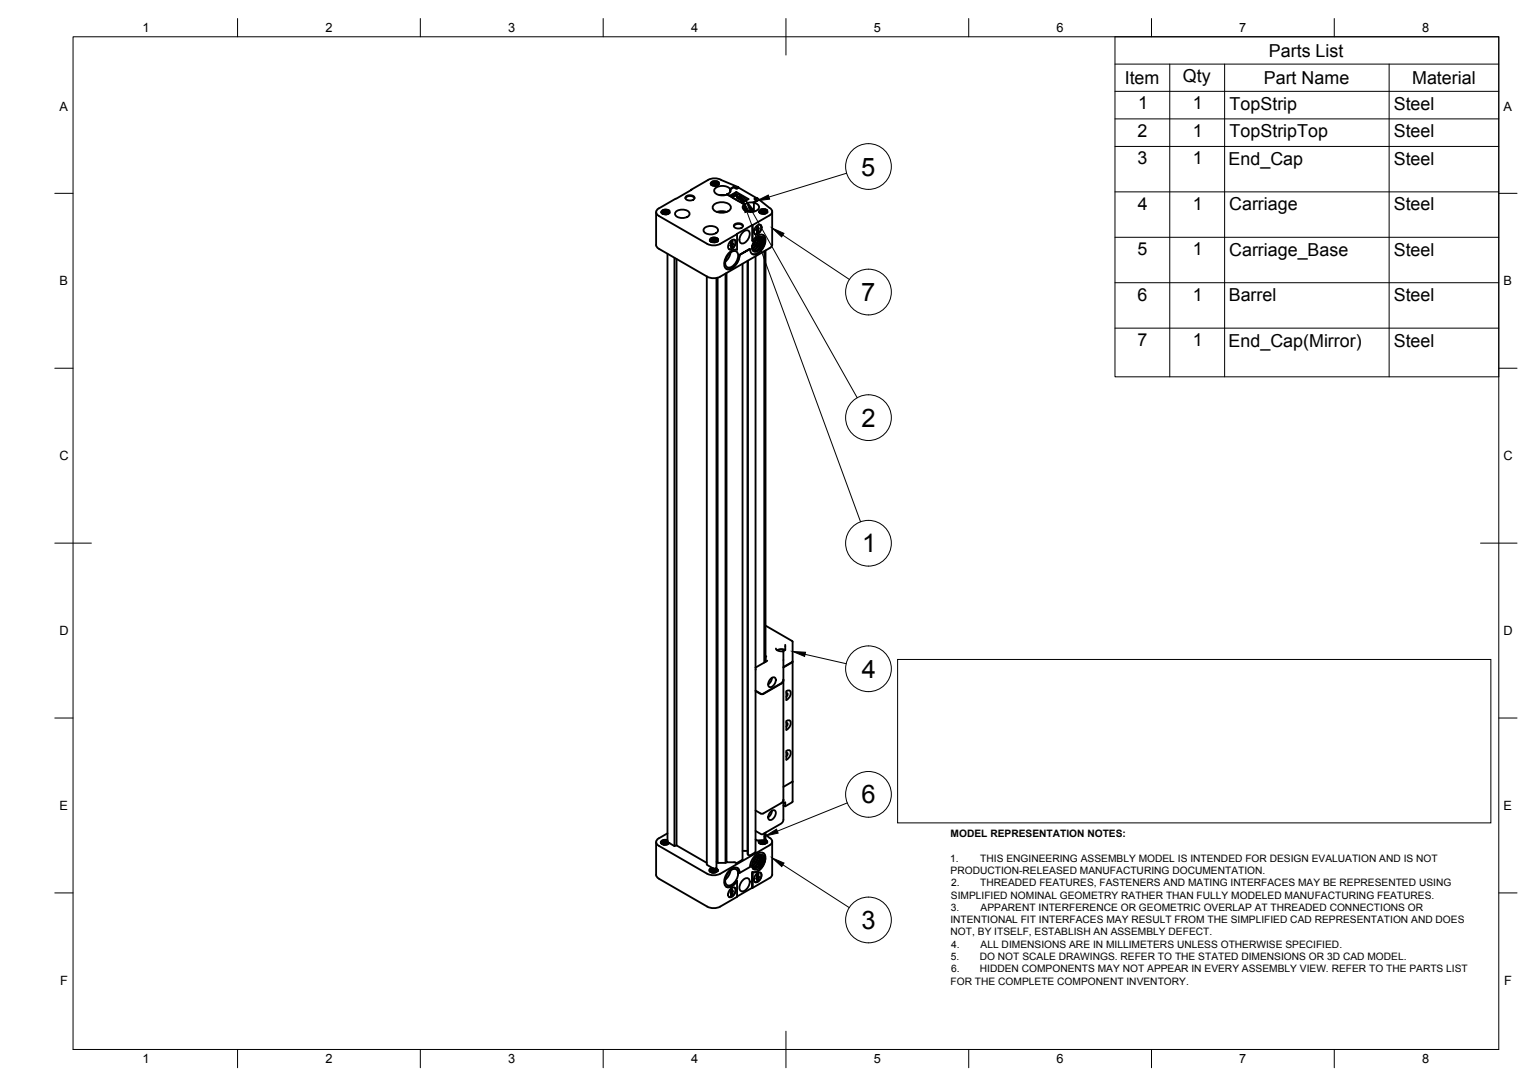
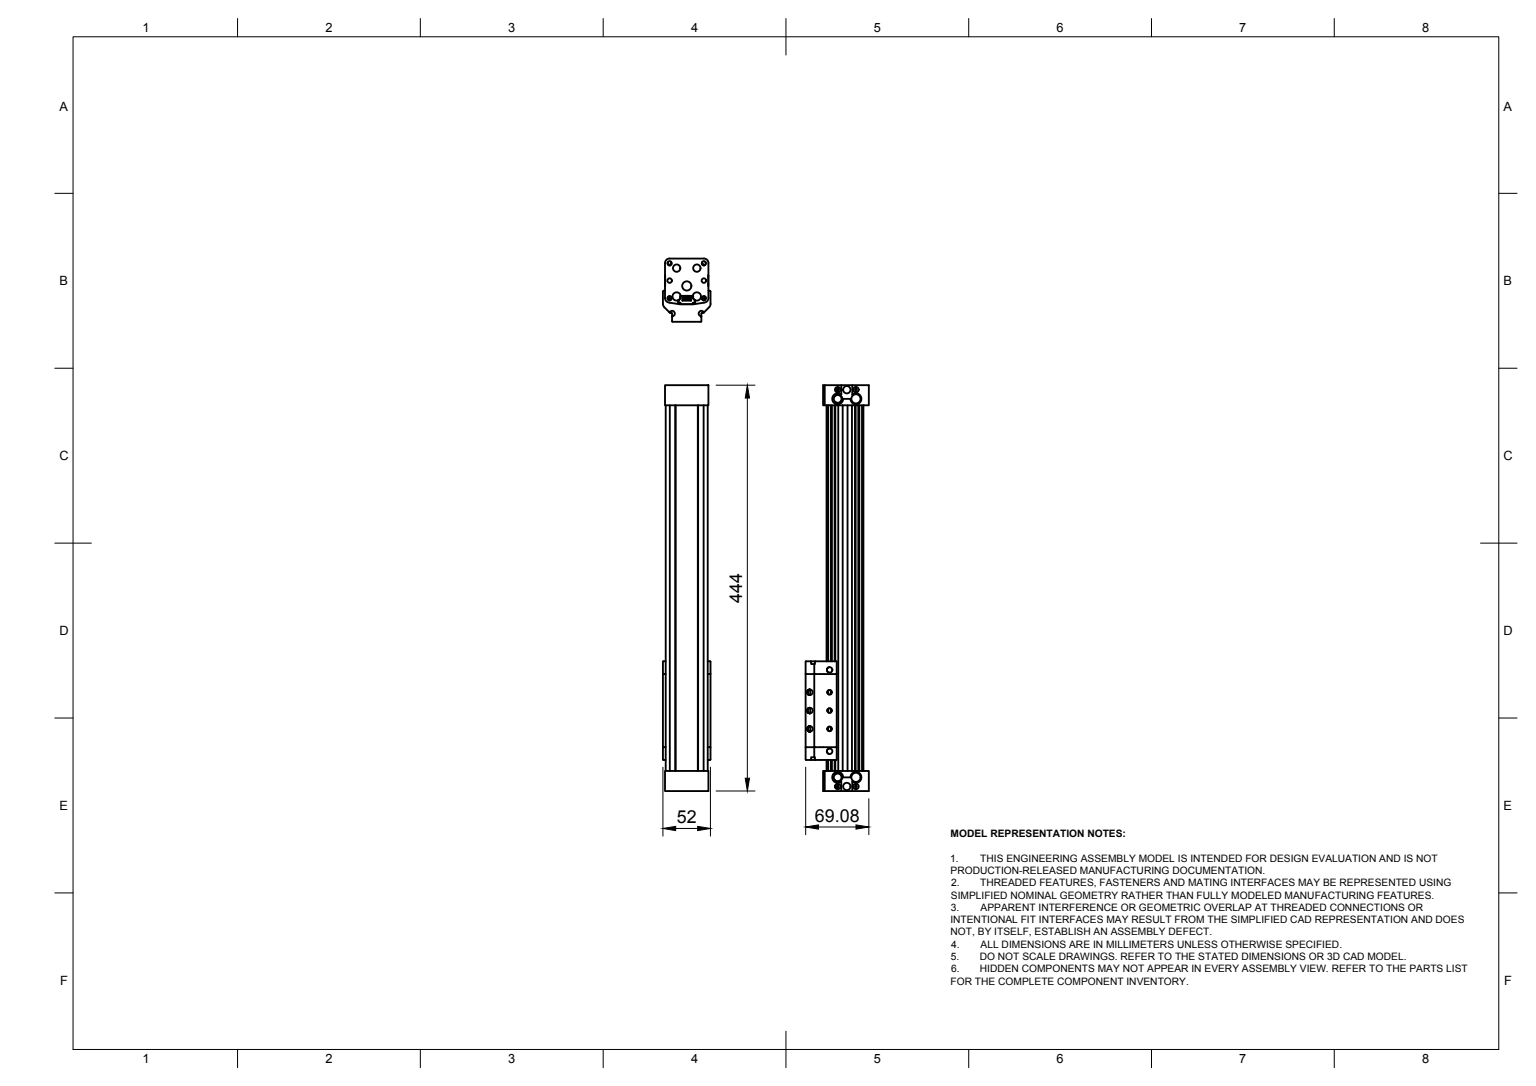
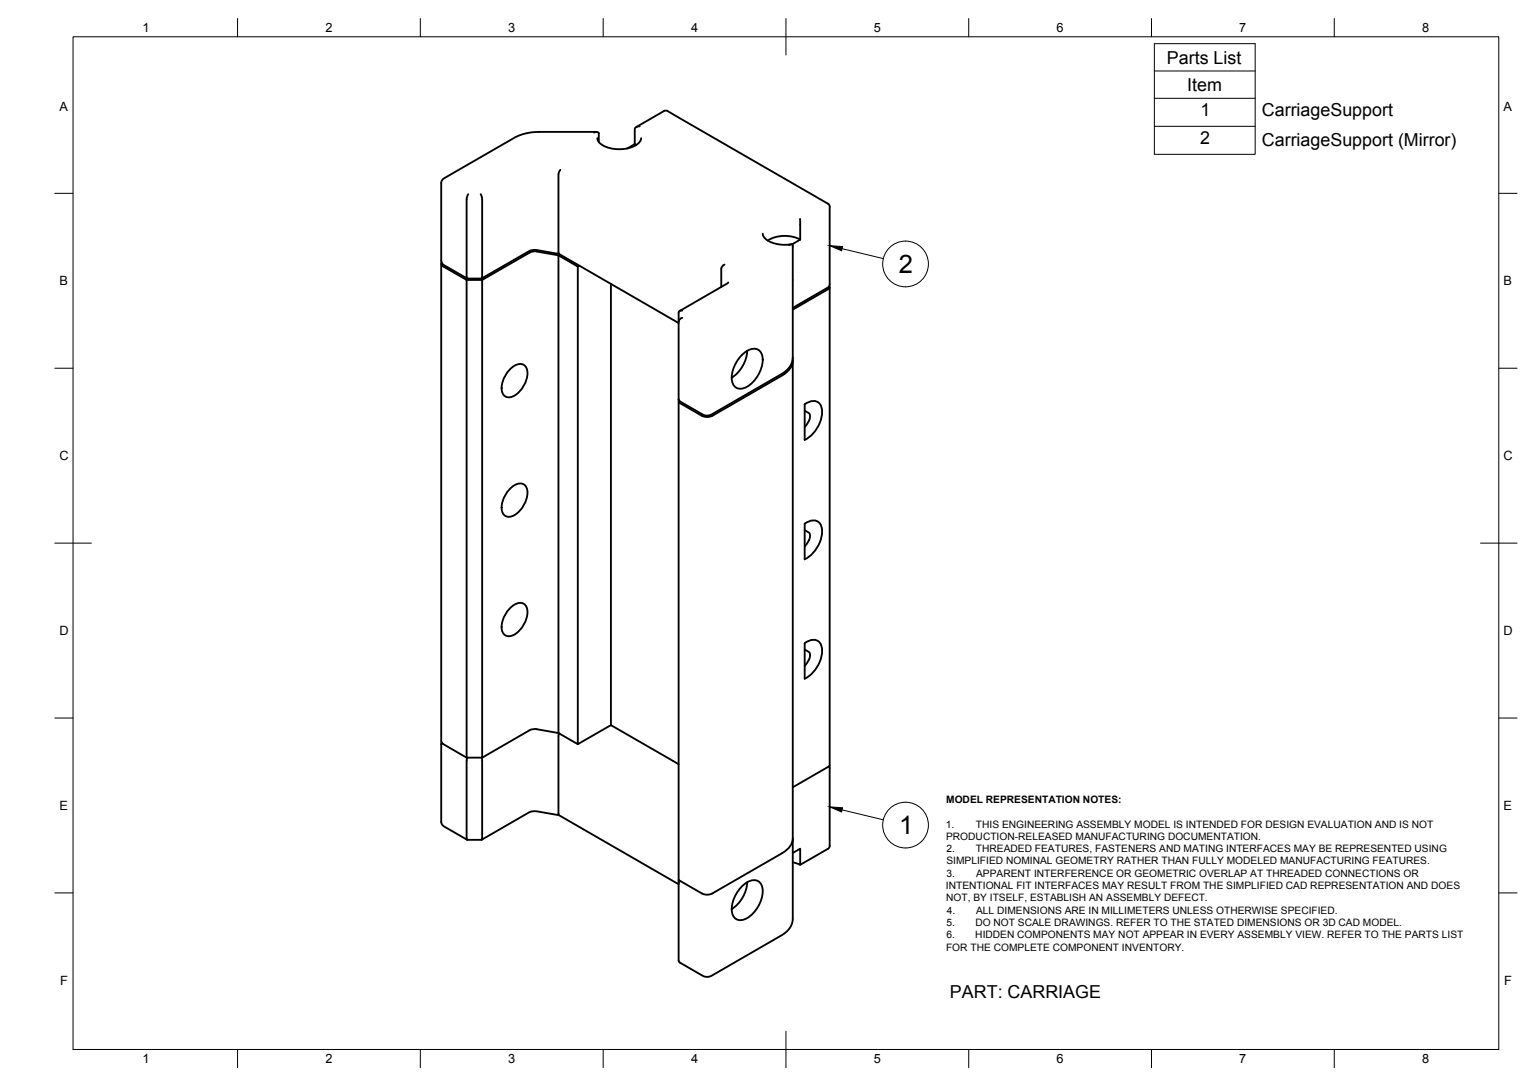
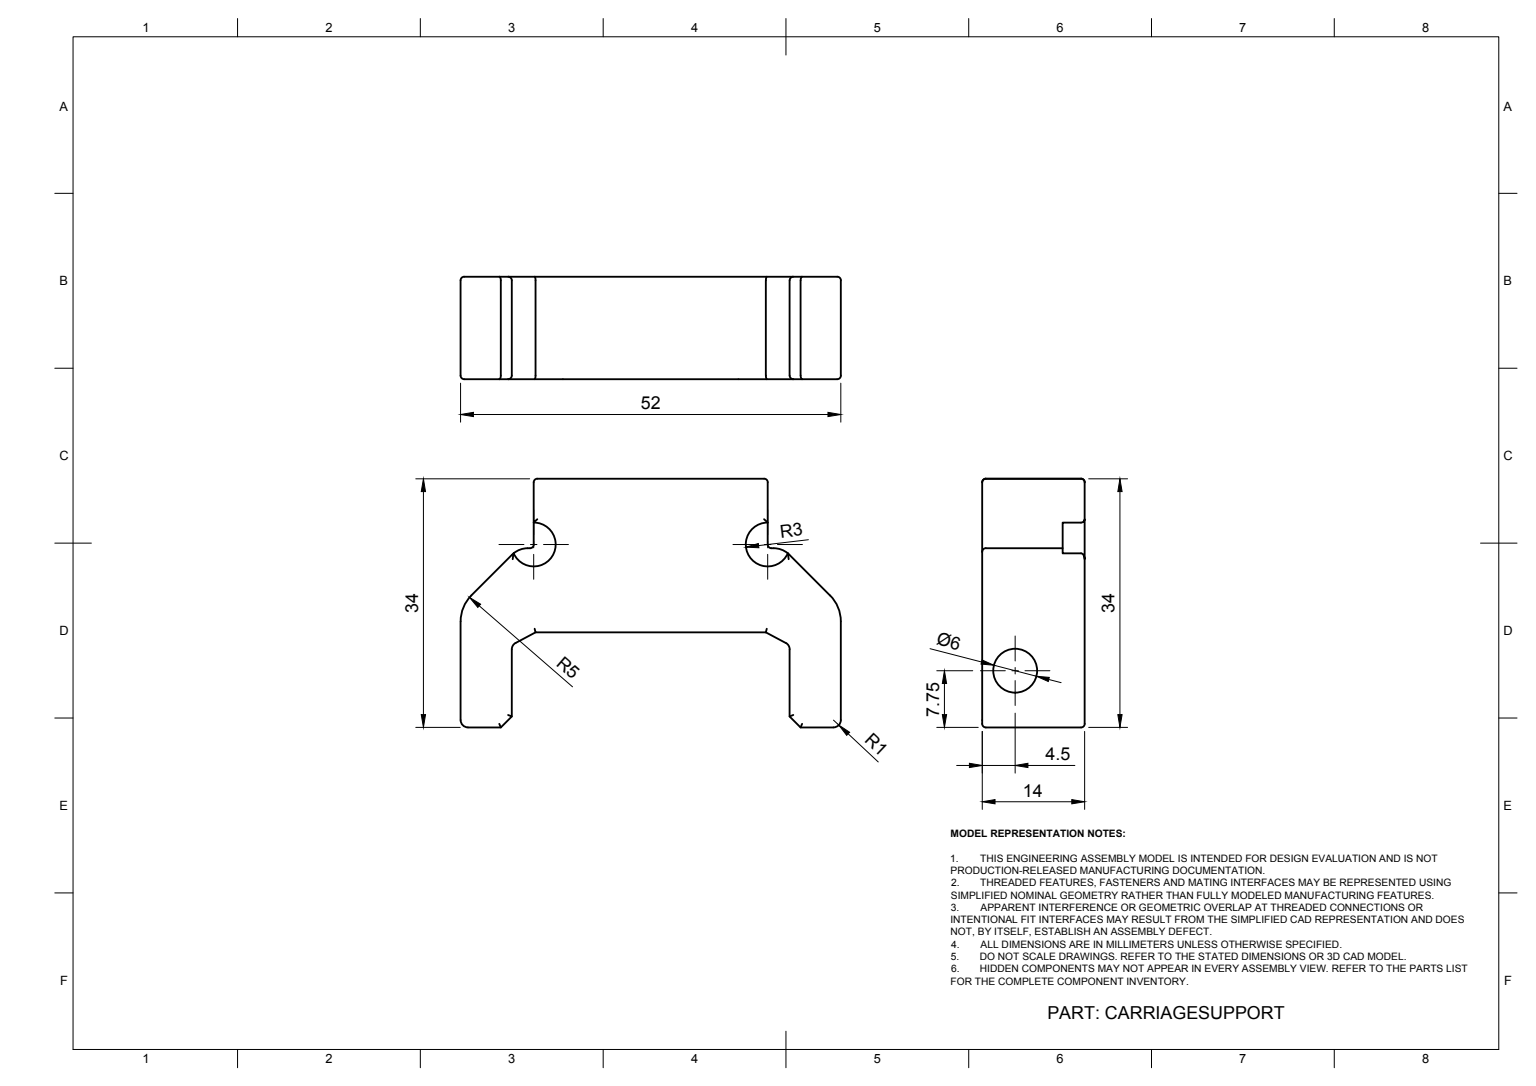
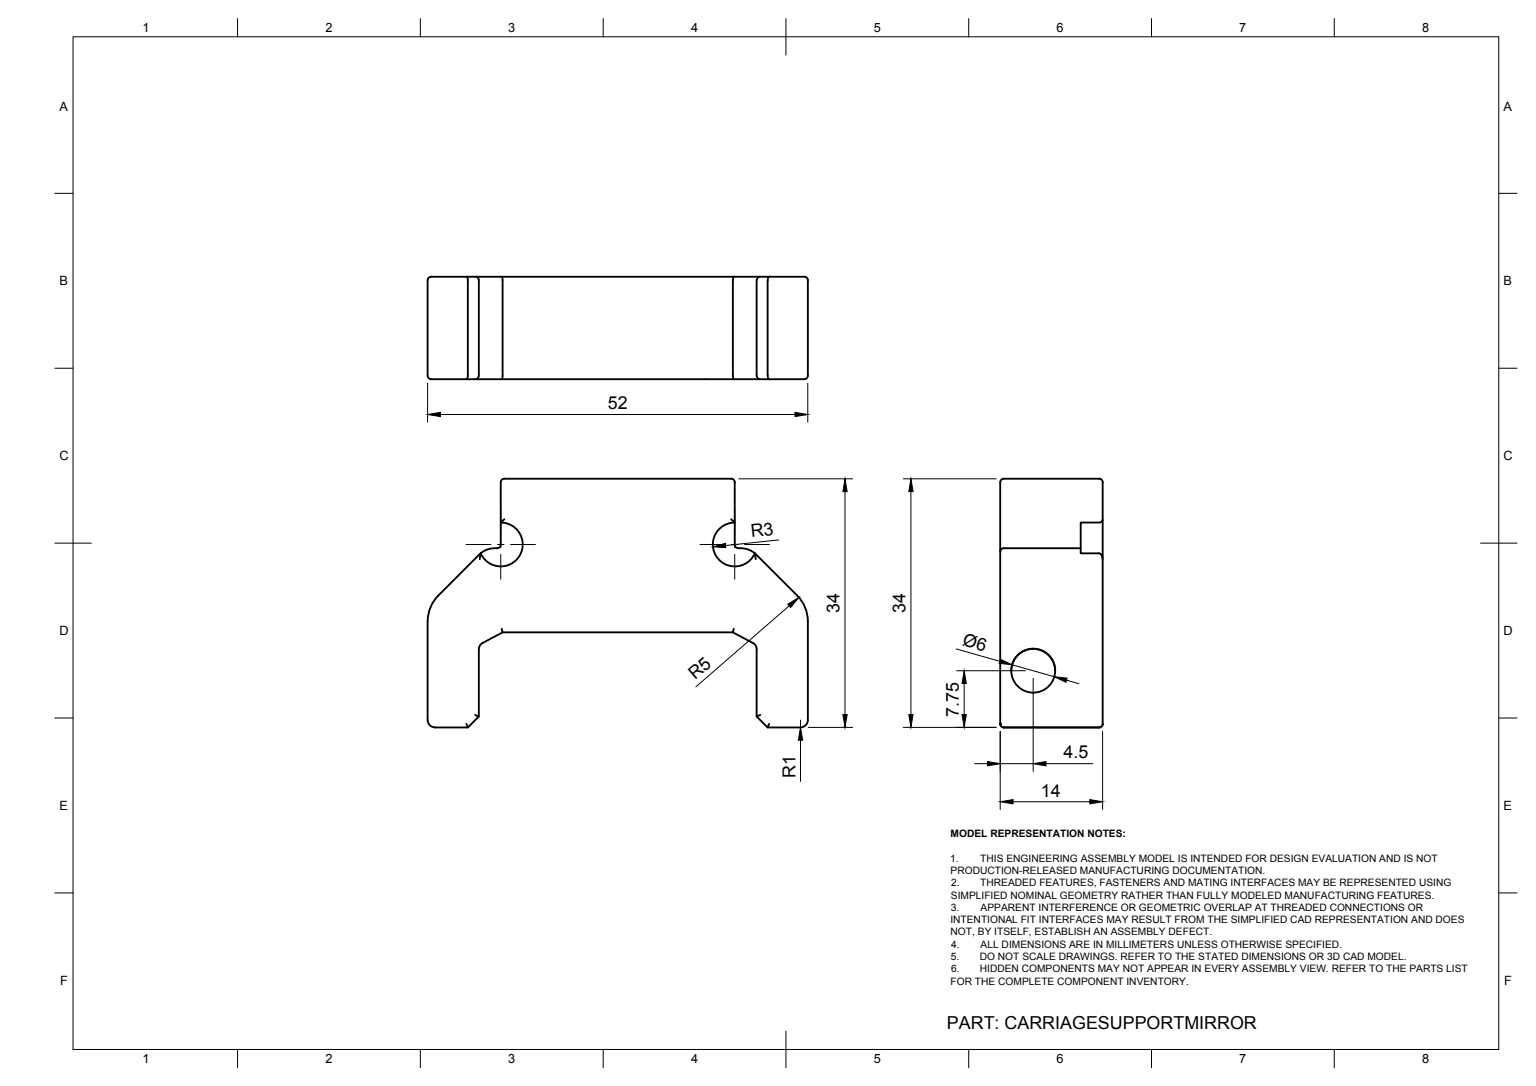
ISO-10303-21;
HEADER;
/* Generated by software containing ST-Developer
 * from STEP Tools, Inc. (www.steptools.com) 
 */

FILE_DESCRIPTION(
/* description */ (''),
/* implementation_level */ '2;1');

FILE_NAME(
/* name */ 'MAS-604',
/* time_stamp */ '2026-10-05T11:01:41-07:00',
/* author */ (''),
/* organization */ (''),
/* preprocessor_version */ 'ST-DEVELOPER v20.2',
/* originating_system */ 'Autodesk Translation Framework v15.15.0.0',
/* authorisation */ '');

FILE_SCHEMA (('AUTOMOTIVE_DESIGN { 1 0 10303 214 3 1 1 }'));
ENDSEC;

DATA;
#10=MECHANICAL_DESIGN_GEOMETRIC_PRESENTATION_REPRESENTATION('',(#2137,#2138,
#2139,#2140,#2141,#2142,#2143,#2144,#2145),#215609);
#11=ITEM_DEFINED_TRANSFORMATION($,$,#28710,#29431);
#12=ITEM_DEFINED_TRANSFORMATION($,$,#28931,#29432);
#13=ITEM_DEFINED_TRANSFORMATION($,$,#28179,#30157);
#14=ITEM_DEFINED_TRANSFORMATION($,$,#28227,#30158);
#15=ITEM_DEFINED_TRANSFORMATION($,$,#28272,#30159);
#16=ITEM_DEFINED_TRANSFORMATION($,$,#28709,#30160);
#17=ITEM_DEFINED_TRANSFORMATION($,$,#29433,#30161);
#18=ITEM_DEFINED_TRANSFORMATION($,$,#29550,#30162);
#19=ITEM_DEFINED_TRANSFORMATION($,$,#29720,#30163);
#20=(
REPRESENTATION_RELATIONSHIP($,$,#215648,#215647)
REPRESENTATION_RELATIONSHIP_WITH_TRANSFORMATION(#11)
SHAPE_REPRESENTATION_RELATIONSHIP()
);
#21=(
REPRESENTATION_RELATIONSHIP($,$,#215649,#215647)
REPRESENTATION_RELATIONSHIP_WITH_TRANSFORMATION(#12)
SHAPE_REPRESENTATION_RELATIONSHIP()
);
#22=(
REPRESENTATION_RELATIONSHIP($,$,#215644,#215643)
REPRESENTATION_RELATIONSHIP_WITH_TRANSFORMATION(#13)
SHAPE_REPRESENTATION_RELATIONSHIP()
);
#23=(
REPRESENTATION_RELATIONSHIP($,$,#215645,#215643)
REPRESENTATION_RELATIONSHIP_WITH_TRANSFORMATION(#14)
SHAPE_REPRESENTATION_RELATIONSHIP()
);
#24=(
REPRESENTATION_RELATIONSHIP($,$,#215646,#215643)
REPRESENTATION_RELATIONSHIP_WITH_TRANSFORMATION(#15)
SHAPE_REPRESENTATION_RELATIONSHIP()
);
#25=(
REPRESENTATION_RELATIONSHIP($,$,#215647,#215643)
REPRESENTATION_RELATIONSHIP_WITH_TRANSFORMATION(#16)
SHAPE_REPRESENTATION_RELATIONSHIP()
);
#26=(
REPRESENTATION_RELATIONSHIP($,$,#215650,#215643)
REPRESENTATION_RELATIONSHIP_WITH_TRANSFORMATION(#17)
SHAPE_REPRESENTATION_RELATIONSHIP()
);
#27=(
REPRESENTATION_RELATIONSHIP($,$,#215651,#215643)
REPRESENTATION_RELATIONSHIP_WITH_TRANSFORMATION(#18)
SHAPE_REPRESENTATION_RELATIONSHIP()
);
#28=(
REPRESENTATION_RELATIONSHIP($,$,#215652,#215643)
REPRESENTATION_RELATIONSHIP_WITH_TRANSFORMATION(#19)
SHAPE_REPRESENTATION_RELATIONSHIP()
);
#29=CONTEXT_DEPENDENT_SHAPE_REPRESENTATION(#20,#215631);
#30=CONTEXT_DEPENDENT_SHAPE_REPRESENTATION(#21,#215632);
#31=CONTEXT_DEPENDENT_SHAPE_REPRESENTATION(#22,#215636);
#32=CONTEXT_DEPENDENT_SHAPE_REPRESENTATION(#23,#215637);
#33=CONTEXT_DEPENDENT_SHAPE_REPRESENTATION(#24,#215638);
#34=CONTEXT_DEPENDENT_SHAPE_REPRESENTATION(#25,#215639);
#35=CONTEXT_DEPENDENT_SHAPE_REPRESENTATION(#26,#215640);
#36=CONTEXT_DEPENDENT_SHAPE_REPRESENTATION(#27,#215641);
#37=CONTEXT_DEPENDENT_SHAPE_REPRESENTATION(#28,#215642);
#38=NEXT_ASSEMBLY_USAGE_OCCURRENCE('CarregeSupport:1',
'CarregeSupport:1','CarregeSupport:1',#215658,#215659,
'CarregeSupport:1');
#39=NEXT_ASSEMBLY_USAGE_OCCURRENCE('CarregeSupport(Mirror):1',
'CarregeSupport(Mirror):1','CarregeSupport(Mirror):1',#215658,#215660,
'CarregeSupport(Mirror):1');
#40=NEXT_ASSEMBLY_USAGE_OCCURRENCE('TopStrip:1','TopStrip:1',
'TopStrip:1',#215654,#215655,'TopStrip:1');
#41=NEXT_ASSEMBLY_USAGE_OCCURRENCE('TopStripTop:1','TopStripTop:1',
'TopStripTop:1',#215654,#215656,'TopStripTop:1');
#42=NEXT_ASSEMBLY_USAGE_OCCURRENCE('End_Cap:1','End_Cap:1','End_Cap:1',
#215654,#215657,'End_Cap:1');
#43=NEXT_ASSEMBLY_USAGE_OCCURRENCE('Carriage:1','Carriage:1',
'Carriage:1',#215654,#215658,'Carriage:1');
#44=NEXT_ASSEMBLY_USAGE_OCCURRENCE('Carriage_Base:1','Carriage_Base:1',
'Carriage_Base:1',#215654,#215661,'Carriage_Base:1');
#45=NEXT_ASSEMBLY_USAGE_OCCURRENCE('Barrel:1','Barrel:1','Barrel:1',#215654,
#215662,'Barrel:1');
#46=NEXT_ASSEMBLY_USAGE_OCCURRENCE('End_Cap(Mirror):1',
'End_Cap(Mirror):1','End_Cap(Mirror):1',#215654,#215663,
'End_Cap(Mirror):1');
#47=SPHERICAL_SURFACE('',#28803,0.5);
#48=SPHERICAL_SURFACE('',#28805,0.5);
#49=SPHERICAL_SURFACE('',#28844,0.5);
#50=SPHERICAL_SURFACE('',#28850,0.5);
#51=SPHERICAL_SURFACE('',#29024,0.5);
#52=SPHERICAL_SURFACE('',#29026,0.5);
#53=SPHERICAL_SURFACE('',#29065,0.5);
#54=SPHERICAL_SURFACE('',#29071,0.5);
#55=(
BOUNDED_SURFACE()
B_SPLINE_SURFACE(2,2,((#124503,#124504,#124505),(#124506,#124507,#124508),
(#124509,#124510,#124511)),.UNSPECIFIED.,.F.,.F.,.F.)
B_SPLINE_SURFACE_WITH_KNOTS((3,3),(3,3),(-1.57079632679498,3.62708052714211E-14),
(-3.14159265358979,-1.57079632679461),.UNSPECIFIED.)
GEOMETRIC_REPRESENTATION_ITEM()
RATIONAL_B_SPLINE_SURFACE(((1.,0.707106781186447,1.),(0.707106781186491,
0.499999999999889,0.707106781186491),(1.,0.707106781186447,1.)))
REPRESENTATION_ITEM('')
SURFACE()
);
#56=(
BOUNDED_SURFACE()
B_SPLINE_SURFACE(2,2,((#124580,#124581,#124582),(#124583,#124584,#124585),
(#124586,#124587,#124588)),.UNSPECIFIED.,.F.,.F.,.F.)
B_SPLINE_SURFACE_WITH_KNOTS((3,3),(3,3),(-1.57079632679491,8.49689085742031E-14),
(-1.57076063039803,3.56963973534065E-5),.UNSPECIFIED.)
GEOMETRIC_REPRESENTATION_ITEM()
RATIONAL_B_SPLINE_SURFACE(((1.,0.707106781186375,1.),(0.707106781186495,
0.499999999999841,0.707106781186495),(1.,0.707106781186375,1.)))
REPRESENTATION_ITEM('')
SURFACE()
);
#57=(
BOUNDED_SURFACE()
B_SPLINE_SURFACE(2,2,((#124901,#124902,#124903),(#124904,#124905,#124906),
(#124907,#124908,#124909)),.UNSPECIFIED.,.F.,.F.,.F.)
B_SPLINE_SURFACE_WITH_KNOTS((3,3),(3,3),(-9.79900252594829E-15,1.57079632679518),
(-1.57076063039766,3.56963969770062E-5),.UNSPECIFIED.)
GEOMETRIC_REPRESENTATION_ITEM()
RATIONAL_B_SPLINE_SURFACE(((1.,0.707106781186639,1.),(0.70710678118645,
0.499999999999996,0.70710678118645),(1.,0.707106781186639,1.)))
REPRESENTATION_ITEM('')
SURFACE()
);
#58=(
BOUNDED_SURFACE()
B_SPLINE_SURFACE(2,2,((#124959,#124960,#124961),(#124962,#124963,#124964),
(#124965,#124966,#124967)),.UNSPECIFIED.,.F.,.F.,.F.)
B_SPLINE_SURFACE_WITH_KNOTS((3,3),(3,3),(-7.03247557642951E-14,1.57079632679488),
(-3.14159265358978,-1.57079632679492),.UNSPECIFIED.)
GEOMETRIC_REPRESENTATION_ITEM()
RATIONAL_B_SPLINE_SURFACE(((1.,0.707106781186562,1.),(0.707106781186541,
0.500000000000006,0.707106781186541),(1.,0.707106781186562,1.)))
REPRESENTATION_ITEM('')
SURFACE()
);
#59=(
BOUNDED_SURFACE()
B_SPLINE_SURFACE(2,2,((#125098,#125099,#125100),(#125101,#125102,#125103),
(#125104,#125105,#125106)),.UNSPECIFIED.,.F.,.F.,.F.)
B_SPLINE_SURFACE_WITH_KNOTS((3,3),(3,3),(-3.62708052714211E-14,1.57079632679498),
(-3.14159265358979,-1.57079632679461),.UNSPECIFIED.)
GEOMETRIC_REPRESENTATION_ITEM()
RATIONAL_B_SPLINE_SURFACE(((1.,0.707106781186447,1.),(0.707106781186491,
0.499999999999889,0.707106781186491),(1.,0.707106781186447,1.)))
REPRESENTATION_ITEM('')
SURFACE()
);
#60=(
BOUNDED_SURFACE()
B_SPLINE_SURFACE(2,2,((#125175,#125176,#125177),(#125178,#125179,#125180),
(#125181,#125182,#125183)),.UNSPECIFIED.,.F.,.F.,.F.)
B_SPLINE_SURFACE_WITH_KNOTS((3,3),(3,3),(-8.49689085742031E-14,1.57079632679491),
(-1.57076063039803,3.56963973534065E-5),.UNSPECIFIED.)
GEOMETRIC_REPRESENTATION_ITEM()
RATIONAL_B_SPLINE_SURFACE(((1.,0.707106781186375,1.),(0.707106781186495,
0.499999999999841,0.707106781186495),(1.,0.707106781186375,1.)))
REPRESENTATION_ITEM('')
SURFACE()
);
#61=(
BOUNDED_SURFACE()
B_SPLINE_SURFACE(2,2,((#125496,#125497,#125498),(#125499,#125500,#125501),
(#125502,#125503,#125504)),.UNSPECIFIED.,.F.,.F.,.F.)
B_SPLINE_SURFACE_WITH_KNOTS((3,3),(3,3),(-1.57079632679518,9.79900252594829E-15),
(-1.57076063039766,3.56963969770062E-5),.UNSPECIFIED.)
GEOMETRIC_REPRESENTATION_ITEM()
RATIONAL_B_SPLINE_SURFACE(((1.,0.707106781186639,1.),(0.70710678118645,
0.499999999999996,0.70710678118645),(1.,0.707106781186639,1.)))
REPRESENTATION_ITEM('')
SURFACE()
);
#62=(
BOUNDED_SURFACE()
B_SPLINE_SURFACE(2,2,((#125554,#125555,#125556),(#125557,#125558,#125559),
(#125560,#125561,#125562)),.UNSPECIFIED.,.F.,.F.,.F.)
B_SPLINE_SURFACE_WITH_KNOTS((3,3),(3,3),(-1.57079632679488,7.03247557642951E-14),
(-3.14159265358978,-1.57079632679492),.UNSPECIFIED.)
GEOMETRIC_REPRESENTATION_ITEM()
RATIONAL_B_SPLINE_SURFACE(((1.,0.707106781186562,1.),(0.707106781186541,
0.500000000000006,0.707106781186541),(1.,0.707106781186562,1.)))
REPRESENTATION_ITEM('')
SURFACE()
);
#63=TOROIDAL_SURFACE('',#28727,1.008,0.5);
#64=TOROIDAL_SURFACE('',#28733,2.5,0.5);
#65=TOROIDAL_SURFACE('',#28739,4.5,0.5);
#66=TOROIDAL_SURFACE('',#28754,1.49999999999999,0.5);
#67=TOROIDAL_SURFACE('',#28763,1.5,0.5);
#68=TOROIDAL_SURFACE('',#28778,4.5,0.5);
#69=TOROIDAL_SURFACE('',#28784,2.5,0.5);
#70=TOROIDAL_SURFACE('',#28790,1.008,0.5);
#71=TOROIDAL_SURFACE('',#28834,3.5,0.5);
#72=TOROIDAL_SURFACE('',#28845,3.5,0.5);
#73=TOROIDAL_SURFACE('',#28865,2.5,0.5);
#74=TOROIDAL_SURFACE('',#28873,4.5,0.5);
#75=TOROIDAL_SURFACE('',#28874,2.5,0.5);
#76=TOROIDAL_SURFACE('',#28880,1.5,0.5);
#77=TOROIDAL_SURFACE('',#28892,1.49999999999999,0.5);
#78=TOROIDAL_SURFACE('',#28898,4.5,0.5);
#79=TOROIDAL_SURFACE('',#28948,1.008,0.5);
#80=TOROIDAL_SURFACE('',#28954,2.5,0.5);
#81=TOROIDAL_SURFACE('',#28960,4.5,0.5);
#82=TOROIDAL_SURFACE('',#28975,1.49999999999999,0.5);
#83=TOROIDAL_SURFACE('',#28984,1.5,0.5);
#84=TOROIDAL_SURFACE('',#28999,4.5,0.5);
#85=TOROIDAL_SURFACE('',#29005,2.5,0.5);
#86=TOROIDAL_SURFACE('',#29011,1.008,0.5);
#87=TOROIDAL_SURFACE('',#29055,3.5,0.5);
#88=TOROIDAL_SURFACE('',#29066,3.5,0.5);
#89=TOROIDAL_SURFACE('',#29086,2.5,0.5);
#90=TOROIDAL_SURFACE('',#29094,4.5,0.5);
#91=TOROIDAL_SURFACE('',#29095,2.5,0.5);
#92=TOROIDAL_SURFACE('',#29101,1.5,0.5);
#93=TOROIDAL_SURFACE('',#29113,1.49999999999999,0.5);
#94=TOROIDAL_SURFACE('',#29119,4.5,0.5);
#95=ELLIPSE('',#28721,0.51530681467495,0.5);
#96=ELLIPSE('',#28749,0.541196100146195,0.5);
#97=ELLIPSE('',#28751,0.541196100146199,0.5);
#98=ELLIPSE('',#28759,0.515306814674945,0.5);
#99=ELLIPSE('',#28768,0.541196100146198,0.5);
#100=ELLIPSE('',#28770,0.541196100146195,0.5);
#101=ELLIPSE('',#28869,0.541196100146197,0.5);
#102=ELLIPSE('',#28876,0.541196100146196,0.5);
#103=ELLIPSE('',#28879,0.51530681467495,0.5);
#104=ELLIPSE('',#28885,0.515306814674951,0.5);
#105=ELLIPSE('',#28891,0.541196100146195,0.5);
#106=ELLIPSE('',#28897,0.541196100146198,0.5);
#107=ELLIPSE('',#28941,0.51530681467495,0.5);
#108=ELLIPSE('',#28970,0.541196100146195,0.5);
#109=ELLIPSE('',#28972,0.541196100146199,0.5);
#110=ELLIPSE('',#28980,0.515306814674945,0.5);
#111=ELLIPSE('',#28989,0.541196100146198,0.5);
#112=ELLIPSE('',#28991,0.541196100146195,0.5);
#113=ELLIPSE('',#29089,0.541196100146197,0.5);
#114=ELLIPSE('',#29097,0.541196100146196,0.5);
#115=ELLIPSE('',#29099,0.51530681467495,0.5);
#116=ELLIPSE('',#29105,0.515306814674951,0.5);
#117=ELLIPSE('',#29111,0.541196100146195,0.5);
#118=ELLIPSE('',#29118,0.541196100146198,0.5);
#119=ELLIPSE('',#29169,4.24264068711927,3.);
#120=ELLIPSE('',#29170,4.24264068711929,3.);
#121=ELLIPSE('',#29171,4.24264068711929,3.);
#122=ELLIPSE('',#29172,4.24279214221557,3.);
#123=ELLIPSE('',#29173,4.24279214221557,3.);
#124=ELLIPSE('',#29174,4.24248924824133,3.);
#125=ELLIPSE('',#29179,4.24248924824133,3.);
#126=ELLIPSE('',#29180,4.24279214221557,3.);
#127=ELLIPSE('',#29181,4.24264068711929,3.);
#128=ELLIPSE('',#29182,4.24264068711927,3.);
#129=ELLIPSE('',#29189,4.24264068711927,3.);
#130=ELLIPSE('',#29190,4.24264068711929,3.);
#131=ELLIPSE('',#29191,4.24264068711929,3.);
#132=ELLIPSE('',#29192,4.24279214221557,3.);
#133=ELLIPSE('',#29193,4.24279214221557,3.);
#134=ELLIPSE('',#29194,4.24248924824133,3.);
#135=ELLIPSE('',#29199,4.24248924824133,3.);
#136=ELLIPSE('',#29200,4.24279214221557,3.);
#137=ELLIPSE('',#29201,4.24264068711929,3.);
#138=ELLIPSE('',#29202,4.24264068711927,3.);
#139=ELLIPSE('',#29209,4.24264068711928,3.00000000000001);
#140=ELLIPSE('',#29210,4.24264068711931,3.00000000000001);
#141=ELLIPSE('',#29211,4.24264068711931,3.00000000000001);
#142=ELLIPSE('',#29212,4.24279214221559,3.00000000000001);
#143=ELLIPSE('',#29213,4.24279214221559,3.00000000000001);
#144=ELLIPSE('',#29214,4.24248924824134,3.00000000000001);
#145=ELLIPSE('',#29219,4.24248924824134,3.00000000000001);
#146=ELLIPSE('',#29220,4.24279214221559,3.00000000000001);
#147=ELLIPSE('',#29221,4.24264068711931,3.00000000000001);
#148=ELLIPSE('',#29222,4.24264068711928,3.00000000000001);
#149=B_SPLINE_SURFACE_WITH_KNOTS('',3,3,((#115948,#115949,#115950,#115951,
#115952,#115953,#115954,#115955,#115956,#115957,#115958,#115959,#115960,
#115961,#115962,#115963,#115964,#115965,#115966,#115967,#115968,#115969,
#115970,#115971,#115972,#115973,#115974,#115975,#115976,#115977,#115978,
#115979,#115980,#115981,#115982,#115983,#115984,#115985,#115986,#115987,
#115988,#115989,#115990,#115991,#115992,#115993,#115994,#115995,#115996,
#115997,#115998,#115999,#116000,#116001),(#116002,#116003,#116004,#116005,
#116006,#116007,#116008,#116009,#116010,#116011,#116012,#116013,#116014,
#116015,#116016,#116017,#116018,#116019,#116020,#116021,#116022,#116023,
#116024,#116025,#116026,#116027,#116028,#116029,#116030,#116031,#116032,
#116033,#116034,#116035,#116036,#116037,#116038,#116039,#116040,#116041,
#116042,#116043,#116044,#116045,#116046,#116047,#116048,#116049,#116050,
#116051,#116052,#116053,#116054,#116055),(#116056,#116057,#116058,#116059,
#116060,#116061,#116062,#116063,#116064,#116065,#116066,#116067,#116068,
#116069,#116070,#116071,#116072,#116073,#116074,#116075,#116076,#116077,
#116078,#116079,#116080,#116081,#116082,#116083,#116084,#116085,#116086,
#116087,#116088,#116089,#116090,#116091,#116092,#116093,#116094,#116095,
#116096,#116097,#116098,#116099,#116100,#116101,#116102,#116103,#116104,
#116105,#116106,#116107,#116108,#116109),(#116110,#116111,#116112,#116113,
#116114,#116115,#116116,#116117,#116118,#116119,#116120,#116121,#116122,
#116123,#116124,#116125,#116126,#116127,#116128,#116129,#116130,#116131,
#116132,#116133,#116134,#116135,#116136,#116137,#116138,#116139,#116140,
#116141,#116142,#116143,#116144,#116145,#116146,#116147,#116148,#116149,
#116150,#116151,#116152,#116153,#116154,#116155,#116156,#116157,#116158,
#116159,#116160,#116161,#116162,#116163)),.UNSPECIFIED.,.F.,.F.,.F.,(4,
4),(4,1,1,1,1,1,1,1,1,1,1,1,1,1,1,1,1,1,1,1,1,1,1,1,1,1,1,1,1,1,1,1,1,1,
1,1,1,1,1,1,1,1,1,1,1,1,1,1,1,1,1,4),(-0.000626221895392836,0.0969365212249631),
(11.8528940954716,12.340290362188,12.8276378599491,13.3149853577101,13.8023328554711,
14.2896803532321,14.7770278509931,15.2643753487541,15.7517228465151,16.2390703442761,
16.7264178420371,17.2137653397981,17.7011128375591,18.1884603353201,18.6758078330811,
19.1631553308421,19.6505028286031,20.1378503263641,20.6251978241251,21.1125453218861,
21.5998928196471,22.0872403174081,22.5745878151691,23.0619353129301,23.5492828106911,
24.5239778062131,25.4986728017351,26.4733677972571,26.9607152950181,27.4480627927791,
27.9354102905401,28.4227577883011,28.9101052860621,29.3974527838231,29.8848002815841,
30.3721477793451,30.8594952771061,31.3468427748671,31.8341902726282,32.3215377703892,
32.8088852681502,33.2962327659112,33.7835802636722,34.2709277614332,34.7582752591942,
35.2456227569552,35.7329702547162,36.2203177524772,36.7076652502382,37.1950127479992,
37.6823602457602,38.1697077435212),.UNSPECIFIED.);
#150=B_SPLINE_SURFACE_WITH_KNOTS('',3,3,((#116370,#116371,#116372,#116373,
#116374,#116375,#116376,#116377,#116378,#116379,#116380,#116381,#116382,
#116383,#116384,#116385,#116386,#116387,#116388,#116389,#116390,#116391,
#116392,#116393,#116394,#116395,#116396,#116397,#116398,#116399,#116400,
#116401,#116402,#116403,#116404,#116405,#116406,#116407,#116408,#116409,
#116410,#116411,#116412,#116413,#116414,#116415,#116416,#116417,#116418,
#116419,#116420,#116421,#116422,#116423),(#116424,#116425,#116426,#116427,
#116428,#116429,#116430,#116431,#116432,#116433,#116434,#116435,#116436,
#116437,#116438,#116439,#116440,#116441,#116442,#116443,#116444,#116445,
#116446,#116447,#116448,#116449,#116450,#116451,#116452,#116453,#116454,
#116455,#116456,#116457,#116458,#116459,#116460,#116461,#116462,#116463,
#116464,#116465,#116466,#116467,#116468,#116469,#116470,#116471,#116472,
#116473,#116474,#116475,#116476,#116477),(#116478,#116479,#116480,#116481,
#116482,#116483,#116484,#116485,#116486,#116487,#116488,#116489,#116490,
#116491,#116492,#116493,#116494,#116495,#116496,#116497,#116498,#116499,
#116500,#116501,#116502,#116503,#116504,#116505,#116506,#116507,#116508,
#116509,#116510,#116511,#116512,#116513,#116514,#116515,#116516,#116517,
#116518,#116519,#116520,#116521,#116522,#116523,#116524,#116525,#116526,
#116527,#116528,#116529,#116530,#116531),(#116532,#116533,#116534,#116535,
#116536,#116537,#116538,#116539,#116540,#116541,#116542,#116543,#116544,
#116545,#116546,#116547,#116548,#116549,#116550,#116551,#116552,#116553,
#116554,#116555,#116556,#116557,#116558,#116559,#116560,#116561,#116562,
#116563,#116564,#116565,#116566,#116567,#116568,#116569,#116570,#116571,
#116572,#116573,#116574,#116575,#116576,#116577,#116578,#116579,#116580,
#116581,#116582,#116583,#116584,#116585)),.UNSPECIFIED.,.F.,.F.,.F.,(4,
4),(4,1,1,1,1,1,1,1,1,1,1,1,1,1,1,1,1,1,1,1,1,1,1,1,1,1,1,1,1,1,1,1,1,1,
1,1,1,1,1,1,1,1,1,1,1,1,1,1,1,1,1,4),(-0.000403511276840155,0.0967757900741628),
(14.399609326548,14.886956824309,15.37430432207,15.861651819831,16.348999317592,
16.836346815353,17.323694313114,17.811041810875,18.298389308636,18.785736806397,
19.273084304158,19.7604318019191,20.2477792996801,20.7351267974411,21.2224742952021,
21.7098217929631,22.1971692907241,22.6845167884851,23.1718642862461,23.6592117840071,
24.1465592817681,24.6339067795291,25.1212542772901,25.6086017750511,26.0959492728121,
27.0706442683341,28.0453392638561,29.0200342593781,29.5073817571391,29.9947292549001,
30.4820767526611,30.9694242504221,31.4567717481831,31.9441192459441,32.4314667437051,
32.9188142414661,33.4061617392271,33.8935092369881,34.3808567347491,34.8682042325101,
35.3555517302711,35.8428992280321,36.3302467257931,36.8175942235541,37.3049417213151,
37.7922892190762,38.2796367168372,38.7669842145982,39.2543317123592,39.7416792101202,
40.2290267078812,40.7164229770097),.UNSPECIFIED.);
#151=B_SPLINE_SURFACE_WITH_KNOTS('',3,3,((#116789,#116790,#116791,#116792,
#116793,#116794,#116795,#116796,#116797,#116798,#116799,#116800,#116801,
#116802,#116803,#116804,#116805,#116806,#116807,#116808,#116809,#116810,
#116811,#116812,#116813,#116814,#116815,#116816,#116817,#116818,#116819,
#116820,#116821,#116822,#116823,#116824,#116825,#116826,#116827,#116828,
#116829,#116830,#116831,#116832,#116833,#116834,#116835,#116836,#116837,
#116838,#116839,#116840,#116841,#116842),(#116843,#116844,#116845,#116846,
#116847,#116848,#116849,#116850,#116851,#116852,#116853,#116854,#116855,
#116856,#116857,#116858,#116859,#116860,#116861,#116862,#116863,#116864,
#116865,#116866,#116867,#116868,#116869,#116870,#116871,#116872,#116873,
#116874,#116875,#116876,#116877,#116878,#116879,#116880,#116881,#116882,
#116883,#116884,#116885,#116886,#116887,#116888,#116889,#116890,#116891,
#116892,#116893,#116894,#116895,#116896),(#116897,#116898,#116899,#116900,
#116901,#116902,#116903,#116904,#116905,#116906,#116907,#116908,#116909,
#116910,#116911,#116912,#116913,#116914,#116915,#116916,#116917,#116918,
#116919,#116920,#116921,#116922,#116923,#116924,#116925,#116926,#116927,
#116928,#116929,#116930,#116931,#116932,#116933,#116934,#116935,#116936,
#116937,#116938,#116939,#116940,#116941,#116942,#116943,#116944,#116945,
#116946,#116947,#116948,#116949,#116950),(#116951,#116952,#116953,#116954,
#116955,#116956,#116957,#116958,#116959,#116960,#116961,#116962,#116963,
#116964,#116965,#116966,#116967,#116968,#116969,#116970,#116971,#116972,
#116973,#116974,#116975,#116976,#116977,#116978,#116979,#116980,#116981,
#116982,#116983,#116984,#116985,#116986,#116987,#116988,#116989,#116990,
#116991,#116992,#116993,#116994,#116995,#116996,#116997,#116998,#116999,
#117000,#117001,#117002,#117003,#117004)),.UNSPECIFIED.,.F.,.F.,.F.,(4,
4),(4,1,1,1,1,1,1,1,1,1,1,1,1,1,1,1,1,1,1,1,1,1,1,1,1,1,1,1,1,1,1,1,1,1,
1,1,1,1,1,1,1,1,1,1,1,1,1,1,1,1,1,4),(-0.000626380093345518,0.0969365193294648),
(11.8528940858174,12.340290362188,12.827637859949,13.31498535771,13.802332855471,
14.289680353232,14.777027850993,15.264375348754,15.751722846515,16.239070344276,
16.7264178420371,17.2137653397981,17.7011128375591,18.1884603353201,18.6758078330811,
19.1631553308421,19.6505028286031,20.1378503263641,20.6251978241251,21.1125453218861,
21.5998928196471,22.0872403174081,22.5745878151691,23.0619353129301,23.5492828106911,
24.5239778062131,25.4986728017351,26.4733677972571,26.9607152950181,27.4480627927791,
27.9354102905401,28.4227577883011,28.9101052860621,29.3974527838231,29.8848002815841,
30.3721477793451,30.8594952771061,31.3468427748671,31.8341902726281,32.3215377703891,
32.8088852681501,33.2962327659111,33.7835802636721,34.2709277614331,34.7582752591941,
35.2456227569552,35.7329702547162,36.2203177524772,36.7076652502382,37.1950127479992,
37.6823602457602,38.1697077435212),.UNSPECIFIED.);
#152=B_SPLINE_SURFACE_WITH_KNOTS('',3,3,((#117214,#117215,#117216,#117217,
#117218,#117219,#117220,#117221,#117222,#117223,#117224,#117225,#117226,
#117227,#117228,#117229,#117230,#117231,#117232,#117233,#117234,#117235,
#117236,#117237,#117238,#117239,#117240,#117241,#117242,#117243,#117244,
#117245,#117246,#117247,#117248,#117249,#117250,#117251,#117252,#117253,
#117254,#117255,#117256,#117257,#117258,#117259,#117260,#117261,#117262,
#117263,#117264,#117265,#117266,#117267),(#117268,#117269,#117270,#117271,
#117272,#117273,#117274,#117275,#117276,#117277,#117278,#117279,#117280,
#117281,#117282,#117283,#117284,#117285,#117286,#117287,#117288,#117289,
#117290,#117291,#117292,#117293,#117294,#117295,#117296,#117297,#117298,
#117299,#117300,#117301,#117302,#117303,#117304,#117305,#117306,#117307,
#117308,#117309,#117310,#117311,#117312,#117313,#117314,#117315,#117316,
#117317,#117318,#117319,#117320,#117321),(#117322,#117323,#117324,#117325,
#117326,#117327,#117328,#117329,#117330,#117331,#117332,#117333,#117334,
#117335,#117336,#117337,#117338,#117339,#117340,#117341,#117342,#117343,
#117344,#117345,#117346,#117347,#117348,#117349,#117350,#117351,#117352,
#117353,#117354,#117355,#117356,#117357,#117358,#117359,#117360,#117361,
#117362,#117363,#117364,#117365,#117366,#117367,#117368,#117369,#117370,
#117371,#117372,#117373,#117374,#117375),(#117376,#117377,#117378,#117379,
#117380,#117381,#117382,#117383,#117384,#117385,#117386,#117387,#117388,
#117389,#117390,#117391,#117392,#117393,#117394,#117395,#117396,#117397,
#117398,#117399,#117400,#117401,#117402,#117403,#117404,#117405,#117406,
#117407,#117408,#117409,#117410,#117411,#117412,#117413,#117414,#117415,
#117416,#117417,#117418,#117419,#117420,#117421,#117422,#117423,#117424,
#117425,#117426,#117427,#117428,#117429)),.UNSPECIFIED.,.F.,.F.,.F.,(4,
4),(4,1,1,1,1,1,1,1,1,1,1,1,1,1,1,1,1,1,1,1,1,1,1,1,1,1,1,1,1,1,1,1,1,1,
1,1,1,1,1,1,1,1,1,1,1,1,1,1,1,1,1,4),(-0.000403508817394493,0.0967757699182735),
(14.399609326548,14.886956824309,15.37430432207,15.861651819831,16.348999317592,
16.836346815353,17.323694313114,17.811041810875,18.298389308636,18.785736806397,
19.273084304158,19.760431801919,20.24777929968,20.735126797441,21.222474295202,
21.709821792963,22.1971692907241,22.6845167884851,23.1718642862461,23.6592117840071,
24.1465592817681,24.6339067795291,25.1212542772901,25.6086017750511,26.0959492728121,
27.0706442683341,28.0453392638561,29.0200342593781,29.5073817571391,29.9947292549001,
30.4820767526611,30.9694242504221,31.4567717481831,31.9441192459441,32.4314667437051,
32.9188142414661,33.4061617392271,33.8935092369881,34.3808567347491,34.8682042325101,
35.3555517302711,35.8428992280321,36.3302467257931,36.8175942235541,37.3049417213151,
37.7922892190761,38.2796367168371,38.7669842145981,39.2543317123591,39.7416792101202,
40.2290267078812,40.7164229892059),.UNSPECIFIED.);
#153=B_SPLINE_SURFACE_WITH_KNOTS('',3,3,((#117642,#117643,#117644,#117645,
#117646,#117647,#117648,#117649,#117650,#117651,#117652,#117653,#117654,
#117655,#117656,#117657,#117658,#117659,#117660,#117661,#117662,#117663,
#117664,#117665,#117666,#117667,#117668,#117669,#117670,#117671,#117672,
#117673,#117674,#117675,#117676,#117677,#117678,#117679,#117680,#117681,
#117682,#117683,#117684,#117685,#117686,#117687,#117688,#117689,#117690,
#117691,#117692,#117693,#117694,#117695,#117696,#117697,#117698,#117699,
#117700,#117701,#117702,#117703,#117704,#117705,#117706,#117707,#117708,
#117709,#117710,#117711,#117712,#117713,#117714,#117715,#117716,#117717,
#117718,#117719,#117720,#117721,#117722,#117723,#117724,#117725,#117726,
#117727,#117728,#117729,#117730,#117731,#117732,#117733,#117734,#117735,
#117736,#117737,#117738,#117739,#117740,#117741,#117742,#117743,#117744,
#117745,#117746,#117747,#117748,#117749,#117750,#117751,#117752,#117753,
#117754,#117755,#117756,#117757,#117758,#117759,#117760,#117761,#117762,
#117763,#117764,#117765,#117766,#117767,#117768,#117769,#117770,#117771,
#117772,#117773,#117774,#117775,#117776,#117777,#117778,#117779,#117780,
#117781,#117782,#117783,#117784,#117785,#117786,#117787,#117788,#117789,
#117790,#117791,#117792,#117793,#117794,#117795,#117796,#117797,#117798,
#117799,#117800,#117801,#117802,#117803,#117804,#117805,#117806,#117807,
#117808,#117809,#117810,#117811,#117812,#117813,#117814,#117815,#117816,
#117817,#117818,#117819),(#117820,#117821,#117822,#117823,#117824,#117825,
#117826,#117827,#117828,#117829,#117830,#117831,#117832,#117833,#117834,
#117835,#117836,#117837,#117838,#117839,#117840,#117841,#117842,#117843,
#117844,#117845,#117846,#117847,#117848,#117849,#117850,#117851,#117852,
#117853,#117854,#117855,#117856,#117857,#117858,#117859,#117860,#117861,
#117862,#117863,#117864,#117865,#117866,#117867,#117868,#117869,#117870,
#117871,#117872,#117873,#117874,#117875,#117876,#117877,#117878,#117879,
#117880,#117881,#117882,#117883,#117884,#117885,#117886,#117887,#117888,
#117889,#117890,#117891,#117892,#117893,#117894,#117895,#117896,#117897,
#117898,#117899,#117900,#117901,#117902,#117903,#117904,#117905,#117906,
#117907,#117908,#117909,#117910,#117911,#117912,#117913,#117914,#117915,
#117916,#117917,#117918,#117919,#117920,#117921,#117922,#117923,#117924,
#117925,#117926,#117927,#117928,#117929,#117930,#117931,#117932,#117933,
#117934,#117935,#117936,#117937,#117938,#117939,#117940,#117941,#117942,
#117943,#117944,#117945,#117946,#117947,#117948,#117949,#117950,#117951,
#117952,#117953,#117954,#117955,#117956,#117957,#117958,#117959,#117960,
#117961,#117962,#117963,#117964,#117965,#117966,#117967,#117968,#117969,
#117970,#117971,#117972,#117973,#117974,#117975,#117976,#117977,#117978,
#117979,#117980,#117981,#117982,#117983,#117984,#117985,#117986,#117987,
#117988,#117989,#117990,#117991,#117992,#117993,#117994,#117995,#117996,
#117997),(#117998,#117999,#118000,#118001,#118002,#118003,#118004,#118005,
#118006,#118007,#118008,#118009,#118010,#118011,#118012,#118013,#118014,
#118015,#118016,#118017,#118018,#118019,#118020,#118021,#118022,#118023,
#118024,#118025,#118026,#118027,#118028,#118029,#118030,#118031,#118032,
#118033,#118034,#118035,#118036,#118037,#118038,#118039,#118040,#118041,
#118042,#118043,#118044,#118045,#118046,#118047,#118048,#118049,#118050,
#118051,#118052,#118053,#118054,#118055,#118056,#118057,#118058,#118059,
#118060,#118061,#118062,#118063,#118064,#118065,#118066,#118067,#118068,
#118069,#118070,#118071,#118072,#118073,#118074,#118075,#118076,#118077,
#118078,#118079,#118080,#118081,#118082,#118083,#118084,#118085,#118086,
#118087,#118088,#118089,#118090,#118091,#118092,#118093,#118094,#118095,
#118096,#118097,#118098,#118099,#118100,#118101,#118102,#118103,#118104,
#118105,#118106,#118107,#118108,#118109,#118110,#118111,#118112,#118113,
#118114,#118115,#118116,#118117,#118118,#118119,#118120,#118121,#118122,
#118123,#118124,#118125,#118126,#118127,#118128,#118129,#118130,#118131,
#118132,#118133,#118134,#118135,#118136,#118137,#118138,#118139,#118140,
#118141,#118142,#118143,#118144,#118145,#118146,#118147,#118148,#118149,
#118150,#118151,#118152,#118153,#118154,#118155,#118156,#118157,#118158,
#118159,#118160,#118161,#118162,#118163,#118164,#118165,#118166,#118167,
#118168,#118169,#118170,#118171,#118172,#118173,#118174,#118175),(#118176,
#118177,#118178,#118179,#118180,#118181,#118182,#118183,#118184,#118185,
#118186,#118187,#118188,#118189,#118190,#118191,#118192,#118193,#118194,
#118195,#118196,#118197,#118198,#118199,#118200,#118201,#118202,#118203,
#118204,#118205,#118206,#118207,#118208,#118209,#118210,#118211,#118212,
#118213,#118214,#118215,#118216,#118217,#118218,#118219,#118220,#118221,
#118222,#118223,#118224,#118225,#118226,#118227,#118228,#118229,#118230,
#118231,#118232,#118233,#118234,#118235,#118236,#118237,#118238,#118239,
#118240,#118241,#118242,#118243,#118244,#118245,#118246,#118247,#118248,
#118249,#118250,#118251,#118252,#118253,#118254,#118255,#118256,#118257,
#118258,#118259,#118260,#118261,#118262,#118263,#118264,#118265,#118266,
#118267,#118268,#118269,#118270,#118271,#118272,#118273,#118274,#118275,
#118276,#118277,#118278,#118279,#118280,#118281,#118282,#118283,#118284,
#118285,#118286,#118287,#118288,#118289,#118290,#118291,#118292,#118293,
#118294,#118295,#118296,#118297,#118298,#118299,#118300,#118301,#118302,
#118303,#118304,#118305,#118306,#118307,#118308,#118309,#118310,#118311,
#118312,#118313,#118314,#118315,#118316,#118317,#118318,#118319,#118320,
#118321,#118322,#118323,#118324,#118325,#118326,#118327,#118328,#118329,
#118330,#118331,#118332,#118333,#118334,#118335,#118336,#118337,#118338,
#118339,#118340,#118341,#118342,#118343,#118344,#118345,#118346,#118347,
#118348,#118349,#118350,#118351,#118352,#118353)),.UNSPECIFIED.,.F.,.F.,
 .F.,(4,4),(4,1,1,1,1,1,1,1,1,1,1,1,1,1,1,1,1,1,1,1,1,1,1,1,1,1,1,1,1,1,
1,1,1,1,1,1,1,1,1,1,1,1,1,1,1,1,1,1,1,1,1,1,1,1,1,1,1,1,1,1,1,1,1,1,1,1,
1,1,1,1,1,1,1,1,1,1,1,1,1,1,1,1,1,1,1,1,1,1,1,1,1,1,1,1,1,1,1,1,1,1,1,1,
1,1,1,1,1,1,1,1,1,1,1,1,1,1,1,1,1,1,1,1,1,1,1,1,1,1,1,1,1,1,1,1,1,1,1,1,
1,1,1,1,1,1,1,1,1,1,1,1,1,1,1,1,1,1,1,1,1,1,1,1,1,1,1,1,1,1,1,1,1,1,1,1,
1,4),(-0.000439606948779746,0.0515314320759051),(11.8664846275776,12.8657606844883,
13.8645971344502,14.8634335844121,15.8622700343739,16.8611064843358,17.8599429342977,
18.8587793842595,19.8576158342214,20.8564522841833,21.8552887341452,22.854125184107,
23.8529616340689,24.8517980840308,25.8506345339927,26.8494709839545,27.8483074339164,
28.8471438838783,29.8459803338402,30.844816783802,31.8436532337639,32.8424896837258,
33.8413261336877,34.8401625836495,35.8389990336114,36.8378354835733,37.8366719335352,
38.835508383497,39.8343448334589,40.8331812834208,41.8320177333826,42.8308541833445,
43.8296906333064,44.8285270832683,45.8273635332301,46.826199983192,47.8250364331539,
48.8238728831158,49.8227093330776,50.8215457830395,51.8203822330014,52.8192186829633,
53.8180551329251,54.816891582887,55.8157280328489,56.8145644828108,57.8134009327726,
58.8122373827345,59.8110738326964,60.8099102826583,61.8087467326201,62.807583182582,
63.8064196325439,64.8052560825058,65.8040925324676,66.8029289824295,67.8017654323914,
68.8006018823532,69.7994383323151,70.798274782277,71.7971112322389,72.7959476822007,
73.7947841321626,74.7936205821245,75.7924570320864,76.7912934820482,77.7901299320101,
78.788966381972,79.7878028319339,80.7866392818957,81.7854757318576,82.7843121818195,
83.7831486317814,84.7819850817432,85.7808215317051,86.779657981667,87.7784944316288,
88.7773308815907,89.7761673315526,90.7750037815145,91.7738402314764,92.7726766814382,
93.7715131314001,94.770349581362,95.7691860313238,96.7680224812857,97.7668589312476,
98.7656953812095,99.7645318311714,100.763368281133,101.762204731095,102.761041181057,
103.759877631019,104.758714080981,105.757550530943,106.756386980904,107.755223430866,
108.754059880828,109.75289633079,110.751732780752,111.750569230714,112.749405680676,
113.748242130638,114.747078580599,115.745915030561,116.744751480523,117.743587930485,
118.742424380447,119.741260830409,120.740097280371,121.738933730333,122.737770180294,
123.736606630256,124.735443080218,125.73427953018,126.733115980142,127.731952430104,
128.730788880066,129.729625330028,130.728461779989,131.727298229951,132.726134679913,
133.724971129875,134.723807579837,135.722644029799,136.721480479761,137.720316929723,
138.719153379684,139.717989829646,140.716826279608,141.71566272957,142.714499179532,
143.713335629494,144.712172079456,145.711008529418,146.709844979379,147.708681429341,
148.707517879303,149.706354329265,150.705190779227,151.704027229189,152.702863679151,
153.701700129113,154.700536579074,155.699373029036,156.698209478998,157.69704592896,
158.695882378922,159.694718828884,160.693555278846,161.692391728808,162.691228178769,
163.690064628731,164.688901078693,165.687737528655,166.686573978617,167.685410428579,
168.684246878541,169.683083328503,170.681919778464,171.680756228426,172.679592678388,
173.67842912835,174.677265578312,175.676102028274,176.674938478236,177.673774928198,
178.672611378159,179.671447828121,180.670284278083,181.669120728045,182.667957178007,
183.666793627969,184.665630077931,185.664466527893,186.663302977854),
 .UNSPECIFIED.);
#154=B_SPLINE_SURFACE_WITH_KNOTS('',3,3,((#118442,#118443,#118444,#118445,
#118446,#118447,#118448,#118449,#118450,#118451,#118452,#118453,#118454,
#118455,#118456,#118457,#118458,#118459,#118460,#118461,#118462,#118463,
#118464,#118465,#118466,#118467,#118468,#118469,#118470,#118471,#118472,
#118473,#118474,#118475,#118476,#118477,#118478,#118479,#118480,#118481,
#118482,#118483,#118484,#118485,#118486,#118487,#118488,#118489,#118490,
#118491,#118492,#118493,#118494,#118495,#118496,#118497,#118498,#118499,
#118500,#118501,#118502,#118503,#118504,#118505,#118506,#118507,#118508,
#118509,#118510,#118511,#118512,#118513,#118514,#118515,#118516,#118517,
#118518,#118519,#118520,#118521,#118522,#118523,#118524,#118525,#118526,
#118527,#118528,#118529,#118530,#118531,#118532,#118533,#118534,#118535,
#118536,#118537,#118538,#118539,#118540,#118541,#118542,#118543,#118544,
#118545,#118546,#118547,#118548,#118549,#118550,#118551,#118552,#118553,
#118554,#118555,#118556,#118557,#118558,#118559,#118560,#118561,#118562,
#118563,#118564,#118565,#118566,#118567,#118568,#118569,#118570,#118571,
#118572,#118573,#118574,#118575,#118576,#118577,#118578,#118579,#118580,
#118581,#118582,#118583,#118584,#118585,#118586,#118587,#118588,#118589,
#118590,#118591,#118592,#118593,#118594,#118595,#118596,#118597,#118598,
#118599,#118600,#118601,#118602,#118603,#118604,#118605,#118606,#118607,
#118608,#118609,#118610,#118611,#118612,#118613,#118614,#118615,#118616,
#118617,#118618,#118619),(#118620,#118621,#118622,#118623,#118624,#118625,
#118626,#118627,#118628,#118629,#118630,#118631,#118632,#118633,#118634,
#118635,#118636,#118637,#118638,#118639,#118640,#118641,#118642,#118643,
#118644,#118645,#118646,#118647,#118648,#118649,#118650,#118651,#118652,
#118653,#118654,#118655,#118656,#118657,#118658,#118659,#118660,#118661,
#118662,#118663,#118664,#118665,#118666,#118667,#118668,#118669,#118670,
#118671,#118672,#118673,#118674,#118675,#118676,#118677,#118678,#118679,
#118680,#118681,#118682,#118683,#118684,#118685,#118686,#118687,#118688,
#118689,#118690,#118691,#118692,#118693,#118694,#118695,#118696,#118697,
#118698,#118699,#118700,#118701,#118702,#118703,#118704,#118705,#118706,
#118707,#118708,#118709,#118710,#118711,#118712,#118713,#118714,#118715,
#118716,#118717,#118718,#118719,#118720,#118721,#118722,#118723,#118724,
#118725,#118726,#118727,#118728,#118729,#118730,#118731,#118732,#118733,
#118734,#118735,#118736,#118737,#118738,#118739,#118740,#118741,#118742,
#118743,#118744,#118745,#118746,#118747,#118748,#118749,#118750,#118751,
#118752,#118753,#118754,#118755,#118756,#118757,#118758,#118759,#118760,
#118761,#118762,#118763,#118764,#118765,#118766,#118767,#118768,#118769,
#118770,#118771,#118772,#118773,#118774,#118775,#118776,#118777,#118778,
#118779,#118780,#118781,#118782,#118783,#118784,#118785,#118786,#118787,
#118788,#118789,#118790,#118791,#118792,#118793,#118794,#118795,#118796,
#118797),(#118798,#118799,#118800,#118801,#118802,#118803,#118804,#118805,
#118806,#118807,#118808,#118809,#118810,#118811,#118812,#118813,#118814,
#118815,#118816,#118817,#118818,#118819,#118820,#118821,#118822,#118823,
#118824,#118825,#118826,#118827,#118828,#118829,#118830,#118831,#118832,
#118833,#118834,#118835,#118836,#118837,#118838,#118839,#118840,#118841,
#118842,#118843,#118844,#118845,#118846,#118847,#118848,#118849,#118850,
#118851,#118852,#118853,#118854,#118855,#118856,#118857,#118858,#118859,
#118860,#118861,#118862,#118863,#118864,#118865,#118866,#118867,#118868,
#118869,#118870,#118871,#118872,#118873,#118874,#118875,#118876,#118877,
#118878,#118879,#118880,#118881,#118882,#118883,#118884,#118885,#118886,
#118887,#118888,#118889,#118890,#118891,#118892,#118893,#118894,#118895,
#118896,#118897,#118898,#118899,#118900,#118901,#118902,#118903,#118904,
#118905,#118906,#118907,#118908,#118909,#118910,#118911,#118912,#118913,
#118914,#118915,#118916,#118917,#118918,#118919,#118920,#118921,#118922,
#118923,#118924,#118925,#118926,#118927,#118928,#118929,#118930,#118931,
#118932,#118933,#118934,#118935,#118936,#118937,#118938,#118939,#118940,
#118941,#118942,#118943,#118944,#118945,#118946,#118947,#118948,#118949,
#118950,#118951,#118952,#118953,#118954,#118955,#118956,#118957,#118958,
#118959,#118960,#118961,#118962,#118963,#118964,#118965,#118966,#118967,
#118968,#118969,#118970,#118971,#118972,#118973,#118974,#118975),(#118976,
#118977,#118978,#118979,#118980,#118981,#118982,#118983,#118984,#118985,
#118986,#118987,#118988,#118989,#118990,#118991,#118992,#118993,#118994,
#118995,#118996,#118997,#118998,#118999,#119000,#119001,#119002,#119003,
#119004,#119005,#119006,#119007,#119008,#119009,#119010,#119011,#119012,
#119013,#119014,#119015,#119016,#119017,#119018,#119019,#119020,#119021,
#119022,#119023,#119024,#119025,#119026,#119027,#119028,#119029,#119030,
#119031,#119032,#119033,#119034,#119035,#119036,#119037,#119038,#119039,
#119040,#119041,#119042,#119043,#119044,#119045,#119046,#119047,#119048,
#119049,#119050,#119051,#119052,#119053,#119054,#119055,#119056,#119057,
#119058,#119059,#119060,#119061,#119062,#119063,#119064,#119065,#119066,
#119067,#119068,#119069,#119070,#119071,#119072,#119073,#119074,#119075,
#119076,#119077,#119078,#119079,#119080,#119081,#119082,#119083,#119084,
#119085,#119086,#119087,#119088,#119089,#119090,#119091,#119092,#119093,
#119094,#119095,#119096,#119097,#119098,#119099,#119100,#119101,#119102,
#119103,#119104,#119105,#119106,#119107,#119108,#119109,#119110,#119111,
#119112,#119113,#119114,#119115,#119116,#119117,#119118,#119119,#119120,
#119121,#119122,#119123,#119124,#119125,#119126,#119127,#119128,#119129,
#119130,#119131,#119132,#119133,#119134,#119135,#119136,#119137,#119138,
#119139,#119140,#119141,#119142,#119143,#119144,#119145,#119146,#119147,
#119148,#119149,#119150,#119151,#119152,#119153)),.UNSPECIFIED.,.F.,.F.,
 .F.,(4,4),(4,1,1,1,1,1,1,1,1,1,1,1,1,1,1,1,1,1,1,1,1,1,1,1,1,1,1,1,1,1,
1,1,1,1,1,1,1,1,1,1,1,1,1,1,1,1,1,1,1,1,1,1,1,1,1,1,1,1,1,1,1,1,1,1,1,1,
1,1,1,1,1,1,1,1,1,1,1,1,1,1,1,1,1,1,1,1,1,1,1,1,1,1,1,1,1,1,1,1,1,1,1,1,
1,1,1,1,1,1,1,1,1,1,1,1,1,1,1,1,1,1,1,1,1,1,1,1,1,1,1,1,1,1,1,1,1,1,1,1,
1,1,1,1,1,1,1,1,1,1,1,1,1,1,1,1,1,1,1,1,1,1,1,1,1,1,1,1,1,1,1,1,1,1,1,1,
1,4),(-0.000378201108639058,0.051592837406338),(14.3986268518925,15.3974633018543,
16.3962997518162,17.3951362017781,18.39397265174,19.3928091017018,20.3916455516637,
21.3904820016256,22.3893184515875,23.3881549015493,24.3869913515112,25.3858278014731,
26.3846642514349,27.3835007013968,28.3823371513587,29.3811736013206,30.3800100512824,
31.3788465012443,32.3776829512062,33.3765194011681,34.3753558511299,35.3741923010918,
36.3730287510537,37.3718652010156,38.3707016509774,39.3695381009393,40.3683745509012,
41.3672110008631,42.3660474508249,43.3648839007868,44.3637203507487,45.3625568007106,
46.3613932506724,47.3602297006343,48.3590661505962,49.3579026005581,50.3567390505199,
51.3555755004818,52.3544119504437,53.3532484004055,54.3520848503674,55.3509213003293,
56.3497577502912,57.348594200253,58.3474306502149,59.3462671001768,60.3451035501387,
61.3439400001005,62.3427764500624,63.3416129000243,64.3404493499862,65.339285799948,
66.3381222499099,67.3369586998718,68.3357951498337,69.3346315997955,70.3334680497574,
71.3323044997193,72.3311409496812,73.329977399643,74.3288138496049,75.3276502995668,
76.3264867495287,77.3253231994905,78.3241596494524,79.3229960994143,80.3218325493762,
81.320668999338,82.3195054492999,83.3183418992618,84.3171783492237,85.3160147991855,
86.3148512491474,87.3136876991093,88.3125241490712,89.311360599033,90.3101970489949,
91.3090334989568,92.3078699489186,93.3067063988805,94.3055428488424,95.3043792988043,
96.3032157487661,97.302052198728,98.3008886486899,99.2997250986518,100.298561548614,
101.297397998576,102.296234448537,103.295070898499,104.293907348461,105.292743798423,
106.291580248385,107.290416698347,108.289253148309,109.288089598271,110.286926048232,
111.285762498194,112.284598948156,113.283435398118,114.28227184808,115.281108298042,
116.279944748004,117.278781197966,118.277617647927,119.276454097889,120.275290547851,
121.274126997813,122.272963447775,123.271799897737,124.270636347699,125.26947279766,
126.268309247622,127.267145697584,128.265982147546,129.264818597508,130.26365504747,
131.262491497432,132.261327947394,133.260164397355,134.259000847317,135.257837297279,
136.256673747241,137.255510197203,138.254346647165,139.253183097127,140.252019547089,
141.25085599705,142.249692447012,143.248528896974,144.247365346936,145.246201796898,
146.24503824686,147.243874696822,148.242711146784,149.241547596745,150.240384046707,
151.239220496669,152.238056946631,153.236893396593,154.235729846555,155.234566296517,
156.233402746479,157.23223919644,158.231075646402,159.229912096364,160.228748546326,
161.227584996288,162.22642144625,163.225257896212,164.224094346174,165.222930796135,
166.221767246097,167.220603696059,168.219440146021,169.218276595983,170.217113045945,
171.215949495907,172.214785945869,173.21362239583,174.212458845792,175.211295295754,
176.210131745716,177.208968195678,178.20780464564,179.206641095602,180.205477545564,
181.204313995525,182.203150445487,183.201986895449,184.200823345411,185.199659795373,
186.198496245335,187.197332695297,188.196169145259,189.195445198776),
 .UNSPECIFIED.);
#155=B_SPLINE_SURFACE_WITH_KNOTS('',3,3,((#119245,#119246,#119247,#119248,
#119249,#119250,#119251,#119252,#119253,#119254,#119255,#119256,#119257,
#119258,#119259,#119260,#119261,#119262,#119263,#119264,#119265,#119266,
#119267,#119268,#119269,#119270,#119271,#119272,#119273,#119274,#119275,
#119276,#119277,#119278,#119279,#119280,#119281,#119282,#119283,#119284,
#119285,#119286,#119287,#119288,#119289,#119290,#119291,#119292,#119293,
#119294,#119295,#119296,#119297,#119298,#119299,#119300,#119301,#119302,
#119303,#119304,#119305,#119306,#119307,#119308,#119309,#119310,#119311,
#119312,#119313,#119314,#119315,#119316,#119317,#119318,#119319,#119320,
#119321,#119322,#119323,#119324,#119325,#119326,#119327,#119328,#119329,
#119330,#119331,#119332,#119333,#119334,#119335,#119336,#119337,#119338,
#119339,#119340,#119341,#119342,#119343,#119344,#119345,#119346,#119347,
#119348,#119349,#119350,#119351,#119352,#119353,#119354,#119355,#119356,
#119357,#119358,#119359,#119360,#119361,#119362,#119363,#119364,#119365,
#119366,#119367,#119368,#119369,#119370,#119371,#119372,#119373,#119374,
#119375,#119376,#119377,#119378,#119379,#119380,#119381,#119382,#119383,
#119384,#119385,#119386,#119387,#119388,#119389,#119390,#119391,#119392,
#119393,#119394,#119395,#119396,#119397,#119398,#119399,#119400,#119401,
#119402,#119403,#119404,#119405,#119406,#119407,#119408,#119409,#119410,
#119411,#119412,#119413,#119414,#119415,#119416,#119417,#119418,#119419,
#119420,#119421,#119422),(#119423,#119424,#119425,#119426,#119427,#119428,
#119429,#119430,#119431,#119432,#119433,#119434,#119435,#119436,#119437,
#119438,#119439,#119440,#119441,#119442,#119443,#119444,#119445,#119446,
#119447,#119448,#119449,#119450,#119451,#119452,#119453,#119454,#119455,
#119456,#119457,#119458,#119459,#119460,#119461,#119462,#119463,#119464,
#119465,#119466,#119467,#119468,#119469,#119470,#119471,#119472,#119473,
#119474,#119475,#119476,#119477,#119478,#119479,#119480,#119481,#119482,
#119483,#119484,#119485,#119486,#119487,#119488,#119489,#119490,#119491,
#119492,#119493,#119494,#119495,#119496,#119497,#119498,#119499,#119500,
#119501,#119502,#119503,#119504,#119505,#119506,#119507,#119508,#119509,
#119510,#119511,#119512,#119513,#119514,#119515,#119516,#119517,#119518,
#119519,#119520,#119521,#119522,#119523,#119524,#119525,#119526,#119527,
#119528,#119529,#119530,#119531,#119532,#119533,#119534,#119535,#119536,
#119537,#119538,#119539,#119540,#119541,#119542,#119543,#119544,#119545,
#119546,#119547,#119548,#119549,#119550,#119551,#119552,#119553,#119554,
#119555,#119556,#119557,#119558,#119559,#119560,#119561,#119562,#119563,
#119564,#119565,#119566,#119567,#119568,#119569,#119570,#119571,#119572,
#119573,#119574,#119575,#119576,#119577,#119578,#119579,#119580,#119581,
#119582,#119583,#119584,#119585,#119586,#119587,#119588,#119589,#119590,
#119591,#119592,#119593,#119594,#119595,#119596,#119597,#119598,#119599,
#119600),(#119601,#119602,#119603,#119604,#119605,#119606,#119607,#119608,
#119609,#119610,#119611,#119612,#119613,#119614,#119615,#119616,#119617,
#119618,#119619,#119620,#119621,#119622,#119623,#119624,#119625,#119626,
#119627,#119628,#119629,#119630,#119631,#119632,#119633,#119634,#119635,
#119636,#119637,#119638,#119639,#119640,#119641,#119642,#119643,#119644,
#119645,#119646,#119647,#119648,#119649,#119650,#119651,#119652,#119653,
#119654,#119655,#119656,#119657,#119658,#119659,#119660,#119661,#119662,
#119663,#119664,#119665,#119666,#119667,#119668,#119669,#119670,#119671,
#119672,#119673,#119674,#119675,#119676,#119677,#119678,#119679,#119680,
#119681,#119682,#119683,#119684,#119685,#119686,#119687,#119688,#119689,
#119690,#119691,#119692,#119693,#119694,#119695,#119696,#119697,#119698,
#119699,#119700,#119701,#119702,#119703,#119704,#119705,#119706,#119707,
#119708,#119709,#119710,#119711,#119712,#119713,#119714,#119715,#119716,
#119717,#119718,#119719,#119720,#119721,#119722,#119723,#119724,#119725,
#119726,#119727,#119728,#119729,#119730,#119731,#119732,#119733,#119734,
#119735,#119736,#119737,#119738,#119739,#119740,#119741,#119742,#119743,
#119744,#119745,#119746,#119747,#119748,#119749,#119750,#119751,#119752,
#119753,#119754,#119755,#119756,#119757,#119758,#119759,#119760,#119761,
#119762,#119763,#119764,#119765,#119766,#119767,#119768,#119769,#119770,
#119771,#119772,#119773,#119774,#119775,#119776,#119777,#119778),(#119779,
#119780,#119781,#119782,#119783,#119784,#119785,#119786,#119787,#119788,
#119789,#119790,#119791,#119792,#119793,#119794,#119795,#119796,#119797,
#119798,#119799,#119800,#119801,#119802,#119803,#119804,#119805,#119806,
#119807,#119808,#119809,#119810,#119811,#119812,#119813,#119814,#119815,
#119816,#119817,#119818,#119819,#119820,#119821,#119822,#119823,#119824,
#119825,#119826,#119827,#119828,#119829,#119830,#119831,#119832,#119833,
#119834,#119835,#119836,#119837,#119838,#119839,#119840,#119841,#119842,
#119843,#119844,#119845,#119846,#119847,#119848,#119849,#119850,#119851,
#119852,#119853,#119854,#119855,#119856,#119857,#119858,#119859,#119860,
#119861,#119862,#119863,#119864,#119865,#119866,#119867,#119868,#119869,
#119870,#119871,#119872,#119873,#119874,#119875,#119876,#119877,#119878,
#119879,#119880,#119881,#119882,#119883,#119884,#119885,#119886,#119887,
#119888,#119889,#119890,#119891,#119892,#119893,#119894,#119895,#119896,
#119897,#119898,#119899,#119900,#119901,#119902,#119903,#119904,#119905,
#119906,#119907,#119908,#119909,#119910,#119911,#119912,#119913,#119914,
#119915,#119916,#119917,#119918,#119919,#119920,#119921,#119922,#119923,
#119924,#119925,#119926,#119927,#119928,#119929,#119930,#119931,#119932,
#119933,#119934,#119935,#119936,#119937,#119938,#119939,#119940,#119941,
#119942,#119943,#119944,#119945,#119946,#119947,#119948,#119949,#119950,
#119951,#119952,#119953,#119954,#119955,#119956)),.UNSPECIFIED.,.F.,.F.,
 .F.,(4,4),(4,1,1,1,1,1,1,1,1,1,1,1,1,1,1,1,1,1,1,1,1,1,1,1,1,1,1,1,1,1,
1,1,1,1,1,1,1,1,1,1,1,1,1,1,1,1,1,1,1,1,1,1,1,1,1,1,1,1,1,1,1,1,1,1,1,1,
1,1,1,1,1,1,1,1,1,1,1,1,1,1,1,1,1,1,1,1,1,1,1,1,1,1,1,1,1,1,1,1,1,1,1,1,
1,1,1,1,1,1,1,1,1,1,1,1,1,1,1,1,1,1,1,1,1,1,1,1,1,1,1,1,1,1,1,1,1,1,1,1,
1,1,1,1,1,1,1,1,1,1,1,1,1,1,1,1,1,1,1,1,1,1,1,1,1,1,1,1,1,1,1,1,1,1,1,1,
1,4),(-0.000439572862182687,0.0515314610720387),(11.8664846616642,12.8657606844883,
13.8645971344502,14.8634335844121,15.8622700343739,16.8611064843358,17.8599429342977,
18.8587793842595,19.8576158342214,20.8564522841833,21.8552887341452,22.854125184107,
23.8529616340689,24.8517980840308,25.8506345339927,26.8494709839545,27.8483074339164,
28.8471438838783,29.8459803338402,30.844816783802,31.8436532337639,32.8424896837258,
33.8413261336877,34.8401625836495,35.8389990336114,36.8378354835733,37.8366719335352,
38.835508383497,39.8343448334589,40.8331812834208,41.8320177333826,42.8308541833445,
43.8296906333064,44.8285270832683,45.8273635332301,46.826199983192,47.8250364331539,
48.8238728831158,49.8227093330776,50.8215457830395,51.8203822330014,52.8192186829633,
53.8180551329251,54.816891582887,55.8157280328489,56.8145644828108,57.8134009327726,
58.8122373827345,59.8110738326964,60.8099102826583,61.8087467326201,62.807583182582,
63.8064196325439,64.8052560825058,65.8040925324676,66.8029289824295,67.8017654323914,
68.8006018823532,69.7994383323151,70.798274782277,71.7971112322389,72.7959476822007,
73.7947841321626,74.7936205821245,75.7924570320864,76.7912934820482,77.7901299320101,
78.788966381972,79.7878028319339,80.7866392818957,81.7854757318576,82.7843121818195,
83.7831486317814,84.7819850817432,85.7808215317051,86.779657981667,87.7784944316289,
88.7773308815907,89.7761673315526,90.7750037815145,91.7738402314764,92.7726766814382,
93.7715131314001,94.770349581362,95.7691860313239,96.7680224812857,97.7668589312476,
98.7656953812095,99.7645318311714,100.763368281133,101.762204731095,102.761041181057,
103.759877631019,104.758714080981,105.757550530943,106.756386980904,107.755223430866,
108.754059880828,109.75289633079,110.751732780752,111.750569230714,112.749405680676,
113.748242130638,114.747078580599,115.745915030561,116.744751480523,117.743587930485,
118.742424380447,119.741260830409,120.740097280371,121.738933730333,122.737770180294,
123.736606630256,124.735443080218,125.73427953018,126.733115980142,127.731952430104,
128.730788880066,129.729625330028,130.728461779989,131.727298229951,132.726134679913,
133.724971129875,134.723807579837,135.722644029799,136.721480479761,137.720316929723,
138.719153379684,139.717989829646,140.716826279608,141.71566272957,142.714499179532,
143.713335629494,144.712172079456,145.711008529418,146.709844979379,147.708681429341,
148.707517879303,149.706354329265,150.705190779227,151.704027229189,152.702863679151,
153.701700129113,154.700536579074,155.699373029036,156.698209478998,157.69704592896,
158.695882378922,159.694718828884,160.693555278846,161.692391728808,162.691228178769,
163.690064628731,164.688901078693,165.687737528655,166.686573978617,167.685410428579,
168.684246878541,169.683083328503,170.681919778464,171.680756228426,172.679592678388,
173.67842912835,174.677265578312,175.676102028274,176.674938478236,177.673774928198,
178.672611378159,179.671447828121,180.670284278083,181.669120728045,182.667957178007,
183.666793627969,184.665630077931,185.664466527893,186.663302977854),
 .UNSPECIFIED.);
#156=B_SPLINE_SURFACE_WITH_KNOTS('',3,3,((#120045,#120046,#120047,#120048,
#120049,#120050,#120051,#120052,#120053,#120054,#120055,#120056,#120057,
#120058,#120059,#120060,#120061,#120062,#120063,#120064,#120065,#120066,
#120067,#120068,#120069,#120070,#120071,#120072,#120073,#120074,#120075,
#120076,#120077,#120078,#120079,#120080,#120081,#120082,#120083,#120084,
#120085,#120086,#120087,#120088,#120089,#120090,#120091,#120092,#120093,
#120094,#120095,#120096,#120097,#120098,#120099,#120100,#120101,#120102,
#120103,#120104,#120105,#120106,#120107,#120108,#120109,#120110,#120111,
#120112,#120113,#120114,#120115,#120116,#120117,#120118,#120119,#120120,
#120121,#120122,#120123,#120124,#120125,#120126,#120127,#120128,#120129,
#120130,#120131,#120132,#120133,#120134,#120135,#120136,#120137,#120138,
#120139,#120140,#120141,#120142,#120143,#120144,#120145,#120146,#120147,
#120148,#120149,#120150,#120151,#120152,#120153,#120154,#120155,#120156,
#120157,#120158,#120159,#120160,#120161,#120162,#120163,#120164,#120165,
#120166,#120167,#120168,#120169,#120170,#120171,#120172,#120173,#120174,
#120175,#120176,#120177,#120178,#120179,#120180,#120181,#120182,#120183,
#120184,#120185,#120186,#120187,#120188,#120189,#120190,#120191,#120192,
#120193,#120194,#120195,#120196,#120197,#120198,#120199,#120200,#120201,
#120202,#120203,#120204,#120205,#120206,#120207,#120208,#120209,#120210,
#120211,#120212,#120213,#120214,#120215,#120216,#120217,#120218,#120219,
#120220,#120221,#120222),(#120223,#120224,#120225,#120226,#120227,#120228,
#120229,#120230,#120231,#120232,#120233,#120234,#120235,#120236,#120237,
#120238,#120239,#120240,#120241,#120242,#120243,#120244,#120245,#120246,
#120247,#120248,#120249,#120250,#120251,#120252,#120253,#120254,#120255,
#120256,#120257,#120258,#120259,#120260,#120261,#120262,#120263,#120264,
#120265,#120266,#120267,#120268,#120269,#120270,#120271,#120272,#120273,
#120274,#120275,#120276,#120277,#120278,#120279,#120280,#120281,#120282,
#120283,#120284,#120285,#120286,#120287,#120288,#120289,#120290,#120291,
#120292,#120293,#120294,#120295,#120296,#120297,#120298,#120299,#120300,
#120301,#120302,#120303,#120304,#120305,#120306,#120307,#120308,#120309,
#120310,#120311,#120312,#120313,#120314,#120315,#120316,#120317,#120318,
#120319,#120320,#120321,#120322,#120323,#120324,#120325,#120326,#120327,
#120328,#120329,#120330,#120331,#120332,#120333,#120334,#120335,#120336,
#120337,#120338,#120339,#120340,#120341,#120342,#120343,#120344,#120345,
#120346,#120347,#120348,#120349,#120350,#120351,#120352,#120353,#120354,
#120355,#120356,#120357,#120358,#120359,#120360,#120361,#120362,#120363,
#120364,#120365,#120366,#120367,#120368,#120369,#120370,#120371,#120372,
#120373,#120374,#120375,#120376,#120377,#120378,#120379,#120380,#120381,
#120382,#120383,#120384,#120385,#120386,#120387,#120388,#120389,#120390,
#120391,#120392,#120393,#120394,#120395,#120396,#120397,#120398,#120399,
#120400),(#120401,#120402,#120403,#120404,#120405,#120406,#120407,#120408,
#120409,#120410,#120411,#120412,#120413,#120414,#120415,#120416,#120417,
#120418,#120419,#120420,#120421,#120422,#120423,#120424,#120425,#120426,
#120427,#120428,#120429,#120430,#120431,#120432,#120433,#120434,#120435,
#120436,#120437,#120438,#120439,#120440,#120441,#120442,#120443,#120444,
#120445,#120446,#120447,#120448,#120449,#120450,#120451,#120452,#120453,
#120454,#120455,#120456,#120457,#120458,#120459,#120460,#120461,#120462,
#120463,#120464,#120465,#120466,#120467,#120468,#120469,#120470,#120471,
#120472,#120473,#120474,#120475,#120476,#120477,#120478,#120479,#120480,
#120481,#120482,#120483,#120484,#120485,#120486,#120487,#120488,#120489,
#120490,#120491,#120492,#120493,#120494,#120495,#120496,#120497,#120498,
#120499,#120500,#120501,#120502,#120503,#120504,#120505,#120506,#120507,
#120508,#120509,#120510,#120511,#120512,#120513,#120514,#120515,#120516,
#120517,#120518,#120519,#120520,#120521,#120522,#120523,#120524,#120525,
#120526,#120527,#120528,#120529,#120530,#120531,#120532,#120533,#120534,
#120535,#120536,#120537,#120538,#120539,#120540,#120541,#120542,#120543,
#120544,#120545,#120546,#120547,#120548,#120549,#120550,#120551,#120552,
#120553,#120554,#120555,#120556,#120557,#120558,#120559,#120560,#120561,
#120562,#120563,#120564,#120565,#120566,#120567,#120568,#120569,#120570,
#120571,#120572,#120573,#120574,#120575,#120576,#120577,#120578),(#120579,
#120580,#120581,#120582,#120583,#120584,#120585,#120586,#120587,#120588,
#120589,#120590,#120591,#120592,#120593,#120594,#120595,#120596,#120597,
#120598,#120599,#120600,#120601,#120602,#120603,#120604,#120605,#120606,
#120607,#120608,#120609,#120610,#120611,#120612,#120613,#120614,#120615,
#120616,#120617,#120618,#120619,#120620,#120621,#120622,#120623,#120624,
#120625,#120626,#120627,#120628,#120629,#120630,#120631,#120632,#120633,
#120634,#120635,#120636,#120637,#120638,#120639,#120640,#120641,#120642,
#120643,#120644,#120645,#120646,#120647,#120648,#120649,#120650,#120651,
#120652,#120653,#120654,#120655,#120656,#120657,#120658,#120659,#120660,
#120661,#120662,#120663,#120664,#120665,#120666,#120667,#120668,#120669,
#120670,#120671,#120672,#120673,#120674,#120675,#120676,#120677,#120678,
#120679,#120680,#120681,#120682,#120683,#120684,#120685,#120686,#120687,
#120688,#120689,#120690,#120691,#120692,#120693,#120694,#120695,#120696,
#120697,#120698,#120699,#120700,#120701,#120702,#120703,#120704,#120705,
#120706,#120707,#120708,#120709,#120710,#120711,#120712,#120713,#120714,
#120715,#120716,#120717,#120718,#120719,#120720,#120721,#120722,#120723,
#120724,#120725,#120726,#120727,#120728,#120729,#120730,#120731,#120732,
#120733,#120734,#120735,#120736,#120737,#120738,#120739,#120740,#120741,
#120742,#120743,#120744,#120745,#120746,#120747,#120748,#120749,#120750,
#120751,#120752,#120753,#120754,#120755,#120756)),.UNSPECIFIED.,.F.,.F.,
 .F.,(4,4),(4,1,1,1,1,1,1,1,1,1,1,1,1,1,1,1,1,1,1,1,1,1,1,1,1,1,1,1,1,1,
1,1,1,1,1,1,1,1,1,1,1,1,1,1,1,1,1,1,1,1,1,1,1,1,1,1,1,1,1,1,1,1,1,1,1,1,
1,1,1,1,1,1,1,1,1,1,1,1,1,1,1,1,1,1,1,1,1,1,1,1,1,1,1,1,1,1,1,1,1,1,1,1,
1,1,1,1,1,1,1,1,1,1,1,1,1,1,1,1,1,1,1,1,1,1,1,1,1,1,1,1,1,1,1,1,1,1,1,1,
1,1,1,1,1,1,1,1,1,1,1,1,1,1,1,1,1,1,1,1,1,1,1,1,1,1,1,1,1,1,1,1,1,1,1,1,
1,4),(-0.000378192696996877,0.0515928473073541),(14.3986268518925,15.3974633018543,
16.3962997518162,17.3951362017781,18.39397265174,19.3928091017018,20.3916455516637,
21.3904820016256,22.3893184515875,23.3881549015493,24.3869913515112,25.3858278014731,
26.3846642514349,27.3835007013968,28.3823371513587,29.3811736013206,30.3800100512824,
31.3788465012443,32.3776829512062,33.3765194011681,34.3753558511299,35.3741923010918,
36.3730287510537,37.3718652010156,38.3707016509774,39.3695381009393,40.3683745509012,
41.3672110008631,42.3660474508249,43.3648839007868,44.3637203507487,45.3625568007106,
46.3613932506724,47.3602297006343,48.3590661505962,49.3579026005581,50.3567390505199,
51.3555755004818,52.3544119504437,53.3532484004055,54.3520848503674,55.3509213003293,
56.3497577502912,57.348594200253,58.3474306502149,59.3462671001768,60.3451035501387,
61.3439400001005,62.3427764500624,63.3416129000243,64.3404493499862,65.339285799948,
66.3381222499099,67.3369586998718,68.3357951498337,69.3346315997955,70.3334680497574,
71.3323044997193,72.3311409496812,73.329977399643,74.3288138496049,75.3276502995668,
76.3264867495287,77.3253231994905,78.3241596494524,79.3229960994143,80.3218325493762,
81.320668999338,82.3195054492999,83.3183418992618,84.3171783492237,85.3160147991855,
86.3148512491474,87.3136876991093,88.3125241490712,89.311360599033,90.3101970489949,
91.3090334989568,92.3078699489186,93.3067063988805,94.3055428488424,95.3043792988043,
96.3032157487661,97.302052198728,98.3008886486899,99.2997250986518,100.298561548614,
101.297397998576,102.296234448537,103.295070898499,104.293907348461,105.292743798423,
106.291580248385,107.290416698347,108.289253148309,109.288089598271,110.286926048232,
111.285762498194,112.284598948156,113.283435398118,114.28227184808,115.281108298042,
116.279944748004,117.278781197966,118.277617647927,119.276454097889,120.275290547851,
121.274126997813,122.272963447775,123.271799897737,124.270636347699,125.26947279766,
126.268309247622,127.267145697584,128.265982147546,129.264818597508,130.26365504747,
131.262491497432,132.261327947394,133.260164397355,134.259000847317,135.257837297279,
136.256673747241,137.255510197203,138.254346647165,139.253183097127,140.252019547089,
141.25085599705,142.249692447012,143.248528896974,144.247365346936,145.246201796898,
146.24503824686,147.243874696822,148.242711146784,149.241547596745,150.240384046707,
151.239220496669,152.238056946631,153.236893396593,154.235729846555,155.234566296517,
156.233402746479,157.23223919644,158.231075646402,159.229912096364,160.228748546326,
161.227584996288,162.22642144625,163.225257896212,164.224094346174,165.222930796135,
166.221767246097,167.220603696059,168.219440146021,169.218276595983,170.217113045945,
171.215949495907,172.214785945869,173.21362239583,174.212458845792,175.211295295754,
176.210131745716,177.208968195678,178.20780464564,179.206641095602,180.205477545564,
181.204313995525,182.203150445487,183.201986895449,184.200823345411,185.199659795373,
186.198496245335,187.197332695297,188.196169145259,189.195445208677),
 .UNSPECIFIED.);
#157=B_SPLINE_SURFACE_WITH_KNOTS('',3,3,((#120845,#120846,#120847,#120848,
#120849,#120850,#120851,#120852,#120853,#120854,#120855,#120856,#120857,
#120858,#120859,#120860,#120861,#120862,#120863,#120864,#120865,#120866,
#120867,#120868,#120869,#120870,#120871,#120872,#120873,#120874,#120875,
#120876,#120877,#120878,#120879,#120880,#120881,#120882,#120883,#120884,
#120885,#120886,#120887,#120888,#120889,#120890,#120891,#120892,#120893,
#120894,#120895,#120896,#120897,#120898,#120899,#120900,#120901,#120902,
#120903,#120904,#120905,#120906,#120907,#120908,#120909,#120910,#120911,
#120912,#120913,#120914,#120915,#120916,#120917,#120918,#120919,#120920,
#120921,#120922,#120923,#120924,#120925,#120926,#120927,#120928,#120929,
#120930,#120931,#120932,#120933,#120934,#120935,#120936,#120937,#120938,
#120939,#120940,#120941,#120942,#120943,#120944,#120945,#120946,#120947,
#120948,#120949,#120950,#120951,#120952,#120953,#120954,#120955,#120956,
#120957,#120958,#120959,#120960,#120961,#120962,#120963,#120964,#120965,
#120966,#120967,#120968,#120969,#120970,#120971,#120972,#120973,#120974,
#120975,#120976,#120977,#120978,#120979,#120980,#120981,#120982,#120983,
#120984,#120985,#120986,#120987,#120988,#120989,#120990,#120991,#120992,
#120993,#120994,#120995,#120996,#120997,#120998,#120999,#121000,#121001,
#121002,#121003,#121004,#121005,#121006,#121007,#121008,#121009,#121010,
#121011,#121012,#121013,#121014,#121015,#121016,#121017,#121018,#121019,
#121020,#121021,#121022),(#121023,#121024,#121025,#121026,#121027,#121028,
#121029,#121030,#121031,#121032,#121033,#121034,#121035,#121036,#121037,
#121038,#121039,#121040,#121041,#121042,#121043,#121044,#121045,#121046,
#121047,#121048,#121049,#121050,#121051,#121052,#121053,#121054,#121055,
#121056,#121057,#121058,#121059,#121060,#121061,#121062,#121063,#121064,
#121065,#121066,#121067,#121068,#121069,#121070,#121071,#121072,#121073,
#121074,#121075,#121076,#121077,#121078,#121079,#121080,#121081,#121082,
#121083,#121084,#121085,#121086,#121087,#121088,#121089,#121090,#121091,
#121092,#121093,#121094,#121095,#121096,#121097,#121098,#121099,#121100,
#121101,#121102,#121103,#121104,#121105,#121106,#121107,#121108,#121109,
#121110,#121111,#121112,#121113,#121114,#121115,#121116,#121117,#121118,
#121119,#121120,#121121,#121122,#121123,#121124,#121125,#121126,#121127,
#121128,#121129,#121130,#121131,#121132,#121133,#121134,#121135,#121136,
#121137,#121138,#121139,#121140,#121141,#121142,#121143,#121144,#121145,
#121146,#121147,#121148,#121149,#121150,#121151,#121152,#121153,#121154,
#121155,#121156,#121157,#121158,#121159,#121160,#121161,#121162,#121163,
#121164,#121165,#121166,#121167,#121168,#121169,#121170,#121171,#121172,
#121173,#121174,#121175,#121176,#121177,#121178,#121179,#121180,#121181,
#121182,#121183,#121184,#121185,#121186,#121187,#121188,#121189,#121190,
#121191,#121192,#121193,#121194,#121195,#121196,#121197,#121198,#121199,
#121200),(#121201,#121202,#121203,#121204,#121205,#121206,#121207,#121208,
#121209,#121210,#121211,#121212,#121213,#121214,#121215,#121216,#121217,
#121218,#121219,#121220,#121221,#121222,#121223,#121224,#121225,#121226,
#121227,#121228,#121229,#121230,#121231,#121232,#121233,#121234,#121235,
#121236,#121237,#121238,#121239,#121240,#121241,#121242,#121243,#121244,
#121245,#121246,#121247,#121248,#121249,#121250,#121251,#121252,#121253,
#121254,#121255,#121256,#121257,#121258,#121259,#121260,#121261,#121262,
#121263,#121264,#121265,#121266,#121267,#121268,#121269,#121270,#121271,
#121272,#121273,#121274,#121275,#121276,#121277,#121278,#121279,#121280,
#121281,#121282,#121283,#121284,#121285,#121286,#121287,#121288,#121289,
#121290,#121291,#121292,#121293,#121294,#121295,#121296,#121297,#121298,
#121299,#121300,#121301,#121302,#121303,#121304,#121305,#121306,#121307,
#121308,#121309,#121310,#121311,#121312,#121313,#121314,#121315,#121316,
#121317,#121318,#121319,#121320,#121321,#121322,#121323,#121324,#121325,
#121326,#121327,#121328,#121329,#121330,#121331,#121332,#121333,#121334,
#121335,#121336,#121337,#121338,#121339,#121340,#121341,#121342,#121343,
#121344,#121345,#121346,#121347,#121348,#121349,#121350,#121351,#121352,
#121353,#121354,#121355,#121356,#121357,#121358,#121359,#121360,#121361,
#121362,#121363,#121364,#121365,#121366,#121367,#121368,#121369,#121370,
#121371,#121372,#121373,#121374,#121375,#121376,#121377,#121378),(#121379,
#121380,#121381,#121382,#121383,#121384,#121385,#121386,#121387,#121388,
#121389,#121390,#121391,#121392,#121393,#121394,#121395,#121396,#121397,
#121398,#121399,#121400,#121401,#121402,#121403,#121404,#121405,#121406,
#121407,#121408,#121409,#121410,#121411,#121412,#121413,#121414,#121415,
#121416,#121417,#121418,#121419,#121420,#121421,#121422,#121423,#121424,
#121425,#121426,#121427,#121428,#121429,#121430,#121431,#121432,#121433,
#121434,#121435,#121436,#121437,#121438,#121439,#121440,#121441,#121442,
#121443,#121444,#121445,#121446,#121447,#121448,#121449,#121450,#121451,
#121452,#121453,#121454,#121455,#121456,#121457,#121458,#121459,#121460,
#121461,#121462,#121463,#121464,#121465,#121466,#121467,#121468,#121469,
#121470,#121471,#121472,#121473,#121474,#121475,#121476,#121477,#121478,
#121479,#121480,#121481,#121482,#121483,#121484,#121485,#121486,#121487,
#121488,#121489,#121490,#121491,#121492,#121493,#121494,#121495,#121496,
#121497,#121498,#121499,#121500,#121501,#121502,#121503,#121504,#121505,
#121506,#121507,#121508,#121509,#121510,#121511,#121512,#121513,#121514,
#121515,#121516,#121517,#121518,#121519,#121520,#121521,#121522,#121523,
#121524,#121525,#121526,#121527,#121528,#121529,#121530,#121531,#121532,
#121533,#121534,#121535,#121536,#121537,#121538,#121539,#121540,#121541,
#121542,#121543,#121544,#121545,#121546,#121547,#121548,#121549,#121550,
#121551,#121552,#121553,#121554,#121555,#121556)),.UNSPECIFIED.,.F.,.F.,
 .F.,(4,4),(4,1,1,1,1,1,1,1,1,1,1,1,1,1,1,1,1,1,1,1,1,1,1,1,1,1,1,1,1,1,
1,1,1,1,1,1,1,1,1,1,1,1,1,1,1,1,1,1,1,1,1,1,1,1,1,1,1,1,1,1,1,1,1,1,1,1,
1,1,1,1,1,1,1,1,1,1,1,1,1,1,1,1,1,1,1,1,1,1,1,1,1,1,1,1,1,1,1,1,1,1,1,1,
1,1,1,1,1,1,1,1,1,1,1,1,1,1,1,1,1,1,1,1,1,1,1,1,1,1,1,1,1,1,1,1,1,1,1,1,
1,1,1,1,1,1,1,1,1,1,1,1,1,1,1,1,1,1,1,1,1,1,1,1,1,1,1,1,1,1,1,1,1,1,1,1,
1,4),(-0.000439572128271918,0.0515314616970906),(11.8664846623981,12.8657606844883,
13.8645971344502,14.8634335844121,15.8622700343739,16.8611064843358,17.8599429342977,
18.8587793842596,19.8576158342214,20.8564522841833,21.8552887341452,22.854125184107,
23.8529616340689,24.8517980840308,25.8506345339927,26.8494709839545,27.8483074339164,
28.8471438838783,29.8459803338402,30.844816783802,31.8436532337639,32.8424896837258,
33.8413261336877,34.8401625836495,35.8389990336114,36.8378354835733,37.8366719335352,
38.835508383497,39.8343448334589,40.8331812834208,41.8320177333827,42.8308541833445,
43.8296906333064,44.8285270832683,45.8273635332302,46.826199983192,47.8250364331539,
48.8238728831158,49.8227093330777,50.8215457830395,51.8203822330014,52.8192186829633,
53.8180551329252,54.816891582887,55.8157280328489,56.8145644828108,57.8134009327727,
58.8122373827345,59.8110738326964,60.8099102826583,61.8087467326202,62.807583182582,
63.8064196325439,64.8052560825058,65.8040925324676,66.8029289824295,67.8017654323914,
68.8006018823533,69.7994383323151,70.798274782277,71.7971112322389,72.7959476822008,
73.7947841321626,74.7936205821245,75.7924570320864,76.7912934820483,77.7901299320101,
78.788966381972,79.7878028319339,80.7866392818958,81.7854757318576,82.7843121818195,
83.7831486317814,84.7819850817433,85.7808215317051,86.779657981667,87.7784944316289,
88.7773308815908,89.7761673315526,90.7750037815145,91.7738402314764,92.7726766814383,
93.7715131314001,94.770349581362,95.7691860313239,96.7680224812858,97.7668589312476,
98.7656953812095,99.7645318311714,100.763368281133,101.762204731095,102.761041181057,
103.759877631019,104.758714080981,105.757550530943,106.756386980905,107.755223430866,
108.754059880828,109.75289633079,110.751732780752,111.750569230714,112.749405680676,
113.748242130638,114.747078580599,115.745915030561,116.744751480523,117.743587930485,
118.742424380447,119.741260830409,120.740097280371,121.738933730333,122.737770180294,
123.736606630256,124.735443080218,125.73427953018,126.733115980142,127.731952430104,
128.730788880066,129.729625330028,130.728461779989,131.727298229951,132.726134679913,
133.724971129875,134.723807579837,135.722644029799,136.721480479761,137.720316929723,
138.719153379684,139.717989829646,140.716826279608,141.71566272957,142.714499179532,
143.713335629494,144.712172079456,145.711008529418,146.709844979379,147.708681429341,
148.707517879303,149.706354329265,150.705190779227,151.704027229189,152.702863679151,
153.701700129113,154.700536579074,155.699373029036,156.698209478998,157.69704592896,
158.695882378922,159.694718828884,160.693555278846,161.692391728808,162.691228178769,
163.690064628731,164.688901078693,165.687737528655,166.686573978617,167.685410428579,
168.684246878541,169.683083328503,170.681919778464,171.680756228426,172.679592678388,
173.67842912835,174.677265578312,175.676102028274,176.674938478236,177.673774928198,
178.672611378159,179.671447828121,180.670284278083,181.669120728045,182.667957178007,
183.666793627969,184.665630077931,185.664466527893,186.663302977854),
 .UNSPECIFIED.);
#158=B_SPLINE_SURFACE_WITH_KNOTS('',3,3,((#121645,#121646,#121647,#121648,
#121649,#121650,#121651,#121652,#121653,#121654,#121655,#121656,#121657,
#121658,#121659,#121660,#121661,#121662,#121663,#121664,#121665,#121666,
#121667,#121668,#121669,#121670,#121671,#121672,#121673,#121674,#121675,
#121676,#121677,#121678,#121679,#121680,#121681,#121682,#121683,#121684,
#121685,#121686,#121687,#121688,#121689,#121690,#121691,#121692,#121693,
#121694,#121695,#121696,#121697,#121698,#121699,#121700,#121701,#121702,
#121703,#121704,#121705,#121706,#121707,#121708,#121709,#121710,#121711,
#121712,#121713,#121714,#121715,#121716,#121717,#121718,#121719,#121720,
#121721,#121722,#121723,#121724,#121725,#121726,#121727,#121728,#121729,
#121730,#121731,#121732,#121733,#121734,#121735,#121736,#121737,#121738,
#121739,#121740,#121741,#121742,#121743,#121744,#121745,#121746,#121747,
#121748,#121749,#121750,#121751,#121752,#121753,#121754,#121755,#121756,
#121757,#121758,#121759,#121760,#121761,#121762,#121763,#121764,#121765,
#121766,#121767,#121768,#121769,#121770,#121771,#121772,#121773,#121774,
#121775,#121776,#121777,#121778,#121779,#121780,#121781,#121782,#121783,
#121784,#121785,#121786,#121787,#121788,#121789,#121790,#121791,#121792,
#121793,#121794,#121795,#121796,#121797,#121798,#121799,#121800,#121801,
#121802,#121803,#121804,#121805,#121806,#121807,#121808,#121809,#121810,
#121811,#121812,#121813,#121814,#121815,#121816,#121817,#121818,#121819,
#121820,#121821,#121822),(#121823,#121824,#121825,#121826,#121827,#121828,
#121829,#121830,#121831,#121832,#121833,#121834,#121835,#121836,#121837,
#121838,#121839,#121840,#121841,#121842,#121843,#121844,#121845,#121846,
#121847,#121848,#121849,#121850,#121851,#121852,#121853,#121854,#121855,
#121856,#121857,#121858,#121859,#121860,#121861,#121862,#121863,#121864,
#121865,#121866,#121867,#121868,#121869,#121870,#121871,#121872,#121873,
#121874,#121875,#121876,#121877,#121878,#121879,#121880,#121881,#121882,
#121883,#121884,#121885,#121886,#121887,#121888,#121889,#121890,#121891,
#121892,#121893,#121894,#121895,#121896,#121897,#121898,#121899,#121900,
#121901,#121902,#121903,#121904,#121905,#121906,#121907,#121908,#121909,
#121910,#121911,#121912,#121913,#121914,#121915,#121916,#121917,#121918,
#121919,#121920,#121921,#121922,#121923,#121924,#121925,#121926,#121927,
#121928,#121929,#121930,#121931,#121932,#121933,#121934,#121935,#121936,
#121937,#121938,#121939,#121940,#121941,#121942,#121943,#121944,#121945,
#121946,#121947,#121948,#121949,#121950,#121951,#121952,#121953,#121954,
#121955,#121956,#121957,#121958,#121959,#121960,#121961,#121962,#121963,
#121964,#121965,#121966,#121967,#121968,#121969,#121970,#121971,#121972,
#121973,#121974,#121975,#121976,#121977,#121978,#121979,#121980,#121981,
#121982,#121983,#121984,#121985,#121986,#121987,#121988,#121989,#121990,
#121991,#121992,#121993,#121994,#121995,#121996,#121997,#121998,#121999,
#122000),(#122001,#122002,#122003,#122004,#122005,#122006,#122007,#122008,
#122009,#122010,#122011,#122012,#122013,#122014,#122015,#122016,#122017,
#122018,#122019,#122020,#122021,#122022,#122023,#122024,#122025,#122026,
#122027,#122028,#122029,#122030,#122031,#122032,#122033,#122034,#122035,
#122036,#122037,#122038,#122039,#122040,#122041,#122042,#122043,#122044,
#122045,#122046,#122047,#122048,#122049,#122050,#122051,#122052,#122053,
#122054,#122055,#122056,#122057,#122058,#122059,#122060,#122061,#122062,
#122063,#122064,#122065,#122066,#122067,#122068,#122069,#122070,#122071,
#122072,#122073,#122074,#122075,#122076,#122077,#122078,#122079,#122080,
#122081,#122082,#122083,#122084,#122085,#122086,#122087,#122088,#122089,
#122090,#122091,#122092,#122093,#122094,#122095,#122096,#122097,#122098,
#122099,#122100,#122101,#122102,#122103,#122104,#122105,#122106,#122107,
#122108,#122109,#122110,#122111,#122112,#122113,#122114,#122115,#122116,
#122117,#122118,#122119,#122120,#122121,#122122,#122123,#122124,#122125,
#122126,#122127,#122128,#122129,#122130,#122131,#122132,#122133,#122134,
#122135,#122136,#122137,#122138,#122139,#122140,#122141,#122142,#122143,
#122144,#122145,#122146,#122147,#122148,#122149,#122150,#122151,#122152,
#122153,#122154,#122155,#122156,#122157,#122158,#122159,#122160,#122161,
#122162,#122163,#122164,#122165,#122166,#122167,#122168,#122169,#122170,
#122171,#122172,#122173,#122174,#122175,#122176,#122177,#122178),(#122179,
#122180,#122181,#122182,#122183,#122184,#122185,#122186,#122187,#122188,
#122189,#122190,#122191,#122192,#122193,#122194,#122195,#122196,#122197,
#122198,#122199,#122200,#122201,#122202,#122203,#122204,#122205,#122206,
#122207,#122208,#122209,#122210,#122211,#122212,#122213,#122214,#122215,
#122216,#122217,#122218,#122219,#122220,#122221,#122222,#122223,#122224,
#122225,#122226,#122227,#122228,#122229,#122230,#122231,#122232,#122233,
#122234,#122235,#122236,#122237,#122238,#122239,#122240,#122241,#122242,
#122243,#122244,#122245,#122246,#122247,#122248,#122249,#122250,#122251,
#122252,#122253,#122254,#122255,#122256,#122257,#122258,#122259,#122260,
#122261,#122262,#122263,#122264,#122265,#122266,#122267,#122268,#122269,
#122270,#122271,#122272,#122273,#122274,#122275,#122276,#122277,#122278,
#122279,#122280,#122281,#122282,#122283,#122284,#122285,#122286,#122287,
#122288,#122289,#122290,#122291,#122292,#122293,#122294,#122295,#122296,
#122297,#122298,#122299,#122300,#122301,#122302,#122303,#122304,#122305,
#122306,#122307,#122308,#122309,#122310,#122311,#122312,#122313,#122314,
#122315,#122316,#122317,#122318,#122319,#122320,#122321,#122322,#122323,
#122324,#122325,#122326,#122327,#122328,#122329,#122330,#122331,#122332,
#122333,#122334,#122335,#122336,#122337,#122338,#122339,#122340,#122341,
#122342,#122343,#122344,#122345,#122346,#122347,#122348,#122349,#122350,
#122351,#122352,#122353,#122354,#122355,#122356)),.UNSPECIFIED.,.F.,.F.,
 .F.,(4,4),(4,1,1,1,1,1,1,1,1,1,1,1,1,1,1,1,1,1,1,1,1,1,1,1,1,1,1,1,1,1,
1,1,1,1,1,1,1,1,1,1,1,1,1,1,1,1,1,1,1,1,1,1,1,1,1,1,1,1,1,1,1,1,1,1,1,1,
1,1,1,1,1,1,1,1,1,1,1,1,1,1,1,1,1,1,1,1,1,1,1,1,1,1,1,1,1,1,1,1,1,1,1,1,
1,1,1,1,1,1,1,1,1,1,1,1,1,1,1,1,1,1,1,1,1,1,1,1,1,1,1,1,1,1,1,1,1,1,1,1,
1,1,1,1,1,1,1,1,1,1,1,1,1,1,1,1,1,1,1,1,1,1,1,1,1,1,1,1,1,1,1,1,1,1,1,1,
1,4),(-0.000378196170333863,0.0515928432182127),(14.3986268518925,15.3974633018543,
16.3962997518162,17.3951362017781,18.39397265174,19.3928091017018,20.3916455516637,
21.3904820016256,22.3893184515875,23.3881549015493,24.3869913515112,25.3858278014731,
26.384664251435,27.3835007013968,28.3823371513587,29.3811736013206,30.3800100512825,
31.3788465012443,32.3776829512062,33.3765194011681,34.37535585113,35.3741923010918,
36.3730287510537,37.3718652010156,38.3707016509774,39.3695381009393,40.3683745509012,
41.3672110008631,42.3660474508249,43.3648839007868,44.3637203507487,45.3625568007106,
46.3613932506724,47.3602297006343,48.3590661505962,49.3579026005581,50.3567390505199,
51.3555755004818,52.3544119504437,53.3532484004056,54.3520848503674,55.3509213003293,
56.3497577502912,57.3485942002531,58.3474306502149,59.3462671001768,60.3451035501387,
61.3439400001006,62.3427764500624,63.3416129000243,64.3404493499862,65.3392857999481,
66.3381222499099,67.3369586998718,68.3357951498337,69.3346315997956,70.3334680497574,
71.3323044997193,72.3311409496812,73.3299773996431,74.3288138496049,75.3276502995668,
76.3264867495287,77.3253231994906,78.3241596494524,79.3229960994143,80.3218325493762,
81.3206689993381,82.3195054492999,83.3183418992618,84.3171783492237,85.3160147991856,
86.3148512491474,87.3136876991093,88.3125241490712,89.3113605990331,90.3101970489949,
91.3090334989568,92.3078699489187,93.3067063988806,94.3055428488424,95.3043792988043,
96.3032157487662,97.302052198728,98.3008886486899,99.2997250986518,100.298561548614,
101.297397998576,102.296234448537,103.295070898499,104.293907348461,105.292743798423,
106.291580248385,107.290416698347,108.289253148309,109.288089598271,110.286926048232,
111.285762498194,112.284598948156,113.283435398118,114.28227184808,115.281108298042,
116.279944748004,117.278781197966,118.277617647927,119.276454097889,120.275290547851,
121.274126997813,122.272963447775,123.271799897737,124.270636347699,125.269472797661,
126.268309247622,127.267145697584,128.265982147546,129.264818597508,130.26365504747,
131.262491497432,132.261327947394,133.260164397356,134.259000847317,135.257837297279,
136.256673747241,137.255510197203,138.254346647165,139.253183097127,140.252019547089,
141.250855997051,142.249692447012,143.248528896974,144.247365346936,145.246201796898,
146.24503824686,147.243874696822,148.242711146784,149.241547596746,150.240384046707,
151.239220496669,152.238056946631,153.236893396593,154.235729846555,155.234566296517,
156.233402746479,157.232239196441,158.231075646402,159.229912096364,160.228748546326,
161.227584996288,162.22642144625,163.225257896212,164.224094346174,165.222930796136,
166.221767246097,167.220603696059,168.219440146021,169.218276595983,170.217113045945,
171.215949495907,172.214785945869,173.21362239583,174.212458845792,175.211295295754,
176.210131745716,177.208968195678,178.20780464564,179.206641095602,180.205477545564,
181.204313995525,182.203150445487,183.201986895449,184.200823345411,185.199659795373,
186.198496245335,187.197332695297,188.196169145259,189.195445204588),
 .UNSPECIFIED.);
#159=B_SPLINE_SURFACE_WITH_KNOTS('',3,3,((#122445,#122446,#122447,#122448,
#122449,#122450,#122451,#122452,#122453,#122454,#122455,#122456,#122457,
#122458,#122459,#122460,#122461,#122462,#122463,#122464,#122465,#122466,
#122467,#122468,#122469,#122470,#122471,#122472,#122473,#122474,#122475,
#122476,#122477,#122478,#122479,#122480,#122481,#122482,#122483,#122484,
#122485,#122486,#122487,#122488,#122489,#122490,#122491,#122492,#122493,
#122494,#122495,#122496,#122497,#122498,#122499,#122500,#122501,#122502,
#122503,#122504,#122505,#122506,#122507,#122508,#122509,#122510,#122511,
#122512,#122513,#122514,#122515,#122516,#122517,#122518,#122519,#122520,
#122521,#122522,#122523,#122524,#122525,#122526,#122527,#122528,#122529,
#122530,#122531,#122532,#122533,#122534,#122535,#122536,#122537,#122538,
#122539,#122540,#122541,#122542,#122543,#122544,#122545,#122546,#122547,
#122548,#122549,#122550,#122551,#122552,#122553,#122554,#122555,#122556,
#122557,#122558,#122559,#122560,#122561,#122562,#122563,#122564,#122565,
#122566,#122567,#122568,#122569,#122570,#122571,#122572,#122573,#122574,
#122575,#122576,#122577,#122578,#122579,#122580,#122581,#122582,#122583,
#122584,#122585,#122586,#122587,#122588,#122589,#122590,#122591,#122592,
#122593,#122594,#122595,#122596,#122597,#122598,#122599,#122600,#122601,
#122602,#122603,#122604,#122605,#122606,#122607,#122608,#122609,#122610,
#122611,#122612,#122613,#122614,#122615,#122616,#122617,#122618,#122619,
#122620,#122621,#122622),(#122623,#122624,#122625,#122626,#122627,#122628,
#122629,#122630,#122631,#122632,#122633,#122634,#122635,#122636,#122637,
#122638,#122639,#122640,#122641,#122642,#122643,#122644,#122645,#122646,
#122647,#122648,#122649,#122650,#122651,#122652,#122653,#122654,#122655,
#122656,#122657,#122658,#122659,#122660,#122661,#122662,#122663,#122664,
#122665,#122666,#122667,#122668,#122669,#122670,#122671,#122672,#122673,
#122674,#122675,#122676,#122677,#122678,#122679,#122680,#122681,#122682,
#122683,#122684,#122685,#122686,#122687,#122688,#122689,#122690,#122691,
#122692,#122693,#122694,#122695,#122696,#122697,#122698,#122699,#122700,
#122701,#122702,#122703,#122704,#122705,#122706,#122707,#122708,#122709,
#122710,#122711,#122712,#122713,#122714,#122715,#122716,#122717,#122718,
#122719,#122720,#122721,#122722,#122723,#122724,#122725,#122726,#122727,
#122728,#122729,#122730,#122731,#122732,#122733,#122734,#122735,#122736,
#122737,#122738,#122739,#122740,#122741,#122742,#122743,#122744,#122745,
#122746,#122747,#122748,#122749,#122750,#122751,#122752,#122753,#122754,
#122755,#122756,#122757,#122758,#122759,#122760,#122761,#122762,#122763,
#122764,#122765,#122766,#122767,#122768,#122769,#122770,#122771,#122772,
#122773,#122774,#122775,#122776,#122777,#122778,#122779,#122780,#122781,
#122782,#122783,#122784,#122785,#122786,#122787,#122788,#122789,#122790,
#122791,#122792,#122793,#122794,#122795,#122796,#122797,#122798,#122799,
#122800),(#122801,#122802,#122803,#122804,#122805,#122806,#122807,#122808,
#122809,#122810,#122811,#122812,#122813,#122814,#122815,#122816,#122817,
#122818,#122819,#122820,#122821,#122822,#122823,#122824,#122825,#122826,
#122827,#122828,#122829,#122830,#122831,#122832,#122833,#122834,#122835,
#122836,#122837,#122838,#122839,#122840,#122841,#122842,#122843,#122844,
#122845,#122846,#122847,#122848,#122849,#122850,#122851,#122852,#122853,
#122854,#122855,#122856,#122857,#122858,#122859,#122860,#122861,#122862,
#122863,#122864,#122865,#122866,#122867,#122868,#122869,#122870,#122871,
#122872,#122873,#122874,#122875,#122876,#122877,#122878,#122879,#122880,
#122881,#122882,#122883,#122884,#122885,#122886,#122887,#122888,#122889,
#122890,#122891,#122892,#122893,#122894,#122895,#122896,#122897,#122898,
#122899,#122900,#122901,#122902,#122903,#122904,#122905,#122906,#122907,
#122908,#122909,#122910,#122911,#122912,#122913,#122914,#122915,#122916,
#122917,#122918,#122919,#122920,#122921,#122922,#122923,#122924,#122925,
#122926,#122927,#122928,#122929,#122930,#122931,#122932,#122933,#122934,
#122935,#122936,#122937,#122938,#122939,#122940,#122941,#122942,#122943,
#122944,#122945,#122946,#122947,#122948,#122949,#122950,#122951,#122952,
#122953,#122954,#122955,#122956,#122957,#122958,#122959,#122960,#122961,
#122962,#122963,#122964,#122965,#122966,#122967,#122968,#122969,#122970,
#122971,#122972,#122973,#122974,#122975,#122976,#122977,#122978),(#122979,
#122980,#122981,#122982,#122983,#122984,#122985,#122986,#122987,#122988,
#122989,#122990,#122991,#122992,#122993,#122994,#122995,#122996,#122997,
#122998,#122999,#123000,#123001,#123002,#123003,#123004,#123005,#123006,
#123007,#123008,#123009,#123010,#123011,#123012,#123013,#123014,#123015,
#123016,#123017,#123018,#123019,#123020,#123021,#123022,#123023,#123024,
#123025,#123026,#123027,#123028,#123029,#123030,#123031,#123032,#123033,
#123034,#123035,#123036,#123037,#123038,#123039,#123040,#123041,#123042,
#123043,#123044,#123045,#123046,#123047,#123048,#123049,#123050,#123051,
#123052,#123053,#123054,#123055,#123056,#123057,#123058,#123059,#123060,
#123061,#123062,#123063,#123064,#123065,#123066,#123067,#123068,#123069,
#123070,#123071,#123072,#123073,#123074,#123075,#123076,#123077,#123078,
#123079,#123080,#123081,#123082,#123083,#123084,#123085,#123086,#123087,
#123088,#123089,#123090,#123091,#123092,#123093,#123094,#123095,#123096,
#123097,#123098,#123099,#123100,#123101,#123102,#123103,#123104,#123105,
#123106,#123107,#123108,#123109,#123110,#123111,#123112,#123113,#123114,
#123115,#123116,#123117,#123118,#123119,#123120,#123121,#123122,#123123,
#123124,#123125,#123126,#123127,#123128,#123129,#123130,#123131,#123132,
#123133,#123134,#123135,#123136,#123137,#123138,#123139,#123140,#123141,
#123142,#123143,#123144,#123145,#123146,#123147,#123148,#123149,#123150,
#123151,#123152,#123153,#123154,#123155,#123156)),.UNSPECIFIED.,.F.,.F.,
 .F.,(4,4),(4,1,1,1,1,1,1,1,1,1,1,1,1,1,1,1,1,1,1,1,1,1,1,1,1,1,1,1,1,1,
1,1,1,1,1,1,1,1,1,1,1,1,1,1,1,1,1,1,1,1,1,1,1,1,1,1,1,1,1,1,1,1,1,1,1,1,
1,1,1,1,1,1,1,1,1,1,1,1,1,1,1,1,1,1,1,1,1,1,1,1,1,1,1,1,1,1,1,1,1,1,1,1,
1,1,1,1,1,1,1,1,1,1,1,1,1,1,1,1,1,1,1,1,1,1,1,1,1,1,1,1,1,1,1,1,1,1,1,1,
1,1,1,1,1,1,1,1,1,1,1,1,1,1,1,1,1,1,1,1,1,1,1,1,1,1,1,1,1,1,1,1,1,1,1,1,
1,4),(-0.000439583499978536,0.051531452015598),(11.8664846510264,12.8657606844883,
13.8645971344502,14.8634335844121,15.8622700343739,16.8611064843358,17.8599429342977,
18.8587793842596,19.8576158342214,20.8564522841833,21.8552887341452,22.854125184107,
23.8529616340689,24.8517980840308,25.8506345339927,26.8494709839545,27.8483074339164,
28.8471438838783,29.8459803338402,30.844816783802,31.8436532337639,32.8424896837258,
33.8413261336877,34.8401625836495,35.8389990336114,36.8378354835733,37.8366719335352,
38.835508383497,39.8343448334589,40.8331812834208,41.8320177333827,42.8308541833445,
43.8296906333064,44.8285270832683,45.8273635332302,46.826199983192,47.8250364331539,
48.8238728831158,49.8227093330777,50.8215457830395,51.8203822330014,52.8192186829633,
53.8180551329252,54.816891582887,55.8157280328489,56.8145644828108,57.8134009327727,
58.8122373827345,59.8110738326964,60.8099102826583,61.8087467326202,62.807583182582,
63.8064196325439,64.8052560825058,65.8040925324676,66.8029289824295,67.8017654323914,
68.8006018823533,69.7994383323151,70.798274782277,71.7971112322389,72.7959476822008,
73.7947841321626,74.7936205821245,75.7924570320864,76.7912934820483,77.7901299320101,
78.788966381972,79.7878028319339,80.7866392818958,81.7854757318576,82.7843121818195,
83.7831486317814,84.7819850817433,85.7808215317051,86.779657981667,87.7784944316289,
88.7773308815908,89.7761673315526,90.7750037815145,91.7738402314764,92.7726766814383,
93.7715131314001,94.770349581362,95.7691860313239,96.7680224812858,97.7668589312476,
98.7656953812095,99.7645318311714,100.763368281133,101.762204731095,102.761041181057,
103.759877631019,104.758714080981,105.757550530943,106.756386980905,107.755223430866,
108.754059880828,109.75289633079,110.751732780752,111.750569230714,112.749405680676,
113.748242130638,114.747078580599,115.745915030561,116.744751480523,117.743587930485,
118.742424380447,119.741260830409,120.740097280371,121.738933730333,122.737770180294,
123.736606630256,124.735443080218,125.73427953018,126.733115980142,127.731952430104,
128.730788880066,129.729625330028,130.728461779989,131.727298229951,132.726134679913,
133.724971129875,134.723807579837,135.722644029799,136.721480479761,137.720316929723,
138.719153379684,139.717989829646,140.716826279608,141.71566272957,142.714499179532,
143.713335629494,144.712172079456,145.711008529418,146.709844979379,147.708681429341,
148.707517879303,149.706354329265,150.705190779227,151.704027229189,152.702863679151,
153.701700129113,154.700536579074,155.699373029036,156.698209478998,157.69704592896,
158.695882378922,159.694718828884,160.693555278846,161.692391728808,162.691228178769,
163.690064628731,164.688901078693,165.687737528655,166.686573978617,167.685410428579,
168.684246878541,169.683083328503,170.681919778464,171.680756228426,172.679592678388,
173.67842912835,174.677265578312,175.676102028274,176.674938478236,177.673774928198,
178.672611378159,179.671447828121,180.670284278083,181.669120728045,182.667957178007,
183.666793627969,184.665630077931,185.664466527893,186.663302977854),
 .UNSPECIFIED.);
#160=B_SPLINE_SURFACE_WITH_KNOTS('',3,3,((#123242,#123243,#123244,#123245,
#123246,#123247,#123248,#123249,#123250,#123251,#123252,#123253,#123254,
#123255,#123256,#123257,#123258,#123259,#123260,#123261,#123262,#123263,
#123264,#123265,#123266,#123267,#123268,#123269,#123270,#123271,#123272,
#123273,#123274,#123275,#123276,#123277,#123278,#123279,#123280,#123281,
#123282,#123283,#123284,#123285,#123286,#123287,#123288,#123289,#123290,
#123291,#123292,#123293,#123294,#123295,#123296,#123297,#123298,#123299,
#123300,#123301,#123302,#123303,#123304,#123305,#123306,#123307,#123308,
#123309,#123310,#123311,#123312,#123313,#123314,#123315,#123316,#123317,
#123318,#123319,#123320,#123321,#123322,#123323,#123324,#123325,#123326,
#123327,#123328,#123329,#123330,#123331,#123332,#123333,#123334,#123335,
#123336,#123337,#123338,#123339,#123340,#123341,#123342,#123343,#123344,
#123345,#123346,#123347,#123348,#123349,#123350,#123351,#123352,#123353,
#123354,#123355,#123356,#123357,#123358,#123359,#123360,#123361,#123362,
#123363,#123364,#123365,#123366,#123367,#123368,#123369,#123370,#123371,
#123372,#123373,#123374,#123375,#123376,#123377,#123378,#123379,#123380,
#123381,#123382,#123383,#123384,#123385,#123386,#123387,#123388,#123389,
#123390,#123391,#123392,#123393,#123394,#123395,#123396,#123397,#123398,
#123399,#123400,#123401,#123402,#123403,#123404,#123405,#123406,#123407,
#123408,#123409,#123410,#123411,#123412,#123413,#123414,#123415,#123416,
#123417,#123418,#123419),(#123420,#123421,#123422,#123423,#123424,#123425,
#123426,#123427,#123428,#123429,#123430,#123431,#123432,#123433,#123434,
#123435,#123436,#123437,#123438,#123439,#123440,#123441,#123442,#123443,
#123444,#123445,#123446,#123447,#123448,#123449,#123450,#123451,#123452,
#123453,#123454,#123455,#123456,#123457,#123458,#123459,#123460,#123461,
#123462,#123463,#123464,#123465,#123466,#123467,#123468,#123469,#123470,
#123471,#123472,#123473,#123474,#123475,#123476,#123477,#123478,#123479,
#123480,#123481,#123482,#123483,#123484,#123485,#123486,#123487,#123488,
#123489,#123490,#123491,#123492,#123493,#123494,#123495,#123496,#123497,
#123498,#123499,#123500,#123501,#123502,#123503,#123504,#123505,#123506,
#123507,#123508,#123509,#123510,#123511,#123512,#123513,#123514,#123515,
#123516,#123517,#123518,#123519,#123520,#123521,#123522,#123523,#123524,
#123525,#123526,#123527,#123528,#123529,#123530,#123531,#123532,#123533,
#123534,#123535,#123536,#123537,#123538,#123539,#123540,#123541,#123542,
#123543,#123544,#123545,#123546,#123547,#123548,#123549,#123550,#123551,
#123552,#123553,#123554,#123555,#123556,#123557,#123558,#123559,#123560,
#123561,#123562,#123563,#123564,#123565,#123566,#123567,#123568,#123569,
#123570,#123571,#123572,#123573,#123574,#123575,#123576,#123577,#123578,
#123579,#123580,#123581,#123582,#123583,#123584,#123585,#123586,#123587,
#123588,#123589,#123590,#123591,#123592,#123593,#123594,#123595,#123596,
#123597),(#123598,#123599,#123600,#123601,#123602,#123603,#123604,#123605,
#123606,#123607,#123608,#123609,#123610,#123611,#123612,#123613,#123614,
#123615,#123616,#123617,#123618,#123619,#123620,#123621,#123622,#123623,
#123624,#123625,#123626,#123627,#123628,#123629,#123630,#123631,#123632,
#123633,#123634,#123635,#123636,#123637,#123638,#123639,#123640,#123641,
#123642,#123643,#123644,#123645,#123646,#123647,#123648,#123649,#123650,
#123651,#123652,#123653,#123654,#123655,#123656,#123657,#123658,#123659,
#123660,#123661,#123662,#123663,#123664,#123665,#123666,#123667,#123668,
#123669,#123670,#123671,#123672,#123673,#123674,#123675,#123676,#123677,
#123678,#123679,#123680,#123681,#123682,#123683,#123684,#123685,#123686,
#123687,#123688,#123689,#123690,#123691,#123692,#123693,#123694,#123695,
#123696,#123697,#123698,#123699,#123700,#123701,#123702,#123703,#123704,
#123705,#123706,#123707,#123708,#123709,#123710,#123711,#123712,#123713,
#123714,#123715,#123716,#123717,#123718,#123719,#123720,#123721,#123722,
#123723,#123724,#123725,#123726,#123727,#123728,#123729,#123730,#123731,
#123732,#123733,#123734,#123735,#123736,#123737,#123738,#123739,#123740,
#123741,#123742,#123743,#123744,#123745,#123746,#123747,#123748,#123749,
#123750,#123751,#123752,#123753,#123754,#123755,#123756,#123757,#123758,
#123759,#123760,#123761,#123762,#123763,#123764,#123765,#123766,#123767,
#123768,#123769,#123770,#123771,#123772,#123773,#123774,#123775),(#123776,
#123777,#123778,#123779,#123780,#123781,#123782,#123783,#123784,#123785,
#123786,#123787,#123788,#123789,#123790,#123791,#123792,#123793,#123794,
#123795,#123796,#123797,#123798,#123799,#123800,#123801,#123802,#123803,
#123804,#123805,#123806,#123807,#123808,#123809,#123810,#123811,#123812,
#123813,#123814,#123815,#123816,#123817,#123818,#123819,#123820,#123821,
#123822,#123823,#123824,#123825,#123826,#123827,#123828,#123829,#123830,
#123831,#123832,#123833,#123834,#123835,#123836,#123837,#123838,#123839,
#123840,#123841,#123842,#123843,#123844,#123845,#123846,#123847,#123848,
#123849,#123850,#123851,#123852,#123853,#123854,#123855,#123856,#123857,
#123858,#123859,#123860,#123861,#123862,#123863,#123864,#123865,#123866,
#123867,#123868,#123869,#123870,#123871,#123872,#123873,#123874,#123875,
#123876,#123877,#123878,#123879,#123880,#123881,#123882,#123883,#123884,
#123885,#123886,#123887,#123888,#123889,#123890,#123891,#123892,#123893,
#123894,#123895,#123896,#123897,#123898,#123899,#123900,#123901,#123902,
#123903,#123904,#123905,#123906,#123907,#123908,#123909,#123910,#123911,
#123912,#123913,#123914,#123915,#123916,#123917,#123918,#123919,#123920,
#123921,#123922,#123923,#123924,#123925,#123926,#123927,#123928,#123929,
#123930,#123931,#123932,#123933,#123934,#123935,#123936,#123937,#123938,
#123939,#123940,#123941,#123942,#123943,#123944,#123945,#123946,#123947,
#123948,#123949,#123950,#123951,#123952,#123953)),.UNSPECIFIED.,.F.,.F.,
 .F.,(4,4),(4,1,1,1,1,1,1,1,1,1,1,1,1,1,1,1,1,1,1,1,1,1,1,1,1,1,1,1,1,1,
1,1,1,1,1,1,1,1,1,1,1,1,1,1,1,1,1,1,1,1,1,1,1,1,1,1,1,1,1,1,1,1,1,1,1,1,
1,1,1,1,1,1,1,1,1,1,1,1,1,1,1,1,1,1,1,1,1,1,1,1,1,1,1,1,1,1,1,1,1,1,1,1,
1,1,1,1,1,1,1,1,1,1,1,1,1,1,1,1,1,1,1,1,1,1,1,1,1,1,1,1,1,1,1,1,1,1,1,1,
1,1,1,1,1,1,1,1,1,1,1,1,1,1,1,1,1,1,1,1,1,1,1,1,1,1,1,1,1,1,1,1,1,1,1,1,
1,4),(-0.000378221444736312,0.0515928134973294),(14.3986268518925,15.3974633018543,
16.3962997518162,17.3951362017781,18.39397265174,19.3928091017018,20.3916455516637,
21.3904820016256,22.3893184515875,23.3881549015493,24.3869913515112,25.3858278014731,
26.384664251435,27.3835007013968,28.3823371513587,29.3811736013206,30.3800100512825,
31.3788465012443,32.3776829512062,33.3765194011681,34.37535585113,35.3741923010918,
36.3730287510537,37.3718652010156,38.3707016509774,39.3695381009393,40.3683745509012,
41.3672110008631,42.3660474508249,43.3648839007868,44.3637203507487,45.3625568007106,
46.3613932506724,47.3602297006343,48.3590661505962,49.3579026005581,50.3567390505199,
51.3555755004818,52.3544119504437,53.3532484004056,54.3520848503674,55.3509213003293,
56.3497577502912,57.3485942002531,58.3474306502149,59.3462671001768,60.3451035501387,
61.3439400001006,62.3427764500624,63.3416129000243,64.3404493499862,65.3392857999481,
66.3381222499099,67.3369586998718,68.3357951498337,69.3346315997956,70.3334680497574,
71.3323044997193,72.3311409496812,73.3299773996431,74.3288138496049,75.3276502995668,
76.3264867495287,77.3253231994906,78.3241596494524,79.3229960994143,80.3218325493762,
81.3206689993381,82.3195054492999,83.3183418992618,84.3171783492237,85.3160147991856,
86.3148512491474,87.3136876991093,88.3125241490712,89.3113605990331,90.3101970489949,
91.3090334989568,92.3078699489187,93.3067063988806,94.3055428488424,95.3043792988043,
96.3032157487662,97.302052198728,98.3008886486899,99.2997250986518,100.298561548614,
101.297397998576,102.296234448537,103.295070898499,104.293907348461,105.292743798423,
106.291580248385,107.290416698347,108.289253148309,109.288089598271,110.286926048232,
111.285762498194,112.284598948156,113.283435398118,114.28227184808,115.281108298042,
116.279944748004,117.278781197966,118.277617647927,119.276454097889,120.275290547851,
121.274126997813,122.272963447775,123.271799897737,124.270636347699,125.269472797661,
126.268309247622,127.267145697584,128.265982147546,129.264818597508,130.26365504747,
131.262491497432,132.261327947394,133.260164397356,134.259000847317,135.257837297279,
136.256673747241,137.255510197203,138.254346647165,139.253183097127,140.252019547089,
141.250855997051,142.249692447012,143.248528896974,144.247365346936,145.246201796898,
146.24503824686,147.243874696822,148.242711146784,149.241547596746,150.240384046707,
151.239220496669,152.238056946631,153.236893396593,154.235729846555,155.234566296517,
156.233402746479,157.232239196441,158.231075646402,159.229912096364,160.228748546326,
161.227584996288,162.22642144625,163.225257896212,164.224094346174,165.222930796136,
166.221767246097,167.220603696059,168.219440146021,169.218276595983,170.217113045945,
171.215949495907,172.214785945869,173.21362239583,174.212458845792,175.211295295754,
176.210131745716,177.208968195678,178.20780464564,179.206641095602,180.205477545564,
181.204313995525,182.203150445487,183.201986895449,184.200823345411,185.199659795373,
186.198496245335,187.197332695297,188.196169145259,189.195445174867),
 .UNSPECIFIED.);
#161=B_SPLINE_SURFACE_WITH_KNOTS('',3,3,((#207102,#207103,#207104,#207105,
#207106,#207107,#207108,#207109,#207110,#207111,#207112,#207113,#207114,
#207115,#207116,#207117,#207118,#207119,#207120,#207121,#207122,#207123,
#207124,#207125,#207126,#207127,#207128,#207129,#207130,#207131,#207132,
#207133,#207134,#207135,#207136,#207137,#207138,#207139,#207140,#207141,
#207142,#207143,#207144,#207145,#207146,#207147,#207148,#207149,#207150,
#207151,#207152,#207153,#207154,#207155),(#207156,#207157,#207158,#207159,
#207160,#207161,#207162,#207163,#207164,#207165,#207166,#207167,#207168,
#207169,#207170,#207171,#207172,#207173,#207174,#207175,#207176,#207177,
#207178,#207179,#207180,#207181,#207182,#207183,#207184,#207185,#207186,
#207187,#207188,#207189,#207190,#207191,#207192,#207193,#207194,#207195,
#207196,#207197,#207198,#207199,#207200,#207201,#207202,#207203,#207204,
#207205,#207206,#207207,#207208,#207209),(#207210,#207211,#207212,#207213,
#207214,#207215,#207216,#207217,#207218,#207219,#207220,#207221,#207222,
#207223,#207224,#207225,#207226,#207227,#207228,#207229,#207230,#207231,
#207232,#207233,#207234,#207235,#207236,#207237,#207238,#207239,#207240,
#207241,#207242,#207243,#207244,#207245,#207246,#207247,#207248,#207249,
#207250,#207251,#207252,#207253,#207254,#207255,#207256,#207257,#207258,
#207259,#207260,#207261,#207262,#207263),(#207264,#207265,#207266,#207267,
#207268,#207269,#207270,#207271,#207272,#207273,#207274,#207275,#207276,
#207277,#207278,#207279,#207280,#207281,#207282,#207283,#207284,#207285,
#207286,#207287,#207288,#207289,#207290,#207291,#207292,#207293,#207294,
#207295,#207296,#207297,#207298,#207299,#207300,#207301,#207302,#207303,
#207304,#207305,#207306,#207307,#207308,#207309,#207310,#207311,#207312,
#207313,#207314,#207315,#207316,#207317)),.UNSPECIFIED.,.F.,.F.,.F.,(4,
4),(4,1,1,1,1,1,1,1,1,1,1,1,1,1,1,1,1,1,1,1,1,1,1,1,1,1,1,1,1,1,1,1,1,1,
1,1,1,1,1,1,1,1,1,1,1,1,1,1,1,1,1,4),(-0.000616514442677502,0.096936516137423),
(11.8528940954716,12.340290362188,12.8276378599491,13.3149853577101,13.8023328554711,
14.2896803532321,14.7770278509931,15.2643753487541,15.7517228465151,16.2390703442761,
16.7264178420371,17.2137653397981,17.7011128375591,18.1884603353201,18.6758078330811,
19.1631553308421,19.6505028286031,20.1378503263641,20.6251978241251,21.1125453218861,
21.5998928196471,22.0872403174081,22.5745878151691,23.0619353129301,23.5492828106911,
24.5239778062131,25.4986728017351,26.4733677972571,26.9607152950181,27.4480627927791,
27.9354102905401,28.4227577883011,28.9101052860621,29.3974527838231,29.8848002815841,
30.3721477793451,30.8594952771061,31.3468427748671,31.8341902726282,32.3215377703892,
32.8088852681502,33.2962327659112,33.7835802636722,34.2709277614332,34.7582752591942,
35.2456227569552,35.7329702547162,36.2203177524772,36.7076652502382,37.1950127479992,
37.6823602457602,38.1697077435212),.UNSPECIFIED.);
#162=B_SPLINE_SURFACE_WITH_KNOTS('',3,3,((#207524,#207525,#207526,#207527,
#207528,#207529,#207530,#207531,#207532,#207533,#207534,#207535,#207536,
#207537,#207538,#207539,#207540,#207541,#207542,#207543,#207544,#207545,
#207546,#207547,#207548,#207549,#207550,#207551,#207552,#207553,#207554,
#207555,#207556,#207557,#207558,#207559,#207560,#207561,#207562,#207563,
#207564,#207565,#207566,#207567,#207568,#207569,#207570,#207571,#207572,
#207573,#207574,#207575,#207576,#207577),(#207578,#207579,#207580,#207581,
#207582,#207583,#207584,#207585,#207586,#207587,#207588,#207589,#207590,
#207591,#207592,#207593,#207594,#207595,#207596,#207597,#207598,#207599,
#207600,#207601,#207602,#207603,#207604,#207605,#207606,#207607,#207608,
#207609,#207610,#207611,#207612,#207613,#207614,#207615,#207616,#207617,
#207618,#207619,#207620,#207621,#207622,#207623,#207624,#207625,#207626,
#207627,#207628,#207629,#207630,#207631),(#207632,#207633,#207634,#207635,
#207636,#207637,#207638,#207639,#207640,#207641,#207642,#207643,#207644,
#207645,#207646,#207647,#207648,#207649,#207650,#207651,#207652,#207653,
#207654,#207655,#207656,#207657,#207658,#207659,#207660,#207661,#207662,
#207663,#207664,#207665,#207666,#207667,#207668,#207669,#207670,#207671,
#207672,#207673,#207674,#207675,#207676,#207677,#207678,#207679,#207680,
#207681,#207682,#207683,#207684,#207685),(#207686,#207687,#207688,#207689,
#207690,#207691,#207692,#207693,#207694,#207695,#207696,#207697,#207698,
#207699,#207700,#207701,#207702,#207703,#207704,#207705,#207706,#207707,
#207708,#207709,#207710,#207711,#207712,#207713,#207714,#207715,#207716,
#207717,#207718,#207719,#207720,#207721,#207722,#207723,#207724,#207725,
#207726,#207727,#207728,#207729,#207730,#207731,#207732,#207733,#207734,
#207735,#207736,#207737,#207738,#207739)),.UNSPECIFIED.,.F.,.F.,.F.,(4,
4),(4,1,1,1,1,1,1,1,1,1,1,1,1,1,1,1,1,1,1,1,1,1,1,1,1,1,1,1,1,1,1,1,1,1,
1,1,1,1,1,1,1,1,1,1,1,1,1,1,1,1,1,4),(-0.000403550678892824,0.0971495250489538),
(14.399609326548,14.886956824309,15.37430432207,15.861651819831,16.348999317592,
16.836346815353,17.323694313114,17.811041810875,18.298389308636,18.785736806397,
19.273084304158,19.7604318019191,20.2477792996801,20.7351267974411,21.2224742952021,
21.7098217929631,22.1971692907241,22.6845167884851,23.1718642862461,23.6592117840071,
24.1465592817681,24.6339067795291,25.1212542772901,25.6086017750511,26.0959492728121,
27.0706442683341,28.0453392638561,29.0200342593781,29.5073817571391,29.9947292549001,
30.4820767526611,30.9694242504221,31.4567717481831,31.9441192459441,32.4314667437051,
32.9188142414661,33.4061617392271,33.8935092369881,34.3808567347491,34.8682042325101,
35.3555517302711,35.8428992280321,36.3302467257931,36.8175942235541,37.3049417213151,
37.7922892190762,38.2796367168372,38.7669842145982,39.2543317123592,39.7416792101202,
40.2290267078812,40.7164229770097),.UNSPECIFIED.);
#163=B_SPLINE_SURFACE_WITH_KNOTS('',3,3,((#207943,#207944,#207945,#207946,
#207947,#207948,#207949,#207950,#207951,#207952,#207953,#207954,#207955,
#207956,#207957,#207958,#207959,#207960,#207961,#207962,#207963,#207964,
#207965,#207966,#207967,#207968,#207969,#207970,#207971,#207972,#207973,
#207974,#207975,#207976,#207977,#207978,#207979,#207980,#207981,#207982,
#207983,#207984,#207985,#207986,#207987,#207988,#207989,#207990,#207991,
#207992,#207993,#207994,#207995,#207996),(#207997,#207998,#207999,#208000,
#208001,#208002,#208003,#208004,#208005,#208006,#208007,#208008,#208009,
#208010,#208011,#208012,#208013,#208014,#208015,#208016,#208017,#208018,
#208019,#208020,#208021,#208022,#208023,#208024,#208025,#208026,#208027,
#208028,#208029,#208030,#208031,#208032,#208033,#208034,#208035,#208036,
#208037,#208038,#208039,#208040,#208041,#208042,#208043,#208044,#208045,
#208046,#208047,#208048,#208049,#208050),(#208051,#208052,#208053,#208054,
#208055,#208056,#208057,#208058,#208059,#208060,#208061,#208062,#208063,
#208064,#208065,#208066,#208067,#208068,#208069,#208070,#208071,#208072,
#208073,#208074,#208075,#208076,#208077,#208078,#208079,#208080,#208081,
#208082,#208083,#208084,#208085,#208086,#208087,#208088,#208089,#208090,
#208091,#208092,#208093,#208094,#208095,#208096,#208097,#208098,#208099,
#208100,#208101,#208102,#208103,#208104),(#208105,#208106,#208107,#208108,
#208109,#208110,#208111,#208112,#208113,#208114,#208115,#208116,#208117,
#208118,#208119,#208120,#208121,#208122,#208123,#208124,#208125,#208126,
#208127,#208128,#208129,#208130,#208131,#208132,#208133,#208134,#208135,
#208136,#208137,#208138,#208139,#208140,#208141,#208142,#208143,#208144,
#208145,#208146,#208147,#208148,#208149,#208150,#208151,#208152,#208153,
#208154,#208155,#208156,#208157,#208158)),.UNSPECIFIED.,.F.,.F.,.F.,(4,
4),(4,1,1,1,1,1,1,1,1,1,1,1,1,1,1,1,1,1,1,1,1,1,1,1,1,1,1,1,1,1,1,1,1,1,
1,1,1,1,1,1,1,1,1,1,1,1,1,1,1,1,1,4),(-0.000616665549394816,0.0969365142669611),
(11.8528940858174,12.340290362188,12.827637859949,13.31498535771,13.802332855471,
14.289680353232,14.777027850993,15.264375348754,15.751722846515,16.239070344276,
16.7264178420371,17.2137653397981,17.7011128375591,18.1884603353201,18.6758078330811,
19.1631553308421,19.6505028286031,20.1378503263641,20.6251978241251,21.1125453218861,
21.5998928196471,22.0872403174081,22.5745878151691,23.0619353129301,23.5492828106911,
24.5239778062131,25.4986728017351,26.4733677972571,26.9607152950181,27.4480627927791,
27.9354102905401,28.4227577883011,28.9101052860621,29.3974527838231,29.8848002815841,
30.3721477793451,30.8594952771061,31.3468427748671,31.8341902726281,32.3215377703891,
32.8088852681501,33.2962327659111,33.7835802636721,34.2709277614331,34.7582752591941,
35.2456227569552,35.7329702547162,36.2203177524772,36.7076652502382,37.1950127479992,
37.6823602457602,38.1697077435212),.UNSPECIFIED.);
#164=B_SPLINE_SURFACE_WITH_KNOTS('',3,3,((#208368,#208369,#208370,#208371,
#208372,#208373,#208374,#208375,#208376,#208377,#208378,#208379,#208380,
#208381,#208382,#208383,#208384,#208385,#208386,#208387,#208388,#208389,
#208390,#208391,#208392,#208393,#208394,#208395,#208396,#208397,#208398,
#208399,#208400,#208401,#208402,#208403,#208404,#208405,#208406,#208407,
#208408,#208409,#208410,#208411,#208412,#208413,#208414,#208415,#208416,
#208417,#208418,#208419,#208420,#208421),(#208422,#208423,#208424,#208425,
#208426,#208427,#208428,#208429,#208430,#208431,#208432,#208433,#208434,
#208435,#208436,#208437,#208438,#208439,#208440,#208441,#208442,#208443,
#208444,#208445,#208446,#208447,#208448,#208449,#208450,#208451,#208452,
#208453,#208454,#208455,#208456,#208457,#208458,#208459,#208460,#208461,
#208462,#208463,#208464,#208465,#208466,#208467,#208468,#208469,#208470,
#208471,#208472,#208473,#208474,#208475),(#208476,#208477,#208478,#208479,
#208480,#208481,#208482,#208483,#208484,#208485,#208486,#208487,#208488,
#208489,#208490,#208491,#208492,#208493,#208494,#208495,#208496,#208497,
#208498,#208499,#208500,#208501,#208502,#208503,#208504,#208505,#208506,
#208507,#208508,#208509,#208510,#208511,#208512,#208513,#208514,#208515,
#208516,#208517,#208518,#208519,#208520,#208521,#208522,#208523,#208524,
#208525,#208526,#208527,#208528,#208529),(#208530,#208531,#208532,#208533,
#208534,#208535,#208536,#208537,#208538,#208539,#208540,#208541,#208542,
#208543,#208544,#208545,#208546,#208547,#208548,#208549,#208550,#208551,
#208552,#208553,#208554,#208555,#208556,#208557,#208558,#208559,#208560,
#208561,#208562,#208563,#208564,#208565,#208566,#208567,#208568,#208569,
#208570,#208571,#208572,#208573,#208574,#208575,#208576,#208577,#208578,
#208579,#208580,#208581,#208582,#208583)),.UNSPECIFIED.,.F.,.F.,.F.,(4,
4),(4,1,1,1,1,1,1,1,1,1,1,1,1,1,1,1,1,1,1,1,1,1,1,1,1,1,1,1,1,1,1,1,1,1,
1,1,1,1,1,1,1,1,1,1,1,1,1,1,1,1,1,4),(-0.000403548226902083,0.0971496961622332),
(14.399609326548,14.886956824309,15.37430432207,15.861651819831,16.348999317592,
16.836346815353,17.323694313114,17.811041810875,18.298389308636,18.785736806397,
19.273084304158,19.760431801919,20.24777929968,20.735126797441,21.222474295202,
21.709821792963,22.1971692907241,22.6845167884851,23.1718642862461,23.6592117840071,
24.1465592817681,24.6339067795291,25.1212542772901,25.6086017750511,26.0959492728121,
27.0706442683341,28.0453392638561,29.0200342593781,29.5073817571391,29.9947292549001,
30.4820767526611,30.9694242504221,31.4567717481831,31.9441192459441,32.4314667437051,
32.9188142414661,33.4061617392271,33.8935092369881,34.3808567347491,34.8682042325101,
35.3555517302711,35.8428992280321,36.3302467257931,36.8175942235541,37.3049417213151,
37.7922892190761,38.2796367168371,38.7669842145981,39.2543317123591,39.7416792101202,
40.2290267078812,40.7164229892059),.UNSPECIFIED.);
#165=B_SPLINE_SURFACE_WITH_KNOTS('',3,3,((#208796,#208797,#208798,#208799,
#208800,#208801,#208802,#208803,#208804,#208805,#208806,#208807,#208808,
#208809,#208810,#208811,#208812,#208813,#208814,#208815,#208816,#208817,
#208818,#208819,#208820,#208821,#208822,#208823,#208824,#208825,#208826,
#208827,#208828,#208829,#208830,#208831,#208832,#208833,#208834,#208835,
#208836,#208837,#208838,#208839,#208840,#208841,#208842,#208843,#208844,
#208845,#208846,#208847,#208848,#208849,#208850,#208851,#208852,#208853,
#208854,#208855,#208856,#208857,#208858,#208859,#208860,#208861,#208862,
#208863,#208864,#208865,#208866,#208867,#208868,#208869,#208870,#208871,
#208872,#208873,#208874,#208875,#208876,#208877,#208878,#208879,#208880,
#208881,#208882,#208883,#208884,#208885,#208886,#208887,#208888,#208889,
#208890,#208891,#208892,#208893,#208894,#208895,#208896,#208897,#208898,
#208899,#208900,#208901,#208902,#208903,#208904,#208905,#208906,#208907,
#208908,#208909,#208910,#208911,#208912,#208913,#208914,#208915,#208916,
#208917,#208918,#208919,#208920,#208921,#208922,#208923,#208924,#208925,
#208926,#208927,#208928,#208929,#208930,#208931,#208932,#208933,#208934,
#208935,#208936,#208937,#208938,#208939,#208940,#208941,#208942,#208943,
#208944,#208945,#208946,#208947,#208948,#208949,#208950,#208951,#208952,
#208953,#208954,#208955,#208956,#208957,#208958,#208959,#208960,#208961,
#208962,#208963,#208964,#208965,#208966,#208967,#208968,#208969,#208970,
#208971,#208972,#208973),(#208974,#208975,#208976,#208977,#208978,#208979,
#208980,#208981,#208982,#208983,#208984,#208985,#208986,#208987,#208988,
#208989,#208990,#208991,#208992,#208993,#208994,#208995,#208996,#208997,
#208998,#208999,#209000,#209001,#209002,#209003,#209004,#209005,#209006,
#209007,#209008,#209009,#209010,#209011,#209012,#209013,#209014,#209015,
#209016,#209017,#209018,#209019,#209020,#209021,#209022,#209023,#209024,
#209025,#209026,#209027,#209028,#209029,#209030,#209031,#209032,#209033,
#209034,#209035,#209036,#209037,#209038,#209039,#209040,#209041,#209042,
#209043,#209044,#209045,#209046,#209047,#209048,#209049,#209050,#209051,
#209052,#209053,#209054,#209055,#209056,#209057,#209058,#209059,#209060,
#209061,#209062,#209063,#209064,#209065,#209066,#209067,#209068,#209069,
#209070,#209071,#209072,#209073,#209074,#209075,#209076,#209077,#209078,
#209079,#209080,#209081,#209082,#209083,#209084,#209085,#209086,#209087,
#209088,#209089,#209090,#209091,#209092,#209093,#209094,#209095,#209096,
#209097,#209098,#209099,#209100,#209101,#209102,#209103,#209104,#209105,
#209106,#209107,#209108,#209109,#209110,#209111,#209112,#209113,#209114,
#209115,#209116,#209117,#209118,#209119,#209120,#209121,#209122,#209123,
#209124,#209125,#209126,#209127,#209128,#209129,#209130,#209131,#209132,
#209133,#209134,#209135,#209136,#209137,#209138,#209139,#209140,#209141,
#209142,#209143,#209144,#209145,#209146,#209147,#209148,#209149,#209150,
#209151),(#209152,#209153,#209154,#209155,#209156,#209157,#209158,#209159,
#209160,#209161,#209162,#209163,#209164,#209165,#209166,#209167,#209168,
#209169,#209170,#209171,#209172,#209173,#209174,#209175,#209176,#209177,
#209178,#209179,#209180,#209181,#209182,#209183,#209184,#209185,#209186,
#209187,#209188,#209189,#209190,#209191,#209192,#209193,#209194,#209195,
#209196,#209197,#209198,#209199,#209200,#209201,#209202,#209203,#209204,
#209205,#209206,#209207,#209208,#209209,#209210,#209211,#209212,#209213,
#209214,#209215,#209216,#209217,#209218,#209219,#209220,#209221,#209222,
#209223,#209224,#209225,#209226,#209227,#209228,#209229,#209230,#209231,
#209232,#209233,#209234,#209235,#209236,#209237,#209238,#209239,#209240,
#209241,#209242,#209243,#209244,#209245,#209246,#209247,#209248,#209249,
#209250,#209251,#209252,#209253,#209254,#209255,#209256,#209257,#209258,
#209259,#209260,#209261,#209262,#209263,#209264,#209265,#209266,#209267,
#209268,#209269,#209270,#209271,#209272,#209273,#209274,#209275,#209276,
#209277,#209278,#209279,#209280,#209281,#209282,#209283,#209284,#209285,
#209286,#209287,#209288,#209289,#209290,#209291,#209292,#209293,#209294,
#209295,#209296,#209297,#209298,#209299,#209300,#209301,#209302,#209303,
#209304,#209305,#209306,#209307,#209308,#209309,#209310,#209311,#209312,
#209313,#209314,#209315,#209316,#209317,#209318,#209319,#209320,#209321,
#209322,#209323,#209324,#209325,#209326,#209327,#209328,#209329),(#209330,
#209331,#209332,#209333,#209334,#209335,#209336,#209337,#209338,#209339,
#209340,#209341,#209342,#209343,#209344,#209345,#209346,#209347,#209348,
#209349,#209350,#209351,#209352,#209353,#209354,#209355,#209356,#209357,
#209358,#209359,#209360,#209361,#209362,#209363,#209364,#209365,#209366,
#209367,#209368,#209369,#209370,#209371,#209372,#209373,#209374,#209375,
#209376,#209377,#209378,#209379,#209380,#209381,#209382,#209383,#209384,
#209385,#209386,#209387,#209388,#209389,#209390,#209391,#209392,#209393,
#209394,#209395,#209396,#209397,#209398,#209399,#209400,#209401,#209402,
#209403,#209404,#209405,#209406,#209407,#209408,#209409,#209410,#209411,
#209412,#209413,#209414,#209415,#209416,#209417,#209418,#209419,#209420,
#209421,#209422,#209423,#209424,#209425,#209426,#209427,#209428,#209429,
#209430,#209431,#209432,#209433,#209434,#209435,#209436,#209437,#209438,
#209439,#209440,#209441,#209442,#209443,#209444,#209445,#209446,#209447,
#209448,#209449,#209450,#209451,#209452,#209453,#209454,#209455,#209456,
#209457,#209458,#209459,#209460,#209461,#209462,#209463,#209464,#209465,
#209466,#209467,#209468,#209469,#209470,#209471,#209472,#209473,#209474,
#209475,#209476,#209477,#209478,#209479,#209480,#209481,#209482,#209483,
#209484,#209485,#209486,#209487,#209488,#209489,#209490,#209491,#209492,
#209493,#209494,#209495,#209496,#209497,#209498,#209499,#209500,#209501,
#209502,#209503,#209504,#209505,#209506,#209507)),.UNSPECIFIED.,.F.,.F.,
 .F.,(4,4),(4,1,1,1,1,1,1,1,1,1,1,1,1,1,1,1,1,1,1,1,1,1,1,1,1,1,1,1,1,1,
1,1,1,1,1,1,1,1,1,1,1,1,1,1,1,1,1,1,1,1,1,1,1,1,1,1,1,1,1,1,1,1,1,1,1,1,
1,1,1,1,1,1,1,1,1,1,1,1,1,1,1,1,1,1,1,1,1,1,1,1,1,1,1,1,1,1,1,1,1,1,1,1,
1,1,1,1,1,1,1,1,1,1,1,1,1,1,1,1,1,1,1,1,1,1,1,1,1,1,1,1,1,1,1,1,1,1,1,1,
1,1,1,1,1,1,1,1,1,1,1,1,1,1,1,1,1,1,1,1,1,1,1,1,1,1,1,1,1,1,1,1,1,1,1,1,
1,4),(-0.000439606948779753,0.0515314320759051),(11.8664846275776,12.8657606844883,
13.8645971344502,14.8634335844121,15.8622700343739,16.8611064843358,17.8599429342977,
18.8587793842595,19.8576158342214,20.8564522841833,21.8552887341452,22.854125184107,
23.8529616340689,24.8517980840308,25.8506345339927,26.8494709839545,27.8483074339164,
28.8471438838783,29.8459803338402,30.844816783802,31.8436532337639,32.8424896837258,
33.8413261336877,34.8401625836495,35.8389990336114,36.8378354835733,37.8366719335352,
38.835508383497,39.8343448334589,40.8331812834208,41.8320177333826,42.8308541833445,
43.8296906333064,44.8285270832683,45.8273635332301,46.826199983192,47.8250364331539,
48.8238728831158,49.8227093330776,50.8215457830395,51.8203822330014,52.8192186829633,
53.8180551329251,54.816891582887,55.8157280328489,56.8145644828108,57.8134009327726,
58.8122373827345,59.8110738326964,60.8099102826583,61.8087467326201,62.807583182582,
63.8064196325439,64.8052560825058,65.8040925324676,66.8029289824295,67.8017654323914,
68.8006018823532,69.7994383323151,70.798274782277,71.7971112322389,72.7959476822007,
73.7947841321626,74.7936205821245,75.7924570320864,76.7912934820482,77.7901299320101,
78.788966381972,79.7878028319339,80.7866392818957,81.7854757318576,82.7843121818195,
83.7831486317814,84.7819850817432,85.7808215317051,86.779657981667,87.7784944316288,
88.7773308815907,89.7761673315526,90.7750037815145,91.7738402314764,92.7726766814382,
93.7715131314001,94.770349581362,95.7691860313238,96.7680224812857,97.7668589312476,
98.7656953812095,99.7645318311714,100.763368281133,101.762204731095,102.761041181057,
103.759877631019,104.758714080981,105.757550530943,106.756386980904,107.755223430866,
108.754059880828,109.75289633079,110.751732780752,111.750569230714,112.749405680676,
113.748242130638,114.747078580599,115.745915030561,116.744751480523,117.743587930485,
118.742424380447,119.741260830409,120.740097280371,121.738933730333,122.737770180294,
123.736606630256,124.735443080218,125.73427953018,126.733115980142,127.731952430104,
128.730788880066,129.729625330028,130.728461779989,131.727298229951,132.726134679913,
133.724971129875,134.723807579837,135.722644029799,136.721480479761,137.720316929723,
138.719153379684,139.717989829646,140.716826279608,141.71566272957,142.714499179532,
143.713335629494,144.712172079456,145.711008529418,146.709844979379,147.708681429341,
148.707517879303,149.706354329265,150.705190779227,151.704027229189,152.702863679151,
153.701700129113,154.700536579074,155.699373029036,156.698209478998,157.69704592896,
158.695882378922,159.694718828884,160.693555278846,161.692391728808,162.691228178769,
163.690064628731,164.688901078693,165.687737528655,166.686573978617,167.685410428579,
168.684246878541,169.683083328503,170.681919778464,171.680756228426,172.679592678388,
173.67842912835,174.677265578312,175.676102028274,176.674938478236,177.673774928198,
178.672611378159,179.671447828121,180.670284278083,181.669120728045,182.667957178007,
183.666793627969,184.665630077931,185.664466527893,186.663302977854),
 .UNSPECIFIED.);
#166=B_SPLINE_SURFACE_WITH_KNOTS('',3,3,((#209596,#209597,#209598,#209599,
#209600,#209601,#209602,#209603,#209604,#209605,#209606,#209607,#209608,
#209609,#209610,#209611,#209612,#209613,#209614,#209615,#209616,#209617,
#209618,#209619,#209620,#209621,#209622,#209623,#209624,#209625,#209626,
#209627,#209628,#209629,#209630,#209631,#209632,#209633,#209634,#209635,
#209636,#209637,#209638,#209639,#209640,#209641,#209642,#209643,#209644,
#209645,#209646,#209647,#209648,#209649,#209650,#209651,#209652,#209653,
#209654,#209655,#209656,#209657,#209658,#209659,#209660,#209661,#209662,
#209663,#209664,#209665,#209666,#209667,#209668,#209669,#209670,#209671,
#209672,#209673,#209674,#209675,#209676,#209677,#209678,#209679,#209680,
#209681,#209682,#209683,#209684,#209685,#209686,#209687,#209688,#209689,
#209690,#209691,#209692,#209693,#209694,#209695,#209696,#209697,#209698,
#209699,#209700,#209701,#209702,#209703,#209704,#209705,#209706,#209707,
#209708,#209709,#209710,#209711,#209712,#209713,#209714,#209715,#209716,
#209717,#209718,#209719,#209720,#209721,#209722,#209723,#209724,#209725,
#209726,#209727,#209728,#209729,#209730,#209731,#209732,#209733,#209734,
#209735,#209736,#209737,#209738,#209739,#209740,#209741,#209742,#209743,
#209744,#209745,#209746,#209747,#209748,#209749,#209750,#209751,#209752,
#209753,#209754,#209755,#209756,#209757,#209758,#209759,#209760,#209761,
#209762,#209763,#209764,#209765,#209766,#209767,#209768,#209769,#209770,
#209771,#209772,#209773),(#209774,#209775,#209776,#209777,#209778,#209779,
#209780,#209781,#209782,#209783,#209784,#209785,#209786,#209787,#209788,
#209789,#209790,#209791,#209792,#209793,#209794,#209795,#209796,#209797,
#209798,#209799,#209800,#209801,#209802,#209803,#209804,#209805,#209806,
#209807,#209808,#209809,#209810,#209811,#209812,#209813,#209814,#209815,
#209816,#209817,#209818,#209819,#209820,#209821,#209822,#209823,#209824,
#209825,#209826,#209827,#209828,#209829,#209830,#209831,#209832,#209833,
#209834,#209835,#209836,#209837,#209838,#209839,#209840,#209841,#209842,
#209843,#209844,#209845,#209846,#209847,#209848,#209849,#209850,#209851,
#209852,#209853,#209854,#209855,#209856,#209857,#209858,#209859,#209860,
#209861,#209862,#209863,#209864,#209865,#209866,#209867,#209868,#209869,
#209870,#209871,#209872,#209873,#209874,#209875,#209876,#209877,#209878,
#209879,#209880,#209881,#209882,#209883,#209884,#209885,#209886,#209887,
#209888,#209889,#209890,#209891,#209892,#209893,#209894,#209895,#209896,
#209897,#209898,#209899,#209900,#209901,#209902,#209903,#209904,#209905,
#209906,#209907,#209908,#209909,#209910,#209911,#209912,#209913,#209914,
#209915,#209916,#209917,#209918,#209919,#209920,#209921,#209922,#209923,
#209924,#209925,#209926,#209927,#209928,#209929,#209930,#209931,#209932,
#209933,#209934,#209935,#209936,#209937,#209938,#209939,#209940,#209941,
#209942,#209943,#209944,#209945,#209946,#209947,#209948,#209949,#209950,
#209951),(#209952,#209953,#209954,#209955,#209956,#209957,#209958,#209959,
#209960,#209961,#209962,#209963,#209964,#209965,#209966,#209967,#209968,
#209969,#209970,#209971,#209972,#209973,#209974,#209975,#209976,#209977,
#209978,#209979,#209980,#209981,#209982,#209983,#209984,#209985,#209986,
#209987,#209988,#209989,#209990,#209991,#209992,#209993,#209994,#209995,
#209996,#209997,#209998,#209999,#210000,#210001,#210002,#210003,#210004,
#210005,#210006,#210007,#210008,#210009,#210010,#210011,#210012,#210013,
#210014,#210015,#210016,#210017,#210018,#210019,#210020,#210021,#210022,
#210023,#210024,#210025,#210026,#210027,#210028,#210029,#210030,#210031,
#210032,#210033,#210034,#210035,#210036,#210037,#210038,#210039,#210040,
#210041,#210042,#210043,#210044,#210045,#210046,#210047,#210048,#210049,
#210050,#210051,#210052,#210053,#210054,#210055,#210056,#210057,#210058,
#210059,#210060,#210061,#210062,#210063,#210064,#210065,#210066,#210067,
#210068,#210069,#210070,#210071,#210072,#210073,#210074,#210075,#210076,
#210077,#210078,#210079,#210080,#210081,#210082,#210083,#210084,#210085,
#210086,#210087,#210088,#210089,#210090,#210091,#210092,#210093,#210094,
#210095,#210096,#210097,#210098,#210099,#210100,#210101,#210102,#210103,
#210104,#210105,#210106,#210107,#210108,#210109,#210110,#210111,#210112,
#210113,#210114,#210115,#210116,#210117,#210118,#210119,#210120,#210121,
#210122,#210123,#210124,#210125,#210126,#210127,#210128,#210129),(#210130,
#210131,#210132,#210133,#210134,#210135,#210136,#210137,#210138,#210139,
#210140,#210141,#210142,#210143,#210144,#210145,#210146,#210147,#210148,
#210149,#210150,#210151,#210152,#210153,#210154,#210155,#210156,#210157,
#210158,#210159,#210160,#210161,#210162,#210163,#210164,#210165,#210166,
#210167,#210168,#210169,#210170,#210171,#210172,#210173,#210174,#210175,
#210176,#210177,#210178,#210179,#210180,#210181,#210182,#210183,#210184,
#210185,#210186,#210187,#210188,#210189,#210190,#210191,#210192,#210193,
#210194,#210195,#210196,#210197,#210198,#210199,#210200,#210201,#210202,
#210203,#210204,#210205,#210206,#210207,#210208,#210209,#210210,#210211,
#210212,#210213,#210214,#210215,#210216,#210217,#210218,#210219,#210220,
#210221,#210222,#210223,#210224,#210225,#210226,#210227,#210228,#210229,
#210230,#210231,#210232,#210233,#210234,#210235,#210236,#210237,#210238,
#210239,#210240,#210241,#210242,#210243,#210244,#210245,#210246,#210247,
#210248,#210249,#210250,#210251,#210252,#210253,#210254,#210255,#210256,
#210257,#210258,#210259,#210260,#210261,#210262,#210263,#210264,#210265,
#210266,#210267,#210268,#210269,#210270,#210271,#210272,#210273,#210274,
#210275,#210276,#210277,#210278,#210279,#210280,#210281,#210282,#210283,
#210284,#210285,#210286,#210287,#210288,#210289,#210290,#210291,#210292,
#210293,#210294,#210295,#210296,#210297,#210298,#210299,#210300,#210301,
#210302,#210303,#210304,#210305,#210306,#210307)),.UNSPECIFIED.,.F.,.F.,
 .F.,(4,4),(4,1,1,1,1,1,1,1,1,1,1,1,1,1,1,1,1,1,1,1,1,1,1,1,1,1,1,1,1,1,
1,1,1,1,1,1,1,1,1,1,1,1,1,1,1,1,1,1,1,1,1,1,1,1,1,1,1,1,1,1,1,1,1,1,1,1,
1,1,1,1,1,1,1,1,1,1,1,1,1,1,1,1,1,1,1,1,1,1,1,1,1,1,1,1,1,1,1,1,1,1,1,1,
1,1,1,1,1,1,1,1,1,1,1,1,1,1,1,1,1,1,1,1,1,1,1,1,1,1,1,1,1,1,1,1,1,1,1,1,
1,1,1,1,1,1,1,1,1,1,1,1,1,1,1,1,1,1,1,1,1,1,1,1,1,1,1,1,1,1,1,1,1,1,1,1,
1,4),(-0.000378201108638619,0.051592837406338),(14.3986268518925,15.3974633018543,
16.3962997518162,17.3951362017781,18.39397265174,19.3928091017018,20.3916455516637,
21.3904820016256,22.3893184515875,23.3881549015493,24.3869913515112,25.3858278014731,
26.3846642514349,27.3835007013968,28.3823371513587,29.3811736013206,30.3800100512824,
31.3788465012443,32.3776829512062,33.3765194011681,34.3753558511299,35.3741923010918,
36.3730287510537,37.3718652010156,38.3707016509774,39.3695381009393,40.3683745509012,
41.3672110008631,42.3660474508249,43.3648839007868,44.3637203507487,45.3625568007106,
46.3613932506724,47.3602297006343,48.3590661505962,49.3579026005581,50.3567390505199,
51.3555755004818,52.3544119504437,53.3532484004055,54.3520848503674,55.3509213003293,
56.3497577502912,57.348594200253,58.3474306502149,59.3462671001768,60.3451035501387,
61.3439400001005,62.3427764500624,63.3416129000243,64.3404493499862,65.339285799948,
66.3381222499099,67.3369586998718,68.3357951498337,69.3346315997955,70.3334680497574,
71.3323044997193,72.3311409496812,73.329977399643,74.3288138496049,75.3276502995668,
76.3264867495287,77.3253231994905,78.3241596494524,79.3229960994143,80.3218325493762,
81.320668999338,82.3195054492999,83.3183418992618,84.3171783492237,85.3160147991855,
86.3148512491474,87.3136876991093,88.3125241490712,89.311360599033,90.3101970489949,
91.3090334989568,92.3078699489186,93.3067063988805,94.3055428488424,95.3043792988043,
96.3032157487661,97.302052198728,98.3008886486899,99.2997250986518,100.298561548614,
101.297397998576,102.296234448537,103.295070898499,104.293907348461,105.292743798423,
106.291580248385,107.290416698347,108.289253148309,109.288089598271,110.286926048232,
111.285762498194,112.284598948156,113.283435398118,114.28227184808,115.281108298042,
116.279944748004,117.278781197966,118.277617647927,119.276454097889,120.275290547851,
121.274126997813,122.272963447775,123.271799897737,124.270636347699,125.26947279766,
126.268309247622,127.267145697584,128.265982147546,129.264818597508,130.26365504747,
131.262491497432,132.261327947394,133.260164397355,134.259000847317,135.257837297279,
136.256673747241,137.255510197203,138.254346647165,139.253183097127,140.252019547089,
141.25085599705,142.249692447012,143.248528896974,144.247365346936,145.246201796898,
146.24503824686,147.243874696822,148.242711146784,149.241547596745,150.240384046707,
151.239220496669,152.238056946631,153.236893396593,154.235729846555,155.234566296517,
156.233402746479,157.23223919644,158.231075646402,159.229912096364,160.228748546326,
161.227584996288,162.22642144625,163.225257896212,164.224094346174,165.222930796135,
166.221767246097,167.220603696059,168.219440146021,169.218276595983,170.217113045945,
171.215949495907,172.214785945869,173.21362239583,174.212458845792,175.211295295754,
176.210131745716,177.208968195678,178.20780464564,179.206641095602,180.205477545564,
181.204313995525,182.203150445487,183.201986895449,184.200823345411,185.199659795373,
186.198496245335,187.197332695297,188.196169145259,189.195445198776),
 .UNSPECIFIED.);
#167=B_SPLINE_SURFACE_WITH_KNOTS('',3,3,((#210399,#210400,#210401,#210402,
#210403,#210404,#210405,#210406,#210407,#210408,#210409,#210410,#210411,
#210412,#210413,#210414,#210415,#210416,#210417,#210418,#210419,#210420,
#210421,#210422,#210423,#210424,#210425,#210426,#210427,#210428,#210429,
#210430,#210431,#210432,#210433,#210434,#210435,#210436,#210437,#210438,
#210439,#210440,#210441,#210442,#210443,#210444,#210445,#210446,#210447,
#210448,#210449,#210450,#210451,#210452,#210453,#210454,#210455,#210456,
#210457,#210458,#210459,#210460,#210461,#210462,#210463,#210464,#210465,
#210466,#210467,#210468,#210469,#210470,#210471,#210472,#210473,#210474,
#210475,#210476,#210477,#210478,#210479,#210480,#210481,#210482,#210483,
#210484,#210485,#210486,#210487,#210488,#210489,#210490,#210491,#210492,
#210493,#210494,#210495,#210496,#210497,#210498,#210499,#210500,#210501,
#210502,#210503,#210504,#210505,#210506,#210507,#210508,#210509,#210510,
#210511,#210512,#210513,#210514,#210515,#210516,#210517,#210518,#210519,
#210520,#210521,#210522,#210523,#210524,#210525,#210526,#210527,#210528,
#210529,#210530,#210531,#210532,#210533,#210534,#210535,#210536,#210537,
#210538,#210539,#210540,#210541,#210542,#210543,#210544,#210545,#210546,
#210547,#210548,#210549,#210550,#210551,#210552,#210553,#210554,#210555,
#210556,#210557,#210558,#210559,#210560,#210561,#210562,#210563,#210564,
#210565,#210566,#210567,#210568,#210569,#210570,#210571,#210572,#210573,
#210574,#210575,#210576),(#210577,#210578,#210579,#210580,#210581,#210582,
#210583,#210584,#210585,#210586,#210587,#210588,#210589,#210590,#210591,
#210592,#210593,#210594,#210595,#210596,#210597,#210598,#210599,#210600,
#210601,#210602,#210603,#210604,#210605,#210606,#210607,#210608,#210609,
#210610,#210611,#210612,#210613,#210614,#210615,#210616,#210617,#210618,
#210619,#210620,#210621,#210622,#210623,#210624,#210625,#210626,#210627,
#210628,#210629,#210630,#210631,#210632,#210633,#210634,#210635,#210636,
#210637,#210638,#210639,#210640,#210641,#210642,#210643,#210644,#210645,
#210646,#210647,#210648,#210649,#210650,#210651,#210652,#210653,#210654,
#210655,#210656,#210657,#210658,#210659,#210660,#210661,#210662,#210663,
#210664,#210665,#210666,#210667,#210668,#210669,#210670,#210671,#210672,
#210673,#210674,#210675,#210676,#210677,#210678,#210679,#210680,#210681,
#210682,#210683,#210684,#210685,#210686,#210687,#210688,#210689,#210690,
#210691,#210692,#210693,#210694,#210695,#210696,#210697,#210698,#210699,
#210700,#210701,#210702,#210703,#210704,#210705,#210706,#210707,#210708,
#210709,#210710,#210711,#210712,#210713,#210714,#210715,#210716,#210717,
#210718,#210719,#210720,#210721,#210722,#210723,#210724,#210725,#210726,
#210727,#210728,#210729,#210730,#210731,#210732,#210733,#210734,#210735,
#210736,#210737,#210738,#210739,#210740,#210741,#210742,#210743,#210744,
#210745,#210746,#210747,#210748,#210749,#210750,#210751,#210752,#210753,
#210754),(#210755,#210756,#210757,#210758,#210759,#210760,#210761,#210762,
#210763,#210764,#210765,#210766,#210767,#210768,#210769,#210770,#210771,
#210772,#210773,#210774,#210775,#210776,#210777,#210778,#210779,#210780,
#210781,#210782,#210783,#210784,#210785,#210786,#210787,#210788,#210789,
#210790,#210791,#210792,#210793,#210794,#210795,#210796,#210797,#210798,
#210799,#210800,#210801,#210802,#210803,#210804,#210805,#210806,#210807,
#210808,#210809,#210810,#210811,#210812,#210813,#210814,#210815,#210816,
#210817,#210818,#210819,#210820,#210821,#210822,#210823,#210824,#210825,
#210826,#210827,#210828,#210829,#210830,#210831,#210832,#210833,#210834,
#210835,#210836,#210837,#210838,#210839,#210840,#210841,#210842,#210843,
#210844,#210845,#210846,#210847,#210848,#210849,#210850,#210851,#210852,
#210853,#210854,#210855,#210856,#210857,#210858,#210859,#210860,#210861,
#210862,#210863,#210864,#210865,#210866,#210867,#210868,#210869,#210870,
#210871,#210872,#210873,#210874,#210875,#210876,#210877,#210878,#210879,
#210880,#210881,#210882,#210883,#210884,#210885,#210886,#210887,#210888,
#210889,#210890,#210891,#210892,#210893,#210894,#210895,#210896,#210897,
#210898,#210899,#210900,#210901,#210902,#210903,#210904,#210905,#210906,
#210907,#210908,#210909,#210910,#210911,#210912,#210913,#210914,#210915,
#210916,#210917,#210918,#210919,#210920,#210921,#210922,#210923,#210924,
#210925,#210926,#210927,#210928,#210929,#210930,#210931,#210932),(#210933,
#210934,#210935,#210936,#210937,#210938,#210939,#210940,#210941,#210942,
#210943,#210944,#210945,#210946,#210947,#210948,#210949,#210950,#210951,
#210952,#210953,#210954,#210955,#210956,#210957,#210958,#210959,#210960,
#210961,#210962,#210963,#210964,#210965,#210966,#210967,#210968,#210969,
#210970,#210971,#210972,#210973,#210974,#210975,#210976,#210977,#210978,
#210979,#210980,#210981,#210982,#210983,#210984,#210985,#210986,#210987,
#210988,#210989,#210990,#210991,#210992,#210993,#210994,#210995,#210996,
#210997,#210998,#210999,#211000,#211001,#211002,#211003,#211004,#211005,
#211006,#211007,#211008,#211009,#211010,#211011,#211012,#211013,#211014,
#211015,#211016,#211017,#211018,#211019,#211020,#211021,#211022,#211023,
#211024,#211025,#211026,#211027,#211028,#211029,#211030,#211031,#211032,
#211033,#211034,#211035,#211036,#211037,#211038,#211039,#211040,#211041,
#211042,#211043,#211044,#211045,#211046,#211047,#211048,#211049,#211050,
#211051,#211052,#211053,#211054,#211055,#211056,#211057,#211058,#211059,
#211060,#211061,#211062,#211063,#211064,#211065,#211066,#211067,#211068,
#211069,#211070,#211071,#211072,#211073,#211074,#211075,#211076,#211077,
#211078,#211079,#211080,#211081,#211082,#211083,#211084,#211085,#211086,
#211087,#211088,#211089,#211090,#211091,#211092,#211093,#211094,#211095,
#211096,#211097,#211098,#211099,#211100,#211101,#211102,#211103,#211104,
#211105,#211106,#211107,#211108,#211109,#211110)),.UNSPECIFIED.,.F.,.F.,
 .F.,(4,4),(4,1,1,1,1,1,1,1,1,1,1,1,1,1,1,1,1,1,1,1,1,1,1,1,1,1,1,1,1,1,
1,1,1,1,1,1,1,1,1,1,1,1,1,1,1,1,1,1,1,1,1,1,1,1,1,1,1,1,1,1,1,1,1,1,1,1,
1,1,1,1,1,1,1,1,1,1,1,1,1,1,1,1,1,1,1,1,1,1,1,1,1,1,1,1,1,1,1,1,1,1,1,1,
1,1,1,1,1,1,1,1,1,1,1,1,1,1,1,1,1,1,1,1,1,1,1,1,1,1,1,1,1,1,1,1,1,1,1,1,
1,1,1,1,1,1,1,1,1,1,1,1,1,1,1,1,1,1,1,1,1,1,1,1,1,1,1,1,1,1,1,1,1,1,1,1,
1,4),(-0.000439572862182752,0.0515314610720388),(11.8664846616642,12.8657606844883,
13.8645971344502,14.8634335844121,15.8622700343739,16.8611064843358,17.8599429342977,
18.8587793842595,19.8576158342214,20.8564522841833,21.8552887341452,22.854125184107,
23.8529616340689,24.8517980840308,25.8506345339927,26.8494709839545,27.8483074339164,
28.8471438838783,29.8459803338402,30.844816783802,31.8436532337639,32.8424896837258,
33.8413261336877,34.8401625836495,35.8389990336114,36.8378354835733,37.8366719335352,
38.835508383497,39.8343448334589,40.8331812834208,41.8320177333826,42.8308541833445,
43.8296906333064,44.8285270832683,45.8273635332301,46.826199983192,47.8250364331539,
48.8238728831158,49.8227093330776,50.8215457830395,51.8203822330014,52.8192186829633,
53.8180551329251,54.816891582887,55.8157280328489,56.8145644828108,57.8134009327726,
58.8122373827345,59.8110738326964,60.8099102826583,61.8087467326201,62.807583182582,
63.8064196325439,64.8052560825058,65.8040925324676,66.8029289824295,67.8017654323914,
68.8006018823532,69.7994383323151,70.798274782277,71.7971112322389,72.7959476822007,
73.7947841321626,74.7936205821245,75.7924570320864,76.7912934820482,77.7901299320101,
78.788966381972,79.7878028319339,80.7866392818957,81.7854757318576,82.7843121818195,
83.7831486317814,84.7819850817432,85.7808215317051,86.779657981667,87.7784944316289,
88.7773308815907,89.7761673315526,90.7750037815145,91.7738402314764,92.7726766814382,
93.7715131314001,94.770349581362,95.7691860313239,96.7680224812857,97.7668589312476,
98.7656953812095,99.7645318311714,100.763368281133,101.762204731095,102.761041181057,
103.759877631019,104.758714080981,105.757550530943,106.756386980904,107.755223430866,
108.754059880828,109.75289633079,110.751732780752,111.750569230714,112.749405680676,
113.748242130638,114.747078580599,115.745915030561,116.744751480523,117.743587930485,
118.742424380447,119.741260830409,120.740097280371,121.738933730333,122.737770180294,
123.736606630256,124.735443080218,125.73427953018,126.733115980142,127.731952430104,
128.730788880066,129.729625330028,130.728461779989,131.727298229951,132.726134679913,
133.724971129875,134.723807579837,135.722644029799,136.721480479761,137.720316929723,
138.719153379684,139.717989829646,140.716826279608,141.71566272957,142.714499179532,
143.713335629494,144.712172079456,145.711008529418,146.709844979379,147.708681429341,
148.707517879303,149.706354329265,150.705190779227,151.704027229189,152.702863679151,
153.701700129113,154.700536579074,155.699373029036,156.698209478998,157.69704592896,
158.695882378922,159.694718828884,160.693555278846,161.692391728808,162.691228178769,
163.690064628731,164.688901078693,165.687737528655,166.686573978617,167.685410428579,
168.684246878541,169.683083328503,170.681919778464,171.680756228426,172.679592678388,
173.67842912835,174.677265578312,175.676102028274,176.674938478236,177.673774928198,
178.672611378159,179.671447828121,180.670284278083,181.669120728045,182.667957178007,
183.666793627969,184.665630077931,185.664466527893,186.663302977854),
 .UNSPECIFIED.);
#168=B_SPLINE_SURFACE_WITH_KNOTS('',3,3,((#211199,#211200,#211201,#211202,
#211203,#211204,#211205,#211206,#211207,#211208,#211209,#211210,#211211,
#211212,#211213,#211214,#211215,#211216,#211217,#211218,#211219,#211220,
#211221,#211222,#211223,#211224,#211225,#211226,#211227,#211228,#211229,
#211230,#211231,#211232,#211233,#211234,#211235,#211236,#211237,#211238,
#211239,#211240,#211241,#211242,#211243,#211244,#211245,#211246,#211247,
#211248,#211249,#211250,#211251,#211252,#211253,#211254,#211255,#211256,
#211257,#211258,#211259,#211260,#211261,#211262,#211263,#211264,#211265,
#211266,#211267,#211268,#211269,#211270,#211271,#211272,#211273,#211274,
#211275,#211276,#211277,#211278,#211279,#211280,#211281,#211282,#211283,
#211284,#211285,#211286,#211287,#211288,#211289,#211290,#211291,#211292,
#211293,#211294,#211295,#211296,#211297,#211298,#211299,#211300,#211301,
#211302,#211303,#211304,#211305,#211306,#211307,#211308,#211309,#211310,
#211311,#211312,#211313,#211314,#211315,#211316,#211317,#211318,#211319,
#211320,#211321,#211322,#211323,#211324,#211325,#211326,#211327,#211328,
#211329,#211330,#211331,#211332,#211333,#211334,#211335,#211336,#211337,
#211338,#211339,#211340,#211341,#211342,#211343,#211344,#211345,#211346,
#211347,#211348,#211349,#211350,#211351,#211352,#211353,#211354,#211355,
#211356,#211357,#211358,#211359,#211360,#211361,#211362,#211363,#211364,
#211365,#211366,#211367,#211368,#211369,#211370,#211371,#211372,#211373,
#211374,#211375,#211376),(#211377,#211378,#211379,#211380,#211381,#211382,
#211383,#211384,#211385,#211386,#211387,#211388,#211389,#211390,#211391,
#211392,#211393,#211394,#211395,#211396,#211397,#211398,#211399,#211400,
#211401,#211402,#211403,#211404,#211405,#211406,#211407,#211408,#211409,
#211410,#211411,#211412,#211413,#211414,#211415,#211416,#211417,#211418,
#211419,#211420,#211421,#211422,#211423,#211424,#211425,#211426,#211427,
#211428,#211429,#211430,#211431,#211432,#211433,#211434,#211435,#211436,
#211437,#211438,#211439,#211440,#211441,#211442,#211443,#211444,#211445,
#211446,#211447,#211448,#211449,#211450,#211451,#211452,#211453,#211454,
#211455,#211456,#211457,#211458,#211459,#211460,#211461,#211462,#211463,
#211464,#211465,#211466,#211467,#211468,#211469,#211470,#211471,#211472,
#211473,#211474,#211475,#211476,#211477,#211478,#211479,#211480,#211481,
#211482,#211483,#211484,#211485,#211486,#211487,#211488,#211489,#211490,
#211491,#211492,#211493,#211494,#211495,#211496,#211497,#211498,#211499,
#211500,#211501,#211502,#211503,#211504,#211505,#211506,#211507,#211508,
#211509,#211510,#211511,#211512,#211513,#211514,#211515,#211516,#211517,
#211518,#211519,#211520,#211521,#211522,#211523,#211524,#211525,#211526,
#211527,#211528,#211529,#211530,#211531,#211532,#211533,#211534,#211535,
#211536,#211537,#211538,#211539,#211540,#211541,#211542,#211543,#211544,
#211545,#211546,#211547,#211548,#211549,#211550,#211551,#211552,#211553,
#211554),(#211555,#211556,#211557,#211558,#211559,#211560,#211561,#211562,
#211563,#211564,#211565,#211566,#211567,#211568,#211569,#211570,#211571,
#211572,#211573,#211574,#211575,#211576,#211577,#211578,#211579,#211580,
#211581,#211582,#211583,#211584,#211585,#211586,#211587,#211588,#211589,
#211590,#211591,#211592,#211593,#211594,#211595,#211596,#211597,#211598,
#211599,#211600,#211601,#211602,#211603,#211604,#211605,#211606,#211607,
#211608,#211609,#211610,#211611,#211612,#211613,#211614,#211615,#211616,
#211617,#211618,#211619,#211620,#211621,#211622,#211623,#211624,#211625,
#211626,#211627,#211628,#211629,#211630,#211631,#211632,#211633,#211634,
#211635,#211636,#211637,#211638,#211639,#211640,#211641,#211642,#211643,
#211644,#211645,#211646,#211647,#211648,#211649,#211650,#211651,#211652,
#211653,#211654,#211655,#211656,#211657,#211658,#211659,#211660,#211661,
#211662,#211663,#211664,#211665,#211666,#211667,#211668,#211669,#211670,
#211671,#211672,#211673,#211674,#211675,#211676,#211677,#211678,#211679,
#211680,#211681,#211682,#211683,#211684,#211685,#211686,#211687,#211688,
#211689,#211690,#211691,#211692,#211693,#211694,#211695,#211696,#211697,
#211698,#211699,#211700,#211701,#211702,#211703,#211704,#211705,#211706,
#211707,#211708,#211709,#211710,#211711,#211712,#211713,#211714,#211715,
#211716,#211717,#211718,#211719,#211720,#211721,#211722,#211723,#211724,
#211725,#211726,#211727,#211728,#211729,#211730,#211731,#211732),(#211733,
#211734,#211735,#211736,#211737,#211738,#211739,#211740,#211741,#211742,
#211743,#211744,#211745,#211746,#211747,#211748,#211749,#211750,#211751,
#211752,#211753,#211754,#211755,#211756,#211757,#211758,#211759,#211760,
#211761,#211762,#211763,#211764,#211765,#211766,#211767,#211768,#211769,
#211770,#211771,#211772,#211773,#211774,#211775,#211776,#211777,#211778,
#211779,#211780,#211781,#211782,#211783,#211784,#211785,#211786,#211787,
#211788,#211789,#211790,#211791,#211792,#211793,#211794,#211795,#211796,
#211797,#211798,#211799,#211800,#211801,#211802,#211803,#211804,#211805,
#211806,#211807,#211808,#211809,#211810,#211811,#211812,#211813,#211814,
#211815,#211816,#211817,#211818,#211819,#211820,#211821,#211822,#211823,
#211824,#211825,#211826,#211827,#211828,#211829,#211830,#211831,#211832,
#211833,#211834,#211835,#211836,#211837,#211838,#211839,#211840,#211841,
#211842,#211843,#211844,#211845,#211846,#211847,#211848,#211849,#211850,
#211851,#211852,#211853,#211854,#211855,#211856,#211857,#211858,#211859,
#211860,#211861,#211862,#211863,#211864,#211865,#211866,#211867,#211868,
#211869,#211870,#211871,#211872,#211873,#211874,#211875,#211876,#211877,
#211878,#211879,#211880,#211881,#211882,#211883,#211884,#211885,#211886,
#211887,#211888,#211889,#211890,#211891,#211892,#211893,#211894,#211895,
#211896,#211897,#211898,#211899,#211900,#211901,#211902,#211903,#211904,
#211905,#211906,#211907,#211908,#211909,#211910)),.UNSPECIFIED.,.F.,.F.,
 .F.,(4,4),(4,1,1,1,1,1,1,1,1,1,1,1,1,1,1,1,1,1,1,1,1,1,1,1,1,1,1,1,1,1,
1,1,1,1,1,1,1,1,1,1,1,1,1,1,1,1,1,1,1,1,1,1,1,1,1,1,1,1,1,1,1,1,1,1,1,1,
1,1,1,1,1,1,1,1,1,1,1,1,1,1,1,1,1,1,1,1,1,1,1,1,1,1,1,1,1,1,1,1,1,1,1,1,
1,1,1,1,1,1,1,1,1,1,1,1,1,1,1,1,1,1,1,1,1,1,1,1,1,1,1,1,1,1,1,1,1,1,1,1,
1,1,1,1,1,1,1,1,1,1,1,1,1,1,1,1,1,1,1,1,1,1,1,1,1,1,1,1,1,1,1,1,1,1,1,1,
1,4),(-0.000378192696997217,0.0515928473073539),(14.3986268518925,15.3974633018543,
16.3962997518162,17.3951362017781,18.39397265174,19.3928091017018,20.3916455516637,
21.3904820016256,22.3893184515875,23.3881549015493,24.3869913515112,25.3858278014731,
26.3846642514349,27.3835007013968,28.3823371513587,29.3811736013206,30.3800100512824,
31.3788465012443,32.3776829512062,33.3765194011681,34.3753558511299,35.3741923010918,
36.3730287510537,37.3718652010156,38.3707016509774,39.3695381009393,40.3683745509012,
41.3672110008631,42.3660474508249,43.3648839007868,44.3637203507487,45.3625568007106,
46.3613932506724,47.3602297006343,48.3590661505962,49.3579026005581,50.3567390505199,
51.3555755004818,52.3544119504437,53.3532484004055,54.3520848503674,55.3509213003293,
56.3497577502912,57.348594200253,58.3474306502149,59.3462671001768,60.3451035501387,
61.3439400001005,62.3427764500624,63.3416129000243,64.3404493499862,65.339285799948,
66.3381222499099,67.3369586998718,68.3357951498337,69.3346315997955,70.3334680497574,
71.3323044997193,72.3311409496812,73.329977399643,74.3288138496049,75.3276502995668,
76.3264867495287,77.3253231994905,78.3241596494524,79.3229960994143,80.3218325493762,
81.320668999338,82.3195054492999,83.3183418992618,84.3171783492237,85.3160147991855,
86.3148512491474,87.3136876991093,88.3125241490712,89.311360599033,90.3101970489949,
91.3090334989568,92.3078699489186,93.3067063988805,94.3055428488424,95.3043792988043,
96.3032157487661,97.302052198728,98.3008886486899,99.2997250986518,100.298561548614,
101.297397998576,102.296234448537,103.295070898499,104.293907348461,105.292743798423,
106.291580248385,107.290416698347,108.289253148309,109.288089598271,110.286926048232,
111.285762498194,112.284598948156,113.283435398118,114.28227184808,115.281108298042,
116.279944748004,117.278781197966,118.277617647927,119.276454097889,120.275290547851,
121.274126997813,122.272963447775,123.271799897737,124.270636347699,125.26947279766,
126.268309247622,127.267145697584,128.265982147546,129.264818597508,130.26365504747,
131.262491497432,132.261327947394,133.260164397355,134.259000847317,135.257837297279,
136.256673747241,137.255510197203,138.254346647165,139.253183097127,140.252019547089,
141.25085599705,142.249692447012,143.248528896974,144.247365346936,145.246201796898,
146.24503824686,147.243874696822,148.242711146784,149.241547596745,150.240384046707,
151.239220496669,152.238056946631,153.236893396593,154.235729846555,155.234566296517,
156.233402746479,157.23223919644,158.231075646402,159.229912096364,160.228748546326,
161.227584996288,162.22642144625,163.225257896212,164.224094346174,165.222930796135,
166.221767246097,167.220603696059,168.219440146021,169.218276595983,170.217113045945,
171.215949495907,172.214785945869,173.21362239583,174.212458845792,175.211295295754,
176.210131745716,177.208968195678,178.20780464564,179.206641095602,180.205477545564,
181.204313995525,182.203150445487,183.201986895449,184.200823345411,185.199659795373,
186.198496245335,187.197332695297,188.196169145259,189.195445208677),
 .UNSPECIFIED.);
#169=B_SPLINE_SURFACE_WITH_KNOTS('',3,3,((#211999,#212000,#212001,#212002,
#212003,#212004,#212005,#212006,#212007,#212008,#212009,#212010,#212011,
#212012,#212013,#212014,#212015,#212016,#212017,#212018,#212019,#212020,
#212021,#212022,#212023,#212024,#212025,#212026,#212027,#212028,#212029,
#212030,#212031,#212032,#212033,#212034,#212035,#212036,#212037,#212038,
#212039,#212040,#212041,#212042,#212043,#212044,#212045,#212046,#212047,
#212048,#212049,#212050,#212051,#212052,#212053,#212054,#212055,#212056,
#212057,#212058,#212059,#212060,#212061,#212062,#212063,#212064,#212065,
#212066,#212067,#212068,#212069,#212070,#212071,#212072,#212073,#212074,
#212075,#212076,#212077,#212078,#212079,#212080,#212081,#212082,#212083,
#212084,#212085,#212086,#212087,#212088,#212089,#212090,#212091,#212092,
#212093,#212094,#212095,#212096,#212097,#212098,#212099,#212100,#212101,
#212102,#212103,#212104,#212105,#212106,#212107,#212108,#212109,#212110,
#212111,#212112,#212113,#212114,#212115,#212116,#212117,#212118,#212119,
#212120,#212121,#212122,#212123,#212124,#212125,#212126,#212127,#212128,
#212129,#212130,#212131,#212132,#212133,#212134,#212135,#212136,#212137,
#212138,#212139,#212140,#212141,#212142,#212143,#212144,#212145,#212146,
#212147,#212148,#212149,#212150,#212151,#212152,#212153,#212154,#212155,
#212156,#212157,#212158,#212159,#212160,#212161,#212162,#212163,#212164,
#212165,#212166,#212167,#212168,#212169,#212170,#212171,#212172,#212173,
#212174,#212175,#212176),(#212177,#212178,#212179,#212180,#212181,#212182,
#212183,#212184,#212185,#212186,#212187,#212188,#212189,#212190,#212191,
#212192,#212193,#212194,#212195,#212196,#212197,#212198,#212199,#212200,
#212201,#212202,#212203,#212204,#212205,#212206,#212207,#212208,#212209,
#212210,#212211,#212212,#212213,#212214,#212215,#212216,#212217,#212218,
#212219,#212220,#212221,#212222,#212223,#212224,#212225,#212226,#212227,
#212228,#212229,#212230,#212231,#212232,#212233,#212234,#212235,#212236,
#212237,#212238,#212239,#212240,#212241,#212242,#212243,#212244,#212245,
#212246,#212247,#212248,#212249,#212250,#212251,#212252,#212253,#212254,
#212255,#212256,#212257,#212258,#212259,#212260,#212261,#212262,#212263,
#212264,#212265,#212266,#212267,#212268,#212269,#212270,#212271,#212272,
#212273,#212274,#212275,#212276,#212277,#212278,#212279,#212280,#212281,
#212282,#212283,#212284,#212285,#212286,#212287,#212288,#212289,#212290,
#212291,#212292,#212293,#212294,#212295,#212296,#212297,#212298,#212299,
#212300,#212301,#212302,#212303,#212304,#212305,#212306,#212307,#212308,
#212309,#212310,#212311,#212312,#212313,#212314,#212315,#212316,#212317,
#212318,#212319,#212320,#212321,#212322,#212323,#212324,#212325,#212326,
#212327,#212328,#212329,#212330,#212331,#212332,#212333,#212334,#212335,
#212336,#212337,#212338,#212339,#212340,#212341,#212342,#212343,#212344,
#212345,#212346,#212347,#212348,#212349,#212350,#212351,#212352,#212353,
#212354),(#212355,#212356,#212357,#212358,#212359,#212360,#212361,#212362,
#212363,#212364,#212365,#212366,#212367,#212368,#212369,#212370,#212371,
#212372,#212373,#212374,#212375,#212376,#212377,#212378,#212379,#212380,
#212381,#212382,#212383,#212384,#212385,#212386,#212387,#212388,#212389,
#212390,#212391,#212392,#212393,#212394,#212395,#212396,#212397,#212398,
#212399,#212400,#212401,#212402,#212403,#212404,#212405,#212406,#212407,
#212408,#212409,#212410,#212411,#212412,#212413,#212414,#212415,#212416,
#212417,#212418,#212419,#212420,#212421,#212422,#212423,#212424,#212425,
#212426,#212427,#212428,#212429,#212430,#212431,#212432,#212433,#212434,
#212435,#212436,#212437,#212438,#212439,#212440,#212441,#212442,#212443,
#212444,#212445,#212446,#212447,#212448,#212449,#212450,#212451,#212452,
#212453,#212454,#212455,#212456,#212457,#212458,#212459,#212460,#212461,
#212462,#212463,#212464,#212465,#212466,#212467,#212468,#212469,#212470,
#212471,#212472,#212473,#212474,#212475,#212476,#212477,#212478,#212479,
#212480,#212481,#212482,#212483,#212484,#212485,#212486,#212487,#212488,
#212489,#212490,#212491,#212492,#212493,#212494,#212495,#212496,#212497,
#212498,#212499,#212500,#212501,#212502,#212503,#212504,#212505,#212506,
#212507,#212508,#212509,#212510,#212511,#212512,#212513,#212514,#212515,
#212516,#212517,#212518,#212519,#212520,#212521,#212522,#212523,#212524,
#212525,#212526,#212527,#212528,#212529,#212530,#212531,#212532),(#212533,
#212534,#212535,#212536,#212537,#212538,#212539,#212540,#212541,#212542,
#212543,#212544,#212545,#212546,#212547,#212548,#212549,#212550,#212551,
#212552,#212553,#212554,#212555,#212556,#212557,#212558,#212559,#212560,
#212561,#212562,#212563,#212564,#212565,#212566,#212567,#212568,#212569,
#212570,#212571,#212572,#212573,#212574,#212575,#212576,#212577,#212578,
#212579,#212580,#212581,#212582,#212583,#212584,#212585,#212586,#212587,
#212588,#212589,#212590,#212591,#212592,#212593,#212594,#212595,#212596,
#212597,#212598,#212599,#212600,#212601,#212602,#212603,#212604,#212605,
#212606,#212607,#212608,#212609,#212610,#212611,#212612,#212613,#212614,
#212615,#212616,#212617,#212618,#212619,#212620,#212621,#212622,#212623,
#212624,#212625,#212626,#212627,#212628,#212629,#212630,#212631,#212632,
#212633,#212634,#212635,#212636,#212637,#212638,#212639,#212640,#212641,
#212642,#212643,#212644,#212645,#212646,#212647,#212648,#212649,#212650,
#212651,#212652,#212653,#212654,#212655,#212656,#212657,#212658,#212659,
#212660,#212661,#212662,#212663,#212664,#212665,#212666,#212667,#212668,
#212669,#212670,#212671,#212672,#212673,#212674,#212675,#212676,#212677,
#212678,#212679,#212680,#212681,#212682,#212683,#212684,#212685,#212686,
#212687,#212688,#212689,#212690,#212691,#212692,#212693,#212694,#212695,
#212696,#212697,#212698,#212699,#212700,#212701,#212702,#212703,#212704,
#212705,#212706,#212707,#212708,#212709,#212710)),.UNSPECIFIED.,.F.,.F.,
 .F.,(4,4),(4,1,1,1,1,1,1,1,1,1,1,1,1,1,1,1,1,1,1,1,1,1,1,1,1,1,1,1,1,1,
1,1,1,1,1,1,1,1,1,1,1,1,1,1,1,1,1,1,1,1,1,1,1,1,1,1,1,1,1,1,1,1,1,1,1,1,
1,1,1,1,1,1,1,1,1,1,1,1,1,1,1,1,1,1,1,1,1,1,1,1,1,1,1,1,1,1,1,1,1,1,1,1,
1,1,1,1,1,1,1,1,1,1,1,1,1,1,1,1,1,1,1,1,1,1,1,1,1,1,1,1,1,1,1,1,1,1,1,1,
1,1,1,1,1,1,1,1,1,1,1,1,1,1,1,1,1,1,1,1,1,1,1,1,1,1,1,1,1,1,1,1,1,1,1,1,
1,4),(-0.000439572128272221,0.0515314616970906),(11.8664846623981,12.8657606844883,
13.8645971344502,14.8634335844121,15.8622700343739,16.8611064843358,17.8599429342977,
18.8587793842596,19.8576158342214,20.8564522841833,21.8552887341452,22.854125184107,
23.8529616340689,24.8517980840308,25.8506345339927,26.8494709839545,27.8483074339164,
28.8471438838783,29.8459803338402,30.844816783802,31.8436532337639,32.8424896837258,
33.8413261336877,34.8401625836495,35.8389990336114,36.8378354835733,37.8366719335352,
38.835508383497,39.8343448334589,40.8331812834208,41.8320177333827,42.8308541833445,
43.8296906333064,44.8285270832683,45.8273635332302,46.826199983192,47.8250364331539,
48.8238728831158,49.8227093330777,50.8215457830395,51.8203822330014,52.8192186829633,
53.8180551329252,54.816891582887,55.8157280328489,56.8145644828108,57.8134009327727,
58.8122373827345,59.8110738326964,60.8099102826583,61.8087467326202,62.807583182582,
63.8064196325439,64.8052560825058,65.8040925324676,66.8029289824295,67.8017654323914,
68.8006018823533,69.7994383323151,70.798274782277,71.7971112322389,72.7959476822008,
73.7947841321626,74.7936205821245,75.7924570320864,76.7912934820483,77.7901299320101,
78.788966381972,79.7878028319339,80.7866392818958,81.7854757318576,82.7843121818195,
83.7831486317814,84.7819850817433,85.7808215317051,86.779657981667,87.7784944316289,
88.7773308815908,89.7761673315526,90.7750037815145,91.7738402314764,92.7726766814383,
93.7715131314001,94.770349581362,95.7691860313239,96.7680224812858,97.7668589312476,
98.7656953812095,99.7645318311714,100.763368281133,101.762204731095,102.761041181057,
103.759877631019,104.758714080981,105.757550530943,106.756386980905,107.755223430866,
108.754059880828,109.75289633079,110.751732780752,111.750569230714,112.749405680676,
113.748242130638,114.747078580599,115.745915030561,116.744751480523,117.743587930485,
118.742424380447,119.741260830409,120.740097280371,121.738933730333,122.737770180294,
123.736606630256,124.735443080218,125.73427953018,126.733115980142,127.731952430104,
128.730788880066,129.729625330028,130.728461779989,131.727298229951,132.726134679913,
133.724971129875,134.723807579837,135.722644029799,136.721480479761,137.720316929723,
138.719153379684,139.717989829646,140.716826279608,141.71566272957,142.714499179532,
143.713335629494,144.712172079456,145.711008529418,146.709844979379,147.708681429341,
148.707517879303,149.706354329265,150.705190779227,151.704027229189,152.702863679151,
153.701700129113,154.700536579074,155.699373029036,156.698209478998,157.69704592896,
158.695882378922,159.694718828884,160.693555278846,161.692391728808,162.691228178769,
163.690064628731,164.688901078693,165.687737528655,166.686573978617,167.685410428579,
168.684246878541,169.683083328503,170.681919778464,171.680756228426,172.679592678388,
173.67842912835,174.677265578312,175.676102028274,176.674938478236,177.673774928198,
178.672611378159,179.671447828121,180.670284278083,181.669120728045,182.667957178007,
183.666793627969,184.665630077931,185.664466527893,186.663302977854),
 .UNSPECIFIED.);
#170=B_SPLINE_SURFACE_WITH_KNOTS('',3,3,((#212799,#212800,#212801,#212802,
#212803,#212804,#212805,#212806,#212807,#212808,#212809,#212810,#212811,
#212812,#212813,#212814,#212815,#212816,#212817,#212818,#212819,#212820,
#212821,#212822,#212823,#212824,#212825,#212826,#212827,#212828,#212829,
#212830,#212831,#212832,#212833,#212834,#212835,#212836,#212837,#212838,
#212839,#212840,#212841,#212842,#212843,#212844,#212845,#212846,#212847,
#212848,#212849,#212850,#212851,#212852,#212853,#212854,#212855,#212856,
#212857,#212858,#212859,#212860,#212861,#212862,#212863,#212864,#212865,
#212866,#212867,#212868,#212869,#212870,#212871,#212872,#212873,#212874,
#212875,#212876,#212877,#212878,#212879,#212880,#212881,#212882,#212883,
#212884,#212885,#212886,#212887,#212888,#212889,#212890,#212891,#212892,
#212893,#212894,#212895,#212896,#212897,#212898,#212899,#212900,#212901,
#212902,#212903,#212904,#212905,#212906,#212907,#212908,#212909,#212910,
#212911,#212912,#212913,#212914,#212915,#212916,#212917,#212918,#212919,
#212920,#212921,#212922,#212923,#212924,#212925,#212926,#212927,#212928,
#212929,#212930,#212931,#212932,#212933,#212934,#212935,#212936,#212937,
#212938,#212939,#212940,#212941,#212942,#212943,#212944,#212945,#212946,
#212947,#212948,#212949,#212950,#212951,#212952,#212953,#212954,#212955,
#212956,#212957,#212958,#212959,#212960,#212961,#212962,#212963,#212964,
#212965,#212966,#212967,#212968,#212969,#212970,#212971,#212972,#212973,
#212974,#212975,#212976),(#212977,#212978,#212979,#212980,#212981,#212982,
#212983,#212984,#212985,#212986,#212987,#212988,#212989,#212990,#212991,
#212992,#212993,#212994,#212995,#212996,#212997,#212998,#212999,#213000,
#213001,#213002,#213003,#213004,#213005,#213006,#213007,#213008,#213009,
#213010,#213011,#213012,#213013,#213014,#213015,#213016,#213017,#213018,
#213019,#213020,#213021,#213022,#213023,#213024,#213025,#213026,#213027,
#213028,#213029,#213030,#213031,#213032,#213033,#213034,#213035,#213036,
#213037,#213038,#213039,#213040,#213041,#213042,#213043,#213044,#213045,
#213046,#213047,#213048,#213049,#213050,#213051,#213052,#213053,#213054,
#213055,#213056,#213057,#213058,#213059,#213060,#213061,#213062,#213063,
#213064,#213065,#213066,#213067,#213068,#213069,#213070,#213071,#213072,
#213073,#213074,#213075,#213076,#213077,#213078,#213079,#213080,#213081,
#213082,#213083,#213084,#213085,#213086,#213087,#213088,#213089,#213090,
#213091,#213092,#213093,#213094,#213095,#213096,#213097,#213098,#213099,
#213100,#213101,#213102,#213103,#213104,#213105,#213106,#213107,#213108,
#213109,#213110,#213111,#213112,#213113,#213114,#213115,#213116,#213117,
#213118,#213119,#213120,#213121,#213122,#213123,#213124,#213125,#213126,
#213127,#213128,#213129,#213130,#213131,#213132,#213133,#213134,#213135,
#213136,#213137,#213138,#213139,#213140,#213141,#213142,#213143,#213144,
#213145,#213146,#213147,#213148,#213149,#213150,#213151,#213152,#213153,
#213154),(#213155,#213156,#213157,#213158,#213159,#213160,#213161,#213162,
#213163,#213164,#213165,#213166,#213167,#213168,#213169,#213170,#213171,
#213172,#213173,#213174,#213175,#213176,#213177,#213178,#213179,#213180,
#213181,#213182,#213183,#213184,#213185,#213186,#213187,#213188,#213189,
#213190,#213191,#213192,#213193,#213194,#213195,#213196,#213197,#213198,
#213199,#213200,#213201,#213202,#213203,#213204,#213205,#213206,#213207,
#213208,#213209,#213210,#213211,#213212,#213213,#213214,#213215,#213216,
#213217,#213218,#213219,#213220,#213221,#213222,#213223,#213224,#213225,
#213226,#213227,#213228,#213229,#213230,#213231,#213232,#213233,#213234,
#213235,#213236,#213237,#213238,#213239,#213240,#213241,#213242,#213243,
#213244,#213245,#213246,#213247,#213248,#213249,#213250,#213251,#213252,
#213253,#213254,#213255,#213256,#213257,#213258,#213259,#213260,#213261,
#213262,#213263,#213264,#213265,#213266,#213267,#213268,#213269,#213270,
#213271,#213272,#213273,#213274,#213275,#213276,#213277,#213278,#213279,
#213280,#213281,#213282,#213283,#213284,#213285,#213286,#213287,#213288,
#213289,#213290,#213291,#213292,#213293,#213294,#213295,#213296,#213297,
#213298,#213299,#213300,#213301,#213302,#213303,#213304,#213305,#213306,
#213307,#213308,#213309,#213310,#213311,#213312,#213313,#213314,#213315,
#213316,#213317,#213318,#213319,#213320,#213321,#213322,#213323,#213324,
#213325,#213326,#213327,#213328,#213329,#213330,#213331,#213332),(#213333,
#213334,#213335,#213336,#213337,#213338,#213339,#213340,#213341,#213342,
#213343,#213344,#213345,#213346,#213347,#213348,#213349,#213350,#213351,
#213352,#213353,#213354,#213355,#213356,#213357,#213358,#213359,#213360,
#213361,#213362,#213363,#213364,#213365,#213366,#213367,#213368,#213369,
#213370,#213371,#213372,#213373,#213374,#213375,#213376,#213377,#213378,
#213379,#213380,#213381,#213382,#213383,#213384,#213385,#213386,#213387,
#213388,#213389,#213390,#213391,#213392,#213393,#213394,#213395,#213396,
#213397,#213398,#213399,#213400,#213401,#213402,#213403,#213404,#213405,
#213406,#213407,#213408,#213409,#213410,#213411,#213412,#213413,#213414,
#213415,#213416,#213417,#213418,#213419,#213420,#213421,#213422,#213423,
#213424,#213425,#213426,#213427,#213428,#213429,#213430,#213431,#213432,
#213433,#213434,#213435,#213436,#213437,#213438,#213439,#213440,#213441,
#213442,#213443,#213444,#213445,#213446,#213447,#213448,#213449,#213450,
#213451,#213452,#213453,#213454,#213455,#213456,#213457,#213458,#213459,
#213460,#213461,#213462,#213463,#213464,#213465,#213466,#213467,#213468,
#213469,#213470,#213471,#213472,#213473,#213474,#213475,#213476,#213477,
#213478,#213479,#213480,#213481,#213482,#213483,#213484,#213485,#213486,
#213487,#213488,#213489,#213490,#213491,#213492,#213493,#213494,#213495,
#213496,#213497,#213498,#213499,#213500,#213501,#213502,#213503,#213504,
#213505,#213506,#213507,#213508,#213509,#213510)),.UNSPECIFIED.,.F.,.F.,
 .F.,(4,4),(4,1,1,1,1,1,1,1,1,1,1,1,1,1,1,1,1,1,1,1,1,1,1,1,1,1,1,1,1,1,
1,1,1,1,1,1,1,1,1,1,1,1,1,1,1,1,1,1,1,1,1,1,1,1,1,1,1,1,1,1,1,1,1,1,1,1,
1,1,1,1,1,1,1,1,1,1,1,1,1,1,1,1,1,1,1,1,1,1,1,1,1,1,1,1,1,1,1,1,1,1,1,1,
1,1,1,1,1,1,1,1,1,1,1,1,1,1,1,1,1,1,1,1,1,1,1,1,1,1,1,1,1,1,1,1,1,1,1,1,
1,1,1,1,1,1,1,1,1,1,1,1,1,1,1,1,1,1,1,1,1,1,1,1,1,1,1,1,1,1,1,1,1,1,1,1,
1,4),(-0.000378196170333693,0.0515928432182127),(14.3986268518925,15.3974633018543,
16.3962997518162,17.3951362017781,18.39397265174,19.3928091017018,20.3916455516637,
21.3904820016256,22.3893184515875,23.3881549015493,24.3869913515112,25.3858278014731,
26.384664251435,27.3835007013968,28.3823371513587,29.3811736013206,30.3800100512825,
31.3788465012443,32.3776829512062,33.3765194011681,34.37535585113,35.3741923010918,
36.3730287510537,37.3718652010156,38.3707016509774,39.3695381009393,40.3683745509012,
41.3672110008631,42.3660474508249,43.3648839007868,44.3637203507487,45.3625568007106,
46.3613932506724,47.3602297006343,48.3590661505962,49.3579026005581,50.3567390505199,
51.3555755004818,52.3544119504437,53.3532484004056,54.3520848503674,55.3509213003293,
56.3497577502912,57.3485942002531,58.3474306502149,59.3462671001768,60.3451035501387,
61.3439400001006,62.3427764500624,63.3416129000243,64.3404493499862,65.3392857999481,
66.3381222499099,67.3369586998718,68.3357951498337,69.3346315997956,70.3334680497574,
71.3323044997193,72.3311409496812,73.3299773996431,74.3288138496049,75.3276502995668,
76.3264867495287,77.3253231994906,78.3241596494524,79.3229960994143,80.3218325493762,
81.3206689993381,82.3195054492999,83.3183418992618,84.3171783492237,85.3160147991856,
86.3148512491474,87.3136876991093,88.3125241490712,89.3113605990331,90.3101970489949,
91.3090334989568,92.3078699489187,93.3067063988806,94.3055428488424,95.3043792988043,
96.3032157487662,97.302052198728,98.3008886486899,99.2997250986518,100.298561548614,
101.297397998576,102.296234448537,103.295070898499,104.293907348461,105.292743798423,
106.291580248385,107.290416698347,108.289253148309,109.288089598271,110.286926048232,
111.285762498194,112.284598948156,113.283435398118,114.28227184808,115.281108298042,
116.279944748004,117.278781197966,118.277617647927,119.276454097889,120.275290547851,
121.274126997813,122.272963447775,123.271799897737,124.270636347699,125.269472797661,
126.268309247622,127.267145697584,128.265982147546,129.264818597508,130.26365504747,
131.262491497432,132.261327947394,133.260164397356,134.259000847317,135.257837297279,
136.256673747241,137.255510197203,138.254346647165,139.253183097127,140.252019547089,
141.250855997051,142.249692447012,143.248528896974,144.247365346936,145.246201796898,
146.24503824686,147.243874696822,148.242711146784,149.241547596746,150.240384046707,
151.239220496669,152.238056946631,153.236893396593,154.235729846555,155.234566296517,
156.233402746479,157.232239196441,158.231075646402,159.229912096364,160.228748546326,
161.227584996288,162.22642144625,163.225257896212,164.224094346174,165.222930796136,
166.221767246097,167.220603696059,168.219440146021,169.218276595983,170.217113045945,
171.215949495907,172.214785945869,173.21362239583,174.212458845792,175.211295295754,
176.210131745716,177.208968195678,178.20780464564,179.206641095602,180.205477545564,
181.204313995525,182.203150445487,183.201986895449,184.200823345411,185.199659795373,
186.198496245335,187.197332695297,188.196169145259,189.195445204588),
 .UNSPECIFIED.);
#171=B_SPLINE_SURFACE_WITH_KNOTS('',3,3,((#213599,#213600,#213601,#213602,
#213603,#213604,#213605,#213606,#213607,#213608,#213609,#213610,#213611,
#213612,#213613,#213614,#213615,#213616,#213617,#213618,#213619,#213620,
#213621,#213622,#213623,#213624,#213625,#213626,#213627,#213628,#213629,
#213630,#213631,#213632,#213633,#213634,#213635,#213636,#213637,#213638,
#213639,#213640,#213641,#213642,#213643,#213644,#213645,#213646,#213647,
#213648,#213649,#213650,#213651,#213652,#213653,#213654,#213655,#213656,
#213657,#213658,#213659,#213660,#213661,#213662,#213663,#213664,#213665,
#213666,#213667,#213668,#213669,#213670,#213671,#213672,#213673,#213674,
#213675,#213676,#213677,#213678,#213679,#213680,#213681,#213682,#213683,
#213684,#213685,#213686,#213687,#213688,#213689,#213690,#213691,#213692,
#213693,#213694,#213695,#213696,#213697,#213698,#213699,#213700,#213701,
#213702,#213703,#213704,#213705,#213706,#213707,#213708,#213709,#213710,
#213711,#213712,#213713,#213714,#213715,#213716,#213717,#213718,#213719,
#213720,#213721,#213722,#213723,#213724,#213725,#213726,#213727,#213728,
#213729,#213730,#213731,#213732,#213733,#213734,#213735,#213736,#213737,
#213738,#213739,#213740,#213741,#213742,#213743,#213744,#213745,#213746,
#213747,#213748,#213749,#213750,#213751,#213752,#213753,#213754,#213755,
#213756,#213757,#213758,#213759,#213760,#213761,#213762,#213763,#213764,
#213765,#213766,#213767,#213768,#213769,#213770,#213771,#213772,#213773,
#213774,#213775,#213776),(#213777,#213778,#213779,#213780,#213781,#213782,
#213783,#213784,#213785,#213786,#213787,#213788,#213789,#213790,#213791,
#213792,#213793,#213794,#213795,#213796,#213797,#213798,#213799,#213800,
#213801,#213802,#213803,#213804,#213805,#213806,#213807,#213808,#213809,
#213810,#213811,#213812,#213813,#213814,#213815,#213816,#213817,#213818,
#213819,#213820,#213821,#213822,#213823,#213824,#213825,#213826,#213827,
#213828,#213829,#213830,#213831,#213832,#213833,#213834,#213835,#213836,
#213837,#213838,#213839,#213840,#213841,#213842,#213843,#213844,#213845,
#213846,#213847,#213848,#213849,#213850,#213851,#213852,#213853,#213854,
#213855,#213856,#213857,#213858,#213859,#213860,#213861,#213862,#213863,
#213864,#213865,#213866,#213867,#213868,#213869,#213870,#213871,#213872,
#213873,#213874,#213875,#213876,#213877,#213878,#213879,#213880,#213881,
#213882,#213883,#213884,#213885,#213886,#213887,#213888,#213889,#213890,
#213891,#213892,#213893,#213894,#213895,#213896,#213897,#213898,#213899,
#213900,#213901,#213902,#213903,#213904,#213905,#213906,#213907,#213908,
#213909,#213910,#213911,#213912,#213913,#213914,#213915,#213916,#213917,
#213918,#213919,#213920,#213921,#213922,#213923,#213924,#213925,#213926,
#213927,#213928,#213929,#213930,#213931,#213932,#213933,#213934,#213935,
#213936,#213937,#213938,#213939,#213940,#213941,#213942,#213943,#213944,
#213945,#213946,#213947,#213948,#213949,#213950,#213951,#213952,#213953,
#213954),(#213955,#213956,#213957,#213958,#213959,#213960,#213961,#213962,
#213963,#213964,#213965,#213966,#213967,#213968,#213969,#213970,#213971,
#213972,#213973,#213974,#213975,#213976,#213977,#213978,#213979,#213980,
#213981,#213982,#213983,#213984,#213985,#213986,#213987,#213988,#213989,
#213990,#213991,#213992,#213993,#213994,#213995,#213996,#213997,#213998,
#213999,#214000,#214001,#214002,#214003,#214004,#214005,#214006,#214007,
#214008,#214009,#214010,#214011,#214012,#214013,#214014,#214015,#214016,
#214017,#214018,#214019,#214020,#214021,#214022,#214023,#214024,#214025,
#214026,#214027,#214028,#214029,#214030,#214031,#214032,#214033,#214034,
#214035,#214036,#214037,#214038,#214039,#214040,#214041,#214042,#214043,
#214044,#214045,#214046,#214047,#214048,#214049,#214050,#214051,#214052,
#214053,#214054,#214055,#214056,#214057,#214058,#214059,#214060,#214061,
#214062,#214063,#214064,#214065,#214066,#214067,#214068,#214069,#214070,
#214071,#214072,#214073,#214074,#214075,#214076,#214077,#214078,#214079,
#214080,#214081,#214082,#214083,#214084,#214085,#214086,#214087,#214088,
#214089,#214090,#214091,#214092,#214093,#214094,#214095,#214096,#214097,
#214098,#214099,#214100,#214101,#214102,#214103,#214104,#214105,#214106,
#214107,#214108,#214109,#214110,#214111,#214112,#214113,#214114,#214115,
#214116,#214117,#214118,#214119,#214120,#214121,#214122,#214123,#214124,
#214125,#214126,#214127,#214128,#214129,#214130,#214131,#214132),(#214133,
#214134,#214135,#214136,#214137,#214138,#214139,#214140,#214141,#214142,
#214143,#214144,#214145,#214146,#214147,#214148,#214149,#214150,#214151,
#214152,#214153,#214154,#214155,#214156,#214157,#214158,#214159,#214160,
#214161,#214162,#214163,#214164,#214165,#214166,#214167,#214168,#214169,
#214170,#214171,#214172,#214173,#214174,#214175,#214176,#214177,#214178,
#214179,#214180,#214181,#214182,#214183,#214184,#214185,#214186,#214187,
#214188,#214189,#214190,#214191,#214192,#214193,#214194,#214195,#214196,
#214197,#214198,#214199,#214200,#214201,#214202,#214203,#214204,#214205,
#214206,#214207,#214208,#214209,#214210,#214211,#214212,#214213,#214214,
#214215,#214216,#214217,#214218,#214219,#214220,#214221,#214222,#214223,
#214224,#214225,#214226,#214227,#214228,#214229,#214230,#214231,#214232,
#214233,#214234,#214235,#214236,#214237,#214238,#214239,#214240,#214241,
#214242,#214243,#214244,#214245,#214246,#214247,#214248,#214249,#214250,
#214251,#214252,#214253,#214254,#214255,#214256,#214257,#214258,#214259,
#214260,#214261,#214262,#214263,#214264,#214265,#214266,#214267,#214268,
#214269,#214270,#214271,#214272,#214273,#214274,#214275,#214276,#214277,
#214278,#214279,#214280,#214281,#214282,#214283,#214284,#214285,#214286,
#214287,#214288,#214289,#214290,#214291,#214292,#214293,#214294,#214295,
#214296,#214297,#214298,#214299,#214300,#214301,#214302,#214303,#214304,
#214305,#214306,#214307,#214308,#214309,#214310)),.UNSPECIFIED.,.F.,.F.,
 .F.,(4,4),(4,1,1,1,1,1,1,1,1,1,1,1,1,1,1,1,1,1,1,1,1,1,1,1,1,1,1,1,1,1,
1,1,1,1,1,1,1,1,1,1,1,1,1,1,1,1,1,1,1,1,1,1,1,1,1,1,1,1,1,1,1,1,1,1,1,1,
1,1,1,1,1,1,1,1,1,1,1,1,1,1,1,1,1,1,1,1,1,1,1,1,1,1,1,1,1,1,1,1,1,1,1,1,
1,1,1,1,1,1,1,1,1,1,1,1,1,1,1,1,1,1,1,1,1,1,1,1,1,1,1,1,1,1,1,1,1,1,1,1,
1,1,1,1,1,1,1,1,1,1,1,1,1,1,1,1,1,1,1,1,1,1,1,1,1,1,1,1,1,1,1,1,1,1,1,1,
1,4),(-0.000439583499978536,0.0515314520155978),(11.8664846510264,12.8657606844883,
13.8645971344502,14.8634335844121,15.8622700343739,16.8611064843358,17.8599429342977,
18.8587793842596,19.8576158342214,20.8564522841833,21.8552887341452,22.854125184107,
23.8529616340689,24.8517980840308,25.8506345339927,26.8494709839545,27.8483074339164,
28.8471438838783,29.8459803338402,30.844816783802,31.8436532337639,32.8424896837258,
33.8413261336877,34.8401625836495,35.8389990336114,36.8378354835733,37.8366719335352,
38.835508383497,39.8343448334589,40.8331812834208,41.8320177333827,42.8308541833445,
43.8296906333064,44.8285270832683,45.8273635332302,46.826199983192,47.8250364331539,
48.8238728831158,49.8227093330777,50.8215457830395,51.8203822330014,52.8192186829633,
53.8180551329252,54.816891582887,55.8157280328489,56.8145644828108,57.8134009327727,
58.8122373827345,59.8110738326964,60.8099102826583,61.8087467326202,62.807583182582,
63.8064196325439,64.8052560825058,65.8040925324676,66.8029289824295,67.8017654323914,
68.8006018823533,69.7994383323151,70.798274782277,71.7971112322389,72.7959476822008,
73.7947841321626,74.7936205821245,75.7924570320864,76.7912934820483,77.7901299320101,
78.788966381972,79.7878028319339,80.7866392818958,81.7854757318576,82.7843121818195,
83.7831486317814,84.7819850817433,85.7808215317051,86.779657981667,87.7784944316289,
88.7773308815908,89.7761673315526,90.7750037815145,91.7738402314764,92.7726766814383,
93.7715131314001,94.770349581362,95.7691860313239,96.7680224812858,97.7668589312476,
98.7656953812095,99.7645318311714,100.763368281133,101.762204731095,102.761041181057,
103.759877631019,104.758714080981,105.757550530943,106.756386980905,107.755223430866,
108.754059880828,109.75289633079,110.751732780752,111.750569230714,112.749405680676,
113.748242130638,114.747078580599,115.745915030561,116.744751480523,117.743587930485,
118.742424380447,119.741260830409,120.740097280371,121.738933730333,122.737770180294,
123.736606630256,124.735443080218,125.73427953018,126.733115980142,127.731952430104,
128.730788880066,129.729625330028,130.728461779989,131.727298229951,132.726134679913,
133.724971129875,134.723807579837,135.722644029799,136.721480479761,137.720316929723,
138.719153379684,139.717989829646,140.716826279608,141.71566272957,142.714499179532,
143.713335629494,144.712172079456,145.711008529418,146.709844979379,147.708681429341,
148.707517879303,149.706354329265,150.705190779227,151.704027229189,152.702863679151,
153.701700129113,154.700536579074,155.699373029036,156.698209478998,157.69704592896,
158.695882378922,159.694718828884,160.693555278846,161.692391728808,162.691228178769,
163.690064628731,164.688901078693,165.687737528655,166.686573978617,167.685410428579,
168.684246878541,169.683083328503,170.681919778464,171.680756228426,172.679592678388,
173.67842912835,174.677265578312,175.676102028274,176.674938478236,177.673774928198,
178.672611378159,179.671447828121,180.670284278083,181.669120728045,182.667957178007,
183.666793627969,184.665630077931,185.664466527893,186.663302977854),
 .UNSPECIFIED.);
#172=B_SPLINE_SURFACE_WITH_KNOTS('',3,3,((#214396,#214397,#214398,#214399,
#214400,#214401,#214402,#214403,#214404,#214405,#214406,#214407,#214408,
#214409,#214410,#214411,#214412,#214413,#214414,#214415,#214416,#214417,
#214418,#214419,#214420,#214421,#214422,#214423,#214424,#214425,#214426,
#214427,#214428,#214429,#214430,#214431,#214432,#214433,#214434,#214435,
#214436,#214437,#214438,#214439,#214440,#214441,#214442,#214443,#214444,
#214445,#214446,#214447,#214448,#214449,#214450,#214451,#214452,#214453,
#214454,#214455,#214456,#214457,#214458,#214459,#214460,#214461,#214462,
#214463,#214464,#214465,#214466,#214467,#214468,#214469,#214470,#214471,
#214472,#214473,#214474,#214475,#214476,#214477,#214478,#214479,#214480,
#214481,#214482,#214483,#214484,#214485,#214486,#214487,#214488,#214489,
#214490,#214491,#214492,#214493,#214494,#214495,#214496,#214497,#214498,
#214499,#214500,#214501,#214502,#214503,#214504,#214505,#214506,#214507,
#214508,#214509,#214510,#214511,#214512,#214513,#214514,#214515,#214516,
#214517,#214518,#214519,#214520,#214521,#214522,#214523,#214524,#214525,
#214526,#214527,#214528,#214529,#214530,#214531,#214532,#214533,#214534,
#214535,#214536,#214537,#214538,#214539,#214540,#214541,#214542,#214543,
#214544,#214545,#214546,#214547,#214548,#214549,#214550,#214551,#214552,
#214553,#214554,#214555,#214556,#214557,#214558,#214559,#214560,#214561,
#214562,#214563,#214564,#214565,#214566,#214567,#214568,#214569,#214570,
#214571,#214572,#214573),(#214574,#214575,#214576,#214577,#214578,#214579,
#214580,#214581,#214582,#214583,#214584,#214585,#214586,#214587,#214588,
#214589,#214590,#214591,#214592,#214593,#214594,#214595,#214596,#214597,
#214598,#214599,#214600,#214601,#214602,#214603,#214604,#214605,#214606,
#214607,#214608,#214609,#214610,#214611,#214612,#214613,#214614,#214615,
#214616,#214617,#214618,#214619,#214620,#214621,#214622,#214623,#214624,
#214625,#214626,#214627,#214628,#214629,#214630,#214631,#214632,#214633,
#214634,#214635,#214636,#214637,#214638,#214639,#214640,#214641,#214642,
#214643,#214644,#214645,#214646,#214647,#214648,#214649,#214650,#214651,
#214652,#214653,#214654,#214655,#214656,#214657,#214658,#214659,#214660,
#214661,#214662,#214663,#214664,#214665,#214666,#214667,#214668,#214669,
#214670,#214671,#214672,#214673,#214674,#214675,#214676,#214677,#214678,
#214679,#214680,#214681,#214682,#214683,#214684,#214685,#214686,#214687,
#214688,#214689,#214690,#214691,#214692,#214693,#214694,#214695,#214696,
#214697,#214698,#214699,#214700,#214701,#214702,#214703,#214704,#214705,
#214706,#214707,#214708,#214709,#214710,#214711,#214712,#214713,#214714,
#214715,#214716,#214717,#214718,#214719,#214720,#214721,#214722,#214723,
#214724,#214725,#214726,#214727,#214728,#214729,#214730,#214731,#214732,
#214733,#214734,#214735,#214736,#214737,#214738,#214739,#214740,#214741,
#214742,#214743,#214744,#214745,#214746,#214747,#214748,#214749,#214750,
#214751),(#214752,#214753,#214754,#214755,#214756,#214757,#214758,#214759,
#214760,#214761,#214762,#214763,#214764,#214765,#214766,#214767,#214768,
#214769,#214770,#214771,#214772,#214773,#214774,#214775,#214776,#214777,
#214778,#214779,#214780,#214781,#214782,#214783,#214784,#214785,#214786,
#214787,#214788,#214789,#214790,#214791,#214792,#214793,#214794,#214795,
#214796,#214797,#214798,#214799,#214800,#214801,#214802,#214803,#214804,
#214805,#214806,#214807,#214808,#214809,#214810,#214811,#214812,#214813,
#214814,#214815,#214816,#214817,#214818,#214819,#214820,#214821,#214822,
#214823,#214824,#214825,#214826,#214827,#214828,#214829,#214830,#214831,
#214832,#214833,#214834,#214835,#214836,#214837,#214838,#214839,#214840,
#214841,#214842,#214843,#214844,#214845,#214846,#214847,#214848,#214849,
#214850,#214851,#214852,#214853,#214854,#214855,#214856,#214857,#214858,
#214859,#214860,#214861,#214862,#214863,#214864,#214865,#214866,#214867,
#214868,#214869,#214870,#214871,#214872,#214873,#214874,#214875,#214876,
#214877,#214878,#214879,#214880,#214881,#214882,#214883,#214884,#214885,
#214886,#214887,#214888,#214889,#214890,#214891,#214892,#214893,#214894,
#214895,#214896,#214897,#214898,#214899,#214900,#214901,#214902,#214903,
#214904,#214905,#214906,#214907,#214908,#214909,#214910,#214911,#214912,
#214913,#214914,#214915,#214916,#214917,#214918,#214919,#214920,#214921,
#214922,#214923,#214924,#214925,#214926,#214927,#214928,#214929),(#214930,
#214931,#214932,#214933,#214934,#214935,#214936,#214937,#214938,#214939,
#214940,#214941,#214942,#214943,#214944,#214945,#214946,#214947,#214948,
#214949,#214950,#214951,#214952,#214953,#214954,#214955,#214956,#214957,
#214958,#214959,#214960,#214961,#214962,#214963,#214964,#214965,#214966,
#214967,#214968,#214969,#214970,#214971,#214972,#214973,#214974,#214975,
#214976,#214977,#214978,#214979,#214980,#214981,#214982,#214983,#214984,
#214985,#214986,#214987,#214988,#214989,#214990,#214991,#214992,#214993,
#214994,#214995,#214996,#214997,#214998,#214999,#215000,#215001,#215002,
#215003,#215004,#215005,#215006,#215007,#215008,#215009,#215010,#215011,
#215012,#215013,#215014,#215015,#215016,#215017,#215018,#215019,#215020,
#215021,#215022,#215023,#215024,#215025,#215026,#215027,#215028,#215029,
#215030,#215031,#215032,#215033,#215034,#215035,#215036,#215037,#215038,
#215039,#215040,#215041,#215042,#215043,#215044,#215045,#215046,#215047,
#215048,#215049,#215050,#215051,#215052,#215053,#215054,#215055,#215056,
#215057,#215058,#215059,#215060,#215061,#215062,#215063,#215064,#215065,
#215066,#215067,#215068,#215069,#215070,#215071,#215072,#215073,#215074,
#215075,#215076,#215077,#215078,#215079,#215080,#215081,#215082,#215083,
#215084,#215085,#215086,#215087,#215088,#215089,#215090,#215091,#215092,
#215093,#215094,#215095,#215096,#215097,#215098,#215099,#215100,#215101,
#215102,#215103,#215104,#215105,#215106,#215107)),.UNSPECIFIED.,.F.,.F.,
 .F.,(4,4),(4,1,1,1,1,1,1,1,1,1,1,1,1,1,1,1,1,1,1,1,1,1,1,1,1,1,1,1,1,1,
1,1,1,1,1,1,1,1,1,1,1,1,1,1,1,1,1,1,1,1,1,1,1,1,1,1,1,1,1,1,1,1,1,1,1,1,
1,1,1,1,1,1,1,1,1,1,1,1,1,1,1,1,1,1,1,1,1,1,1,1,1,1,1,1,1,1,1,1,1,1,1,1,
1,1,1,1,1,1,1,1,1,1,1,1,1,1,1,1,1,1,1,1,1,1,1,1,1,1,1,1,1,1,1,1,1,1,1,1,
1,1,1,1,1,1,1,1,1,1,1,1,1,1,1,1,1,1,1,1,1,1,1,1,1,1,1,1,1,1,1,1,1,1,1,1,
1,4),(-0.00037822144473665,0.0515928134973294),(14.3986268518925,15.3974633018543,
16.3962997518162,17.3951362017781,18.39397265174,19.3928091017018,20.3916455516637,
21.3904820016256,22.3893184515875,23.3881549015493,24.3869913515112,25.3858278014731,
26.384664251435,27.3835007013968,28.3823371513587,29.3811736013206,30.3800100512825,
31.3788465012443,32.3776829512062,33.3765194011681,34.37535585113,35.3741923010918,
36.3730287510537,37.3718652010156,38.3707016509774,39.3695381009393,40.3683745509012,
41.3672110008631,42.3660474508249,43.3648839007868,44.3637203507487,45.3625568007106,
46.3613932506724,47.3602297006343,48.3590661505962,49.3579026005581,50.3567390505199,
51.3555755004818,52.3544119504437,53.3532484004056,54.3520848503674,55.3509213003293,
56.3497577502912,57.3485942002531,58.3474306502149,59.3462671001768,60.3451035501387,
61.3439400001006,62.3427764500624,63.3416129000243,64.3404493499862,65.3392857999481,
66.3381222499099,67.3369586998718,68.3357951498337,69.3346315997956,70.3334680497574,
71.3323044997193,72.3311409496812,73.3299773996431,74.3288138496049,75.3276502995668,
76.3264867495287,77.3253231994906,78.3241596494524,79.3229960994143,80.3218325493762,
81.3206689993381,82.3195054492999,83.3183418992618,84.3171783492237,85.3160147991856,
86.3148512491474,87.3136876991093,88.3125241490712,89.3113605990331,90.3101970489949,
91.3090334989568,92.3078699489187,93.3067063988806,94.3055428488424,95.3043792988043,
96.3032157487662,97.302052198728,98.3008886486899,99.2997250986518,100.298561548614,
101.297397998576,102.296234448537,103.295070898499,104.293907348461,105.292743798423,
106.291580248385,107.290416698347,108.289253148309,109.288089598271,110.286926048232,
111.285762498194,112.284598948156,113.283435398118,114.28227184808,115.281108298042,
116.279944748004,117.278781197966,118.277617647927,119.276454097889,120.275290547851,
121.274126997813,122.272963447775,123.271799897737,124.270636347699,125.269472797661,
126.268309247622,127.267145697584,128.265982147546,129.264818597508,130.26365504747,
131.262491497432,132.261327947394,133.260164397356,134.259000847317,135.257837297279,
136.256673747241,137.255510197203,138.254346647165,139.253183097127,140.252019547089,
141.250855997051,142.249692447012,143.248528896974,144.247365346936,145.246201796898,
146.24503824686,147.243874696822,148.242711146784,149.241547596746,150.240384046707,
151.239220496669,152.238056946631,153.236893396593,154.235729846555,155.234566296517,
156.233402746479,157.232239196441,158.231075646402,159.229912096364,160.228748546326,
161.227584996288,162.22642144625,163.225257896212,164.224094346174,165.222930796136,
166.221767246097,167.220603696059,168.219440146021,169.218276595983,170.217113045945,
171.215949495907,172.214785945869,173.21362239583,174.212458845792,175.211295295754,
176.210131745716,177.208968195678,178.20780464564,179.206641095602,180.205477545564,
181.204313995525,182.203150445487,183.201986895449,184.200823345411,185.199659795373,
186.198496245335,187.197332695297,188.196169145259,189.195445174867),
 .UNSPECIFIED.);
#173=FACE_BOUND('',#4590,.T.);
#174=FACE_BOUND('',#4591,.T.);
#175=FACE_BOUND('',#4592,.T.);
#176=FACE_BOUND('',#4593,.T.);
#177=FACE_BOUND('',#4594,.T.);
#178=FACE_BOUND('',#4595,.T.);
#179=FACE_BOUND('',#4596,.T.);
#180=FACE_BOUND('',#4597,.T.);
#181=FACE_BOUND('',#4598,.T.);
#182=FACE_BOUND('',#4620,.T.);
#183=FACE_BOUND('',#4627,.T.);
#184=FACE_BOUND('',#4628,.T.);
#185=FACE_BOUND('',#4629,.T.);
#186=FACE_BOUND('',#4639,.T.);
#187=FACE_BOUND('',#4653,.T.);
#188=FACE_BOUND('',#4654,.T.);
#189=FACE_BOUND('',#4655,.T.);
#190=FACE_BOUND('',#4665,.T.);
#191=FACE_BOUND('',#4675,.T.);
#192=FACE_BOUND('',#4679,.T.);
#193=FACE_BOUND('',#4680,.T.);
#194=FACE_BOUND('',#4703,.T.);
#195=FACE_BOUND('',#4704,.T.);
#196=FACE_BOUND('',#4715,.T.);
#197=FACE_BOUND('',#4716,.T.);
#198=FACE_BOUND('',#4717,.T.);
#199=FACE_BOUND('',#4718,.T.);
#200=FACE_BOUND('',#4764,.T.);
#201=FACE_BOUND('',#4819,.T.);
#202=FACE_BOUND('',#4876,.T.);
#203=FACE_BOUND('',#4931,.T.);
#204=FACE_BOUND('',#5046,.T.);
#205=FACE_BOUND('',#5047,.T.);
#206=FACE_BOUND('',#5048,.T.);
#207=FACE_BOUND('',#5055,.T.);
#208=FACE_BOUND('',#5056,.T.);
#209=FACE_BOUND('',#5057,.T.);
#210=FACE_BOUND('',#5062,.T.);
#211=FACE_BOUND('',#5063,.T.);
#212=FACE_BOUND('',#5064,.T.);
#213=FACE_BOUND('',#5089,.T.);
#214=FACE_BOUND('',#5090,.T.);
#215=FACE_BOUND('',#5091,.T.);
#216=FACE_BOUND('',#5119,.T.);
#217=FACE_BOUND('',#5154,.T.);
#218=FACE_BOUND('',#5274,.T.);
#219=FACE_BOUND('',#5276,.T.);
#220=FACE_BOUND('',#5535,.T.);
#221=FACE_BOUND('',#5536,.T.);
#222=FACE_BOUND('',#5537,.T.);
#223=FACE_BOUND('',#5538,.T.);
#224=FACE_BOUND('',#5539,.T.);
#225=FACE_BOUND('',#5540,.T.);
#226=FACE_BOUND('',#5541,.T.);
#227=FACE_BOUND('',#5542,.T.);
#228=FACE_BOUND('',#5543,.T.);
#229=FACE_BOUND('',#5565,.T.);
#230=FACE_BOUND('',#5572,.T.);
#231=FACE_BOUND('',#5573,.T.);
#232=FACE_BOUND('',#5574,.T.);
#233=FACE_BOUND('',#5584,.T.);
#234=FACE_BOUND('',#5598,.T.);
#235=FACE_BOUND('',#5599,.T.);
#236=FACE_BOUND('',#5600,.T.);
#237=FACE_BOUND('',#5610,.T.);
#238=FACE_BOUND('',#5620,.T.);
#239=FACE_BOUND('',#5624,.T.);
#240=FACE_BOUND('',#5625,.T.);
#241=FACE_BOUND('',#5648,.T.);
#242=FACE_BOUND('',#5649,.T.);
#243=FACE_BOUND('',#5660,.T.);
#244=FACE_BOUND('',#5661,.T.);
#245=FACE_BOUND('',#5662,.T.);
#246=FACE_BOUND('',#5663,.T.);
#247=B_SPLINE_CURVE_WITH_KNOTS('',3,(#36300,#36301,#36302,#36303,#36304,
#36305),.UNSPECIFIED.,.F.,.F.,(4,1,1,4),(36.782513561854,37.1950127479992,
37.6823602457602,38.1697077435212),.UNSPECIFIED.);
#248=B_SPLINE_CURVE_WITH_KNOTS('',3,(#36308,#36309,#36310,#36311,#36312,
#36313,#36314,#36315,#36316,#36317,#36318,#36319,#36320,#36321,#36322,#36323,
#36324,#36325,#36326,#36327,#36328,#36329,#36330,#36331,#36332,#36333,#36334,
#36335,#36336,#36337,#36338,#36339,#36340,#36341,#36342,#36343,#36344,#36345,
#36346,#36347,#36348,#36349,#36350,#36351,#36352,#36353,#36354,#36355,#36356,
#36357,#36358,#36359,#36360,#36361,#36362,#36363,#36364,#36365,#36366,#36367,
#36368,#36369,#36370,#36371,#36372,#36373,#36374,#36375,#36376,#36377,#36378,
#36379,#36380),.UNSPECIFIED.,.F.,.F.,(4,3,3,3,3,3,3,3,3,3,3,3,3,3,3,3,3,
3,3,3,3,3,3,3,4),(36.7824851161968,36.8175942235541,36.9047259080441,36.9918410494598,
37.0789592472834,37.166072719263,37.2532055288754,37.3049417213151,37.3920685377782,
37.4791788064371,37.5662921716237,37.6534008452347,37.7405289511405,37.7922892190762,
37.8794201571563,37.966534535352,38.0536519523545,38.1407646354665,38.2278966508317,
38.2796367168372,38.3664398614179,38.4532350920939,38.5400193187296,38.6268191082651,
38.6945925143091),.UNSPECIFIED.);
#249=B_SPLINE_CURVE_WITH_KNOTS('',3,(#36386,#36387,#36388,#36389,#36390,
#36391,#36392,#36393,#36394,#36395,#36396,#36397,#36398,#36399,#36400,#36401,
#36402,#36403,#36404,#36405,#36406,#36407,#36408,#36409,#36410,#36411,#36412,
#36413,#36414,#36415,#36416,#36417,#36418,#36419,#36420,#36421,#36422,#36423,
#36424,#36425,#36426,#36427,#36428,#36429,#36430,#36431,#36432,#36433,#36434,
#36435,#36436,#36437,#36438,#36439,#36440,#36441,#36442,#36443,#36444,#36445,
#36446,#36447,#36448,#36449,#36450,#36451,#36452,#36453,#36454,#36455,#36456,
#36457,#36458,#36459,#36460,#36461,#36462,#36463,#36464,#36465,#36466,#36467,
#36468,#36469,#36470,#36471,#36472,#36473,#36474,#36475,#36476,#36477,#36478,
#36479,#36480,#36481,#36482,#36483,#36484,#36485,#36486,#36487,#36488,#36489,
#36490,#36491,#36492,#36493,#36494,#36495,#36496,#36497,#36498,#36499,#36500,
#36501,#36502,#36503,#36504,#36505,#36506,#36507,#36508,#36509,#36510,#36511,
#36512,#36513,#36514,#36515,#36516,#36517,#36518,#36519,#36520,#36521,#36522,
#36523,#36524,#36525,#36526,#36527,#36528,#36529,#36530,#36531,#36532,#36533,
#36534,#36535,#36536),.UNSPECIFIED.,.F.,.F.,(4,3,3,3,3,3,3,3,3,3,3,3,3,
3,3,3,3,3,3,3,3,3,3,3,3,3,3,3,3,3,3,3,3,3,3,3,3,3,3,3,3,3,3,3,3,3,3,3,3,
3,4),(30.4993214241099,30.589364887359,30.6765073736468,30.7680013253765,
30.8594952771061,30.9466072614862,31.0337024468151,31.1208004982627,31.2078937641911,
31.2950064517671,31.3468427748671,31.4339808001712,31.5211023922076,31.6082271424273,
31.6953472086888,31.7824866195326,31.8341902726282,31.9213169014601,32.0084269463445,
32.0955400358983,32.1826484052062,32.2697761653463,32.3215377703892,32.4086680911823,
32.4957818717525,32.5828987261604,32.6700108677988,32.7571423788036,32.8088852681502,
32.8960149192679,32.9831280267967,33.0702442097147,33.1573556823675,33.2444865341393,
33.2962327659112,33.3833626291845,33.4704759436101,33.5575923235023,33.6447039870287,
33.7318350185696,33.7835802636722,33.8707089656242,33.9578211205362,34.0449363548941,
34.1320468835505,34.2191768065887,34.2709277614332,34.3584567439305,34.4459664831206,
34.5334668399684,34.5575191894877),.UNSPECIFIED.);
#250=B_SPLINE_CURVE_WITH_KNOTS('',3,(#36537,#36538,#36539,#36540,#36541,
#36542,#36543,#36544,#36545),.UNSPECIFIED.,.F.,.F.,(4,1,1,1,1,1,4),(34.5575192147699,
34.7582752591942,35.2456227569552,35.7329702547162,36.2203177524772,36.7076652502382,
36.782513561854),.UNSPECIFIED.);
#251=B_SPLINE_CURVE_WITH_KNOTS('',3,(#36547,#36548,#36549,#36550,#36551,
#36552,#36553,#36554,#36555,#36556,#36557,#36558,#36559,#36560,#36561,#36562,
#36563,#36564,#36565,#36566,#36567,#36568,#36569,#36570,#36571,#36572,#36573,
#36574,#36575,#36576,#36577,#36578,#36579,#36580,#36581,#36582,#36583,#36584,
#36585,#36586,#36587,#36588,#36589,#36590,#36591,#36592,#36593,#36594,#36595,
#36596,#36597,#36598,#36599,#36600,#36601,#36602,#36603,#36604,#36605,#36606,
#36607,#36608,#36609,#36610,#36611,#36612,#36613,#36614,#36615,#36616,#36617,
#36618,#36619,#36620,#36621,#36622,#36623,#36624,#36625,#36626,#36627,#36628,
#36629,#36630,#36631),.UNSPECIFIED.,.F.,.F.,(4,3,3,3,3,3,3,3,3,3,3,3,3,
3,3,3,3,3,3,3,3,3,3,3,3,3,3,3,4),(34.5575191894877,34.6447569757657,34.7319918970944,
34.8192474416769,34.8682042325101,34.9553345524685,35.0424483321962,35.1295651857588,
35.2166773265522,35.3038088367198,35.3555517302711,35.4426813814716,35.5297944890805,
35.6169106720737,35.7040221447989,35.7911529966377,35.8428992280321,35.9300290910938,
36.0171424053112,36.1042587850018,36.191370448331,36.278501479683,36.3302467257931,
36.4173750047355,36.5086525326009,36.5957638112878,36.6828711022947,36.7699915625257,
36.7824851161968),.UNSPECIFIED.);
#252=B_SPLINE_CURVE_WITH_KNOTS('',3,(#36632,#36633,#36634,#36635,#36636,
#36637,#36638,#36639,#36640,#36641,#36642,#36643),.UNSPECIFIED.,.F.,.F.,
(4,1,1,1,1,1,1,1,1,4),(30.4992328073076,30.9694242504221,31.4567717481831,
31.9441192459441,32.4314667437051,32.9188142414661,33.4061617392271,33.8935092369881,
34.3808567347491,34.5575191593289),.UNSPECIFIED.);
#253=B_SPLINE_CURVE_WITH_KNOTS('',3,(#36649,#36650,#36651,#36652,#36653,
#36654,#36655,#36656,#36657,#36658,#36659,#36660,#36661,#36662,#36663,#36664,
#36665,#36666,#36667,#36668,#36669,#36670,#36671,#36672,#36673,#36674,#36675,
#36676,#36677,#36678,#36679,#36680,#36681,#36682,#36683,#36684,#36685,#36686,
#36687,#36688,#36689,#36690,#36691,#36692,#36693,#36694,#36695,#36696,#36697,
#36698,#36699,#36700,#36701,#36702,#36703,#36704,#36705,#36706,#36707,#36708,
#36709,#36710,#36711,#36712,#36713,#36714,#36715,#36716,#36717,#36718,#36719,
#36720,#36721,#36722,#36723,#36724,#36725,#36726,#36727,#36728,#36729,#36730,
#36731,#36732,#36733,#36734,#36735,#36736,#36737,#36738,#36739,#36740,#36741,
#36742,#36743,#36744,#36745,#36746,#36747,#36748,#36749,#36750,#36751,#36752,
#36753,#36754,#36755,#36756,#36757,#36758,#36759,#36760,#36761,#36762,#36763,
#36764,#36765,#36766,#36767,#36768,#36769,#36770,#36771,#36772,#36773,#36774,
#36775,#36776,#36777,#36778,#36779,#36780,#36781,#36782,#36783,#36784,#36785,
#36786,#36787,#36788,#36789,#36790,#36791,#36792,#36793,#36794,#36795,#36796,
#36797,#36798,#36799),.UNSPECIFIED.,.F.,.F.,(4,3,3,3,3,3,3,3,3,3,3,3,3,
3,3,3,3,3,3,3,3,3,3,3,3,3,3,3,3,3,3,3,3,3,3,3,3,3,3,3,3,3,3,3,3,3,3,3,3,
3,4),(24.2156474862923,24.3000483267107,24.3845029110786,24.4690844734779,
24.5239778062131,24.6055741796599,24.6870642443222,24.7684687650885,24.8498084045712,
24.9311114331561,25.0123964584347,25.0936820583996,25.174986810145,25.2563827962254,
25.337824621091,25.4194048181542,25.4986728017351,25.5832623133344,25.6677481822996,
25.7521477829318,25.836478417448,25.9207557824206,26.0050040171561,26.0892387031326,
26.1734754092372,26.2577612684093,26.3420733549027,26.426466141403,26.4733677972571,
26.558092298325,26.6427552017968,26.7273710330641,26.8119574560143,26.8965425130992,
26.9607152950181,27.0519442316041,27.1432666559618,27.2346896336238,27.3261417991208,
27.4176104484587,27.4480627927791,27.532586803755,27.6170657800487,27.7015239814603,
27.7859674988434,27.8704340010683,27.9354102905401,28.0240768753705,28.1127462609405,
28.2014356078663,28.2743338823081),.UNSPECIFIED.);
#254=B_SPLINE_CURVE_WITH_KNOTS('',3,(#36800,#36801,#36802,#36803,#36804,
#36805,#36806,#36807,#36808,#36809,#36810,#36811,#36812,#36813,#36814,#36815,
#36816,#36817,#36818,#36819,#36820,#36821,#36822,#36823,#36824,#36825,#36826,
#36827,#36828,#36829,#36830,#36831,#36832,#36833,#36834,#36835,#36836,#36837,
#36838,#36839,#36840,#36841,#36842,#36843,#36844,#36845,#36846,#36847,#36848,
#36849,#36850,#36851,#36852,#36853,#36854,#36855,#36856,#36857,#36858,#36859,
#36860,#36861,#36862,#36863,#36864,#36865,#36866,#36867,#36868,#36869,#36870,
#36871,#36872,#36873,#36874,#36875,#36876,#36877,#36878,#36879,#36880,#36881,
#36882,#36883,#36884),.UNSPECIFIED.,.F.,.F.,(4,3,3,3,3,3,3,3,3,3,3,3,3,
3,3,3,3,3,3,3,3,3,3,3,3,3,3,3,4),(28.2743338824266,28.3664532240664,28.4227577883011,
28.5092520935557,28.5957221727376,28.6821896165034,28.7686504765288,28.8551332349923,
28.9101052860621,28.9974342563849,29.084749014768,29.1720683332772,29.2593832734799,
29.3467162971122,29.3974527838231,29.4845626300906,29.5716559384561,29.6587525257064,
29.7458445655353,29.8329564077084,29.8848002815841,29.9719013840595,30.0589854167832,
30.1460720162916,30.2331536875928,30.3202546601054,30.3721477793451,30.459306450247,
30.4993214241099),.UNSPECIFIED.);
#255=B_SPLINE_CURVE_WITH_KNOTS('',3,(#36886,#36887,#36888,#36889,#36890,
#36891,#36892,#36893),.UNSPECIFIED.,.F.,.F.,(4,1,1,1,1,4),(28.2743353147298,
29.0200342593781,29.5073817571391,29.9947292549001,30.4820767526611,30.4992328073076),
 .UNSPECIFIED.);
#256=B_SPLINE_CURVE_WITH_KNOTS('',3,(#36894,#36895,#36896,#36897,#36898,
#36899,#36900,#36901,#36902,#36903,#36904,#36905,#36906,#36907,#36908,#36909,
#36910,#36911,#36912,#36913,#36914,#36915,#36916,#36917,#36918,#36919,#36920,
#36921,#36922,#36923,#36924,#36925,#36926,#36927,#36928,#36929,#36930,#36931,
#36932,#36933,#36934,#36935,#36936,#36937,#36938,#36939,#36940,#36941,#36942,
#36943,#36944,#36945,#36946,#36947,#36948,#36949,#36950,#36951,#36952,#36953,
#36954,#36955,#36956,#36957,#36958,#36959,#36960,#36961,#36962,#36963,#36964,
#36965,#36966,#36967,#36968,#36969,#36970,#36971,#36972,#36973,#36974,#36975,
#36976,#36977,#36978,#36979,#36980,#36981,#36982,#36983,#36984,#36985,#36986,
#36987,#36988,#36989,#36990,#36991,#36992,#36993,#36994,#36995,#36996,#36997,
#36998,#36999,#37000,#37001,#37002,#37003,#37004,#37005,#37006,#37007,#37008,
#37009,#37010,#37011,#37012,#37013,#37014,#37015,#37016,#37017,#37018,#37019,
#37020,#37021,#37022,#37023,#37024,#37025,#37026,#37027,#37028,#37029,#37030,
#37031,#37032,#37033,#37034,#37035,#37036,#37037,#37038,#37039,#37040,#37041),
 .UNSPECIFIED.,.F.,.F.,(4,3,3,3,3,3,3,3,3,3,3,3,3,3,3,3,3,3,3,3,3,3,3,3,
3,3,3,3,3,3,3,3,3,3,3,3,3,3,3,3,3,3,3,3,3,3,3,3,3,4),(24.2161265625725,
24.304879340127,24.3936266169366,24.4823579099005,24.57107729379,24.6339067795291,
24.7183716294415,24.8028157469338,24.887276430042,24.9717432184832,25.0562660667606,
25.1212542772901,25.2127216661248,25.304178010292,25.3955797066455,25.4869204524289,
25.5781480948867,25.6086017750511,25.6931817036893,25.7777588769285,25.8623793056185,
25.9470206674601,26.0317405844674,26.0959492728121,26.1803442406883,26.2646718670788,
26.3489493912654,26.4331940089271,26.5174394793457,26.6016893548484,26.6859592070288,
26.7702646181268,26.8546699103581,26.9391302810329,27.0237153293478,27.0706442683341,
27.1522405465237,27.2337305154638,27.3151349401118,27.3964744831466,27.4777774150383,
27.5590623434471,27.6403478464199,27.7216525011054,27.8030483905001,27.8844901186951,
27.9660702200751,28.0453392638561,28.1696765530861,28.2743338823081),
 .UNSPECIFIED.);
#257=B_SPLINE_CURVE_WITH_KNOTS('',3,(#37047,#37048,#37049,#37050,#37051,
#37052,#37053,#37054,#37055,#37056,#37057,#37058,#37059,#37060,#37061,#37062,
#37063,#37064,#37065,#37066,#37067,#37068,#37069,#37070,#37071,#37072,#37073,
#37074,#37075,#37076,#37077,#37078,#37079,#37080,#37081,#37082,#37083,#37084,
#37085,#37086,#37087,#37088,#37089,#37090,#37091,#37092,#37093,#37094,#37095,
#37096,#37097,#37098,#37099,#37100,#37101,#37102,#37103,#37104,#37105,#37106,
#37107,#37108,#37109,#37110,#37111,#37112,#37113,#37114,#37115,#37116,#37117,
#37118,#37119,#37120,#37121,#37122,#37123,#37124,#37125,#37126,#37127,#37128,
#37129,#37130,#37131),.UNSPECIFIED.,.F.,.F.,(4,3,3,3,3,3,3,3,3,3,3,3,3,
3,3,3,3,3,3,3,3,3,3,3,3,3,3,3,4),(15.7079632709821,15.7983391757108,15.861651819831,
15.9487473765214,16.0358259589805,16.1229073061607,16.2099838502341,16.2970799349332,
16.348999317592,16.4361366999986,16.523257608915,16.6103816220701,16.6975009223997,
16.7846395292193,16.836346815353,16.923477639889,17.010591951935,17.0977093744499,
17.1848221036438,17.2719542272672,17.323694313114,17.4108212348644,17.4979315648647,
17.5850449249431,17.6721535558284,17.7592815613529,17.811041810875,17.8981734346075,
17.932952833811),.UNSPECIFIED.);
#258=B_SPLINE_CURVE_WITH_KNOTS('',3,(#37133,#37134,#37135,#37136,#37137,
#37138),.UNSPECIFIED.,.F.,.F.,(4,1,1,4),(14.399609326548,14.886956824309,
15.37430432207,15.707963267949),.UNSPECIFIED.);
#259=B_SPLINE_CURVE_WITH_KNOTS('',3,(#37142,#37143,#37144,#37145,#37146,
#37147,#37148,#37149,#37150,#37151,#37152,#37153,#37154,#37155,#37156,#37157,
#37158,#37159,#37160,#37161,#37162,#37163,#37164,#37165,#37166,#37167,#37168,
#37169,#37170,#37171,#37172,#37173,#37174,#37175,#37176,#37177,#37178,#37179,
#37180,#37181,#37182,#37183,#37184,#37185,#37186,#37187,#37188,#37189,#37190,
#37191,#37192,#37193,#37194,#37195,#37196,#37197,#37198,#37199,#37200,#37201,
#37202,#37203,#37204,#37205,#37206,#37207,#37208),.UNSPECIFIED.,.F.,.F.,
(4,3,3,3,3,3,3,3,3,3,3,3,3,3,3,3,3,3,3,3,3,3,4),(13.8747245557601,13.9615196181783,
14.0483128516542,14.1350984649827,14.2219050359775,14.2896803532321,14.3768111748519,
14.4639254839518,14.5510429035049,14.638155629735,14.7252877504178,14.7770278509931,
14.864154772311,14.9512651018674,15.0383784614888,15.1254870919108,15.2126150969663,
15.2643753487541,15.3512430161605,15.4404230791076,15.5272738475405,15.6176185577448,
15.707963267949),.UNSPECIFIED.);
#260=B_SPLINE_CURVE_WITH_KNOTS('',3,(#37209,#37210,#37211,#37212,#37213,
#37214,#37215,#37216,#37217),.UNSPECIFIED.,.F.,.F.,(4,1,1,1,1,1,4),(15.707963267949,
15.7517228465151,16.2390703442761,16.7264178420371,17.2137653397981,17.7011128375591,
17.9329414836179),.UNSPECIFIED.);
#261=B_SPLINE_CURVE_WITH_KNOTS('',3,(#37223,#37224,#37225,#37226,#37227,
#37228),.UNSPECIFIED.,.F.,.F.,(4,1,1,4),(36.7825135685384,37.1950127479992,
37.6823602457602,38.1697077435212),.UNSPECIFIED.);
#262=B_SPLINE_CURVE_WITH_KNOTS('',3,(#37231,#37232,#37233,#37234,#37235,
#37236,#37237,#37238,#37239,#37240,#37241,#37242,#37243,#37244,#37245,#37246,
#37247,#37248,#37249,#37250,#37251,#37252,#37253,#37254,#37255,#37256,#37257,
#37258,#37259,#37260,#37261,#37262,#37263,#37264,#37265,#37266,#37267,#37268,
#37269,#37270,#37271,#37272,#37273,#37274,#37275,#37276,#37277,#37278,#37279,
#37280,#37281,#37282,#37283,#37284,#37285,#37286,#37287,#37288,#37289,#37290,
#37291,#37292,#37293,#37294,#37295,#37296,#37297,#37298,#37299,#37300,#37301,
#37302,#37303),.UNSPECIFIED.,.F.,.F.,(4,3,3,3,3,3,3,3,3,3,3,3,3,3,3,3,3,
3,3,3,3,3,3,3,4),(36.7824851168753,36.8175942235541,36.9047259024205,36.9918410382111,
37.0789592304617,37.1660726969111,37.2532055011074,37.3049417213151,37.3920685401476,
37.4791788111556,37.5662921786384,37.6534008545103,37.7405289626034,37.7922892190761,
37.8794201719593,37.966534565058,38.0536519969681,38.1407646949544,38.2278967250119,
38.2796367168371,38.3664398085489,38.4532349861649,38.5400191597449,38.6268188966943,
38.6945925143091),.UNSPECIFIED.);
#263=B_SPLINE_CURVE_WITH_KNOTS('',3,(#37309,#37310,#37311,#37312,#37313,
#37314,#37315,#37316,#37317,#37318,#37319,#37320,#37321,#37322,#37323,#37324,
#37325,#37326,#37327,#37328,#37329,#37330,#37331,#37332,#37333,#37334,#37335,
#37336,#37337,#37338,#37339,#37340,#37341,#37342,#37343,#37344,#37345,#37346,
#37347,#37348,#37349,#37350,#37351,#37352,#37353,#37354,#37355,#37356,#37357,
#37358,#37359,#37360,#37361,#37362,#37363,#37364,#37365,#37366,#37367,#37368,
#37369,#37370,#37371,#37372,#37373,#37374,#37375,#37376,#37377,#37378,#37379,
#37380,#37381,#37382,#37383,#37384,#37385,#37386,#37387,#37388,#37389,#37390,
#37391,#37392,#37393,#37394,#37395,#37396,#37397,#37398,#37399,#37400,#37401,
#37402,#37403,#37404,#37405,#37406,#37407,#37408,#37409,#37410,#37411,#37412,
#37413,#37414,#37415,#37416,#37417,#37418,#37419,#37420,#37421,#37422,#37423,
#37424,#37425,#37426,#37427,#37428,#37429,#37430,#37431,#37432,#37433,#37434,
#37435,#37436,#37437,#37438,#37439,#37440,#37441,#37442,#37443,#37444,#37445,
#37446,#37447,#37448,#37449,#37450,#37451,#37452,#37453,#37454,#37455,#37456,
#37457,#37458,#37459),.UNSPECIFIED.,.F.,.F.,(4,3,3,3,3,3,3,3,3,3,3,3,3,
3,3,3,3,3,3,3,3,3,3,3,3,3,3,3,3,3,3,3,3,3,3,3,3,3,3,3,3,3,3,3,3,3,3,3,3,
3,4),(30.4993214304177,30.5893648920898,30.6765072859223,30.7680012815142,
30.8594952771061,30.9466073231606,31.0337025710101,31.1208006856437,31.2078940149848,
31.2950067657722,31.3468427748671,31.4339807679861,31.5211023274172,31.6082270447182,
31.6953470779628,31.7824864559265,31.8341902726281,31.9213169142658,32.0084269721101,
32.0955400747291,32.1826484571305,32.2697762302935,32.3215377703891,32.4086680878499,
32.4957818650579,32.5828987160914,32.6700108543567,32.75714236202,32.8088852681501,
32.8960149195982,32.9831280274467,33.0702442106651,33.1573556836068,33.2444865356467,
33.2962327659111,33.3833626283388,33.4704759419317,33.5575923210181,33.6447039837563,
33.7318350145424,33.7835802636721,33.8707089685104,33.9578211263054,34.0449363635137,
34.1320468949955,34.2191768207951,34.2709277614331,34.3584567371214,34.4459664694995,
34.5334668195807,34.5575191894877),.UNSPECIFIED.);
#264=B_SPLINE_CURVE_WITH_KNOTS('',3,(#37460,#37461,#37462,#37463,#37464,
#37465,#37466,#37467,#37468),.UNSPECIFIED.,.F.,.F.,(4,1,1,1,1,1,4),(34.5575192147677,
34.7582752591941,35.2456227569552,35.7329702547162,36.2203177524772,36.7076652502382,
36.7825135685384),.UNSPECIFIED.);
#265=B_SPLINE_CURVE_WITH_KNOTS('',3,(#37470,#37471,#37472,#37473,#37474,
#37475,#37476,#37477,#37478,#37479,#37480,#37481,#37482,#37483,#37484,#37485,
#37486,#37487,#37488,#37489,#37490,#37491,#37492,#37493,#37494,#37495,#37496,
#37497,#37498,#37499,#37500,#37501,#37502,#37503,#37504,#37505,#37506,#37507,
#37508,#37509,#37510,#37511,#37512,#37513,#37514,#37515,#37516,#37517,#37518,
#37519,#37520,#37521,#37522,#37523,#37524,#37525,#37526,#37527,#37528,#37529,
#37530,#37531,#37532,#37533,#37534,#37535,#37536,#37537,#37538,#37539,#37540,
#37541,#37542,#37543,#37544,#37545,#37546,#37547,#37548,#37549,#37550,#37551,
#37552,#37553,#37554),.UNSPECIFIED.,.F.,.F.,(4,3,3,3,3,3,3,3,3,3,3,3,3,
3,3,3,3,3,3,3,3,3,3,3,3,3,3,3,4),(34.5575191894877,34.6447569868975,34.7319919193617,
34.8192474749927,34.8682042325101,34.9553345482705,35.0424483237626,35.1295651730742,
35.2166773096183,35.3038088155763,35.3555517302711,35.4426813818879,35.5297944898996,
35.6169106732714,35.7040221463605,35.7911529985374,35.8428992280321,35.9300290900273,
36.0171424031941,36.1042587818684,36.1913704442032,36.2785014746032,36.3302467257931,
36.4173750083753,36.5086525355003,36.5957638177863,36.6828711123603,36.7699915760908,
36.7824851168753),.UNSPECIFIED.);
#266=B_SPLINE_CURVE_WITH_KNOTS('',3,(#37555,#37556,#37557,#37558,#37559,
#37560,#37561,#37562,#37563,#37564,#37565,#37566),.UNSPECIFIED.,.F.,.F.,
(4,1,1,1,1,1,1,1,1,4),(30.4992330148162,30.9694242504221,31.4567717481831,
31.9441192459441,32.4314667437051,32.9188142414661,33.4061617392271,33.8935092369881,
34.3808567347491,34.5575191593334),.UNSPECIFIED.);
#267=B_SPLINE_CURVE_WITH_KNOTS('',3,(#37572,#37573,#37574,#37575,#37576,
#37577,#37578,#37579,#37580,#37581,#37582,#37583,#37584,#37585,#37586,#37587,
#37588,#37589,#37590,#37591,#37592,#37593,#37594,#37595,#37596,#37597,#37598,
#37599,#37600,#37601,#37602,#37603,#37604,#37605,#37606,#37607,#37608,#37609,
#37610,#37611,#37612,#37613,#37614,#37615,#37616,#37617,#37618,#37619,#37620,
#37621,#37622,#37623,#37624,#37625,#37626,#37627,#37628,#37629,#37630,#37631,
#37632,#37633,#37634,#37635,#37636,#37637,#37638,#37639,#37640,#37641,#37642,
#37643,#37644,#37645,#37646,#37647,#37648,#37649,#37650,#37651,#37652,#37653,
#37654,#37655,#37656,#37657,#37658,#37659,#37660,#37661,#37662,#37663,#37664,
#37665,#37666,#37667,#37668,#37669,#37670,#37671,#37672,#37673,#37674,#37675,
#37676,#37677,#37678,#37679,#37680,#37681,#37682,#37683,#37684,#37685,#37686,
#37687,#37688,#37689,#37690,#37691,#37692,#37693,#37694,#37695,#37696,#37697,
#37698,#37699,#37700,#37701,#37702,#37703,#37704,#37705,#37706,#37707,#37708,
#37709,#37710,#37711,#37712,#37713,#37714,#37715,#37716,#37717,#37718,#37719,
#37720,#37721,#37722),.UNSPECIFIED.,.F.,.F.,(4,3,3,3,3,3,3,3,3,3,3,3,3,
3,3,3,3,3,3,3,3,3,3,3,3,3,3,3,3,3,3,3,3,3,3,3,3,3,3,3,3,3,3,3,3,3,3,3,3,
3,4),(24.2156473321997,24.3000481377873,24.3845026911335,24.469084228759,
24.5239778062131,24.605573799559,24.687063482264,24.7684676194937,24.8498068741228,
24.931109516876,25.0123941556188,25.0936793685597,25.1749837330098,25.2563793332889,
25.3378207724143,25.4194005876772,25.4986728017351,25.583262289203,25.6677481290383,
25.7521476956501,25.8364782913607,25.9207556105826,26.0050037953159,26.0892384271216,
26.1734750749651,26.2577608699837,26.3420728889482,26.4264656031797,26.4733677972571,
26.5580943048163,26.642759224378,26.727377075819,26.8119655200819,26.8965525888317,
26.9607152950181,27.051939514377,27.1432570572615,27.234675022306,27.3261221417869,
27.4175857805144,27.4480627927791,27.5325902280114,27.617072650843,27.7015343147517,
27.7859813021922,27.8704512660146,27.9354102905401,28.0240739238239,28.1127403128143,
28.2014266288529,28.2743338823081),.UNSPECIFIED.);
#268=B_SPLINE_CURVE_WITH_KNOTS('',3,(#37723,#37724,#37725,#37726,#37727,
#37728,#37729,#37730,#37731,#37732,#37733,#37734,#37735,#37736,#37737,#37738,
#37739,#37740,#37741,#37742,#37743,#37744,#37745,#37746,#37747,#37748,#37749,
#37750,#37751,#37752,#37753,#37754,#37755,#37756,#37757,#37758,#37759,#37760,
#37761,#37762,#37763,#37764,#37765,#37766,#37767,#37768,#37769,#37770,#37771,
#37772,#37773,#37774,#37775,#37776,#37777,#37778,#37779,#37780,#37781,#37782,
#37783,#37784,#37785,#37786,#37787,#37788,#37789,#37790,#37791,#37792,#37793,
#37794,#37795,#37796,#37797,#37798,#37799,#37800,#37801,#37802,#37803,#37804,
#37805,#37806,#37807),.UNSPECIFIED.,.F.,.F.,(4,3,3,3,3,3,3,3,3,3,3,3,3,
3,3,3,3,3,3,3,3,3,3,3,3,3,3,3,4),(28.2743338824266,28.3664499676938,28.4227577883011,
28.5092534192787,28.5957248380328,28.6821936309558,28.768655843137,28.8551399477051,
28.9101052860621,28.9974337506621,29.0847479974582,29.1720668007956,29.2593812251369,
29.3467137364858,29.3974527838231,29.4845627017913,29.5716560821199,29.658752741023,
29.7458448521569,29.8329567644714,29.8848002815841,29.9719014591824,30.0589855683635,
30.1460722455977,30.2331539951606,30.3202550460865,30.3721477793451,30.459306360454,
30.4993214304177),.UNSPECIFIED.);
#269=B_SPLINE_CURVE_WITH_KNOTS('',3,(#37809,#37810,#37811,#37812,#37813,
#37814,#37815,#37816),.UNSPECIFIED.,.F.,.F.,(4,1,1,1,1,4),(28.2743353127056,
29.0200342593781,29.5073817571391,29.9947292549001,30.4820767526611,30.4992330148162),
 .UNSPECIFIED.);
#270=B_SPLINE_CURVE_WITH_KNOTS('',3,(#37817,#37818,#37819,#37820,#37821,
#37822,#37823,#37824,#37825,#37826,#37827,#37828,#37829,#37830,#37831,#37832,
#37833,#37834,#37835,#37836,#37837,#37838,#37839,#37840,#37841,#37842,#37843,
#37844,#37845,#37846,#37847,#37848,#37849,#37850,#37851,#37852,#37853,#37854,
#37855,#37856,#37857,#37858,#37859,#37860,#37861,#37862,#37863,#37864,#37865,
#37866,#37867,#37868,#37869,#37870,#37871,#37872,#37873,#37874,#37875,#37876,
#37877,#37878,#37879,#37880,#37881,#37882,#37883,#37884,#37885,#37886,#37887,
#37888,#37889,#37890,#37891,#37892,#37893,#37894,#37895,#37896,#37897,#37898,
#37899,#37900,#37901,#37902,#37903,#37904,#37905,#37906,#37907,#37908,#37909,
#37910,#37911,#37912,#37913,#37914,#37915,#37916,#37917,#37918,#37919,#37920,
#37921,#37922,#37923,#37924,#37925,#37926,#37927,#37928,#37929,#37930,#37931,
#37932,#37933,#37934,#37935,#37936,#37937,#37938,#37939,#37940,#37941,#37942,
#37943,#37944,#37945,#37946,#37947,#37948,#37949,#37950,#37951,#37952,#37953,
#37954,#37955,#37956,#37957,#37958,#37959,#37960,#37961,#37962,#37963,#37964),
 .UNSPECIFIED.,.F.,.F.,(4,3,3,3,3,3,3,3,3,3,3,3,3,3,3,3,3,3,3,3,3,3,3,3,
3,3,3,3,3,3,3,3,3,3,3,3,3,3,3,3,3,3,3,3,3,3,3,3,3,4),(24.2161266164728,
24.3048755834868,24.3936190635417,24.482346583967,24.5710622783973,24.6339067795291,
24.7183759992437,24.8028244958566,24.8872895482853,24.9717606994971,25.0562878722159,
25.1212542772901,25.212715341686,25.3041653224886,25.3955607374181,25.486895306588,
25.578117015447,25.6086017750511,25.6931842451492,25.7777639703814,25.8623869523081,
25.9470308674618,26.0317533205491,26.0959492728121,26.1803441484525,26.2646716876325,
26.3489491297302,26.433193670525,26.5174390722406,26.6016888841523,26.6859586779554,
26.770264035995,26.8546692836303,26.9391296144661,27.0237146307952,27.0706442683341,
27.1522400678308,27.2337295557392,27.3151334973669,27.3964725557215,27.4777750017013,
27.5590594433115,27.640344458871,27.7216486258011,27.8030440293227,27.8844852717219,
27.9660648922686,28.0453392638561,28.1696867713369,28.2743338823081),
 .UNSPECIFIED.);
#271=B_SPLINE_CURVE_WITH_KNOTS('',3,(#37970,#37971,#37972,#37973,#37974,
#37975,#37976,#37977,#37978,#37979,#37980,#37981,#37982,#37983,#37984,#37985,
#37986,#37987,#37988,#37989,#37990,#37991,#37992,#37993,#37994,#37995,#37996,
#37997,#37998,#37999,#38000,#38001,#38002,#38003,#38004,#38005,#38006,#38007,
#38008,#38009,#38010,#38011,#38012,#38013,#38014,#38015,#38016,#38017,#38018,
#38019,#38020,#38021,#38022,#38023,#38024,#38025,#38026,#38027,#38028,#38029,
#38030,#38031,#38032,#38033,#38034,#38035,#38036,#38037,#38038,#38039,#38040,
#38041,#38042,#38043,#38044,#38045,#38046,#38047,#38048,#38049,#38050,#38051,
#38052,#38053,#38054),.UNSPECIFIED.,.F.,.F.,(4,3,3,3,3,3,3,3,3,3,3,3,3,
3,3,3,3,3,3,3,3,3,3,3,3,3,3,3,4),(15.7079632709815,15.7983388023486,15.861651819831,
15.9487475083028,16.0358262241585,16.122907705879,16.2099843848246,16.2970806037435,
16.348999317592,16.4361366409196,16.5232574899998,16.6103814427677,16.6975006825434,
16.784639229082,16.836346815353,16.9234776545726,17.010591981452,17.0977094188805,
17.1848221629971,17.2719543014269,17.323694313114,17.4108212370465,17.4979315692867,
17.5850449316704,17.6721535648928,17.7592815727833,17.811041810875,17.8981734291986,
17.9329528346437),.UNSPECIFIED.);
#272=B_SPLINE_CURVE_WITH_KNOTS('',3,(#38056,#38057,#38058,#38059,#38060,
#38061),.UNSPECIFIED.,.F.,.F.,(4,1,1,4),(14.399609326548,14.886956824309,
15.37430432207,15.707963267949),.UNSPECIFIED.);
#273=B_SPLINE_CURVE_WITH_KNOTS('',3,(#38065,#38066,#38067,#38068,#38069,
#38070,#38071,#38072,#38073,#38074,#38075,#38076,#38077,#38078,#38079,#38080,
#38081,#38082,#38083,#38084,#38085,#38086,#38087,#38088,#38089,#38090,#38091,
#38092,#38093,#38094,#38095,#38096,#38097,#38098,#38099,#38100,#38101,#38102,
#38103,#38104,#38105,#38106,#38107,#38108,#38109,#38110,#38111,#38112,#38113,
#38114,#38115,#38116,#38117,#38118,#38119,#38120,#38121,#38122,#38123,#38124,
#38125,#38126,#38127,#38128,#38129,#38130,#38131),.UNSPECIFIED.,.F.,.F.,
(4,3,3,3,3,3,3,3,3,3,3,3,3,3,3,3,3,3,3,3,3,3,4),(13.8747245557601,13.96151957655,
14.0483127680288,14.1350983392423,14.2219048683033,14.289680353232,14.3768111864995,
14.4639255073661,14.5510429387493,14.6381556768169,14.7252878092448,14.777027850993,
14.8641547740402,14.9512651053716,15.03837846682,15.1254870990942,15.2126151060248,
15.264375348754,15.3512430123807,15.4404230762728,15.5272738407879,15.6176185543684,
15.707963267949),.UNSPECIFIED.);
#274=B_SPLINE_CURVE_WITH_KNOTS('',3,(#38132,#38133,#38134,#38135,#38136,
#38137,#38138,#38139,#38140),.UNSPECIFIED.,.F.,.F.,(4,1,1,1,1,1,4),(15.707963267949,
15.751722846515,16.239070344276,16.7264178420371,17.2137653397981,17.7011128375591,
17.9329414843961),.UNSPECIFIED.);
#275=B_SPLINE_CURVE_WITH_KNOTS('',3,(#38146,#38147,#38148,#38149,#38150,
#38151,#38152,#38153),.UNSPECIFIED.,.F.,.F.,(4,1,1,1,1,4),(181.295997048056,
181.669120728045,182.667957178007,183.666793627969,184.665630077931,185.353966561798),
 .UNSPECIFIED.);
#276=B_SPLINE_CURVE_WITH_KNOTS('',3,(#38155,#38156,#38157,#38158,#38159),
 .UNSPECIFIED.,.F.,.F.,(4,1,4),(185.353966561798,185.664466527893,186.663302977854),
 .UNSPECIFIED.);
#277=B_SPLINE_CURVE_WITH_KNOTS('',3,(#38163,#38164,#38165,#38166,#38167,
#38168,#38169,#38170,#38171,#38172,#38173,#38174,#38175,#38176,#38177,#38178,
#38179,#38180,#38181,#38182,#38183,#38184,#38185,#38186,#38187,#38188,#38189,
#38190,#38191,#38192,#38193,#38194,#38195,#38196,#38197,#38198,#38199,#38200,
#38201,#38202,#38203,#38204,#38205,#38206,#38207,#38208,#38209,#38210,#38211,
#38212,#38213,#38214,#38215,#38216,#38217,#38218,#38219,#38220),
 .UNSPECIFIED.,.F.,.F.,(4,3,3,3,3,3,3,3,3,3,3,3,3,3,3,3,3,3,3,4),(185.353966561798,
185.451129858625,185.54817353966,185.645152137366,185.742096643968,185.839038006741,
185.9360686719,186.033145887057,186.130383559085,186.198496245335,186.297011795472,
186.395389344314,186.494243526173,186.592449207881,186.690623911412,186.788797212158,
186.888153608916,186.986470035736,187.086346417463,187.18622279919),
 .UNSPECIFIED.);
#278=B_SPLINE_CURVE_WITH_KNOTS('',3,(#38221,#38222,#38223,#38224,#38225,
#38226,#38227,#38228),.UNSPECIFIED.,.F.,.F.,(4,1,1,1,1,4),(181.297167488959,
182.203150445487,183.201986895449,184.200823345411,185.199659795373,185.353966561798),
 .UNSPECIFIED.);
#279=B_SPLINE_CURVE_WITH_KNOTS('',3,(#38234,#38235,#38236,#38237,#38238,
#38239,#38240,#38241,#38242,#38243,#38244,#38245,#38246,#38247,#38248,#38249,
#38250,#38251,#38252,#38253,#38254,#38255,#38256,#38257,#38258,#38259,#38260,
#38261,#38262,#38263,#38264,#38265,#38266,#38267,#38268,#38269,#38270,#38271,
#38272,#38273,#38274,#38275,#38276,#38277,#38278,#38279,#38280,#38281,#38282,
#38283,#38284,#38285,#38286,#38287,#38288,#38289,#38290,#38291,#38292,#38293,
#38294,#38295,#38296,#38297,#38298,#38299,#38300,#38301,#38302,#38303,#38304,
#38305,#38306,#38307,#38308,#38309,#38310,#38311,#38312,#38313,#38314,#38315,
#38316,#38317,#38318,#38319,#38320,#38321,#38322,#38323,#38324,#38325,#38326,
#38327,#38328,#38329,#38330,#38331,#38332,#38333,#38334,#38335,#38336,#38337,
#38338,#38339,#38340,#38341,#38342,#38343,#38344,#38345,#38346,#38347,#38348,
#38349,#38350,#38351,#38352,#38353,#38354,#38355,#38356,#38357),
 .UNSPECIFIED.,.F.,.F.,(4,3,3,3,3,3,3,3,3,3,3,3,3,3,3,3,3,3,3,3,3,3,3,3,
3,3,3,3,3,3,3,3,3,3,3,3,3,3,3,3,3,4),(175.013888595044,175.112152253394,
175.210394737751,175.308645521428,175.40699963151,175.505407688072,175.603986032395,
175.676102028274,175.774697491594,175.873152609552,175.973375843138,176.071652747408,
176.169896682952,176.268137135791,176.369837471402,176.468219314363,176.571578896299,
176.674938478236,176.773539089412,176.871999342765,176.972221290944,177.070503263901,
177.168752232521,177.266997676458,177.368691989393,177.467078669032,177.570426798615,
177.673774928198,177.772377752086,177.87084027796,177.971061665485,178.069346039596,
178.167597451745,178.265845378085,178.367536878104,178.465926110356,178.569268744258,
178.672611378159,178.782250156969,178.891545552981,179.000249474037,179.070781030164),
 .UNSPECIFIED.);
#280=B_SPLINE_CURVE_WITH_KNOTS('',3,(#38358,#38359,#38360,#38361,#38362,
#38363),.UNSPECIFIED.,.F.,.F.,(4,1,1,4),(179.070781254618,179.671447828121,
180.670284278083,181.295997048056),.UNSPECIFIED.);
#281=B_SPLINE_CURVE_WITH_KNOTS('',3,(#38365,#38366,#38367,#38368,#38369,
#38370,#38371),.UNSPECIFIED.,.F.,.F.,(4,1,1,1,4),(179.070781254618,179.206641095602,
180.205477545564,181.204313995525,181.297167488959),.UNSPECIFIED.);
#282=B_SPLINE_CURVE_WITH_KNOTS('',3,(#38372,#38373,#38374,#38375,#38376,
#38377,#38378,#38379),.UNSPECIFIED.,.F.,.F.,(4,1,1,1,1,4),(175.012544756164,
175.211295295754,176.210131745716,177.208968195678,178.20780464564,179.070781254618),
 .UNSPECIFIED.);
#283=B_SPLINE_CURVE_WITH_KNOTS('',3,(#38385,#38386,#38387,#38388,#38389,
#38390,#38391,#38392,#38393,#38394,#38395,#38396,#38397,#38398,#38399,#38400,
#38401,#38402,#38403,#38404,#38405,#38406,#38407,#38408,#38409,#38410,#38411,
#38412,#38413,#38414,#38415,#38416,#38417,#38418,#38419,#38420,#38421,#38422,
#38423,#38424,#38425,#38426,#38427,#38428,#38429,#38430,#38431,#38432,#38433,
#38434,#38435,#38436,#38437,#38438,#38439,#38440,#38441,#38442,#38443,#38444,
#38445,#38446,#38447,#38448,#38449,#38450,#38451,#38452,#38453,#38454,#38455,
#38456,#38457,#38458,#38459,#38460,#38461,#38462,#38463,#38464,#38465,#38466,
#38467,#38468,#38469,#38470,#38471,#38472,#38473,#38474,#38475,#38476,#38477,
#38478,#38479,#38480,#38481,#38482,#38483,#38484,#38485,#38486,#38487,#38488,
#38489,#38490,#38491,#38492,#38493,#38494,#38495,#38496,#38497,#38498,#38499,
#38500,#38501,#38502,#38503,#38504,#38505,#38506,#38507,#38508),
 .UNSPECIFIED.,.F.,.F.,(4,3,3,3,3,3,3,3,3,3,3,3,3,3,3,3,3,3,3,3,3,3,3,3,
3,3,3,3,3,3,3,3,3,3,3,3,3,3,3,3,3,4),(168.73049948352,168.829027726418,
168.927431036374,169.025741344548,169.124002438926,169.222243820297,169.320494962343,
169.418850307068,169.517260913146,169.615840311951,169.683083328503,169.781681404697,
169.880139138671,169.980361718645,170.078641227933,170.176887758804,170.275130793941,
170.376828040072,170.475212406819,170.578566092641,170.681919778464,170.780517924844,
170.878975728609,170.979198291086,171.077477868714,171.175724467241,171.273967569265,
171.375664734055,171.474049165113,171.57740269677,171.680756228426,171.779354490085,
171.877812410303,171.978034943814,172.076314639908,172.174561357392,172.272804578702,
172.374501603624,172.472886153556,172.576239415972,172.679592678388,172.787595947439),
 .UNSPECIFIED.);
#284=B_SPLINE_CURVE_WITH_KNOTS('',3,(#38509,#38510,#38511,#38512,#38513,
#38514,#38515,#38516,#38517,#38518,#38519,#38520,#38521,#38522,#38523,#38524,
#38525,#38526,#38527,#38528,#38529,#38530,#38531,#38532,#38533,#38534,#38535,
#38536,#38537,#38538,#38539,#38540,#38541,#38542,#38543,#38544,#38545,#38546,
#38547,#38548,#38549,#38550,#38551,#38552,#38553,#38554,#38555,#38556,#38557,
#38558,#38559,#38560,#38561,#38562,#38563,#38564,#38565,#38566,#38567,#38568,
#38569,#38570,#38571,#38572,#38573,#38574,#38575,#38576,#38577,#38578,#38579,
#38580,#38581),.UNSPECIFIED.,.F.,.F.,(4,3,3,3,3,3,3,3,3,3,3,3,3,3,3,3,3,
3,3,3,3,3,3,3,4),(172.787595947668,172.884841559506,172.984040005612,173.081071838667,
173.178059271087,173.275033215733,173.375882193887,173.472980628238,173.570144972561,
173.667458410759,173.67842912835,173.777027506202,173.875485539322,173.975708044196,
174.073987844422,174.172234662569,174.270477980966,174.372174880302,174.470559517526,
174.573912547919,174.677265578312,174.775844825957,174.874301063312,174.972645507633,
175.013888595044),.UNSPECIFIED.);
#285=B_SPLINE_CURVE_WITH_KNOTS('',3,(#38583,#38584,#38585,#38586,#38587,
#38588),.UNSPECIFIED.,.F.,.F.,(4,1,1,4),(172.787601414733,173.21362239583,
174.212458845792,175.012544756164),.UNSPECIFIED.);
#286=B_SPLINE_CURVE_WITH_KNOTS('',3,(#38589,#38590,#38591,#38592,#38593,
#38594,#38595,#38596,#38597,#38598,#38599,#38600,#38601,#38602,#38603,#38604,
#38605,#38606,#38607,#38608,#38609,#38610,#38611,#38612,#38613,#38614,#38615,
#38616,#38617,#38618,#38619,#38620,#38621,#38622,#38623,#38624,#38625,#38626,
#38627,#38628,#38629,#38630,#38631,#38632,#38633,#38634,#38635,#38636,#38637,
#38638,#38639,#38640,#38641,#38642,#38643,#38644,#38645,#38646,#38647,#38648,
#38649,#38650,#38651,#38652,#38653,#38654,#38655,#38656,#38657,#38658,#38659,
#38660,#38661,#38662,#38663,#38664,#38665,#38666,#38667,#38668,#38669,#38670,
#38671,#38672,#38673,#38674,#38675,#38676,#38677,#38678,#38679,#38680,#38681,
#38682,#38683,#38684,#38685,#38686,#38687,#38688,#38689,#38690,#38691,#38692,
#38693,#38694,#38695,#38696,#38697,#38698,#38699,#38700,#38701,#38702,#38703,
#38704,#38705,#38706,#38707,#38708,#38709,#38710,#38711,#38712),
 .UNSPECIFIED.,.F.,.F.,(4,3,3,3,3,3,3,3,3,3,3,3,3,3,3,3,3,3,3,3,3,3,3,3,
3,3,3,3,3,3,3,3,3,3,3,3,3,3,3,3,3,4),(168.73021503563,168.828460503106,
168.92680521135,169.025197844636,169.123767881175,169.218276595983,169.316874714603,
169.415332491002,169.51555506037,169.61383461178,169.71208118457,169.810324261369,
169.912021457513,170.010405864863,170.113759455404,170.217113045945,170.315711171922,
170.414168955614,170.514391523151,170.612671081646,170.710917661431,170.809160745123,
170.910857932819,171.009242346745,171.112595921326,171.215949495907,171.314547642583,
171.413005447132,171.513228009474,171.611507589065,171.709754189987,171.807997294831,
171.90969445759,172.008078892486,172.111432419178,172.214785945869,172.315617765289,
172.416285943601,172.51678187547,172.617176498695,172.717484580153,172.787595947439),
 .UNSPECIFIED.);
#287=B_SPLINE_CURVE_WITH_KNOTS('',3,(#38718,#38719,#38720,#38721,#38722,
#38723,#38724,#38725),.UNSPECIFIED.,.F.,.F.,(4,1,1,1,1,4),(162.446146668403,
162.691228178769,163.690064628731,164.688901078693,165.687737528655,166.504405682607),
 .UNSPECIFIED.);
#288=B_SPLINE_CURVE_WITH_KNOTS('',3,(#38726,#38727,#38728,#38729,#38730,
#38731,#38732,#38733,#38734,#38735,#38736,#38737,#38738,#38739,#38740,#38741,
#38742,#38743,#38744,#38745,#38746,#38747,#38748,#38749,#38750,#38751,#38752,
#38753,#38754,#38755,#38756,#38757,#38758,#38759,#38760,#38761,#38762,#38763,
#38764,#38765,#38766,#38767,#38768,#38769,#38770,#38771,#38772,#38773,#38774,
#38775,#38776,#38777,#38778,#38779,#38780,#38781,#38782,#38783,#38784,#38785,
#38786,#38787,#38788,#38789,#38790,#38791,#38792,#38793,#38794,#38795),
 .UNSPECIFIED.,.F.,.F.,(4,3,3,3,3,3,3,3,3,3,3,3,3,3,3,3,3,3,3,3,3,3,3,4),
(166.504410640259,166.652910770048,166.686573978617,166.78517209724,166.883629873641,
166.983852443008,167.08213199442,167.180378567212,167.278621644013,167.380318840155,
167.478703247507,167.582056838043,167.685410428579,167.784008554557,167.882466338249,
167.982688905786,168.080968464281,168.179215044066,168.277458127759,168.379155315454,
168.477539729381,168.580893303961,168.684246878541,168.73049948352),
 .UNSPECIFIED.);
#289=B_SPLINE_CURVE_WITH_KNOTS('',3,(#38797,#38798,#38799,#38800,#38801,
#38802,#38803,#38804,#38805,#38806,#38807,#38808,#38809,#38810,#38811,#38812,
#38813,#38814,#38815,#38816,#38817,#38818,#38819,#38820,#38821,#38822,#38823,
#38824,#38825,#38826,#38827,#38828,#38829,#38830,#38831,#38832,#38833,#38834,
#38835,#38836,#38837,#38838,#38839,#38840,#38841,#38842,#38843,#38844,#38845,
#38846,#38847,#38848,#38849,#38850,#38851,#38852,#38853,#38854,#38855,#38856,
#38857,#38858,#38859,#38860,#38861,#38862,#38863,#38864,#38865,#38866,#38867,
#38868,#38869),.UNSPECIFIED.,.F.,.F.,(4,3,3,3,3,3,3,3,3,3,3,3,3,3,3,3,3,
3,3,3,3,3,3,3,4),(166.504410640259,166.6019131263,166.699371433808,166.79681599036,
166.894277201722,166.991846173226,167.089478292235,167.187269535436,167.220603696059,
167.319201820914,167.417659603534,167.517882171345,167.616161728897,167.714408307787,
167.812651390635,167.914348579482,168.012732992696,168.116086569359,168.219440146021,
168.318036793105,168.421081353736,168.51941990506,168.617691685804,168.715928358201,
168.73021503563),.UNSPECIFIED.);
#290=B_SPLINE_CURVE_WITH_KNOTS('',3,(#38870,#38871,#38872,#38873,#38874,
#38875,#38876,#38877,#38878,#38879,#38880,#38881,#38882,#38883,#38884,#38885,
#38886,#38887,#38888,#38889,#38890,#38891,#38892,#38893,#38894,#38895,#38896,
#38897,#38898,#38899,#38900,#38901,#38902,#38903,#38904,#38905,#38906,#38907,
#38908,#38909,#38910,#38911,#38912,#38913,#38914,#38915,#38916,#38917,#38918,
#38919,#38920,#38921,#38922,#38923,#38924,#38925,#38926,#38927,#38928,#38929,
#38930,#38931,#38932,#38933,#38934,#38935,#38936,#38937,#38938,#38939,#38940,
#38941,#38942,#38943,#38944,#38945,#38946,#38947,#38948,#38949,#38950,#38951,
#38952,#38953,#38954,#38955,#38956,#38957,#38958,#38959,#38960,#38961,#38962,
#38963,#38964,#38965,#38966,#38967,#38968,#38969,#38970,#38971,#38972,#38973,
#38974,#38975,#38976,#38977,#38978,#38979,#38980,#38981,#38982,#38983,#38984,
#38985,#38986,#38987,#38988,#38989,#38990,#38991,#38992,#38993),
 .UNSPECIFIED.,.F.,.F.,(4,3,3,3,3,3,3,3,3,3,3,3,3,3,3,3,3,3,3,3,3,3,3,3,
3,3,3,3,3,3,3,3,3,3,3,3,3,3,3,3,3,4),(162.447662171796,162.545987468187,
162.644256962553,162.742500165391,162.840746554158,162.939093168736,163.037489137586,
163.136060795295,163.225257896212,163.323856021116,163.422313803793,163.522536371591,
163.62081592922,163.719062508196,163.817305591138,163.919002779897,164.017387193222,
164.120740769698,164.224094346174,164.322692471118,164.421150253833,164.521372821621,
164.619652379285,164.717898958294,164.816142041267,164.917839229984,165.016223643336,
165.119577219736,165.222930796135,165.321528921635,165.419986704909,165.520209272557,
165.618488830783,165.716735410353,165.814978493886,165.916675681939,166.015060095843,
166.11841367097,166.221767246097,166.344599874415,166.465474953167,166.504410639987),
 .UNSPECIFIED.);
#291=B_SPLINE_CURVE_WITH_KNOTS('',3,(#38999,#39000,#39001,#39002,#39003,
#39004,#39005,#39006,#39007,#39008,#39009,#39010,#39011,#39012,#39013,#39014,
#39015,#39016,#39017,#39018,#39019,#39020,#39021,#39022,#39023,#39024,#39025,
#39026,#39027,#39028,#39029,#39030,#39031,#39032,#39033,#39034,#39035,#39036,
#39037,#39038,#39039,#39040,#39041,#39042,#39043,#39044,#39045,#39046,#39047,
#39048,#39049,#39050,#39051,#39052,#39053,#39054,#39055,#39056,#39057,#39058,
#39059,#39060,#39061,#39062,#39063,#39064,#39065,#39066,#39067,#39068,#39069,
#39070,#39071,#39072,#39073,#39074,#39075,#39076,#39077,#39078,#39079,#39080,
#39081,#39082,#39083,#39084,#39085,#39086,#39087,#39088,#39089,#39090,#39091,
#39092,#39093,#39094,#39095,#39096,#39097,#39098,#39099,#39100,#39101,#39102,
#39103,#39104,#39105,#39106,#39107,#39108,#39109,#39110,#39111,#39112,#39113,
#39114,#39115,#39116,#39117,#39118,#39119,#39120,#39121,#39122,#39123,#39124,
#39125),.UNSPECIFIED.,.F.,.F.,(4,3,3,3,3,3,3,3,3,3,3,3,3,3,3,3,3,3,3,3,
3,3,3,3,3,3,3,3,3,3,3,3,3,3,3,3,3,3,3,3,3,3,4),(156.163987530313,156.262228574752,
156.360486836606,156.458853630025,156.557282386566,156.655872483791,156.698209478998,
156.796807604012,156.895265386799,156.995487954569,157.093767512308,157.192014091391,
157.29025717444,157.39195436307,157.490338776499,157.593692352729,157.69704592896,
157.795644053952,157.894101836717,157.994324404493,158.092603962209,158.190850541271,
158.289093624298,158.390790812954,158.489175226362,158.592528802642,158.695882378922,
158.794480503912,158.892938286675,158.993160854451,159.091440412165,159.189686991224,
159.287930074248,159.389627262907,159.488011676312,159.591365252598,159.694718828884,
159.797216560019,159.903218753284,160.005303397591,160.107256278835,160.209067828953,
160.22122533308),.UNSPECIFIED.);
#292=B_SPLINE_CURVE_WITH_KNOTS('',3,(#39126,#39127,#39128,#39129,#39130,
#39131),.UNSPECIFIED.,.F.,.F.,(4,1,1,4),(160.221227414795,160.693555278846,
161.692391728808,162.446146668403),.UNSPECIFIED.);
#293=B_SPLINE_CURVE_WITH_KNOTS('',3,(#39133,#39134,#39135,#39136,#39137,
#39138,#39139,#39140,#39141,#39142,#39143,#39144,#39145,#39146,#39147,#39148,
#39149,#39150,#39151,#39152,#39153,#39154,#39155,#39156,#39157,#39158,#39159,
#39160,#39161,#39162,#39163,#39164,#39165,#39166,#39167,#39168,#39169,#39170,
#39171,#39172,#39173,#39174,#39175,#39176,#39177,#39178,#39179,#39180,#39181,
#39182,#39183,#39184,#39185,#39186,#39187,#39188,#39189,#39190,#39191,#39192,
#39193,#39194,#39195,#39196,#39197,#39198,#39199,#39200,#39201,#39202,#39203,
#39204,#39205),.UNSPECIFIED.,.F.,.F.,(4,3,3,3,3,3,3,3,3,3,3,3,3,3,3,3,3,
3,3,3,3,3,3,3,4),(160.22122533308,160.228748546326,160.327346671318,160.425804454083,
160.526027021859,160.624306579575,160.722553158637,160.820796241664,160.92249343032,
161.020877843728,161.124231420008,161.227584996288,161.326183121278,161.424640904041,
161.524863471817,161.623143029531,161.72138960859,161.819632691614,161.921329880273,
162.019714293678,162.123067869964,162.22642144625,162.325027406001,162.423481500101,
162.447662171796),.UNSPECIFIED.);
#294=B_SPLINE_CURVE_WITH_KNOTS('',3,(#39206,#39207,#39208,#39209,#39210,
#39211,#39212,#39213,#39214,#39215,#39216,#39217,#39218,#39219,#39220,#39221,
#39222,#39223,#39224,#39225,#39226,#39227,#39228,#39229,#39230,#39231,#39232,
#39233,#39234,#39235,#39236,#39237,#39238,#39239,#39240,#39241,#39242,#39243,
#39244,#39245,#39246,#39247,#39248,#39249,#39250,#39251,#39252,#39253,#39254,
#39255,#39256,#39257,#39258,#39259,#39260,#39261,#39262,#39263,#39264,#39265,
#39266,#39267,#39268,#39269,#39270,#39271,#39272,#39273,#39274,#39275,#39276,
#39277,#39278,#39279,#39280,#39281,#39282,#39283,#39284,#39285,#39286,#39287,
#39288,#39289,#39290,#39291,#39292,#39293,#39294,#39295,#39296,#39297,#39298,
#39299,#39300,#39301,#39302,#39303,#39304,#39305,#39306,#39307,#39308,#39309,
#39310,#39311,#39312,#39313,#39314,#39315,#39316,#39317,#39318,#39319,#39320,
#39321,#39322,#39323,#39324,#39325,#39326,#39327,#39328,#39329),
 .UNSPECIFIED.,.F.,.F.,(4,3,3,3,3,3,3,3,3,3,3,3,3,3,3,3,3,3,3,3,3,3,3,3,
3,3,3,3,3,3,3,3,3,3,3,3,3,3,3,3,3,4),(156.163531866271,156.233402746479,
156.332000871484,156.430458654262,156.530681222034,156.628960779764,156.727207358839,
156.825450441879,156.927147630519,157.025532043939,157.12888562019,157.23223919644,
157.330837321442,157.429295104218,157.529517671991,157.627797229718,157.72604380879,
157.824286891827,157.925984080471,158.024368493888,158.127722070145,158.231075646402,
158.329673771403,158.428131554177,158.528354121951,158.626633679676,158.724880258747,
158.823123341783,158.924820530428,159.023204943844,159.126558520104,159.229912096364,
159.328378576654,159.426704810661,159.526019875932,159.624169149678,159.722285836342,
159.820399593048,159.920606027993,160.018861091251,160.120043212039,160.221225332828),
 .UNSPECIFIED.);
#295=B_SPLINE_CURVE_WITH_KNOTS('',3,(#39335,#39336,#39337,#39338,#39339,
#39340,#39341,#39342),.UNSPECIFIED.,.F.,.F.,(4,1,1,1,1,4),(149.881541639708,
150.705190779227,151.704027229189,152.702863679151,153.701700129113,153.938039726867),
 .UNSPECIFIED.);
#296=B_SPLINE_CURVE_WITH_KNOTS('',3,(#39343,#39344,#39345,#39346,#39347,
#39348,#39349,#39350,#39351,#39352,#39353,#39354,#39355,#39356,#39357,#39358,
#39359,#39360,#39361,#39362,#39363,#39364,#39365,#39366,#39367,#39368,#39369,
#39370,#39371,#39372,#39373,#39374,#39375,#39376,#39377,#39378,#39379,#39380,
#39381,#39382,#39383,#39384,#39385,#39386,#39387,#39388,#39389,#39390,#39391,
#39392,#39393,#39394,#39395,#39396,#39397,#39398,#39399,#39400,#39401,#39402,
#39403,#39404,#39405,#39406,#39407,#39408,#39409,#39410,#39411,#39412),
 .UNSPECIFIED.,.F.,.F.,(4,3,3,3,3,3,3,3,3,3,3,3,3,3,3,3,3,3,3,3,3,3,3,4),
(153.9380400259,154.035163898234,154.132222574362,154.229246955324,154.326267897773,
154.423381488606,154.520541056366,154.617870832504,154.700536579074,154.799134704076,
154.897592486852,154.997815054625,155.096094612352,155.194341191424,155.292584274461,
155.394281463105,155.492665876523,155.596019452779,155.699373029036,155.797975862229,
155.896415143044,155.994759399118,156.093038592398,156.163987530313),
 .UNSPECIFIED.);
#297=B_SPLINE_CURVE_WITH_KNOTS('',3,(#39414,#39415,#39416,#39417,#39418,
#39419,#39420,#39421,#39422,#39423,#39424,#39425,#39426,#39427,#39428,#39429,
#39430,#39431,#39432,#39433,#39434,#39435,#39436,#39437,#39438,#39439,#39440,
#39441,#39442,#39443,#39444,#39445,#39446,#39447,#39448,#39449,#39450,#39451,
#39452,#39453,#39454,#39455,#39456,#39457,#39458,#39459,#39460,#39461,#39462,
#39463,#39464,#39465,#39466,#39467,#39468,#39469,#39470,#39471,#39472,#39473,
#39474,#39475,#39476,#39477,#39478,#39479,#39480,#39481,#39482,#39483),
 .UNSPECIFIED.,.F.,.F.,(4,3,3,3,3,3,3,3,3,3,3,3,3,3,3,3,3,3,3,3,3,3,3,4),
(153.938040202769,154.056659980237,154.176963650994,154.235729846555,154.334327971559,
154.432785754335,154.533008322108,154.631287879836,154.729534458909,154.827777541948,
154.92947473059,155.027859144009,155.131212720263,155.234566296517,155.333169148014,
155.431630381054,155.529972651705,155.628250049486,155.726492098718,155.824728281924,
155.923038846763,156.021391522228,156.119876942615,156.163531866271),
 .UNSPECIFIED.);
#298=B_SPLINE_CURVE_WITH_KNOTS('',3,(#39484,#39485,#39486,#39487,#39488,
#39489,#39490,#39491),.UNSPECIFIED.,.F.,.F.,(4,1,1,1,1,4),(149.880018430852,
150.240384046707,151.239220496669,152.238056946631,153.236893396593,153.9380400259),
 .UNSPECIFIED.);
#299=B_SPLINE_CURVE_WITH_KNOTS('',3,(#39497,#39498,#39499,#39500,#39501,
#39502,#39503,#39504,#39505,#39506,#39507,#39508,#39509,#39510,#39511,#39512,
#39513,#39514,#39515,#39516,#39517,#39518,#39519,#39520,#39521,#39522,#39523,
#39524,#39525,#39526,#39527,#39528,#39529,#39530,#39531,#39532,#39533,#39534,
#39535,#39536,#39537,#39538,#39539,#39540,#39541,#39542,#39543,#39544,#39545,
#39546,#39547,#39548,#39549,#39550,#39551,#39552,#39553,#39554,#39555,#39556,
#39557,#39558,#39559,#39560,#39561,#39562,#39563,#39564,#39565,#39566,#39567,
#39568,#39569,#39570,#39571,#39572,#39573,#39574,#39575,#39576,#39577,#39578,
#39579,#39580,#39581,#39582,#39583,#39584,#39585,#39586,#39587,#39588,#39589,
#39590,#39591,#39592,#39593,#39594,#39595,#39596,#39597,#39598,#39599,#39600,
#39601,#39602,#39603,#39604,#39605,#39606,#39607,#39608,#39609,#39610,#39611,
#39612,#39613,#39614,#39615,#39616,#39617,#39618,#39619,#39620,#39621,#39622,
#39623),.UNSPECIFIED.,.F.,.F.,(4,3,3,3,3,3,3,3,3,3,3,3,3,3,3,3,3,3,3,3,
3,3,3,3,3,3,3,3,3,3,3,3,3,3,3,3,3,3,3,3,3,3,4),(143.597018446188,143.695621188533,
143.713335629494,143.811933754498,143.910391537275,144.010614105047,144.108893662775,
144.207140241849,144.305383324887,144.40708051353,144.505464926948,144.608818503202,
144.712172079456,144.81077020446,144.909227987236,145.009450555009,145.107730112737,
145.20597669181,145.304219774849,145.405916963491,145.50430137691,145.607654953164,
145.711008529418,145.809606654422,145.908064437198,146.008287004971,146.106566562699,
146.204813141772,146.303056224811,146.404753413453,146.503137826872,146.606491403125,
146.709844979379,146.807643480436,146.905302408374,147.002849316603,147.100335701354,
147.197792033696,147.295248746519,147.392798083501,147.490396206244,147.588155506493,
147.65485471872),.UNSPECIFIED.);
#300=B_SPLINE_CURVE_WITH_KNOTS('',3,(#39624,#39625,#39626,#39627,#39628,
#39629,#39630),.UNSPECIFIED.,.F.,.F.,(4,1,1,1,4),(147.65485471872,147.708681429341,
148.707517879303,149.706354329265,149.881541639708),.UNSPECIFIED.);
#301=B_SPLINE_CURVE_WITH_KNOTS('',3,(#39632,#39633,#39634,#39635,#39636,
#39637),.UNSPECIFIED.,.F.,.F.,(4,1,1,4),(147.65485471872,148.242711146784,
149.241547596745,149.880018430852),.UNSPECIFIED.);
#302=B_SPLINE_CURVE_WITH_KNOTS('',3,(#39638,#39639,#39640,#39641,#39642,
#39643,#39644,#39645,#39646,#39647,#39648,#39649,#39650,#39651,#39652,#39653,
#39654,#39655,#39656,#39657,#39658,#39659,#39660,#39661,#39662,#39663,#39664,
#39665,#39666,#39667,#39668,#39669,#39670,#39671,#39672,#39673,#39674,#39675,
#39676,#39677,#39678,#39679,#39680,#39681,#39682,#39683,#39684,#39685,#39686,
#39687,#39688,#39689,#39690,#39691,#39692,#39693,#39694,#39695,#39696,#39697,
#39698,#39699,#39700,#39701,#39702,#39703,#39704,#39705,#39706,#39707,#39708,
#39709,#39710,#39711,#39712,#39713,#39714,#39715,#39716,#39717,#39718,#39719,
#39720,#39721,#39722,#39723,#39724,#39725,#39726,#39727,#39728,#39729,#39730,
#39731,#39732,#39733,#39734,#39735,#39736,#39737,#39738,#39739,#39740,#39741,
#39742,#39743,#39744,#39745,#39746,#39747,#39748,#39749,#39750,#39751,#39752,
#39753,#39754,#39755,#39756,#39757,#39758,#39759,#39760,#39761),
 .UNSPECIFIED.,.F.,.F.,(4,3,3,3,3,3,3,3,3,3,3,3,3,3,3,3,3,3,3,3,3,3,3,3,
3,3,3,3,3,3,3,3,3,3,3,3,3,3,3,3,3,4),(143.597933860091,143.696192254726,
143.794433309395,143.89268649678,143.991045284982,144.089461466197,144.188044027423,
144.247365346936,144.34596347194,144.444421254716,144.544643822489,144.642923380217,
144.741169959291,144.839413042329,144.941110230971,145.03949464439,145.142848220644,
145.246201796898,145.344799921902,145.443257704679,145.543480272451,145.64175983018,
145.740006409253,145.838249492291,145.939946680933,146.038331094352,146.141684670606,
146.24503824686,146.343636371864,146.442094154641,146.542316722413,146.640596280141,
146.738842859215,146.837085942254,146.938783130896,147.037167544314,147.140521120568,
147.243874696822,147.352569174393,147.460952550047,147.568802109383,147.654854305396),
 .UNSPECIFIED.);
#303=B_SPLINE_CURVE_WITH_KNOTS('',3,(#39767,#39768,#39769,#39770,#39771,
#39772,#39773,#39774,#39775,#39776,#39777,#39778,#39779,#39780,#39781,#39782,
#39783,#39784,#39785,#39786,#39787,#39788,#39789,#39790,#39791,#39792,#39793,
#39794,#39795,#39796,#39797,#39798,#39799,#39800,#39801,#39802,#39803,#39804,
#39805,#39806,#39807,#39808,#39809,#39810,#39811,#39812,#39813,#39814,#39815,
#39816,#39817,#39818,#39819,#39820,#39821,#39822,#39823,#39824,#39825,#39826,
#39827,#39828,#39829,#39830,#39831,#39832,#39833,#39834,#39835,#39836,#39837,
#39838,#39839,#39840,#39841,#39842,#39843,#39844,#39845,#39846,#39847,#39848,
#39849,#39850,#39851,#39852,#39853,#39854,#39855,#39856,#39857,#39858,#39859,
#39860,#39861,#39862,#39863,#39864,#39865,#39866,#39867,#39868,#39869,#39870,
#39871,#39872,#39873,#39874,#39875,#39876,#39877,#39878,#39879,#39880,#39881,
#39882,#39883,#39884,#39885,#39886,#39887,#39888,#39889,#39890),
 .UNSPECIFIED.,.F.,.F.,(4,3,3,3,3,3,3,3,3,3,3,3,3,3,3,3,3,3,3,3,3,3,3,3,
3,3,3,3,3,3,3,3,3,3,3,3,3,3,3,3,3,4),(137.314044031679,137.41561225619,
137.513996896003,137.617156912863,137.720316929723,137.818915054727,137.917372837504,
138.017595405276,138.115874963004,138.214121542078,138.312364625116,138.414061813758,
138.512446227177,138.61579980343,138.719153379684,138.817751504688,138.916209287464,
139.016431855237,139.114711412965,139.212957992039,139.311201075077,139.412898263719,
139.511282677138,139.614636253392,139.717989829646,139.81658795465,139.915045737427,
140.015268305199,140.113547862927,140.211794442001,140.310037525039,140.411734713682,
140.5101191271,140.613472703354,140.716826279608,140.815569227393,140.914173010821,
141.012667061739,141.111081830931,141.209449097701,141.307822396312,141.371669411541),
 .UNSPECIFIED.);
#304=B_SPLINE_CURVE_WITH_KNOTS('',3,(#39891,#39892,#39893,#39894,#39895,
#39896,#39897,#39898,#39899,#39900,#39901,#39902,#39903,#39904,#39905,#39906,
#39907,#39908,#39909,#39910,#39911,#39912,#39913,#39914,#39915,#39916,#39917,
#39918,#39919,#39920,#39921,#39922,#39923,#39924,#39925,#39926,#39927,#39928,
#39929,#39930,#39931,#39932,#39933,#39934,#39935,#39936,#39937,#39938,#39939,
#39940,#39941,#39942,#39943,#39944,#39945,#39946,#39947,#39948,#39949,#39950,
#39951,#39952,#39953,#39954,#39955,#39956,#39957),.UNSPECIFIED.,.F.,.F.,
(4,3,3,3,3,3,3,3,3,3,3,3,3,3,3,3,3,3,3,3,3,3,4),(141.371669411768,141.485016004535,
141.600339367052,141.71566272957,141.814260854574,141.91271863735,142.012941205123,
142.111220762851,142.209467341925,142.307710424963,142.409407613605,142.507792027024,
142.611145603278,142.714499179532,142.813105314799,142.911543009971,143.009885026333,
143.108160960057,143.206400336868,143.304679404108,143.402973649619,143.501391759057,
143.597018446188),.UNSPECIFIED.);
#305=B_SPLINE_CURVE_WITH_KNOTS('',3,(#39959,#39960,#39961,#39962,#39963,
#39964,#39965,#39966,#39967,#39968,#39969,#39970,#39971,#39972,#39973,#39974,
#39975,#39976,#39977,#39978,#39979,#39980,#39981,#39982,#39983,#39984,#39985,
#39986,#39987,#39988,#39989,#39990,#39991,#39992,#39993,#39994,#39995,#39996,
#39997,#39998,#39999,#40000,#40001,#40002,#40003,#40004,#40005,#40006,#40007,
#40008,#40009,#40010,#40011,#40012,#40013,#40014,#40015,#40016,#40017,#40018,
#40019,#40020,#40021,#40022,#40023,#40024,#40025,#40026,#40027,#40028),
 .UNSPECIFIED.,.F.,.F.,(4,3,3,3,3,3,3,3,3,3,3,3,3,3,3,3,3,3,3,3,3,3,3,4),
(141.371669411541,141.468831254161,141.566438903267,141.66339620349,141.760311911022,
141.857216996242,141.955335858935,142.052368429038,142.151030438025,142.249692447012,
142.348290572016,142.446748354792,142.546970922565,142.645250480293,142.743497059367,
142.841740142405,142.943437331047,143.041821744466,143.14517532072,143.248528896974,
143.347104955711,143.445558136395,143.543900701735,143.597933860091),
 .UNSPECIFIED.);
#306=B_SPLINE_CURVE_WITH_KNOTS('',3,(#40029,#40030,#40031,#40032,#40033,
#40034,#40035,#40036),.UNSPECIFIED.,.F.,.F.,(4,1,1,1,1,4),(137.314688012658,
138.254346647165,139.253183097127,140.252019547089,141.25085599705,141.371669411541),
 .UNSPECIFIED.);
#307=B_SPLINE_CURVE_WITH_KNOTS('',3,(#40042,#40043,#40044,#40045,#40046,
#40047,#40048,#40049,#40050,#40051,#40052,#40053,#40054,#40055,#40056,#40057,
#40058,#40059,#40060,#40061,#40062,#40063,#40064,#40065,#40066,#40067,#40068,
#40069,#40070,#40071,#40072,#40073,#40074,#40075,#40076,#40077,#40078,#40079,
#40080,#40081,#40082,#40083,#40084,#40085,#40086,#40087,#40088,#40089,#40090,
#40091,#40092,#40093,#40094,#40095,#40096,#40097,#40098,#40099,#40100,#40101,
#40102,#40103,#40104,#40105,#40106,#40107,#40108,#40109,#40110,#40111,#40112,
#40113,#40114,#40115,#40116,#40117,#40118,#40119,#40120,#40121,#40122,#40123,
#40124,#40125,#40126,#40127,#40128,#40129,#40130,#40131,#40132,#40133,#40134,
#40135,#40136,#40137,#40138,#40139,#40140,#40141,#40142,#40143,#40144,#40145,
#40146,#40147,#40148,#40149,#40150,#40151,#40152,#40153,#40154,#40155,#40156,
#40157,#40158,#40159,#40160,#40161,#40162,#40163,#40164,#40165),
 .UNSPECIFIED.,.F.,.F.,(4,3,3,3,3,3,3,3,3,3,3,3,3,3,3,3,3,3,3,3,3,3,3,3,
3,3,3,3,3,3,3,3,3,3,3,3,3,3,3,3,3,4),(131.031654909927,131.129931649269,
131.228177184675,131.326420997262,131.426640305434,131.525027337791,131.626162783871,
131.727298229951,131.825896354955,131.924354137731,132.024576705504,132.122856263232,
132.221102842306,132.319345925344,132.421043113987,132.519427527405,132.622781103659,
132.726134679913,132.824732804917,132.923190587693,133.023413155466,133.121692713194,
133.219939292268,133.318182375306,133.419879563948,133.518263977367,133.621617553621,
133.724971129875,133.823569254879,133.922027037655,134.022249605428,134.120529163156,
134.218775742229,134.317018825268,134.41871601391,134.517100427329,134.620454003583,
134.723807579837,134.8363385207,134.948409000642,135.059693750754,135.088484104126),
 .UNSPECIFIED.);
#308=B_SPLINE_CURVE_WITH_KNOTS('',3,(#40166,#40167,#40168,#40169,#40170,
#40171,#40172,#40173,#40174,#40175,#40176,#40177,#40178,#40179,#40180,#40181,
#40182,#40183,#40184,#40185,#40186,#40187,#40188,#40189,#40190,#40191,#40192,
#40193,#40194,#40195,#40196,#40197,#40198,#40199,#40200,#40201,#40202,#40203,
#40204,#40205,#40206,#40207,#40208,#40209,#40210,#40211,#40212,#40213,#40214,
#40215,#40216,#40217,#40218,#40219,#40220,#40221,#40222,#40223,#40224,#40225,
#40226,#40227,#40228,#40229,#40230,#40231,#40232,#40233,#40234,#40235),
 .UNSPECIFIED.,.F.,.F.,(4,3,3,3,3,3,3,3,3,3,3,3,3,3,3,3,3,3,3,3,3,3,3,4),
(135.088484104361,135.187254556185,135.286029876603,135.384838499173,135.483776463585,
135.582788468007,135.681976179005,135.722644029799,135.821242154803,135.919699937579,
136.019922505352,136.11820206308,136.216448642154,136.314691725192,136.416388913834,
136.514773327253,136.618126903507,136.721480479761,136.820067256337,136.918521077998,
137.017401816418,137.115677656305,137.214860843992,137.314044031679),
 .UNSPECIFIED.);
#309=B_SPLINE_CURVE_WITH_KNOTS('',3,(#40237,#40238,#40239,#40240,#40241,
#40242,#40243),.UNSPECIFIED.,.F.,.F.,(4,1,1,1,4),(135.088484104361,135.257837297279,
136.256673747241,137.255510197203,137.314688012658),.UNSPECIFIED.);
#310=B_SPLINE_CURVE_WITH_KNOTS('',3,(#40244,#40245,#40246,#40247,#40248,
#40249,#40250,#40251,#40252,#40253,#40254,#40255,#40256,#40257,#40258,#40259,
#40260,#40261,#40262,#40263,#40264,#40265,#40266,#40267,#40268,#40269,#40270,
#40271,#40272,#40273,#40274,#40275,#40276,#40277,#40278,#40279,#40280,#40281,
#40282,#40283,#40284,#40285,#40286,#40287,#40288,#40289,#40290,#40291,#40292,
#40293,#40294,#40295,#40296,#40297,#40298,#40299,#40300,#40301,#40302,#40303,
#40304,#40305,#40306,#40307,#40308,#40309,#40310,#40311,#40312,#40313,#40314,
#40315,#40316,#40317,#40318,#40319,#40320,#40321,#40322,#40323,#40324,#40325,
#40326,#40327,#40328,#40329,#40330,#40331,#40332,#40333,#40334,#40335,#40336,
#40337,#40338,#40339,#40340,#40341,#40342,#40343,#40344,#40345,#40346,#40347,
#40348,#40349,#40350,#40351,#40352,#40353,#40354,#40355,#40356,#40357,#40358,
#40359,#40360,#40361,#40362,#40363,#40364,#40365,#40366,#40367,#40368,#40369,
#40370),.UNSPECIFIED.,.F.,.F.,(4,3,3,3,3,3,3,3,3,3,3,3,3,3,3,3,3,3,3,3,
3,3,3,3,3,3,3,3,3,3,3,3,3,3,3,3,3,3,3,3,3,3,4),(131.030544881201,131.128979377099,
131.227573069973,131.262491497432,131.361089622436,131.459547405212,131.559769972985,
131.658049530713,131.756296109786,131.854539192825,131.956236381467,132.054620794886,
132.15797437114,132.261327947394,132.359926072398,132.458383855174,132.558606422947,
132.656885980675,132.755132559748,132.853375642787,132.955072831429,133.053457244848,
133.156810821101,133.260164397355,133.358762522359,133.457220305135,133.557442872908,
133.655722430636,133.753969009709,133.852212092748,133.95390928139,134.052293694809,
134.155647271063,134.259000847317,134.356128675187,134.453094160804,134.549968416923,
134.6467826177,134.743567858739,134.84039997176,134.937256811786,135.034231214226,
135.088484104361),.UNSPECIFIED.);
#311=B_SPLINE_CURVE_WITH_KNOTS('',3,(#40376,#40377,#40378,#40379,#40380,
#40381,#40382,#40383),.UNSPECIFIED.,.F.,.F.,(4,1,1,1,1,4),(124.748033420129,
125.73427953018,126.733115980142,127.731952430104,128.730788880066,128.805298797182),
 .UNSPECIFIED.);
#312=B_SPLINE_CURVE_WITH_KNOTS('',3,(#40384,#40385,#40386,#40387,#40388,
#40389,#40390,#40391,#40392,#40393,#40394,#40395,#40396,#40397,#40398,#40399,
#40400,#40401,#40402,#40403,#40404,#40405,#40406,#40407,#40408,#40409,#40410,
#40411,#40412,#40413,#40414,#40415,#40416,#40417,#40418,#40419,#40420,#40421,
#40422,#40423,#40424,#40425,#40426,#40427,#40428,#40429,#40430,#40431,#40432,
#40433,#40434,#40435,#40436,#40437,#40438,#40439,#40440,#40441,#40442,#40443,
#40444,#40445,#40446,#40447,#40448,#40449,#40450,#40451,#40452,#40453),
 .UNSPECIFIED.,.F.,.F.,(4,3,3,3,3,3,3,3,3,3,3,3,3,3,3,3,3,3,3,3,3,3,3,4),
(128.805298797182,128.902840431273,129.000250613517,129.097560812666,129.194818343698,
129.292053887497,129.389298094495,129.486642967568,129.584044330746,129.68160592498,
129.729625330028,129.828223455032,129.926681237808,130.026903805581,130.125183363309,
130.223429942382,130.321673025421,130.423370214063,130.521754627482,130.625108203735,
130.728461779989,130.827047027854,130.92935096889,131.031654909927),
 .UNSPECIFIED.);
#313=B_SPLINE_CURVE_WITH_KNOTS('',3,(#40455,#40456,#40457,#40458,#40459,
#40460,#40461,#40462,#40463,#40464,#40465,#40466,#40467,#40468,#40469,#40470,
#40471,#40472,#40473,#40474,#40475,#40476,#40477,#40478,#40479,#40480,#40481,
#40482,#40483,#40484,#40485,#40486,#40487,#40488,#40489,#40490,#40491,#40492,
#40493,#40494,#40495,#40496,#40497,#40498,#40499,#40500,#40501,#40502,#40503,
#40504,#40505,#40506,#40507,#40508,#40509,#40510,#40511,#40512,#40513,#40514,
#40515,#40516,#40517,#40518,#40519,#40520,#40521,#40522,#40523,#40524),
 .UNSPECIFIED.,.F.,.F.,(4,3,3,3,3,3,3,3,3,3,3,3,3,3,3,3,3,3,3,3,3,3,3,4),
(128.805299011162,128.910085619872,129.015255759152,129.120630109634,129.226318351048,
129.264818597508,129.363416722512,129.461874505289,129.562097073061,129.660376630789,
129.758623209863,129.856866292901,129.958563481543,130.056947894962,130.160301471216,
130.26365504747,130.36222548666,130.460667523607,130.5590108659,130.657285118185,
130.755545076202,130.853792579344,130.95210867263,131.030544881201),
 .UNSPECIFIED.);
#314=B_SPLINE_CURVE_WITH_KNOTS('',3,(#40525,#40526,#40527,#40528,#40529,
#40530,#40531,#40532),.UNSPECIFIED.,.F.,.F.,(4,1,1,1,1,4),(124.748072377546,
125.26947279766,126.268309247622,127.267145697584,128.265982147546,128.805298797182),
 .UNSPECIFIED.);
#315=B_SPLINE_CURVE_WITH_KNOTS('',3,(#40538,#40539,#40540,#40541,#40542,
#40543,#40544,#40545,#40546,#40547,#40548,#40549,#40550,#40551,#40552,#40553,
#40554,#40555,#40556,#40557,#40558,#40559,#40560,#40561,#40562,#40563,#40564,
#40565,#40566,#40567,#40568,#40569,#40570,#40571,#40572,#40573,#40574,#40575,
#40576,#40577,#40578,#40579,#40580,#40581,#40582,#40583,#40584,#40585,#40586,
#40587,#40588,#40589,#40590,#40591,#40592,#40593,#40594,#40595,#40596,#40597,
#40598,#40599,#40600,#40601,#40602,#40603,#40604,#40605,#40606,#40607,#40608,
#40609,#40610,#40611,#40612,#40613,#40614,#40615,#40616,#40617,#40618,#40619,
#40620,#40621,#40622,#40623,#40624,#40625,#40626,#40627,#40628,#40629,#40630,
#40631,#40632,#40633,#40634,#40635,#40636,#40637,#40638,#40639,#40640,#40641,
#40642,#40643,#40644,#40645,#40646,#40647,#40648,#40649,#40650,#40651,#40652,
#40653,#40654,#40655,#40656,#40657,#40658,#40659,#40660,#40661),
 .UNSPECIFIED.,.F.,.F.,(4,3,3,3,3,3,3,3,3,3,3,3,3,3,3,3,3,3,3,3,3,3,3,3,
3,3,3,3,3,3,3,3,3,3,3,3,3,3,3,3,3,4),(118.464214545145,118.56261566319,
118.66118993359,118.742424380447,118.841022505451,118.939480288228,119.039702856,
119.137982413729,119.236228992802,119.334472075841,119.436169264483,119.534553677901,
119.637907254155,119.741260830409,119.839858955413,119.938316738189,120.038539305962,
120.13681886369,120.235065442764,120.333308525802,120.435005714444,120.533390127863,
120.636743704117,120.740097280371,120.838695405375,120.937153188151,121.037375755924,
121.135655313652,121.233901892726,121.332144975764,121.433842164406,121.532226577825,
121.635580154079,121.738933730333,121.836831200292,121.933909156543,122.030894120917,
122.127817176647,122.226391254986,122.323316910845,122.422715200424,122.522113490002),
 .UNSPECIFIED.);
#316=B_SPLINE_CURVE_WITH_KNOTS('',3,(#40662,#40663,#40664,#40665,#40666,
#40667,#40668),.UNSPECIFIED.,.F.,.F.,(4,1,1,1,4),(122.522113490002,122.737770180294,
123.736606630256,124.735443080218,124.748033420129),.UNSPECIFIED.);
#317=B_SPLINE_CURVE_WITH_KNOTS('',3,(#40670,#40671,#40672,#40673,#40674,
#40675),.UNSPECIFIED.,.F.,.F.,(4,1,1,4),(122.522113490002,123.271799897737,
124.270636347699,124.748072377546),.UNSPECIFIED.);
#318=B_SPLINE_CURVE_WITH_KNOTS('',3,(#40676,#40677,#40678,#40679,#40680,
#40681,#40682,#40683,#40684,#40685,#40686,#40687,#40688,#40689,#40690,#40691,
#40692,#40693,#40694,#40695,#40696,#40697,#40698,#40699,#40700,#40701,#40702,
#40703,#40704,#40705,#40706,#40707,#40708,#40709,#40710,#40711,#40712,#40713,
#40714,#40715,#40716,#40717,#40718,#40719,#40720,#40721,#40722,#40723,#40724,
#40725,#40726,#40727,#40728,#40729,#40730,#40731,#40732,#40733,#40734,#40735,
#40736,#40737,#40738,#40739,#40740,#40741,#40742,#40743,#40744,#40745,#40746,
#40747,#40748,#40749,#40750,#40751,#40752,#40753,#40754,#40755,#40756,#40757,
#40758,#40759,#40760,#40761,#40762,#40763,#40764,#40765,#40766,#40767,#40768,
#40769,#40770,#40771,#40772,#40773,#40774,#40775,#40776,#40777,#40778,#40779,
#40780,#40781,#40782,#40783,#40784,#40785,#40786,#40787,#40788,#40789,#40790,
#40791,#40792,#40793,#40794,#40795,#40796,#40797,#40798,#40799),
 .UNSPECIFIED.,.F.,.F.,(4,3,3,3,3,3,3,3,3,3,3,3,3,3,3,3,3,3,3,3,3,3,3,3,
3,3,3,3,3,3,3,3,3,3,3,3,3,3,3,3,3,4),(118.465360086526,118.566746837947,
118.665030453745,118.763278645539,118.861520898174,118.959786681794,119.058164510988,
119.156609979378,119.255210784522,119.276454097889,119.375052222893,119.47351000567,
119.573732573442,119.67201213117,119.770258710244,119.868501793282,119.970198981925,
120.068583395343,120.171936971597,120.275290547851,120.373888672855,120.472346455631,
120.572569023404,120.670848581132,120.769095160206,120.867338243244,120.969035431886,
121.067419845305,121.170773421559,121.274126997813,121.372725122817,121.471182905593,
121.571405473366,121.669685031094,121.767931610168,121.866174693206,121.967871881848,
122.066256295267,122.169609871521,122.272963447775,122.400857829823,122.522113389964),
 .UNSPECIFIED.);
#319=B_SPLINE_CURVE_WITH_KNOTS('',3,(#40805,#40806,#40807,#40808,#40809,
#40810,#40811,#40812,#40813,#40814,#40815,#40816,#40817,#40818,#40819,#40820,
#40821,#40822,#40823,#40824,#40825,#40826,#40827,#40828,#40829,#40830,#40831,
#40832,#40833,#40834,#40835,#40836,#40837,#40838,#40839,#40840,#40841,#40842,
#40843,#40844,#40845,#40846,#40847,#40848,#40849,#40850,#40851,#40852,#40853,
#40854,#40855,#40856,#40857,#40858,#40859,#40860,#40861,#40862,#40863,#40864,
#40865,#40866,#40867,#40868,#40869,#40870,#40871,#40872,#40873,#40874,#40875,
#40876,#40877,#40878,#40879,#40880,#40881,#40882,#40883,#40884,#40885,#40886,
#40887,#40888,#40889,#40890,#40891,#40892,#40893,#40894,#40895,#40896,#40897,
#40898,#40899,#40900,#40901,#40902,#40903,#40904,#40905,#40906,#40907,#40908,
#40909,#40910,#40911,#40912,#40913,#40914,#40915,#40916,#40917,#40918,#40919,
#40920,#40921,#40922,#40923,#40924,#40925,#40926,#40927,#40928),
 .UNSPECIFIED.,.F.,.F.,(4,3,3,3,3,3,3,3,3,3,3,3,3,3,3,3,3,3,3,3,3,3,3,3,
3,3,3,3,3,3,3,3,3,3,3,3,3,3,3,3,3,4),(112.18179086962,112.280032772378,
112.378281876154,112.47663365233,112.575038389947,112.673614569146,112.749405680676,
112.84800380568,112.946461588456,113.046684156229,113.144963713957,113.243210293031,
113.341453376069,113.443150564711,113.54153497813,113.644888554384,113.748242130638,
113.846840255642,113.945298038418,114.045520606191,114.143800163919,114.242046742992,
114.34028982603,114.441987014672,114.540371428091,114.643725004345,114.747078580599,
114.845676705603,114.94413448838,115.044357056152,115.14263661388,115.240883192953,
115.339126275992,115.440823464634,115.539207878053,115.642561454307,115.745915030561,
115.84988875933,115.953561696348,116.057054365164,116.160309146371,116.238928182547),
 .UNSPECIFIED.);
#320=B_SPLINE_CURVE_WITH_KNOTS('',3,(#40929,#40930,#40931,#40932,#40933,
#40934,#40935,#40936,#40937,#40938,#40939,#40940,#40941,#40942,#40943,#40944,
#40945,#40946,#40947,#40948,#40949,#40950,#40951,#40952,#40953,#40954,#40955,
#40956,#40957,#40958,#40959,#40960,#40961,#40962,#40963,#40964,#40965,#40966,
#40967,#40968,#40969,#40970,#40971,#40972,#40973,#40974,#40975,#40976,#40977,
#40978,#40979,#40980,#40981,#40982,#40983,#40984,#40985,#40986,#40987,#40988,
#40989,#40990,#40991,#40992,#40993,#40994,#40995,#40996,#40997,#40998),
 .UNSPECIFIED.,.F.,.F.,(4,3,3,3,3,3,3,3,3,3,3,3,3,3,3,3,3,3,3,3,3,3,3,4),
(116.238928182823,116.341566510357,116.44447107289,116.547509821617,116.650828963887,
116.744751480523,116.843349605527,116.941807388304,117.042029956076,117.140309513804,
117.238556092878,117.336799175916,117.438496364558,117.536880777977,117.640234354231,
117.743587930485,117.842162082222,117.940606624247,118.03895126967,118.137225626964,
118.235476585645,118.333714612371,118.431998836496,118.464214545145),
 .UNSPECIFIED.);
#321=B_SPLINE_CURVE_WITH_KNOTS('',3,(#41000,#41001,#41002,#41003,#41004,
#41005,#41006,#41007,#41008,#41009,#41010,#41011,#41012,#41013,#41014,#41015,
#41016,#41017,#41018,#41019,#41020,#41021,#41022,#41023,#41024,#41025,#41026,
#41027,#41028,#41029,#41030,#41031,#41032,#41033,#41034,#41035,#41036,#41037,
#41038,#41039,#41040,#41041,#41042,#41043,#41044,#41045,#41046,#41047,#41048,
#41049,#41050,#41051,#41052,#41053,#41054,#41055,#41056,#41057,#41058,#41059,
#41060,#41061,#41062,#41063,#41064,#41065,#41066,#41067,#41068,#41069),
 .UNSPECIFIED.,.F.,.F.,(4,3,3,3,3,3,3,3,3,3,3,3,3,3,3,3,3,3,3,3,3,3,3,4),
(116.238928182823,116.279944748004,116.378542873008,116.477000655784,116.577223223557,
116.675502781285,116.773749360358,116.871992443397,116.973689632039,117.072074045458,
117.175427621712,117.278781197966,117.37737932297,117.475837105746,117.576059673519,
117.674339231247,117.77258581032,117.870828893359,117.972526082001,118.07091049542,
118.174264071673,118.277617647927,118.376189313854,118.465360086526),
 .UNSPECIFIED.);
#322=B_SPLINE_CURVE_WITH_KNOTS('',3,(#41070,#41071,#41072,#41073,#41074,
#41075,#41076,#41077),.UNSPECIFIED.,.F.,.F.,(4,1,1,1,1,4),(112.180986264767,
112.284598948156,113.283435398118,114.28227184808,115.281108298042,116.238922797563),
 .UNSPECIFIED.);
#323=B_SPLINE_CURVE_WITH_KNOTS('',3,(#41083,#41084,#41085,#41086,#41087,
#41088,#41089,#41090,#41091,#41092,#41093,#41094,#41095,#41096,#41097,#41098,
#41099,#41100,#41101,#41102,#41103,#41104,#41105,#41106,#41107,#41108,#41109,
#41110,#41111,#41112,#41113,#41114,#41115,#41116,#41117,#41118,#41119,#41120,
#41121,#41122,#41123,#41124,#41125,#41126,#41127,#41128,#41129,#41130,#41131,
#41132,#41133,#41134,#41135,#41136,#41137,#41138,#41139,#41140,#41141,#41142,
#41143,#41144,#41145,#41146,#41147,#41148,#41149,#41150,#41151,#41152,#41153,
#41154,#41155,#41156,#41157,#41158,#41159,#41160,#41161,#41162,#41163,#41164,
#41165,#41166,#41167,#41168,#41169,#41170,#41171,#41172,#41173,#41174,#41175,
#41176,#41177,#41178,#41179,#41180,#41181,#41182,#41183,#41184,#41185,#41186,
#41187,#41188,#41189,#41190,#41191,#41192,#41193,#41194,#41195,#41196,#41197,
#41198,#41199,#41200,#41201,#41202,#41203,#41204,#41205,#41206),
 .UNSPECIFIED.,.F.,.F.,(4,3,3,3,3,3,3,3,3,3,3,3,3,3,3,3,3,3,3,3,3,3,3,3,
3,3,3,3,3,3,3,3,3,3,3,3,3,3,3,3,3,4),(105.898938865661,105.997345912726,
106.095658421174,106.1939206985,106.292162246928,106.39041254066,106.488766432876,
106.587174674105,106.685752753546,106.756386980904,106.854985105908,106.953442888684,
107.053665456457,107.151945014185,107.250191593259,107.348434676297,107.450131864939,
107.548516278358,107.651869854612,107.755223430866,107.85382155587,107.952279338646,
108.052501906419,108.150781464147,108.249028043221,108.347271126259,108.448968314901,
108.54735272832,108.650706304574,108.754059880828,108.852658005832,108.951115788608,
109.051338356381,109.149617914109,109.247864493183,109.346107576221,109.447804764863,
109.546189178282,109.649542754536,109.75289633079,109.893212936353,109.955742875643),
 .UNSPECIFIED.);
#324=B_SPLINE_CURVE_WITH_KNOTS('',3,(#41207,#41208,#41209,#41210,#41211,
#41212,#41213,#41214,#41215,#41216,#41217,#41218,#41219,#41220,#41221,#41222,
#41223,#41224,#41225,#41226,#41227,#41228,#41229,#41230,#41231,#41232,#41233,
#41234,#41235,#41236,#41237,#41238,#41239,#41240,#41241,#41242,#41243,#41244,
#41245,#41246,#41247,#41248,#41249,#41250,#41251,#41252,#41253,#41254,#41255,
#41256,#41257,#41258,#41259,#41260,#41261,#41262,#41263,#41264,#41265,#41266,
#41267,#41268,#41269,#41270,#41271,#41272,#41273,#41274,#41275,#41276,#41277,
#41278,#41279),.UNSPECIFIED.,.F.,.F.,(4,3,3,3,3,3,3,3,3,3,3,3,3,3,3,3,3,
3,3,3,3,3,3,3,4),(109.955742875951,110.055241614051,110.152151423466,110.249014842069,
110.345862894414,110.447330365999,110.544300028994,110.641334438529,110.738518045248,
110.751732780752,110.850330905756,110.948788688532,111.049011256305,111.147290814033,
111.245537393106,111.343780476145,111.445477664787,111.543862078206,111.64721565446,
111.750569230714,111.849176820424,111.947618966301,112.045965736429,112.144240689708,
112.18179086962),.UNSPECIFIED.);
#325=B_SPLINE_CURVE_WITH_KNOTS('',3,(#41281,#41282,#41283,#41284,#41285,
#41286),.UNSPECIFIED.,.F.,.F.,(4,1,1,4),(109.95575001023,110.286926048232,
111.285762498194,112.180986264767),.UNSPECIFIED.);
#326=B_SPLINE_CURVE_WITH_KNOTS('',3,(#41287,#41288,#41289,#41290,#41291,
#41292,#41293,#41294,#41295,#41296,#41297,#41298,#41299,#41300,#41301,#41302,
#41303,#41304,#41305,#41306,#41307,#41308,#41309,#41310,#41311,#41312,#41313,
#41314,#41315,#41316,#41317,#41318,#41319,#41320,#41321,#41322,#41323,#41324,
#41325,#41326,#41327,#41328,#41329,#41330,#41331,#41332,#41333,#41334,#41335,
#41336,#41337,#41338,#41339,#41340,#41341,#41342,#41343,#41344,#41345,#41346,
#41347,#41348,#41349,#41350,#41351,#41352,#41353,#41354,#41355,#41356,#41357,
#41358,#41359,#41360,#41361,#41362,#41363,#41364,#41365,#41366,#41367,#41368,
#41369,#41370,#41371,#41372,#41373,#41374,#41375,#41376,#41377,#41378,#41379,
#41380,#41381,#41382,#41383,#41384,#41385,#41386,#41387,#41388,#41389,#41390,
#41391,#41392,#41393,#41394,#41395,#41396,#41397,#41398,#41399,#41400,#41401,
#41402,#41403,#41404,#41405,#41406,#41407,#41408,#41409,#41410),
 .UNSPECIFIED.,.F.,.F.,(4,3,3,3,3,3,3,3,3,3,3,3,3,3,3,3,3,3,3,3,3,3,3,3,
3,3,3,3,3,3,3,3,3,3,3,3,3,3,3,3,3,4),(105.898082482581,105.996456924032,
106.09484730115,106.193416271827,106.291580248385,106.390178373389,106.488636156165,
106.588858723938,106.687138281666,106.78538486074,106.883627943778,106.98532513242,
107.083709545839,107.187063122093,107.290416698347,107.389014823351,107.487472606127,
107.5876951739,107.685974731628,107.784221310702,107.88246439374,107.984161582382,
108.082545995801,108.185899572055,108.289253148309,108.387851273313,108.486309056089,
108.586531623862,108.68481118159,108.783057760664,108.881300843702,108.982998032344,
109.081382445763,109.184736022017,109.288089598271,109.386591328536,109.484956309733,
109.583214317042,109.681399820025,109.779540599734,109.877698313766,109.955742875643),
 .UNSPECIFIED.);
#327=B_SPLINE_CURVE_WITH_KNOTS('',3,(#41416,#41417,#41418,#41419,#41420,
#41421,#41422,#41423),.UNSPECIFIED.,.F.,.F.,(4,1,1,1,1,4),(99.6144331696528,
99.7645318311714,100.763368281133,101.762204731095,102.761041181057,103.67254885852),
 .UNSPECIFIED.);
#328=B_SPLINE_CURVE_WITH_KNOTS('',3,(#41424,#41425,#41426,#41427,#41428,
#41429,#41430,#41431,#41432,#41433,#41434,#41435,#41436,#41437,#41438,#41439,
#41440,#41441,#41442,#41443,#41444,#41445,#41446,#41447,#41448,#41449,#41450,
#41451,#41452,#41453,#41454,#41455,#41456,#41457,#41458,#41459,#41460,#41461,
#41462,#41463,#41464,#41465,#41466,#41467,#41468,#41469,#41470,#41471,#41472,
#41473,#41474,#41475,#41476,#41477,#41478,#41479,#41480,#41481,#41482,#41483,
#41484,#41485,#41486,#41487,#41488,#41489,#41490,#41491,#41492,#41493),
 .UNSPECIFIED.,.F.,.F.,(4,3,3,3,3,3,3,3,3,3,3,3,3,3,3,3,3,3,3,3,3,3,3,4),
(103.672557568463,103.759877631019,103.858475756023,103.956933538799,104.057156106572,
104.1554356643,104.253682243374,104.351925326412,104.453622515054,104.552006928473,
104.655360504727,104.758714080981,104.857312205985,104.955769988761,105.055992556534,
105.154272114262,105.252518693335,105.350761776374,105.452458965016,105.550843378435,
105.654196954689,105.757550530943,105.856140410614,105.898938865661),
 .UNSPECIFIED.);
#329=B_SPLINE_CURVE_WITH_KNOTS('',3,(#41495,#41496,#41497,#41498,#41499,
#41500,#41501,#41502,#41503,#41504,#41505,#41506,#41507,#41508,#41509,#41510,
#41511,#41512,#41513,#41514,#41515,#41516,#41517,#41518,#41519,#41520,#41521,
#41522,#41523,#41524,#41525,#41526,#41527,#41528,#41529,#41530,#41531,#41532,
#41533,#41534,#41535,#41536,#41537,#41538,#41539,#41540,#41541,#41542,#41543,
#41544,#41545,#41546,#41547,#41548,#41549,#41550,#41551,#41552,#41553,#41554,
#41555,#41556,#41557,#41558,#41559,#41560,#41561,#41562,#41563,#41564,#41565,
#41566,#41567),.UNSPECIFIED.,.F.,.F.,(4,3,3,3,3,3,3,3,3,3,3,3,3,3,3,3,3,
3,3,3,3,3,3,3,4),(103.672557568463,103.771601702603,103.870660322484,103.96976131202,
104.06899945985,104.168318657834,104.267812431338,104.293907348461,104.392505473465,
104.490963256241,104.591185824014,104.689465381742,104.787711960816,104.885955043854,
104.987652232496,105.086036645915,105.189390222169,105.292743798423,105.391329160737,
105.489781902021,105.591857047161,105.690131953935,105.788367309393,105.88660434371,
105.898082482581),.UNSPECIFIED.);
#330=B_SPLINE_CURVE_WITH_KNOTS('',3,(#41568,#41569,#41570,#41571,#41572,
#41573,#41574,#41575),.UNSPECIFIED.,.F.,.F.,(4,1,1,1,1,4),(99.6160278315589,
100.298561548614,101.297397998576,102.296234448537,103.295070898499,103.672550060583),
 .UNSPECIFIED.);
#331=B_SPLINE_CURVE_WITH_KNOTS('',3,(#41581,#41582,#41583,#41584,#41585,
#41586,#41587,#41588,#41589,#41590,#41591,#41592,#41593,#41594,#41595,#41596,
#41597,#41598,#41599,#41600,#41601,#41602,#41603,#41604,#41605,#41606,#41607,
#41608,#41609,#41610,#41611,#41612,#41613,#41614,#41615,#41616,#41617,#41618,
#41619,#41620,#41621,#41622,#41623,#41624,#41625,#41626,#41627,#41628,#41629,
#41630,#41631,#41632,#41633,#41634,#41635,#41636,#41637,#41638,#41639,#41640,
#41641,#41642,#41643,#41644,#41645,#41646,#41647,#41648,#41649,#41650,#41651,
#41652,#41653,#41654,#41655,#41656,#41657,#41658,#41659,#41660,#41661,#41662,
#41663,#41664,#41665,#41666,#41667,#41668,#41669,#41670,#41671,#41672,#41673,
#41674,#41675,#41676,#41677,#41678,#41679,#41680,#41681,#41682,#41683,#41684,
#41685,#41686,#41687,#41688,#41689,#41690,#41691,#41692,#41693,#41694,#41695,
#41696,#41697,#41698,#41699,#41700,#41701,#41702,#41703,#41704,#41705,#41706,
#41707),.UNSPECIFIED.,.F.,.F.,(4,3,3,3,3,3,3,3,3,3,3,3,3,3,3,3,3,3,3,3,
3,3,3,3,3,3,3,3,3,3,3,3,3,3,3,3,3,3,3,3,3,3,4),(93.3318433927562,93.430100475642,
93.5284654599662,93.6268914127951,93.7254797874492,93.7715131314001,93.8701112564037,
93.9685690391804,94.0687916069531,94.1670711646813,94.2653177437546,94.363560826793,
94.4652580154353,94.5636424288541,94.666996005108,94.770349581362,94.8689477063657,
94.9674054891424,95.067628056915,95.1659076146432,95.2641541937166,95.362397276755,
95.4640944653972,95.562478878816,95.6658324550699,95.7691860313238,95.8677841563276,
95.9662419391042,96.0664645068769,96.1647440646051,96.2629906436785,96.3612337267168,
96.462930915359,96.5613153287778,96.6646689050317,96.7680224812857,96.8674993725788,
96.9668292609828,97.0660403563902,97.1651524247997,97.2642075332236,97.3632407686268,
97.3893722612837),.UNSPECIFIED.);
#332=B_SPLINE_CURVE_WITH_KNOTS('',3,(#41708,#41709,#41710,#41711,#41712,
#41713),.UNSPECIFIED.,.F.,.F.,(4,1,1,4),(97.3893797691262,97.7668589312476,
98.7656953812095,99.6144331696528),.UNSPECIFIED.);
#333=B_SPLINE_CURVE_WITH_KNOTS('',3,(#41715,#41716,#41717,#41718,#41719,
#41720),.UNSPECIFIED.,.F.,.F.,(4,1,1,4),(97.3893809711856,98.3008886486899,
99.2997250986518,99.6160278315589),.UNSPECIFIED.);
#334=B_SPLINE_CURVE_WITH_KNOTS('',3,(#41721,#41722,#41723,#41724,#41725,
#41726,#41727,#41728,#41729,#41730,#41731,#41732,#41733,#41734,#41735,#41736,
#41737,#41738,#41739,#41740,#41741,#41742,#41743,#41744,#41745,#41746,#41747,
#41748,#41749,#41750,#41751,#41752,#41753,#41754,#41755,#41756,#41757,#41758,
#41759,#41760,#41761,#41762,#41763,#41764,#41765,#41766,#41767,#41768,#41769,
#41770,#41771,#41772,#41773,#41774,#41775,#41776,#41777,#41778,#41779,#41780,
#41781,#41782,#41783,#41784,#41785,#41786,#41787,#41788,#41789,#41790,#41791,
#41792,#41793,#41794,#41795,#41796,#41797,#41798,#41799,#41800,#41801,#41802,
#41803,#41804,#41805,#41806,#41807,#41808,#41809,#41810,#41811,#41812,#41813,
#41814,#41815,#41816,#41817,#41818,#41819,#41820,#41821,#41822,#41823,#41824,
#41825,#41826,#41827,#41828,#41829,#41830,#41831,#41832,#41833,#41834,#41835,
#41836,#41837,#41838,#41839,#41840,#41841,#41842,#41843,#41844),
 .UNSPECIFIED.,.F.,.F.,(4,3,3,3,3,3,3,3,3,3,3,3,3,3,3,3,3,3,3,3,3,3,3,3,
3,3,3,3,3,3,3,3,3,3,3,3,3,3,3,3,3,4),(93.3321732640166,93.4307320102719,
93.5291589015738,93.6274833306878,93.7257523216407,93.8239953843585,93.9222419960585,
94.020589057102,94.1189857985572,94.2175578401571,94.3055428488424,94.4041409738461,
94.5025987566228,94.6028213243955,94.7011008821237,94.7993474611971,94.8975905442356,
94.9992877328778,95.0976721462966,95.2010257225504,95.3043792988043,95.402977423808,
95.5014352065847,95.6016577743574,95.6999373320855,95.7981839111589,95.8964269941974,
95.9981241828395,96.0965085962583,96.1998621725122,96.3032157487661,96.4018138737698,
96.5002716565466,96.6004942243192,96.6987737820474,96.7970203611207,96.8952634441592,
96.9969606328014,97.0953450462201,97.1986986224741,97.302052198728,97.3893722612837),
 .UNSPECIFIED.);
#335=B_SPLINE_CURVE_WITH_KNOTS('',3,(#41850,#41851,#41852,#41853,#41854,
#41855,#41856,#41857),.UNSPECIFIED.,.F.,.F.,(4,1,1,1,1,4),(87.0497428708734,
87.7784944316288,88.7773308815907,89.7761673315526,90.7750037815145,91.1061798195662),
 .UNSPECIFIED.);
#336=B_SPLINE_CURVE_WITH_KNOTS('',3,(#41858,#41859,#41860,#41861,#41862,
#41863,#41864,#41865,#41866,#41867,#41868,#41869,#41870,#41871,#41872,#41873,
#41874,#41875,#41876,#41877,#41878,#41879,#41880,#41881,#41882,#41883,#41884,
#41885,#41886,#41887,#41888,#41889,#41890,#41891,#41892,#41893,#41894,#41895,
#41896,#41897,#41898,#41899,#41900,#41901,#41902,#41903,#41904,#41905,#41906,
#41907,#41908,#41909,#41910,#41911,#41912,#41913,#41914,#41915,#41916,#41917,
#41918,#41919,#41920,#41921,#41922,#41923,#41924,#41925,#41926,#41927),
 .UNSPECIFIED.,.F.,.F.,(4,3,3,3,3,3,3,3,3,3,3,3,3,3,3,3,3,3,3,3,3,3,3,4),
(91.1061869541041,91.2043419644769,91.3024795334305,91.4006291648839,91.4988897541855,
91.5972075103077,91.6957053368612,91.7738402314764,91.8724383564801,91.9708961392567,
92.0711187070294,92.1693982647575,92.2676448438309,92.3658879268695,92.4675851155117,
92.5659695289305,92.6693231051843,92.7726766814382,92.8712673172591,92.9697241251359,
93.0680663331458,93.1663410384504,93.2645927043531,93.3318433927562),
 .UNSPECIFIED.);
#337=B_SPLINE_CURVE_WITH_KNOTS('',3,(#41929,#41930,#41931,#41932,#41933,
#41934,#41935,#41936,#41937,#41938,#41939,#41940,#41941,#41942,#41943,#41944,
#41945,#41946,#41947,#41948,#41949,#41950,#41951,#41952,#41953,#41954,#41955,
#41956,#41957,#41958,#41959,#41960,#41961,#41962,#41963,#41964,#41965,#41966,
#41967,#41968,#41969,#41970,#41971,#41972,#41973,#41974,#41975,#41976,#41977,
#41978,#41979,#41980,#41981,#41982,#41983,#41984,#41985,#41986,#41987,#41988,
#41989,#41990,#41991,#41992,#41993,#41994,#41995,#41996,#41997,#41998),
 .UNSPECIFIED.,.F.,.F.,(4,3,3,3,3,3,3,3,3,3,3,3,3,3,3,3,3,3,3,3,3,3,3,4),
(91.1061869541041,91.2465035596787,91.3090334989568,91.4076316239605,91.5060894067373,
91.60631197451,91.7045915322382,91.8028381113116,91.9010811943501,92.0027783829923,
92.1011627964111,92.2045163726649,92.3078699489186,92.4064680739223,92.5049258566991,
92.6051484244717,92.7034279821999,92.8016745612733,92.8999176443118,93.0016148329539,
93.0999992463727,93.2033528226266,93.3067063988805,93.3321732640166),
 .UNSPECIFIED.);
#338=B_SPLINE_CURVE_WITH_KNOTS('',3,(#41999,#42000,#42001,#42002,#42003,
#42004,#42005,#42006,#42007,#42008,#42009,#42010,#42011,#42012,#42013,#42014,
#42015,#42016,#42017,#42018,#42019,#42020,#42021,#42022,#42023,#42024,#42025,
#42026,#42027,#42028,#42029,#42030,#42031,#42032,#42033,#42034,#42035,#42036,
#42037,#42038,#42039,#42040,#42041,#42042,#42043,#42044,#42045,#42046,#42047,
#42048,#42049,#42050,#42051,#42052,#42053,#42054,#42055,#42056,#42057,#42058,
#42059,#42060,#42061,#42062,#42063,#42064,#42065,#42066,#42067,#42068,#42069,
#42070,#42071,#42072,#42073,#42074,#42075,#42076,#42077,#42078,#42079,#42080,
#42081,#42082,#42083,#42084,#42085,#42086,#42087,#42088,#42089,#42090,#42091,
#42092,#42093,#42094,#42095,#42096,#42097,#42098,#42099,#42100,#42101,#42102,
#42103,#42104,#42105,#42106,#42107,#42108,#42109,#42110,#42111,#42112,#42113,
#42114,#42115,#42116,#42117,#42118,#42119,#42120,#42121,#42122,#42123,#42124,
#42125),.UNSPECIFIED.,.F.,.F.,(4,3,3,3,3,3,3,3,3,3,3,3,3,3,3,3,3,3,3,3,
3,3,3,3,3,3,3,3,3,3,3,3,3,3,3,3,3,3,3,3,3,3,4),(87.0482730079683,87.1466827716406,
87.245261692117,87.3136876991093,87.412285824113,87.5107436068897,87.6109661746624,
87.7092457323905,87.8074923114639,87.9057353945024,88.0074325831446,88.1058169965634,
88.2091705728173,88.3125241490712,88.4111222740749,88.5095800568516,88.6098026246243,
88.7080821823525,88.8063287614258,88.9045718444643,89.0062690331065,89.1046534465253,
89.2080070227792,89.311360599033,89.4099587240367,89.5084165068134,89.6086390745861,
89.7069186323142,89.8051652113876,89.9034082944261,90.0051054830683,90.1034898964871,
90.206843472741,90.3101970489949,90.409695787095,90.5067185530535,90.6036495481492,
90.70051989818,90.801936662084,90.8988156754799,90.9957205549589,91.0927209416414,
91.1061869537961),.UNSPECIFIED.);
#339=B_SPLINE_CURVE_WITH_KNOTS('',3,(#42131,#42132,#42133,#42134,#42135,
#42136,#42137,#42138,#42139,#42140,#42141,#42142,#42143,#42144,#42145,#42146,
#42147,#42148,#42149,#42150,#42151,#42152,#42153,#42154,#42155,#42156,#42157,
#42158,#42159,#42160,#42161,#42162,#42163,#42164,#42165,#42166,#42167,#42168,
#42169,#42170,#42171,#42172,#42173,#42174,#42175,#42176,#42177,#42178,#42179,
#42180,#42181,#42182,#42183,#42184,#42185,#42186,#42187,#42188,#42189,#42190,
#42191,#42192,#42193,#42194,#42195,#42196,#42197,#42198,#42199,#42200,#42201,
#42202,#42203,#42204,#42205,#42206,#42207,#42208,#42209,#42210,#42211,#42212,
#42213,#42214,#42215,#42216,#42217,#42218,#42219,#42220,#42221,#42222,#42223,
#42224,#42225,#42226,#42227,#42228,#42229,#42230,#42231,#42232,#42233,#42234,
#42235,#42236,#42237,#42238,#42239,#42240,#42241,#42242,#42243,#42244,#42245,
#42246,#42247,#42248,#42249,#42250,#42251,#42252,#42253,#42254,#42255,#42256,
#42257),.UNSPECIFIED.,.F.,.F.,(4,3,3,3,3,3,3,3,3,3,3,3,3,3,3,3,3,3,3,3,
3,3,3,3,3,3,3,3,3,3,3,3,3,3,3,3,3,3,3,3,3,3,4),(80.765532900003,80.7866392818957,
80.8852374068994,80.9836951896761,81.0839177574488,81.182197315177,81.2804438942504,
81.3786869772888,81.480384165931,81.5787685793498,81.6821221556037,81.7854757318576,
81.8840738568613,81.982531639638,82.0827542074107,82.1810337651389,82.2792803442123,
82.3775234272508,82.479220615893,82.5776050293118,82.6809586055656,82.7843121818195,
82.8829103068232,82.9813680895999,83.0815906573726,83.1798702151008,83.2781167941742,
83.3763598772127,83.4780570658548,83.5764414792737,83.6797950555275,83.7831486317814,
83.8817467567851,83.9802045395619,84.0804271073345,84.1787066650626,84.276953244136,
84.3751963271744,84.4768935158166,84.5752779292354,84.6786315054893,84.7819850817432,
84.8230016469246),.UNSPECIFIED.);
#340=B_SPLINE_CURVE_WITH_KNOTS('',3,(#42258,#42259,#42260,#42261,#42262,
#42263),.UNSPECIFIED.,.F.,.F.,(4,1,1,4),(84.8230070322059,85.7808215317051,
86.779657981667,87.0497428708734),.UNSPECIFIED.);
#341=B_SPLINE_CURVE_WITH_KNOTS('',3,(#42265,#42266,#42267,#42268,#42269,
#42270,#42271,#42272,#42273,#42274,#42275,#42276,#42277,#42278,#42279,#42280,
#42281,#42282,#42283,#42284,#42285,#42286,#42287,#42288,#42289,#42290,#42291,
#42292,#42293,#42294,#42295,#42296,#42297,#42298,#42299,#42300,#42301,#42302,
#42303,#42304,#42305,#42306,#42307,#42308,#42309,#42310,#42311,#42312,#42313,
#42314,#42315,#42316,#42317,#42318,#42319,#42320,#42321,#42322,#42323,#42324,
#42325,#42326,#42327,#42328,#42329,#42330,#42331,#42332,#42333,#42334),
 .UNSPECIFIED.,.F.,.F.,(4,3,3,3,3,3,3,3,3,3,3,3,3,3,3,3,3,3,3,3,3,3,3,4),
(84.8230016472006,84.9261861619504,85.0296647966981,85.1332945907093,85.2372126194225,
85.3160147991855,85.4146129241892,85.513070706966,85.6132932747387,85.7115728324668,
85.8098194115402,85.9080624945788,86.0097596832209,86.1081440966397,86.2114976728936,
86.3148512491474,86.4134243290432,86.5118681332339,86.6102123732759,86.7084866565573,
86.8067399239164,86.9049803913387,87.0032727094089,87.0482730079683),
 .UNSPECIFIED.);
#342=B_SPLINE_CURVE_WITH_KNOTS('',3,(#42335,#42336,#42337,#42338,#42339,
#42340,#42341,#42342,#42343,#42344,#42345,#42346,#42347,#42348,#42349,#42350,
#42351,#42352,#42353,#42354,#42355,#42356,#42357,#42358,#42359,#42360,#42361,
#42362,#42363,#42364,#42365,#42366,#42367,#42368,#42369,#42370,#42371,#42372,
#42373,#42374,#42375,#42376,#42377,#42378,#42379,#42380,#42381,#42382,#42383,
#42384,#42385,#42386,#42387,#42388,#42389,#42390,#42391,#42392,#42393,#42394,
#42395,#42396,#42397,#42398,#42399,#42400,#42401,#42402,#42403,#42404,#42405,
#42406,#42407,#42408,#42409,#42410,#42411,#42412,#42413,#42414,#42415,#42416,
#42417,#42418,#42419,#42420,#42421,#42422,#42423,#42424,#42425,#42426,#42427,
#42428,#42429,#42430,#42431,#42432,#42433,#42434,#42435,#42436,#42437,#42438,
#42439,#42440,#42441,#42442,#42443,#42444,#42445,#42446,#42447,#42448,#42449,
#42450,#42451,#42452,#42453,#42454,#42455,#42456,#42457,#42458),
 .UNSPECIFIED.,.F.,.F.,(4,3,3,3,3,3,3,3,3,3,3,3,3,3,3,3,3,3,3,3,3,3,3,3,
3,3,3,3,3,3,3,3,3,3,3,3,3,3,3,3,3,4),(80.7658264186968,80.8640675910953,
80.9623197955324,81.0606769545392,81.159090517415,81.2576715751211,81.320668999338,
81.4192671243417,81.5177249071185,81.6179474748912,81.7162270326194,81.8144736116928,
81.9127166947314,82.0144138833735,82.1127982967923,82.2161518730461,82.3195054492999,
82.4181035743036,82.5165613570806,82.6167839248532,82.7150634825814,82.8133100616548,
82.9115531446933,83.0132503333354,83.1116347467542,83.214988323008,83.3183418992618,
83.4169400242655,83.5153978070419,83.6156203748147,83.7138999325429,83.8121465116163,
83.9103895946547,84.012086783297,84.1104711967157,84.2138247729697,84.3171783492237,
84.4205578302507,84.5236543867489,84.6265834813182,84.7292989065995,84.8230016469246),
 .UNSPECIFIED.);
#343=B_SPLINE_CURVE_WITH_KNOTS('',3,(#42464,#42465,#42466,#42467,#42468,
#42469,#42470,#42471),.UNSPECIFIED.,.F.,.F.,(4,1,1,1,1,4),(74.4816440654595,
74.7936205821245,75.7924570320864,76.7912934820482,77.7901299320101,78.539816339745),
 .UNSPECIFIED.);
#344=B_SPLINE_CURVE_WITH_KNOTS('',3,(#42472,#42473,#42474,#42475,#42476,
#42477,#42478,#42479,#42480,#42481,#42482,#42483,#42484,#42485,#42486,#42487,
#42488,#42489,#42490,#42491,#42492,#42493,#42494,#42495,#42496,#42497,#42498,
#42499,#42500,#42501,#42502,#42503,#42504,#42505,#42506,#42507,#42508,#42509,
#42510,#42511,#42512,#42513,#42514,#42515,#42516,#42517,#42518,#42519,#42520,
#42521,#42522,#42523,#42524,#42525,#42526,#42527,#42528,#42529,#42530,#42531,
#42532,#42533,#42534,#42535,#42536,#42537,#42538),.UNSPECIFIED.,.F.,.F.,
(4,3,3,3,3,3,3,3,3,3,3,3,3,3,3,3,3,3,3,3,3,3,4),(78.5398164397795,78.6677108218205,
78.788966381972,78.8875645069757,78.9860222897525,79.0862448575251,79.1845244152533,
79.2827709943266,79.3810140773651,79.4827112660073,79.5810956794261,79.68444925568,
79.7878028319339,79.8864023576742,79.984861155696,80.0832042043576,80.1814836418369,
80.279728991266,80.377969735523,80.4762993937422,80.5746716764088,80.6732109326996,
80.765532900003),.UNSPECIFIED.);
#345=B_SPLINE_CURVE_WITH_KNOTS('',3,(#42540,#42541,#42542,#42543,#42544,
#42545,#42546,#42547,#42548,#42549,#42550,#42551,#42552,#42553,#42554,#42555,
#42556,#42557,#42558,#42559,#42560,#42561,#42562,#42563,#42564,#42565,#42566,
#42567,#42568,#42569,#42570,#42571,#42572,#42573,#42574,#42575,#42576,#42577,
#42578,#42579,#42580,#42581,#42582,#42583,#42584,#42585,#42586,#42587,#42588,
#42589,#42590,#42591,#42592,#42593,#42594,#42595,#42596,#42597,#42598,#42599,
#42600,#42601,#42602,#42603,#42604,#42605,#42606,#42607,#42608,#42609),
 .UNSPECIFIED.,.F.,.F.,(4,3,3,3,3,3,3,3,3,3,3,3,3,3,3,3,3,3,3,3,3,3,3,4),
(78.539816339745,78.6377138097037,78.7346673304385,78.8315786913981,78.9284788661295,
79.0271081744507,79.124135318513,79.2235657089636,79.3229960994143,79.421594224418,
79.5200520071949,79.6202745749676,79.7185541326957,79.8168007117691,79.9150437948077,
80.0167409834498,80.1151253968686,80.2184789731224,80.3218325493762,80.4204382921372,
80.5188792313278,80.6172249291511,80.7155010605475,80.7658264186968),
 .UNSPECIFIED.);
#346=B_SPLINE_CURVE_WITH_KNOTS('',3,(#42610,#42611,#42612,#42613,#42614,
#42615,#42616,#42617),.UNSPECIFIED.,.F.,.F.,(4,1,1,1,1,4),(74.4832629992058,
75.3276502995668,76.3264867495287,77.3253231994905,78.3241596494524,78.539816339745),
 .UNSPECIFIED.);
#347=B_SPLINE_CURVE_WITH_KNOTS('',3,(#42623,#42624,#42625,#42626,#42627,
#42628,#42629,#42630,#42631,#42632,#42633,#42634,#42635,#42636,#42637,#42638,
#42639,#42640,#42641,#42642,#42643,#42644,#42645,#42646,#42647,#42648,#42649,
#42650,#42651,#42652,#42653,#42654,#42655,#42656,#42657,#42658,#42659,#42660,
#42661,#42662,#42663,#42664,#42665,#42666,#42667,#42668,#42669,#42670,#42671,
#42672,#42673,#42674,#42675,#42676,#42677,#42678,#42679,#42680,#42681,#42682,
#42683,#42684,#42685,#42686,#42687,#42688,#42689,#42690,#42691,#42692,#42693,
#42694,#42695,#42696,#42697,#42698,#42699,#42700,#42701,#42702,#42703,#42704,
#42705,#42706,#42707,#42708,#42709,#42710,#42711,#42712,#42713,#42714,#42715,
#42716,#42717,#42718,#42719,#42720,#42721,#42722,#42723,#42724,#42725,#42726,
#42727,#42728,#42729,#42730,#42731,#42732,#42733,#42734,#42735,#42736,#42737,
#42738,#42739,#42740,#42741,#42742,#42743,#42744,#42745,#42746),
 .UNSPECIFIED.,.F.,.F.,(4,3,3,3,3,3,3,3,3,3,3,3,3,3,3,3,3,3,3,3,3,3,3,3,
3,3,3,3,3,3,3,3,3,3,3,3,3,3,3,3,3,4),(68.1995885313917,68.2978346979847,
68.3960780479348,68.4972090065394,68.5955944170121,68.6980981496826,68.8006018823532,
68.8992000073569,68.9976577901335,69.0978803579062,69.1961599156344,69.2944064947079,
69.3926495777463,69.4943467663885,69.5927311798074,69.6960847560612,69.7994383323151,
69.8980364573188,69.9964942400958,70.0967168078685,70.1949963655966,70.2932429446698,
70.3914860277081,70.4931832163503,70.5915676297689,70.694921206023,70.798274782277,
70.8968729072807,70.9953306900576,71.0955532578302,71.1938328155585,71.2920793946319,
71.3903224776702,71.4920196663123,71.5904040797312,71.6937576559851,71.7971112322389,
71.9028340905518,72.0081993817381,72.1133399321502,72.2181701837247,72.2566308185864),
 .UNSPECIFIED.);
#348=B_SPLINE_CURVE_WITH_KNOTS('',3,(#42747,#42748,#42749,#42750,#42751,
#42752),.UNSPECIFIED.,.F.,.F.,(4,1,1,4),(72.2566310325654,72.7959476822007,
73.7947841321626,74.4816440654595),.UNSPECIFIED.);
#349=B_SPLINE_CURVE_WITH_KNOTS('',3,(#42754,#42755,#42756,#42757,#42758,
#42759,#42760),.UNSPECIFIED.,.F.,.F.,(4,1,1,1,4),(72.2566310325654,72.3311409496812,
73.329977399643,74.3288138496049,74.4832629992058),.UNSPECIFIED.);
#350=B_SPLINE_CURVE_WITH_KNOTS('',3,(#42761,#42762,#42763,#42764,#42765,
#42766,#42767,#42768,#42769,#42770,#42771,#42772,#42773,#42774,#42775,#42776,
#42777,#42778,#42779,#42780,#42781,#42782,#42783,#42784,#42785,#42786,#42787,
#42788,#42789,#42790,#42791,#42792,#42793,#42794,#42795,#42796,#42797,#42798,
#42799,#42800,#42801,#42802,#42803,#42804,#42805,#42806,#42807,#42808,#42809,
#42810,#42811,#42812,#42813,#42814,#42815,#42816,#42817,#42818,#42819,#42820,
#42821,#42822,#42823,#42824,#42825,#42826,#42827,#42828,#42829,#42830,#42831,
#42832,#42833,#42834,#42835,#42836,#42837,#42838,#42839,#42840,#42841,#42842,
#42843,#42844,#42845,#42846,#42847,#42848,#42849,#42850,#42851,#42852,#42853,
#42854,#42855,#42856,#42857,#42858,#42859,#42860,#42861,#42862,#42863,#42864,
#42865,#42866,#42867,#42868,#42869,#42870,#42871,#42872,#42873,#42874,#42875,
#42876,#42877,#42878,#42879,#42880,#42881,#42882,#42883,#42884,#42885,#42886,
#42887),.UNSPECIFIED.,.F.,.F.,(4,3,3,3,3,3,3,3,3,3,3,3,3,3,3,3,3,3,3,3,
3,3,3,3,3,3,3,3,3,3,3,3,3,3,3,3,3,3,3,3,3,3,4),(68.1987514454805,68.2973434027703,
68.3357951498337,68.4343932748374,68.5328510576141,68.6330736253868,68.7313531831149,
68.8295997621883,68.9278428452268,69.029540033869,69.1279244472877,69.2312780235416,
69.3346315997955,69.4332297247992,69.531687507576,69.6319100753486,69.7301896330768,
69.8284362121502,69.9266792951887,70.0283764838309,70.1267608972497,70.2301144735035,
70.3334680497574,70.4320661747611,70.5305239575379,70.6307465253105,70.7290260830387,
70.8272726621121,70.9255157451506,71.0272129337928,71.1255973472116,71.2289509234654,
71.3323044997193,71.4298807240689,71.5273176349422,71.6246428433671,71.7219081150621,
71.8191441424517,71.9163815796696,72.0137087835221,72.1110862397607,72.2086145464313,
72.2566310325654),.UNSPECIFIED.);
#351=B_SPLINE_CURVE_WITH_KNOTS('',3,(#42893,#42894,#42895,#42896,#42897,
#42898,#42899,#42900),.UNSPECIFIED.,.F.,.F.,(4,1,1,1,1,4),(61.9167164283391,
62.807583182582,63.8064196325439,64.8052560825058,65.8040925324676,65.9734457253857),
 .UNSPECIFIED.);
#352=B_SPLINE_CURVE_WITH_KNOTS('',3,(#42901,#42902,#42903,#42904,#42905,
#42906,#42907,#42908,#42909,#42910,#42911,#42912,#42913,#42914,#42915,#42916,
#42917,#42918,#42919,#42920,#42921,#42922,#42923,#42924,#42925,#42926,#42927,
#42928,#42929,#42930,#42931,#42932,#42933,#42934,#42935,#42936,#42937,#42938,
#42939,#42940,#42941,#42942,#42943,#42944,#42945,#42946,#42947,#42948,#42949,
#42950,#42951,#42952,#42953,#42954,#42955,#42956,#42957,#42958,#42959,#42960,
#42961,#42962,#42963,#42964,#42965,#42966,#42967,#42968,#42969,#42970),
 .UNSPECIFIED.,.F.,.F.,(4,3,3,3,3,3,3,3,3,3,3,3,3,3,3,3,3,3,3,3,3,3,3,4),
(65.9734457253857,66.0704340596178,66.1673127975359,66.2641328887561,66.3609254267911,
66.4577214670339,66.5546134226803,66.6515579893417,66.7486626585401,66.8029289824295,
66.9015271074332,66.9999848902099,67.1002074579826,67.1984870157107,67.2967335947842,
67.3949766778227,67.4966738664649,67.5950582798837,67.6984118561376,67.8017654323914,
67.9012212071415,67.9996662250101,68.0996273782009,68.1995885313917),
 .UNSPECIFIED.);
#353=B_SPLINE_CURVE_WITH_KNOTS('',3,(#42972,#42973,#42974,#42975,#42976,
#42977,#42978,#42979,#42980,#42981,#42982,#42983,#42984,#42985,#42986,#42987,
#42988,#42989,#42990,#42991,#42992,#42993,#42994,#42995,#42996,#42997,#42998,
#42999,#43000,#43001,#43002,#43003,#43004,#43005,#43006,#43007,#43008,#43009,
#43010,#43011,#43012,#43013,#43014,#43015,#43016,#43017,#43018,#43019,#43020,
#43021,#43022,#43023,#43024,#43025,#43026,#43027,#43028,#43029,#43030,#43031,
#43032,#43033,#43034,#43035,#43036,#43037,#43038,#43039,#43040,#43041),
 .UNSPECIFIED.,.F.,.F.,(4,3,3,3,3,3,3,3,3,3,3,3,3,3,3,3,3,3,3,3,3,3,3,4),
(65.9734457256204,66.0848798050745,66.1968635637055,66.3094957826849,66.3381222499099,
66.4367203749136,66.5351781576904,66.635400725463,66.7336802831912,66.8319268622646,
66.9301699453032,67.0318671339454,67.1302515473641,67.233605123618,67.3369586998718,
67.4355663370644,67.5340045943515,67.6323466348136,67.7306220560149,67.8288603843833,
67.9271329658568,68.0254205103276,68.1238183934054,68.1987514454805),
 .UNSPECIFIED.);
#354=B_SPLINE_CURVE_WITH_KNOTS('',3,(#43042,#43043,#43044,#43045,#43046,
#43047,#43048,#43049,#43050,#43051,#43052,#43053,#43054,#43055,#43056,#43057,
#43058,#43059,#43060,#43061,#43062,#43063,#43064,#43065,#43066,#43067,#43068,
#43069,#43070,#43071,#43072,#43073,#43074,#43075,#43076,#43077,#43078,#43079,
#43080,#43081,#43082,#43083,#43084,#43085,#43086,#43087,#43088,#43089,#43090,
#43091,#43092,#43093,#43094,#43095,#43096,#43097,#43098,#43099,#43100,#43101,
#43102,#43103,#43104,#43105,#43106,#43107,#43108,#43109,#43110,#43111,#43112,
#43113,#43114,#43115,#43116,#43117,#43118,#43119,#43120,#43121,#43122,#43123,
#43124,#43125,#43126,#43127,#43128,#43129,#43130,#43131,#43132,#43133,#43134,
#43135,#43136,#43137,#43138,#43139,#43140,#43141,#43142,#43143,#43144,#43145,
#43146,#43147,#43148,#43149,#43150,#43151,#43152,#43153,#43154,#43155,#43156,
#43157,#43158,#43159,#43160,#43161,#43162,#43163,#43164,#43165,#43166,#43167,
#43168),.UNSPECIFIED.,.F.,.F.,(4,3,3,3,3,3,3,3,3,3,3,3,3,3,3,3,3,3,3,3,
3,3,3,3,3,3,3,3,3,3,3,3,3,3,3,3,3,3,3,3,3,3,4),(61.9158792055681,62.0141405477262,
62.1125119549867,62.2109477748074,62.3095423097633,62.3427764500624,62.4413745750661,
62.5398323578432,62.6400549256158,62.738334483344,62.8365810624174,62.9348241454559,
63.036521334098,63.1349057475168,63.2382593237706,63.3416129000243,63.440211025028,
63.538668807805,63.6388913755777,63.7371709333058,63.8354175123792,63.9336605954176,
64.0353577840597,64.1337421974785,64.2370957737324,64.3404493499862,64.4390474749899,
64.5375052577664,64.6377278255391,64.7360073832671,64.8342539623406,64.9324970453788,
65.0341942340211,65.1325786474398,65.2359322236939,65.339285799948,65.4384637976082,
65.5374980774499,65.6364173808601,65.7352455972602,65.8340208922134,65.9327849002204,
65.9734457253857),.UNSPECIFIED.);
#355=B_SPLINE_CURVE_WITH_KNOTS('',3,(#43174,#43175,#43176,#43177,#43178,
#43179,#43180,#43181,#43182,#43183,#43184,#43185,#43186,#43187,#43188,#43189,
#43190,#43191,#43192,#43193,#43194,#43195,#43196,#43197,#43198,#43199,#43200,
#43201,#43202,#43203,#43204,#43205,#43206,#43207,#43208,#43209,#43210,#43211,
#43212,#43213,#43214,#43215,#43216,#43217,#43218,#43219,#43220,#43221,#43222,
#43223,#43224,#43225,#43226,#43227,#43228,#43229,#43230,#43231,#43232,#43233,
#43234,#43235,#43236,#43237,#43238,#43239,#43240,#43241,#43242,#43243,#43244,
#43245,#43246,#43247,#43248,#43249,#43250,#43251,#43252,#43253,#43254,#43255,
#43256,#43257,#43258,#43259,#43260,#43261,#43262,#43263,#43264,#43265,#43266,
#43267,#43268,#43269,#43270,#43271,#43272,#43273,#43274,#43275,#43276,#43277,
#43278,#43279,#43280,#43281,#43282,#43283,#43284,#43285,#43286,#43287,#43288,
#43289,#43290,#43291,#43292,#43293,#43294,#43295,#43296,#43297),
 .UNSPECIFIED.,.F.,.F.,(4,3,3,3,3,3,3,3,3,3,3,3,3,3,3,3,3,3,3,3,3,3,3,3,
3,3,3,3,3,3,3,3,3,3,3,3,3,3,3,3,3,4),(55.6323251401271,55.7308982043818,
55.8157280328489,55.9143261578526,56.0127839406293,56.113006508402,56.2112860661302,
56.3095326452036,56.407775728242,56.5094729168842,56.607857330303,56.7112109065569,
56.8145644828108,56.9131626078145,57.0116203905912,57.1118429583639,57.210122516092,
57.3083690951654,57.4066121782039,57.5083093668461,57.6066937802649,57.7100473565187,
57.8134009327726,57.9119990577762,58.010456840553,58.1106794083257,58.2089589660538,
58.3072055451273,58.4054486281658,58.5071458168079,58.6055302302267,58.7088838064806,
58.8122373827345,58.9094791608007,59.0070768179764,59.1040671063403,59.2009981633324,
59.2979009849175,59.3959908432397,59.4929780422904,59.5916192302483,59.6902604182062),
 .UNSPECIFIED.);
#356=B_SPLINE_CURVE_WITH_KNOTS('',3,(#43298,#43299,#43300,#43301,#43302,
#43303,#43304),.UNSPECIFIED.,.F.,.F.,(4,1,1,1,4),(59.6902604182062,59.8110738326964,
60.8099102826583,61.8087467326201,61.9167164283391),.UNSPECIFIED.);
#357=B_SPLINE_CURVE_WITH_KNOTS('',3,(#43306,#43307,#43308,#43309,#43310,
#43311,#43312,#43313,#43314,#43315,#43316,#43317,#43318,#43319,#43320,#43321,
#43322,#43323,#43324,#43325,#43326,#43327,#43328,#43329,#43330,#43331,#43332,
#43333,#43334,#43335,#43336,#43337,#43338,#43339,#43340,#43341,#43342,#43343,
#43344,#43345,#43346,#43347,#43348,#43349,#43350,#43351,#43352,#43353,#43354,
#43355,#43356,#43357,#43358,#43359,#43360,#43361,#43362,#43363,#43364,#43365,
#43366,#43367,#43368,#43369,#43370,#43371,#43372,#43373,#43374,#43375),
 .UNSPECIFIED.,.F.,.F.,(4,3,3,3,3,3,3,3,3,3,3,3,3,3,3,3,3,3,3,3,3,3,3,4),
(59.6902604182062,59.788634173056,59.8869985815969,59.985382791999,60.0838846667639,
60.1824499292132,60.2811933482969,60.3451035501387,60.4437016751424,60.542159457919,
60.6423820256917,60.7406615834199,60.8389081624932,60.9371512455318,61.038848434174,
61.1372328475928,61.2405864238466,61.3439400001005,61.4425291322825,61.5409847704389,
61.6393272818855,61.7376024228604,61.8358589218425,61.9158792055681),
 .UNSPECIFIED.);
#358=B_SPLINE_CURVE_WITH_KNOTS('',3,(#43376,#43377,#43378,#43379,#43380,
#43381,#43382,#43383,#43384,#43385,#43386,#43387,#43388,#43389,#43390,#43391,
#43392,#43393,#43394,#43395,#43396,#43397,#43398,#43399,#43400,#43401,#43402,
#43403,#43404,#43405,#43406,#43407,#43408,#43409,#43410,#43411,#43412,#43413,
#43414,#43415,#43416,#43417,#43418,#43419,#43420,#43421,#43422,#43423,#43424,
#43425,#43426,#43427,#43428,#43429,#43430,#43431,#43432,#43433,#43434,#43435,
#43436,#43437,#43438,#43439,#43440,#43441,#43442,#43443,#43444,#43445,#43446,
#43447,#43448,#43449,#43450,#43451,#43452,#43453,#43454,#43455,#43456,#43457,
#43458,#43459,#43460,#43461,#43462,#43463,#43464,#43465,#43466,#43467,#43468,
#43469,#43470,#43471,#43472,#43473,#43474,#43475,#43476,#43477,#43478,#43479,
#43480,#43481,#43482,#43483,#43484,#43485,#43486,#43487,#43488,#43489,#43490,
#43491,#43492,#43493,#43494,#43495,#43496,#43497,#43498,#43499),
 .UNSPECIFIED.,.F.,.F.,(4,3,3,3,3,3,3,3,3,3,3,3,3,3,3,3,3,3,3,3,3,3,3,3,
3,3,3,3,3,3,3,3,3,3,3,3,3,3,3,3,3,4),(55.6334624860629,55.7317495305894,
55.8299991741444,55.9282409035089,56.0265041889799,56.124878435732,56.2233185460379,
56.3219158409609,56.3497577502912,56.4483558752949,56.5468136580715,56.6470362258442,
56.7453157835724,56.8435623626458,56.9418054456841,57.0435026343264,57.1418870477452,
57.2452406239991,57.348594200253,57.4471923252568,57.5456501080336,57.6458726758063,
57.7441522335344,57.8423988126078,57.9406418956465,58.0423390842886,58.1407234977073,
58.2440770739611,58.3474306502149,58.4460287752185,58.5444865579953,58.644709125768,
58.7429886834961,58.8412352625696,58.9394783456082,59.0411755342503,59.1395599476692,
59.242913523923,59.3462671001768,59.460882914029,59.5755716660042,59.6902604179793),
 .UNSPECIFIED.);
#359=B_SPLINE_CURVE_WITH_KNOTS('',3,(#43505,#43506,#43507,#43508,#43509,
#43510,#43511,#43512),.UNSPECIFIED.,.F.,.F.,(4,1,1,1,1,4),(49.3495871338273,
49.8227093330776,50.8215457830395,51.8203822330014,52.8192186829633,53.4070751110266),
 .UNSPECIFIED.);
#360=B_SPLINE_CURVE_WITH_KNOTS('',3,(#43513,#43514,#43515,#43516,#43517,
#43518,#43519,#43520,#43521,#43522,#43523,#43524,#43525,#43526,#43527,#43528,
#43529,#43530,#43531,#43532,#43533,#43534,#43535,#43536,#43537,#43538,#43539,
#43540,#43541,#43542,#43543,#43544,#43545,#43546,#43547,#43548,#43549,#43550,
#43551,#43552,#43553,#43554,#43555,#43556,#43557,#43558,#43559,#43560,#43561,
#43562,#43563,#43564,#43565,#43566,#43567,#43568,#43569,#43570,#43571,#43572,
#43573,#43574,#43575,#43576,#43577,#43578,#43579,#43580,#43581,#43582),
 .UNSPECIFIED.,.F.,.F.,(4,3,3,3,3,3,3,3,3,3,3,3,3,3,3,3,3,3,3,3,3,3,3,4),
(53.4070755243489,53.5149520672591,53.6231638610545,53.7318758460054,53.8180551329251,
53.9166532579288,54.0151110407055,54.1153336084782,54.2136131662063,54.3118597452797,
54.4101028283182,54.5118000169604,54.6101844303792,54.7135380066331,54.816891582887,
54.918820777542,55.0172568547355,55.1155965101018,55.2138693416066,55.3121048754619,
55.4103643168845,55.5086391296002,55.6069975818191,55.6323251401271),
 .UNSPECIFIED.);
#361=B_SPLINE_CURVE_WITH_KNOTS('',3,(#43584,#43585,#43586,#43587,#43588,
#43589,#43590,#43591,#43592,#43593,#43594,#43595,#43596,#43597,#43598,#43599,
#43600,#43601,#43602,#43603,#43604,#43605,#43606,#43607,#43608,#43609,#43610,
#43611,#43612,#43613,#43614,#43615,#43616,#43617,#43618,#43619,#43620,#43621,
#43622,#43623,#43624,#43625,#43626,#43627,#43628,#43629,#43630,#43631,#43632,
#43633,#43634,#43635,#43636,#43637,#43638,#43639,#43640,#43641,#43642,#43643,
#43644,#43645,#43646,#43647,#43648,#43649,#43650,#43651,#43652,#43653),
 .UNSPECIFIED.,.F.,.F.,(4,3,3,3,3,3,3,3,3,3,3,3,3,3,3,3,3,3,3,3,3,3,3,4),
(53.4070751110266,53.5048543854907,53.6024983707771,53.7000367768844,53.7975186210124,
53.8949743677961,53.9924344477706,54.0899931990357,54.1876041339867,54.2853815723762,
54.3520848503674,54.4506829753711,54.5491407581481,54.6493633259208,54.7476428836489,
54.8458894627223,54.9441325457608,55.0458297344029,55.1442141478218,55.2475677240755,
55.3509213003293,55.4495112354676,55.5479503969357,55.6334624860629),
 .UNSPECIFIED.);
#362=B_SPLINE_CURVE_WITH_KNOTS('',3,(#43654,#43655,#43656,#43657,#43658,
#43659,#43660,#43661,#43662),.UNSPECIFIED.,.F.,.F.,(4,1,1,1,1,1,4),(49.3496770552549,
49.3579026005581,50.3567390505199,51.3555755004818,52.3544119504437,53.3532484004055,
53.4070751110266),.UNSPECIFIED.);
#363=B_SPLINE_CURVE_WITH_KNOTS('',3,(#43668,#43669,#43670,#43671,#43672,
#43673,#43674,#43675,#43676,#43677,#43678,#43679,#43680,#43681,#43682,#43683,
#43684,#43685,#43686,#43687,#43688,#43689,#43690,#43691,#43692,#43693,#43694,
#43695,#43696,#43697,#43698,#43699,#43700,#43701,#43702,#43703,#43704,#43705,
#43706,#43707,#43708,#43709,#43710,#43711,#43712,#43713,#43714,#43715,#43716,
#43717,#43718,#43719,#43720,#43721,#43722,#43723,#43724,#43725,#43726,#43727,
#43728,#43729,#43730,#43731,#43732,#43733,#43734,#43735,#43736,#43737,#43738,
#43739,#43740,#43741,#43742,#43743,#43744,#43745,#43746,#43747,#43748,#43749,
#43750,#43751,#43752,#43753,#43754,#43755,#43756,#43757,#43758,#43759,#43760,
#43761,#43762,#43763,#43764,#43765,#43766,#43767,#43768,#43769,#43770,#43771,
#43772,#43773,#43774,#43775,#43776,#43777,#43778,#43779,#43780,#43781,#43782,
#43783,#43784,#43785,#43786,#43787,#43788,#43789,#43790,#43791),
 .UNSPECIFIED.,.F.,.F.,(4,3,3,3,3,3,3,3,3,3,3,3,3,3,3,3,3,3,3,3,3,3,3,3,
3,3,3,3,3,3,3,3,3,3,3,3,3,3,3,3,3,4),(43.0671357810666,43.1654506306177,
43.2637141941451,43.3619559753673,43.4602054490314,43.5585578906931,43.6569637353388,
43.7555405095206,43.8296906333064,43.9282887583114,44.0267465410894,44.1269691088618,
44.2252486665913,44.3234952456661,44.4217383287061,44.5234355173466,44.6218199307668,
44.7251735070176,44.8285270832683,44.9271252082716,45.0255829910481,45.1258055588208,
45.2240851165486,45.3223316956214,45.4205747786593,45.522271967302,45.6206563807203,
45.7240099569752,45.8273635332301,45.9259616582337,46.0244194410106,46.1246420087832,
46.2229215665112,46.3211681455844,46.4194112286228,46.5211084172651,46.6194928306838,
46.7228464069379,46.826199983192,46.9466622822371,47.0654828012668,47.1238896269795),
 .UNSPECIFIED.);
#364=B_SPLINE_CURVE_WITH_KNOTS('',3,(#43792,#43793,#43794,#43795,#43796,
#43797),.UNSPECIFIED.,.F.,.F.,(4,1,1,4),(47.123889803847,47.8250364331539,
48.8238728831158,49.3495871338273),.UNSPECIFIED.);
#365=B_SPLINE_CURVE_WITH_KNOTS('',3,(#43799,#43800,#43801,#43802,#43803,
#43804),.UNSPECIFIED.,.F.,.F.,(4,1,1,4),(47.1238901029355,47.3602297006343,
48.3590661505962,49.3496770552549),.UNSPECIFIED.);
#366=B_SPLINE_CURVE_WITH_KNOTS('',3,(#43805,#43806,#43807,#43808,#43809,
#43810,#43811,#43812,#43813,#43814,#43815,#43816,#43817,#43818,#43819,#43820,
#43821,#43822,#43823,#43824,#43825,#43826,#43827,#43828,#43829,#43830,#43831,
#43832,#43833,#43834,#43835,#43836,#43837,#43838,#43839,#43840,#43841,#43842,
#43843,#43844,#43845,#43846,#43847,#43848,#43849,#43850,#43851,#43852,#43853,
#43854,#43855,#43856,#43857,#43858,#43859,#43860,#43861,#43862,#43863,#43864,
#43865,#43866,#43867,#43868,#43869,#43870,#43871,#43872,#43873,#43874,#43875,
#43876,#43877,#43878,#43879,#43880,#43881,#43882,#43883,#43884,#43885,#43886,
#43887,#43888,#43889,#43890,#43891,#43892,#43893,#43894,#43895,#43896,#43897,
#43898,#43899,#43900,#43901,#43902,#43903,#43904,#43905,#43906,#43907,#43908,
#43909,#43910,#43911,#43912,#43913,#43914,#43915,#43916,#43917,#43918,#43919,
#43920,#43921,#43922,#43923,#43924,#43925,#43926,#43927,#43928),
 .UNSPECIFIED.,.F.,.F.,(4,3,3,3,3,3,3,3,3,3,3,3,3,3,3,3,3,3,3,3,3,3,3,3,
3,3,3,3,3,3,3,3,3,3,3,3,3,3,3,3,3,4),(43.0660207258246,43.1644088336187,
43.2646463672028,43.3648839007868,43.4634820258002,43.5619398085867,43.662162376357,
43.7604419340953,43.858688513179,43.9569315962276,44.0586287848579,44.157013198287,
44.2603667745178,44.3637203507487,44.4623184757497,44.5607762585238,44.6609988262972,
44.7592783840227,44.8575249630934,44.9557680461293,45.0574652347747,45.1558496481909,
45.2592032244508,45.3625568007106,45.4611549257133,45.5596127084888,45.6598352762618,
45.7581148339886,45.8563614130607,45.9546044960981,46.0563016847417,46.1546860981592,
46.2580396744158,46.3613932506724,46.4587199838046,46.5559210250952,46.6530274701205,
46.750070296518,46.8471124553622,46.9441490048065,47.0412721236584,47.123889803847),
 .UNSPECIFIED.);
#367=B_SPLINE_CURVE_WITH_KNOTS('',3,(#43934,#43935,#43936,#43937,#43938,
#43939,#43940,#43941,#43942,#43943,#43944,#43945,#43946,#43947,#43948,#43949,
#43950,#43951,#43952,#43953,#43954,#43955,#43956,#43957,#43958,#43959,#43960,
#43961,#43962,#43963,#43964,#43965,#43966,#43967,#43968,#43969,#43970,#43971,
#43972,#43973,#43974,#43975,#43976,#43977,#43978,#43979,#43980,#43981,#43982,
#43983,#43984,#43985,#43986,#43987,#43988,#43989,#43990,#43991,#43992,#43993,
#43994,#43995,#43996,#43997,#43998,#43999,#44000,#44001,#44002,#44003,#44004,
#44005,#44006,#44007,#44008,#44009,#44010,#44011,#44012,#44013,#44014,#44015,
#44016,#44017,#44018,#44019,#44020,#44021,#44022,#44023,#44024,#44025,#44026,
#44027,#44028,#44029,#44030,#44031,#44032,#44033,#44034,#44035,#44036,#44037,
#44038,#44039,#44040,#44041,#44042,#44043,#44044,#44045,#44046,#44047,#44048,
#44049,#44050,#44051,#44052,#44053,#44054,#44055,#44056,#44057,#44058,#44059,
#44060),.UNSPECIFIED.,.F.,.F.,(4,3,3,3,3,3,3,3,3,3,3,3,3,3,3,3,3,3,3,3,
3,3,3,3,3,3,3,3,3,3,3,3,3,3,3,3,3,3,3,3,3,3,4),(36.7830720682974,36.8378354835733,
36.9364336084869,37.0348913911719,37.1351139589673,37.2333935165998,37.3316400955765,
37.4298831785171,37.5315803672716,37.6299647805909,37.7333183570631,37.8366719335352,
37.9352700586074,38.0337278414536,38.1339504092091,38.2322299670085,38.3304765461538,
38.4287196292646,38.5304168178227,38.6288012313141,38.7321548074056,38.835508383497,
38.9341065084865,39.0325642912489,39.1327868590252,39.231066416739,39.3293129957981,
39.4275560788223,39.5292532674815,39.6276376808862,39.7309912571726,39.8343448334589,
39.9329429584521,40.0314007412181,40.1316233089935,40.2299028667105,40.3281494457725,
40.4263925287995,40.5280897174548,40.6264741308619,40.7298277071414,40.8331812834208,
40.8407044966674),.UNSPECIFIED.);
#368=B_SPLINE_CURVE_WITH_KNOTS('',3,(#44061,#44062,#44063,#44064,#44065,
#44066,#44067,#44068,#44069,#44070,#44071,#44072,#44073,#44074,#44075,#44076,
#44077,#44078,#44079,#44080,#44081,#44082,#44083,#44084,#44085,#44086,#44087,
#44088,#44089,#44090,#44091,#44092,#44093,#44094,#44095,#44096,#44097,#44098,
#44099,#44100,#44101,#44102,#44103,#44104,#44105,#44106,#44107,#44108,#44109,
#44110,#44111,#44112,#44113,#44114,#44115,#44116,#44117,#44118,#44119,#44120,
#44121,#44122,#44123,#44124,#44125,#44126,#44127,#44128,#44129,#44130),
 .UNSPECIFIED.,.F.,.F.,(4,3,3,3,3,3,3,3,3,3,3,3,3,3,3,3,3,3,3,3,3,3,3,4),
(40.8407044969197,40.9391705387198,41.037496428004,41.1368115911763,41.2349607512892,
41.3330774110127,41.4311912274061,41.5313978539002,41.6296531901072,41.7308354617449,
41.8320177333826,41.9306158583836,42.0290736411577,42.129296208931,42.2275757666565,
42.3258223457271,42.424065428763,42.5257626174084,42.6241470308245,42.7275006070845,
42.8308541833445,42.9294559188312,43.0279051778647,43.0671357810666),
 .UNSPECIFIED.);
#369=B_SPLINE_CURVE_WITH_KNOTS('',3,(#44132,#44133,#44134,#44135,#44136,
#44137,#44138,#44139,#44140,#44141,#44142,#44143,#44144,#44145,#44146,#44147,
#44148,#44149,#44150,#44151,#44152,#44153,#44154,#44155,#44156,#44157,#44158,
#44159,#44160,#44161,#44162,#44163,#44164,#44165,#44166,#44167,#44168,#44169,
#44170,#44171,#44172,#44173,#44174,#44175,#44176,#44177,#44178,#44179,#44180,
#44181,#44182,#44183,#44184,#44185,#44186,#44187,#44188,#44189,#44190,#44191,
#44192,#44193,#44194,#44195,#44196,#44197,#44198,#44199,#44200,#44201),
 .UNSPECIFIED.,.F.,.F.,(4,3,3,3,3,3,3,3,3,3,3,3,3,3,3,3,3,3,3,3,3,3,3,4),
(40.8407044966674,40.9425310419932,41.0487010317106,41.1508691915795,41.253165848555,
41.355678560324,41.3672110008631,41.4658091258526,41.564266908615,41.6644894763913,
41.7627690341051,41.8610156131641,41.9592586961882,42.0609558848474,42.1593402982522,
42.2626938745385,42.3660474508249,42.4646234053357,42.5630692109104,42.66141458321,
42.7625661188636,42.8608128813695,42.963416803597,43.0660207258246),
 .UNSPECIFIED.);
#370=B_SPLINE_CURVE_WITH_KNOTS('',3,(#44202,#44203,#44204,#44205,#44206,
#44207,#44208,#44209),.UNSPECIFIED.,.F.,.F.,(4,1,1,1,1,4),(36.7838197340187,
37.3718652010156,38.3707016509774,39.3695381009393,40.3683745509012,40.8407024149445),
 .UNSPECIFIED.);
#371=B_SPLINE_CURVE_WITH_KNOTS('',3,(#44215,#44216,#44217,#44218,#44219,
#44220,#44221,#44222,#44223,#44224,#44225,#44226,#44227,#44228,#44229,#44230,
#44231,#44232,#44233,#44234,#44235,#44236,#44237,#44238,#44239,#44240,#44241,
#44242,#44243,#44244,#44245,#44246,#44247,#44248,#44249,#44250,#44251,#44252,
#44253,#44254,#44255,#44256,#44257,#44258,#44259,#44260,#44261,#44262,#44263,
#44264,#44265,#44266,#44267,#44268,#44269,#44270,#44271,#44272,#44273,#44274,
#44275,#44276,#44277,#44278,#44279,#44280,#44281,#44282,#44283,#44284,#44285,
#44286,#44287,#44288,#44289,#44290,#44291,#44292,#44293,#44294,#44295,#44296,
#44297,#44298,#44299,#44300,#44301,#44302,#44303,#44304,#44305,#44306,#44307,
#44308,#44309,#44310,#44311,#44312,#44313,#44314,#44315,#44316,#44317,#44318,
#44319,#44320,#44321,#44322,#44323,#44324,#44325,#44326,#44327,#44328,#44329,
#44330,#44331,#44332,#44333,#44334,#44335,#44336,#44337,#44338,#44339,#44340,
#44341),.UNSPECIFIED.,.F.,.F.,(4,3,3,3,3,3,3,3,3,3,3,3,3,3,3,3,3,3,3,3,
3,3,3,3,3,3,3,3,3,3,3,3,3,3,3,3,3,3,3,3,3,3,4),(30.4997391559443,30.5981023811913,
30.6965255871619,30.7951122973755,30.844816783802,30.9434149029363,31.0418726797402,
31.1420952489931,31.2403748005387,31.3386213733643,31.436864450098,31.5385616460145,
31.6369460530501,31.740299643407,31.8436532337639,31.9422513619608,32.0407091479708,
32.1409317149402,32.2392112759763,32.3374578583783,32.4357009447618,32.5373981295028,
32.6357825462731,32.7391361149995,32.8424896837258,32.9410878085162,33.0395455910849,
33.1397681589102,33.238047716445,33.3362942953307,33.434537378188,33.536234567063,
33.6346189803178,33.7379725570028,33.8413261336877,33.9390973941519,34.0367388270572,
34.1342810926927,34.2317547370095,34.3292101035806,34.4266554953363,34.5241539309141,
34.5575191894878),.UNSPECIFIED.);
#372=B_SPLINE_CURVE_WITH_KNOTS('',3,(#44342,#44343,#44344,#44345,#44346,
#44347,#44348,#44349,#44350,#44351,#44352,#44353,#44354,#44355,#44356,#44357,
#44358,#44359,#44360,#44361,#44362,#44363,#44364,#44365,#44366,#44367,#44368,
#44369,#44370,#44371,#44372,#44373,#44374,#44375,#44376,#44377,#44378,#44379,
#44380,#44381,#44382,#44383,#44384,#44385,#44386,#44387,#44388,#44389,#44390,
#44391,#44392,#44393,#44394,#44395,#44396,#44397,#44398,#44399,#44400,#44401,
#44402,#44403,#44404,#44405,#44406,#44407,#44408,#44409,#44410,#44411),
 .UNSPECIFIED.,.F.,.F.,(4,3,3,3,3,3,3,3,3,3,3,3,3,3,3,3,3,3,3,3,3,3,3,4),
(34.5575191897594,34.6782345503758,34.8009387396348,34.8401625836495,34.9387607091264,
35.0372184923826,35.1374410600362,35.2357206182559,35.3339671978241,35.4322102813602,
35.533907469423,35.6322918833412,35.7356454584763,35.8389990336114,35.9376008413556,
36.0360613066117,36.1344037647116,36.2326817408492,36.3309247589469,36.4291623016086,
36.5274785676935,36.6258371035951,36.7243383499611,36.7830720682974),
 .UNSPECIFIED.);
#373=B_SPLINE_CURVE_WITH_KNOTS('',3,(#44413,#44414,#44415,#44416,#44417,
#44418),.UNSPECIFIED.,.F.,.F.,(4,1,1,4),(34.5575241470784,35.3741923010918,
36.3730287510537,36.7838197340187),.UNSPECIFIED.);
#374=B_SPLINE_CURVE_WITH_KNOTS('',3,(#44419,#44420,#44421,#44422,#44423,
#44424,#44425,#44426,#44427,#44428,#44429,#44430,#44431,#44432,#44433,#44434,
#44435,#44436,#44437,#44438,#44439,#44440,#44441,#44442,#44443,#44444,#44445,
#44446,#44447,#44448,#44449,#44450,#44451,#44452,#44453,#44454,#44455,#44456,
#44457,#44458,#44459,#44460,#44461,#44462,#44463,#44464,#44465,#44466,#44467,
#44468,#44469,#44470,#44471,#44472,#44473,#44474,#44475,#44476,#44477,#44478,
#44479,#44480,#44481,#44482,#44483,#44484,#44485,#44486,#44487,#44488,#44489,
#44490,#44491,#44492,#44493,#44494,#44495,#44496,#44497,#44498,#44499,#44500,
#44501,#44502,#44503,#44504,#44505,#44506,#44507,#44508,#44509,#44510,#44511,
#44512,#44513,#44514,#44515,#44516,#44517,#44518,#44519,#44520,#44521,#44522,
#44523,#44524,#44525,#44526,#44527,#44528,#44529,#44530,#44531,#44532,#44533,
#44534,#44535,#44536,#44537,#44538,#44539,#44540,#44541,#44542),
 .UNSPECIFIED.,.F.,.F.,(4,3,3,3,3,3,3,3,3,3,3,3,3,3,3,3,3,3,3,3,3,3,3,3,
3,3,3,3,3,3,3,3,3,3,3,3,3,3,3,3,3,4),(30.5006743924598,30.599105196373,
30.6974319920214,30.7957023408707,30.8939457544963,30.9921917108564,31.090537495827,
31.188932057399,31.2875029984644,31.3788465012443,31.4774446472446,31.5759024512624,
31.6761250137553,31.7744045931695,31.8726511940475,31.9708942989805,32.0725914620369,
32.1709758973509,32.2743294242786,32.3776829512062,32.4762810765961,32.5747388598255,
32.6749614274933,32.7732409858351,32.8714875655813,32.9697306493509,33.0714278373052,
33.1698122515946,33.2731658263813,33.3765194011681,33.4751175203003,33.5735752971024,
33.6737978663559,33.7720774178991,33.8703239907224,33.9685670674539,34.0702642633729,
34.1686486704062,34.272002260768,34.3753558511299,34.5238559809544,34.5575191894878),
 .UNSPECIFIED.);
#375=B_SPLINE_CURVE_WITH_KNOTS('',3,(#44548,#44549,#44550,#44551,#44552,
#44553,#44554,#44555),.UNSPECIFIED.,.F.,.F.,(4,1,1,1,1,4),(24.2176477571914,
24.8517980840308,25.8506345339927,26.8494709839545,27.8483074339164,28.2743284150372),
 .UNSPECIFIED.);
#376=B_SPLINE_CURVE_WITH_KNOTS('',3,(#44556,#44557,#44558,#44559,#44560,
#44561,#44562,#44563,#44564,#44565,#44566,#44567,#44568,#44569,#44570,#44571,
#44572,#44573,#44574,#44575,#44576,#44577,#44578,#44579,#44580,#44581,#44582,
#44583,#44584,#44585,#44586,#44587,#44588,#44589,#44590,#44591,#44592,#44593,
#44594,#44595,#44596,#44597,#44598,#44599,#44600,#44601,#44602,#44603,#44604,
#44605,#44606,#44607,#44608,#44609,#44610,#44611,#44612,#44613,#44614,#44615,
#44616,#44617,#44618,#44619,#44620,#44621,#44622,#44623,#44624,#44625),
 .UNSPECIFIED.,.F.,.F.,(4,3,3,3,3,3,3,3,3,3,3,3,3,3,3,3,3,3,3,3,3,3,3,4),
(28.2743338823082,28.3746245108422,28.4749734042942,28.5754886326583,28.6760922711292,
28.7769068634701,28.8471438838783,28.9457420298706,29.0441998338806,29.1444223963755,
29.2427019757815,29.3409485766512,29.439191681576,29.540888844642,29.6392732799477,
29.7426268068939,29.8459803338402,29.9445606477316,30.0430096057847,30.1413569295598,
30.2396381186694,30.3378792535517,30.4361386871511,30.4997391559443),
 .UNSPECIFIED.);
#377=B_SPLINE_CURVE_WITH_KNOTS('',3,(#44627,#44628,#44629,#44630,#44631,
#44632,#44633,#44634,#44635,#44636,#44637,#44638,#44639,#44640,#44641,#44642,
#44643,#44644,#44645,#44646,#44647,#44648,#44649,#44650,#44651,#44652,#44653,
#44654,#44655,#44656,#44657,#44658,#44659,#44660,#44661,#44662,#44663,#44664,
#44665,#44666,#44667,#44668,#44669,#44670,#44671,#44672,#44673,#44674,#44675,
#44676,#44677,#44678,#44679,#44680,#44681,#44682,#44683,#44684,#44685,#44686,
#44687,#44688,#44689,#44690,#44691,#44692,#44693,#44694,#44695,#44696),
 .UNSPECIFIED.,.F.,.F.,(4,3,3,3,3,3,3,3,3,3,3,3,3,3,3,3,3,3,3,3,3,3,3,4),
(28.2743338823082,28.3823371513587,28.4809354101241,28.5793933280734,28.6796158622293,
28.7778955576022,28.8761422749412,28.9743854966836,29.0760825228428,29.1744670746393,
29.27782033798,29.3811736013206,29.4797717427214,29.5782295425657,29.6784521061553,
29.7767316824828,29.8749782806886,29.9732213833693,30.0749185503476,30.1733029844888,
30.2766565178856,30.3800100512824,30.4786103666847,30.5006743924598),
 .UNSPECIFIED.);
#378=B_SPLINE_CURVE_WITH_KNOTS('',3,(#44697,#44698,#44699,#44700,#44701,
#44702,#44703,#44704,#44705,#44706,#44707,#44708,#44709,#44710,#44711,#44712,
#44713,#44714,#44715,#44716,#44717,#44718,#44719,#44720,#44721,#44722,#44723,
#44724,#44725,#44726,#44727,#44728,#44729,#44730,#44731,#44732,#44733,#44734,
#44735,#44736,#44737,#44738,#44739,#44740,#44741,#44742,#44743,#44744,#44745,
#44746,#44747,#44748,#44749,#44750,#44751,#44752,#44753,#44754,#44755,#44756,
#44757,#44758,#44759,#44760,#44761,#44762,#44763,#44764,#44765,#44766,#44767,
#44768,#44769,#44770,#44771,#44772,#44773,#44774,#44775,#44776,#44777,#44778,
#44779,#44780,#44781,#44782,#44783,#44784,#44785,#44786,#44787,#44788,#44789,
#44790,#44791,#44792,#44793,#44794,#44795,#44796,#44797,#44798,#44799,#44800,
#44801,#44802,#44803,#44804,#44805,#44806,#44807,#44808,#44809,#44810,#44811,
#44812,#44813,#44814,#44815,#44816,#44817,#44818,#44819,#44820,#44821,#44822,
#44823),.UNSPECIFIED.,.F.,.F.,(4,3,3,3,3,3,3,3,3,3,3,3,3,3,3,3,3,3,3,3,
3,3,3,3,3,3,3,3,3,3,3,3,3,3,3,3,3,3,3,3,3,3,4),(24.2164090613759,24.3149891086871,
24.3869913515112,24.4855869791747,24.584042226434,24.6842654233139,24.7825423701227,
24.8807863158074,24.979026746417,25.080727010181,25.1791087505826,25.2824682760278,
25.3858278014731,25.4844267455965,25.5828853549539,25.683107717014,25.7813881135488,
25.8796355341479,25.9778794603151,26.079575658095,26.1779609099881,26.2813125807115,
26.3846642514349,26.4832625888546,26.5817205901414,26.6819431040484,26.7802228937311,
26.8784697092845,26.9767130330315,27.0784099501228,27.1767946124098,27.2801476569033,
27.3835007013968,27.4808124354761,27.5800026163015,27.6770619119092,27.7740624145151,
27.8710350582304,27.9718597641926,28.0689211628773,28.1660361043295,28.2632831523914,
28.2743338820794),.UNSPECIFIED.);
#379=B_SPLINE_CURVE_WITH_KNOTS('',3,(#44829,#44830,#44831,#44832,#44833,
#44834),.UNSPECIFIED.,.F.,.F.,(4,1,1,4),(15.707963267949,16.3962997518162,
17.3951362017781,17.9335272866486),.UNSPECIFIED.);
#380=B_SPLINE_CURVE_WITH_KNOTS('',3,(#44836,#44837,#44838,#44839,#44840),
 .UNSPECIFIED.,.F.,.F.,(4,1,4),(14.3986268518925,15.3974633018543,15.707963267949),
 .UNSPECIFIED.);
#381=B_SPLINE_CURVE_WITH_KNOTS('',3,(#44844,#44845,#44846,#44847,#44848,
#44849,#44850,#44851,#44852,#44853,#44854,#44855,#44856,#44857,#44858,#44859,
#44860,#44861,#44862,#44863,#44864,#44865,#44866,#44867,#44868,#44869,#44870,
#44871,#44872,#44873,#44874,#44875,#44876,#44877,#44878,#44879,#44880,#44881,
#44882,#44883,#44884,#44885,#44886,#44887,#44888,#44889,#44890,#44891,#44892,
#44893,#44894,#44895,#44896,#44897,#44898,#44899,#44900,#44901),
 .UNSPECIFIED.,.F.,.F.,(4,3,3,3,3,3,3,3,3,3,3,3,3,3,3,3,3,3,3,4),(13.8757070305574,
13.9742332816752,14.0726192270832,14.1714710217493,14.269679438043,14.3678547454402,
14.4660265209369,14.5653782868057,14.6636879754741,14.7635607799431,14.8634335844121,
14.9606976685948,15.0578044132827,15.154822913635,15.2517842191042,15.3487193065272,
15.4457083690103,15.5427241666821,15.6398692546785,15.707963267949),
 .UNSPECIFIED.);
#382=B_SPLINE_CURVE_WITH_KNOTS('',3,(#44902,#44903,#44904,#44905,#44906,
#44907,#44908),.UNSPECIFIED.,.F.,.F.,(4,1,1,1,4),(15.707963267949,15.8622700343739,
16.8611064843358,17.8599429342977,17.9342415312022),.UNSPECIFIED.);
#383=B_SPLINE_CURVE_WITH_KNOTS('',3,(#44914,#44915,#44916,#44917,#44918,
#44919,#44920,#44921),.UNSPECIFIED.,.F.,.F.,(4,1,1,1,1,4),(181.295997131773,
181.669120728045,182.667957178007,183.666793627969,184.665630077931,185.353966561798),
 .UNSPECIFIED.);
#384=B_SPLINE_CURVE_WITH_KNOTS('',3,(#44923,#44924,#44925,#44926,#44927),
 .UNSPECIFIED.,.F.,.F.,(4,1,4),(185.353966561798,185.664466527893,186.663302977854),
 .UNSPECIFIED.);
#385=B_SPLINE_CURVE_WITH_KNOTS('',3,(#44931,#44932,#44933,#44934,#44935,
#44936,#44937,#44938,#44939,#44940,#44941,#44942,#44943,#44944,#44945,#44946,
#44947,#44948,#44949,#44950,#44951,#44952,#44953,#44954,#44955,#44956,#44957,
#44958,#44959,#44960,#44961,#44962,#44963,#44964,#44965,#44966,#44967,#44968,
#44969,#44970,#44971,#44972,#44973,#44974,#44975,#44976,#44977,#44978,#44979,
#44980,#44981,#44982,#44983,#44984,#44985,#44986,#44987,#44988),
 .UNSPECIFIED.,.F.,.F.,(4,3,3,3,3,3,3,3,3,3,3,3,3,3,3,3,3,3,3,4),(185.353966561798,
185.451129857085,185.548173537216,185.645152134409,185.742096640885,185.839038003917,
185.936068669915,186.033145886238,186.130383559937,186.198496245335,186.297011706217,
186.395389165318,186.494243369552,186.592448960961,186.690623574174,186.788796784698,
186.888153288321,186.986469626041,187.086346212615,187.186222799188),
 .UNSPECIFIED.);
#386=B_SPLINE_CURVE_WITH_KNOTS('',3,(#44989,#44990,#44991,#44992,#44993,
#44994,#44995,#44996),.UNSPECIFIED.,.F.,.F.,(4,1,1,1,1,4),(181.297167551772,
182.203150445487,183.201986895449,184.200823345411,185.199659795373,185.353966561798),
 .UNSPECIFIED.);
#387=B_SPLINE_CURVE_WITH_KNOTS('',3,(#45002,#45003,#45004,#45005,#45006,
#45007,#45008,#45009,#45010,#45011,#45012,#45013,#45014,#45015,#45016,#45017,
#45018,#45019,#45020,#45021,#45022,#45023,#45024,#45025,#45026,#45027,#45028,
#45029,#45030,#45031,#45032,#45033,#45034,#45035,#45036,#45037,#45038,#45039,
#45040,#45041,#45042,#45043,#45044,#45045,#45046,#45047,#45048,#45049,#45050,
#45051,#45052,#45053,#45054,#45055,#45056,#45057,#45058,#45059,#45060,#45061,
#45062,#45063,#45064,#45065,#45066,#45067,#45068,#45069,#45070,#45071,#45072,
#45073,#45074,#45075,#45076,#45077,#45078,#45079,#45080,#45081,#45082,#45083,
#45084,#45085,#45086,#45087,#45088,#45089,#45090,#45091,#45092,#45093,#45094,
#45095,#45096,#45097,#45098,#45099,#45100,#45101,#45102,#45103,#45104,#45105,
#45106,#45107,#45108,#45109,#45110,#45111,#45112,#45113,#45114,#45115,#45116,
#45117,#45118,#45119,#45120,#45121,#45122,#45123,#45124,#45125),
 .UNSPECIFIED.,.F.,.F.,(4,3,3,3,3,3,3,3,3,3,3,3,3,3,3,3,3,3,3,3,3,3,3,3,
3,3,3,3,3,3,3,3,3,3,3,3,3,3,3,3,3,4),(175.013888659091,175.112152319873,
175.210394806678,175.308645592818,175.406999705352,175.505407764375,175.603986111103,
175.676102028274,175.774697486027,175.873152598412,175.97337583339,176.071652732112,
176.169896662128,176.268137109468,176.36983745166,176.468219289246,176.571578883741,
176.674938478236,176.773539092151,176.87199934821,176.972221295708,177.070503271274,
177.16875224246,177.266997688919,177.368691998738,177.467078680763,177.570426804481,
177.673774928198,177.772377764237,177.87084030234,177.971061686818,178.069346073265,
178.167597497762,178.265845436446,178.367536921874,178.465926166337,178.569268772248,
178.672611378159,178.782250112465,178.89154546425,179.000249342496,179.070781030154),
 .UNSPECIFIED.);
#388=B_SPLINE_CURVE_WITH_KNOTS('',3,(#45126,#45127,#45128,#45129,#45130,
#45131),.UNSPECIFIED.,.F.,.F.,(4,1,1,4),(179.070781254618,179.671447828121,
180.670284278083,181.295997131773),.UNSPECIFIED.);
#389=B_SPLINE_CURVE_WITH_KNOTS('',3,(#45133,#45134,#45135,#45136,#45137,
#45138,#45139),.UNSPECIFIED.,.F.,.F.,(4,1,1,1,4),(179.070781254618,179.206641095602,
180.205477545564,181.204313995525,181.297167551772),.UNSPECIFIED.);
#390=B_SPLINE_CURVE_WITH_KNOTS('',3,(#45140,#45141,#45142,#45143,#45144,
#45145,#45146,#45147),.UNSPECIFIED.,.F.,.F.,(4,1,1,1,1,4),(175.012544819822,
175.211295295754,176.210131745716,177.208968195678,178.20780464564,179.070781254618),
 .UNSPECIFIED.);
#391=B_SPLINE_CURVE_WITH_KNOTS('',3,(#45153,#45154,#45155,#45156,#45157,
#45158,#45159,#45160,#45161,#45162,#45163,#45164,#45165,#45166,#45167,#45168,
#45169,#45170,#45171,#45172,#45173,#45174,#45175,#45176,#45177,#45178,#45179,
#45180,#45181,#45182,#45183,#45184,#45185,#45186,#45187,#45188,#45189,#45190,
#45191,#45192,#45193,#45194,#45195,#45196,#45197,#45198,#45199,#45200,#45201,
#45202,#45203,#45204,#45205,#45206,#45207,#45208,#45209,#45210,#45211,#45212,
#45213,#45214,#45215,#45216,#45217,#45218,#45219,#45220,#45221,#45222,#45223,
#45224,#45225,#45226,#45227,#45228,#45229,#45230,#45231,#45232,#45233,#45234,
#45235,#45236,#45237,#45238,#45239,#45240,#45241,#45242,#45243,#45244,#45245,
#45246,#45247,#45248,#45249,#45250,#45251,#45252,#45253,#45254,#45255,#45256,
#45257,#45258,#45259,#45260,#45261,#45262,#45263,#45264,#45265,#45266,#45267,
#45268,#45269,#45270,#45271,#45272,#45273,#45274,#45275,#45276),
 .UNSPECIFIED.,.F.,.F.,(4,3,3,3,3,3,3,3,3,3,3,3,3,3,3,3,3,3,3,3,3,3,3,3,
3,3,3,3,3,3,3,3,3,3,3,3,3,3,3,3,3,4),(168.730499547626,168.829027790516,
168.927431100484,169.0257414087,169.124002503139,169.22224388459,169.320495026735,
169.41885037157,169.517260977773,169.615840376683,169.683083328503,169.781681404545,
169.880139138367,169.980361718379,170.078641227516,170.176887758238,170.275130793226,
170.376828039535,170.475212406137,170.578566092301,170.681919778464,170.780517924865,
170.87897572865,170.979198291122,171.077477868766,171.175724467309,171.273967569347,
171.375664734117,171.474049165186,171.577402696806,171.680756228426,171.779354490543,
171.877812411222,171.978034944618,172.076314641176,172.174561359122,172.272804580894,
172.374501605268,172.472886155656,172.576239417022,172.679592678388,172.787595947439),
 .UNSPECIFIED.);
#392=B_SPLINE_CURVE_WITH_KNOTS('',3,(#45277,#45278,#45279,#45280,#45281,
#45282,#45283,#45284,#45285,#45286,#45287,#45288,#45289,#45290,#45291,#45292,
#45293,#45294,#45295,#45296,#45297,#45298,#45299,#45300,#45301,#45302,#45303,
#45304,#45305,#45306,#45307,#45308,#45309,#45310,#45311,#45312,#45313,#45314,
#45315,#45316,#45317,#45318,#45319,#45320,#45321,#45322,#45323,#45324,#45325,
#45326,#45327,#45328,#45329,#45330,#45331,#45332,#45333,#45334,#45335,#45336,
#45337,#45338,#45339,#45340,#45341,#45342,#45343,#45344,#45345,#45346,#45347,
#45348,#45349),.UNSPECIFIED.,.F.,.F.,(4,3,3,3,3,3,3,3,3,3,3,3,3,3,3,3,3,
3,3,3,3,3,3,3,4),(172.787595947668,172.884841558621,172.984040004837,173.081071837019,
173.17805926857,173.275033212353,173.375882191352,173.472980624861,173.57014496835,
173.667458405729,173.67842912835,173.777027506528,173.875485539969,173.975708044762,
174.07398784529,174.172234663731,174.270477982414,174.372174881389,174.470559518877,
174.573912548594,174.677265578312,174.775844828369,174.874301068148,174.972645514908,
175.013888659091),.UNSPECIFIED.);
#393=B_SPLINE_CURVE_WITH_KNOTS('',3,(#45351,#45352,#45353,#45354,#45355,
#45356),.UNSPECIFIED.,.F.,.F.,(4,1,1,4),(172.787601414666,173.21362239583,
174.212458845792,175.012544819822),.UNSPECIFIED.);
#394=B_SPLINE_CURVE_WITH_KNOTS('',3,(#45357,#45358,#45359,#45360,#45361,
#45362,#45363,#45364,#45365,#45366,#45367,#45368,#45369,#45370,#45371,#45372,
#45373,#45374,#45375,#45376,#45377,#45378,#45379,#45380,#45381,#45382,#45383,
#45384,#45385,#45386,#45387,#45388,#45389,#45390,#45391,#45392,#45393,#45394,
#45395,#45396,#45397,#45398,#45399,#45400,#45401,#45402,#45403,#45404,#45405,
#45406,#45407,#45408,#45409,#45410,#45411,#45412,#45413,#45414,#45415,#45416,
#45417,#45418,#45419,#45420,#45421,#45422,#45423,#45424,#45425,#45426,#45427,
#45428,#45429,#45430,#45431,#45432,#45433,#45434,#45435,#45436,#45437,#45438,
#45439,#45440,#45441,#45442,#45443,#45444,#45445,#45446,#45447,#45448,#45449,
#45450,#45451,#45452,#45453,#45454,#45455,#45456,#45457,#45458,#45459,#45460,
#45461,#45462,#45463,#45464,#45465,#45466,#45467,#45468,#45469,#45470,#45471,
#45472,#45473,#45474,#45475,#45476,#45477,#45478,#45479,#45480),
 .UNSPECIFIED.,.F.,.F.,(4,3,3,3,3,3,3,3,3,3,3,3,3,3,3,3,3,3,3,3,3,3,3,3,
3,3,3,3,3,3,3,3,3,3,3,3,3,3,3,3,3,4),(168.730215099249,168.828460566731,
168.926805274994,169.025197908315,169.123767944869,169.218276595983,169.31687471461,
169.415332491016,169.515555060382,169.613834611798,169.712081184595,169.8103242614,
169.912021457536,170.010405864893,170.113759455419,170.217113045945,170.315711171923,
170.414168955616,170.514391523152,170.612671081649,170.710917661434,170.809160745127,
170.910857932822,171.009242346749,171.112595921328,171.215949495907,171.314547642559,
171.413005447084,171.513228009432,171.611507588998,171.709754189896,171.807997294716,
171.909694457505,172.008078892377,172.111432419123,172.214785945869,172.31561776535,
172.416285943722,172.516781875652,172.617176498936,172.717484580452,172.787595947439),
 .UNSPECIFIED.);
#395=B_SPLINE_CURVE_WITH_KNOTS('',3,(#45486,#45487,#45488,#45489,#45490,
#45491,#45492,#45493),.UNSPECIFIED.,.F.,.F.,(4,1,1,1,1,4),(162.44614673284,
162.691228178769,163.690064628731,164.688901078693,165.687737528655,166.504405683219),
 .UNSPECIFIED.);
#396=B_SPLINE_CURVE_WITH_KNOTS('',3,(#45494,#45495,#45496,#45497,#45498,
#45499,#45500,#45501,#45502,#45503,#45504,#45505,#45506,#45507,#45508,#45509,
#45510,#45511,#45512,#45513,#45514,#45515,#45516,#45517,#45518,#45519,#45520,
#45521,#45522,#45523,#45524,#45525,#45526,#45527,#45528,#45529,#45530,#45531,
#45532,#45533,#45534,#45535,#45536,#45537,#45538,#45539,#45540,#45541,#45542,
#45543,#45544,#45545,#45546,#45547,#45548,#45549,#45550,#45551,#45552,#45553,
#45554,#45555,#45556,#45557,#45558,#45559,#45560,#45561,#45562,#45563),
 .UNSPECIFIED.,.F.,.F.,(4,3,3,3,3,3,3,3,3,3,3,3,3,3,3,3,3,3,3,3,3,3,3,4),
(166.504410640259,166.652910770224,166.686573978617,166.785172097217,166.883629873595,
166.983852442968,167.082131994357,167.180378567127,167.278621643905,167.380318840074,
167.478703247404,167.582056837991,167.685410428579,167.784008554554,167.882466338243,
167.98268890578,168.080968464273,168.179215044053,168.277458127742,168.379155315442,
168.477539729364,168.580893303952,168.684246878541,168.730499547626),
 .UNSPECIFIED.);
#397=B_SPLINE_CURVE_WITH_KNOTS('',3,(#45565,#45566,#45567,#45568,#45569,
#45570,#45571,#45572,#45573,#45574,#45575,#45576,#45577,#45578,#45579,#45580,
#45581,#45582,#45583,#45584,#45585,#45586,#45587,#45588,#45589,#45590,#45591,
#45592,#45593,#45594,#45595,#45596,#45597,#45598,#45599,#45600,#45601,#45602,
#45603,#45604,#45605,#45606,#45607,#45608,#45609,#45610,#45611,#45612,#45613,
#45614,#45615,#45616,#45617,#45618,#45619,#45620,#45621,#45622,#45623,#45624,
#45625,#45626,#45627,#45628,#45629,#45630,#45631,#45632,#45633,#45634,#45635,
#45636,#45637),.UNSPECIFIED.,.F.,.F.,(4,3,3,3,3,3,3,3,3,3,3,3,3,3,3,3,3,
3,3,3,3,3,3,3,4),(166.504410640259,166.6019131263,166.699371433809,166.796815990361,
166.894277201725,166.991846173229,167.089478292238,167.18726953544,167.220603696059,
167.319201820915,167.417659603535,167.517882171346,167.616161728898,167.714408307788,
167.812651390637,167.914348579483,168.012732992698,168.11608656936,168.219440146021,
168.318036793093,168.421081369632,168.519419920937,168.617691701668,168.715928374066,
168.730215099249),.UNSPECIFIED.);
#398=B_SPLINE_CURVE_WITH_KNOTS('',3,(#45638,#45639,#45640,#45641,#45642,
#45643,#45644,#45645,#45646,#45647,#45648,#45649,#45650,#45651,#45652,#45653,
#45654,#45655,#45656,#45657,#45658,#45659,#45660,#45661,#45662,#45663,#45664,
#45665,#45666,#45667,#45668,#45669,#45670,#45671,#45672,#45673,#45674,#45675,
#45676,#45677,#45678,#45679,#45680,#45681,#45682,#45683,#45684,#45685,#45686,
#45687,#45688,#45689,#45690,#45691,#45692,#45693,#45694,#45695,#45696,#45697,
#45698,#45699,#45700,#45701,#45702,#45703,#45704,#45705,#45706,#45707,#45708,
#45709,#45710,#45711,#45712,#45713,#45714,#45715,#45716,#45717,#45718,#45719,
#45720,#45721,#45722,#45723,#45724,#45725,#45726,#45727,#45728,#45729,#45730,
#45731,#45732,#45733,#45734,#45735,#45736,#45737,#45738,#45739,#45740,#45741,
#45742,#45743,#45744,#45745,#45746,#45747,#45748,#45749,#45750,#45751,#45752,
#45753,#45754,#45755,#45756,#45757,#45758,#45759,#45760,#45761),
 .UNSPECIFIED.,.F.,.F.,(4,3,3,3,3,3,3,3,3,3,3,3,3,3,3,3,3,3,3,3,3,3,3,3,
3,3,3,3,3,3,3,3,3,3,3,3,3,3,3,3,3,4),(162.4476622356,162.545987531945,162.644257026285,
162.742500229115,162.840746617893,162.939093232495,163.037489201385,163.136060859114,
163.225257896212,163.323856021116,163.422313803793,163.522536371591,163.620815929221,
163.719062508197,163.817305591139,163.919002779898,164.017387193223,164.120740769699,
164.224094346174,164.322692471118,164.421150253833,164.521372821621,164.619652379285,
164.717898958294,164.816142041267,164.917839229984,165.016223643337,165.119577219736,
165.222930796135,165.321528921634,165.419986704907,165.520209272556,165.618488830781,
165.71673541035,165.814978493883,165.916675681936,166.01506009584,166.118413670969,
166.221767246097,166.344599874419,166.465474953174,166.504410639987),
 .UNSPECIFIED.);
#399=B_SPLINE_CURVE_WITH_KNOTS('',3,(#45767,#45768,#45769,#45770,#45771,
#45772,#45773,#45774,#45775,#45776,#45777,#45778,#45779,#45780,#45781,#45782,
#45783,#45784,#45785,#45786,#45787,#45788,#45789,#45790,#45791,#45792,#45793,
#45794,#45795,#45796,#45797,#45798,#45799,#45800,#45801,#45802,#45803,#45804,
#45805,#45806,#45807,#45808,#45809,#45810,#45811,#45812,#45813,#45814,#45815,
#45816,#45817,#45818,#45819,#45820,#45821,#45822,#45823,#45824,#45825,#45826,
#45827,#45828,#45829,#45830,#45831,#45832,#45833,#45834,#45835,#45836,#45837,
#45838,#45839,#45840,#45841,#45842,#45843,#45844,#45845,#45846,#45847,#45848,
#45849,#45850,#45851,#45852,#45853,#45854,#45855,#45856,#45857,#45858,#45859,
#45860,#45861,#45862,#45863,#45864,#45865,#45866,#45867,#45868,#45869,#45870,
#45871,#45872,#45873,#45874,#45875,#45876,#45877,#45878,#45879,#45880,#45881,
#45882,#45883,#45884,#45885,#45886,#45887,#45888,#45889,#45890,#45891,#45892,
#45893),.UNSPECIFIED.,.F.,.F.,(4,3,3,3,3,3,3,3,3,3,3,3,3,3,3,3,3,3,3,3,
3,3,3,3,3,3,3,3,3,3,3,3,3,3,3,3,3,3,3,3,3,3,4),(156.163987593936,156.262228638376,
156.36048690025,156.458853693701,156.557282450291,156.655872547545,156.698209478998,
156.796807604012,156.895265386799,156.995487954569,157.093767512308,157.192014091392,
157.29025717444,157.39195436307,157.490338776499,157.59369235273,157.69704592896,
157.795644053952,157.894101836717,157.994324404493,158.092603962209,158.190850541271,
158.289093624298,158.390790812954,158.489175226362,158.592528802642,158.695882378922,
158.794480503912,158.892938286674,158.993160854451,159.091440412165,159.189686991223,
159.287930074248,159.389627262907,159.488011676311,159.591365252598,159.694718828884,
159.797216560019,159.903218753284,160.005303397592,160.107256278837,160.209067828956,
160.22122533308),.UNSPECIFIED.);
#400=B_SPLINE_CURVE_WITH_KNOTS('',3,(#45894,#45895,#45896,#45897,#45898,
#45899),.UNSPECIFIED.,.F.,.F.,(4,1,1,4),(160.221227414876,160.693555278846,
161.692391728808,162.44614673284),.UNSPECIFIED.);
#401=B_SPLINE_CURVE_WITH_KNOTS('',3,(#45901,#45902,#45903,#45904,#45905,
#45906,#45907,#45908,#45909,#45910,#45911,#45912,#45913,#45914,#45915,#45916,
#45917,#45918,#45919,#45920,#45921,#45922,#45923,#45924,#45925,#45926,#45927,
#45928,#45929,#45930,#45931,#45932,#45933,#45934,#45935,#45936,#45937,#45938,
#45939,#45940,#45941,#45942,#45943,#45944,#45945,#45946,#45947,#45948,#45949,
#45950,#45951,#45952,#45953,#45954,#45955,#45956,#45957,#45958,#45959,#45960,
#45961,#45962,#45963,#45964,#45965,#45966,#45967,#45968,#45969,#45970,#45971,
#45972,#45973),.UNSPECIFIED.,.F.,.F.,(4,3,3,3,3,3,3,3,3,3,3,3,3,3,3,3,3,
3,3,3,3,3,3,3,4),(160.22122533308,160.228748546326,160.327346671318,160.425804454083,
160.526027021859,160.624306579575,160.722553158637,160.820796241665,160.92249343032,
161.020877843728,161.124231420008,161.227584996288,161.326183121278,161.424640904041,
161.524863471817,161.623143029531,161.72138960859,161.819632691614,161.921329880273,
162.019714293678,162.123067869964,162.22642144625,162.325027405982,162.42348150006,
162.4476622356),.UNSPECIFIED.);
#402=B_SPLINE_CURVE_WITH_KNOTS('',3,(#45974,#45975,#45976,#45977,#45978,
#45979,#45980,#45981,#45982,#45983,#45984,#45985,#45986,#45987,#45988,#45989,
#45990,#45991,#45992,#45993,#45994,#45995,#45996,#45997,#45998,#45999,#46000,
#46001,#46002,#46003,#46004,#46005,#46006,#46007,#46008,#46009,#46010,#46011,
#46012,#46013,#46014,#46015,#46016,#46017,#46018,#46019,#46020,#46021,#46022,
#46023,#46024,#46025,#46026,#46027,#46028,#46029,#46030,#46031,#46032,#46033,
#46034,#46035,#46036,#46037,#46038,#46039,#46040,#46041,#46042,#46043,#46044,
#46045,#46046,#46047,#46048,#46049,#46050,#46051,#46052,#46053,#46054,#46055,
#46056,#46057,#46058,#46059,#46060,#46061,#46062,#46063,#46064,#46065,#46066,
#46067,#46068,#46069,#46070,#46071,#46072,#46073,#46074,#46075,#46076,#46077,
#46078,#46079,#46080,#46081,#46082,#46083,#46084,#46085,#46086,#46087,#46088,
#46089,#46090,#46091,#46092,#46093,#46094,#46095,#46096,#46097),
 .UNSPECIFIED.,.F.,.F.,(4,3,3,3,3,3,3,3,3,3,3,3,3,3,3,3,3,3,3,3,3,3,3,3,
3,3,3,3,3,3,3,3,3,3,3,3,3,3,3,3,3,4),(156.163531930331,156.233402746479,
156.332000871484,156.430458654262,156.530681222034,156.628960779764,156.727207358839,
156.825450441878,156.927147630519,157.025532043939,157.128885620189,157.23223919644,
157.330837321442,157.429295104218,157.529517671991,157.627797229718,157.72604380879,
157.824286891827,157.925984080471,158.024368493888,158.127722070145,158.231075646402,
158.329673771403,158.428131554177,158.528354121951,158.626633679676,158.724880258747,
158.823123341783,158.924820530428,159.023204943844,159.126558520104,159.229912096364,
159.328378576654,159.426704810661,159.526019875932,159.624169149677,159.722285836342,
159.820399593048,159.920606027993,160.018861091251,160.120043212039,160.221225332828),
 .UNSPECIFIED.);
#403=B_SPLINE_CURVE_WITH_KNOTS('',3,(#46103,#46104,#46105,#46106,#46107,
#46108,#46109,#46110),.UNSPECIFIED.,.F.,.F.,(4,1,1,1,1,4),(149.881541703048,
150.705190779227,151.704027229189,152.702863679151,153.701700129113,153.93803972631),
 .UNSPECIFIED.);
#404=B_SPLINE_CURVE_WITH_KNOTS('',3,(#46111,#46112,#46113,#46114,#46115,
#46116,#46117,#46118,#46119,#46120,#46121,#46122,#46123,#46124,#46125,#46126,
#46127,#46128,#46129,#46130,#46131,#46132,#46133,#46134,#46135,#46136,#46137,
#46138,#46139,#46140,#46141,#46142,#46143,#46144,#46145,#46146,#46147,#46148,
#46149,#46150,#46151,#46152,#46153,#46154,#46155,#46156,#46157,#46158,#46159,
#46160,#46161,#46162,#46163,#46164,#46165,#46166,#46167,#46168,#46169,#46170,
#46171,#46172,#46173,#46174,#46175,#46176,#46177,#46178,#46179,#46180),
 .UNSPECIFIED.,.F.,.F.,(4,3,3,3,3,3,3,3,3,3,3,3,3,3,3,3,3,3,3,3,3,3,3,4),
(153.9380400259,154.035163898234,154.132222574363,154.229246955325,154.326267897773,
154.423381488606,154.520541056366,154.617870832504,154.700536579074,154.799134704076,
154.897592486852,154.997815054625,155.096094612352,155.194341191424,155.292584274461,
155.394281463105,155.492665876522,155.596019452779,155.699373029036,155.79797586222,
155.89641514303,155.9947593991,156.093038592391,156.163987593936),
 .UNSPECIFIED.);
#405=B_SPLINE_CURVE_WITH_KNOTS('',3,(#46182,#46183,#46184,#46185,#46186,
#46187,#46188,#46189,#46190,#46191,#46192,#46193,#46194,#46195,#46196,#46197,
#46198,#46199,#46200,#46201,#46202,#46203,#46204,#46205,#46206,#46207,#46208,
#46209,#46210,#46211,#46212,#46213,#46214,#46215,#46216,#46217,#46218,#46219,
#46220,#46221,#46222,#46223,#46224,#46225,#46226,#46227,#46228,#46229,#46230,
#46231,#46232,#46233,#46234,#46235,#46236,#46237,#46238,#46239,#46240,#46241,
#46242,#46243,#46244,#46245,#46246,#46247,#46248,#46249,#46250,#46251),
 .UNSPECIFIED.,.F.,.F.,(4,3,3,3,3,3,3,3,3,3,3,3,3,3,3,3,3,3,3,3,3,3,3,4),
(153.938040202764,154.056659980231,154.176963650987,154.235729846555,154.334327971559,
154.432785754335,154.533008322108,154.631287879836,154.729534458909,154.827777541948,
154.92947473059,155.027859144009,155.131212720263,155.234566296517,155.33316914801,
155.431630381046,155.529972651697,155.628250049481,155.726492098717,155.824728281929,
155.923038846792,156.021391522281,156.119876942733,156.163531930331),
 .UNSPECIFIED.);
#406=B_SPLINE_CURVE_WITH_KNOTS('',3,(#46252,#46253,#46254,#46255,#46256,
#46257,#46258,#46259),.UNSPECIFIED.,.F.,.F.,(4,1,1,1,1,4),(149.880018494305,
150.240384046707,151.239220496669,152.238056946631,153.236893396593,153.9380400259),
 .UNSPECIFIED.);
#407=B_SPLINE_CURVE_WITH_KNOTS('',3,(#46265,#46266,#46267,#46268,#46269,
#46270,#46271,#46272,#46273,#46274,#46275,#46276,#46277,#46278,#46279,#46280,
#46281,#46282,#46283,#46284,#46285,#46286,#46287,#46288,#46289,#46290,#46291,
#46292,#46293,#46294,#46295,#46296,#46297,#46298,#46299,#46300,#46301,#46302,
#46303,#46304,#46305,#46306,#46307,#46308,#46309,#46310,#46311,#46312,#46313,
#46314,#46315,#46316,#46317,#46318,#46319,#46320,#46321,#46322,#46323,#46324,
#46325,#46326,#46327,#46328,#46329,#46330,#46331,#46332,#46333,#46334,#46335,
#46336,#46337,#46338,#46339,#46340,#46341,#46342,#46343,#46344,#46345,#46346,
#46347,#46348,#46349,#46350,#46351,#46352,#46353,#46354,#46355,#46356,#46357,
#46358,#46359,#46360,#46361,#46362,#46363,#46364,#46365,#46366,#46367,#46368,
#46369,#46370,#46371,#46372,#46373,#46374,#46375,#46376,#46377,#46378,#46379,
#46380,#46381,#46382,#46383,#46384,#46385,#46386,#46387,#46388,#46389,#46390,
#46391),.UNSPECIFIED.,.F.,.F.,(4,3,3,3,3,3,3,3,3,3,3,3,3,3,3,3,3,3,3,3,
3,3,3,3,3,3,3,3,3,3,3,3,3,3,3,3,3,3,3,3,3,3,4),(143.597018510158,143.695621252539,
143.713335629494,143.811933754498,143.910391537275,144.010614105047,144.108893662775,
144.207140241849,144.305383324887,144.40708051353,144.505464926948,144.608818503202,
144.712172079456,144.81077020446,144.909227987236,145.009450555009,145.107730112737,
145.20597669181,145.304219774849,145.405916963491,145.50430137691,145.607654953164,
145.711008529418,145.809606654422,145.908064437198,146.008287004971,146.106566562699,
146.204813141772,146.303056224811,146.404753413453,146.503137826872,146.606491403125,
146.709844979379,146.807643480436,146.905302408374,147.002849316603,147.100335701354,
147.197792033696,147.295248746519,147.392798083501,147.490396206244,147.588155506493,
147.65485471872),.UNSPECIFIED.);
#408=B_SPLINE_CURVE_WITH_KNOTS('',3,(#46392,#46393,#46394,#46395,#46396,
#46397,#46398),.UNSPECIFIED.,.F.,.F.,(4,1,1,1,4),(147.65485471872,147.708681429341,
148.707517879303,149.706354329265,149.881541703048),.UNSPECIFIED.);
#409=B_SPLINE_CURVE_WITH_KNOTS('',3,(#46400,#46401,#46402,#46403,#46404,
#46405),.UNSPECIFIED.,.F.,.F.,(4,1,1,4),(147.65485471872,148.242711146784,
149.241547596745,149.880018494305),.UNSPECIFIED.);
#410=B_SPLINE_CURVE_WITH_KNOTS('',3,(#46406,#46407,#46408,#46409,#46410,
#46411,#46412,#46413,#46414,#46415,#46416,#46417,#46418,#46419,#46420,#46421,
#46422,#46423,#46424,#46425,#46426,#46427,#46428,#46429,#46430,#46431,#46432,
#46433,#46434,#46435,#46436,#46437,#46438,#46439,#46440,#46441,#46442,#46443,
#46444,#46445,#46446,#46447,#46448,#46449,#46450,#46451,#46452,#46453,#46454,
#46455,#46456,#46457,#46458,#46459,#46460,#46461,#46462,#46463,#46464,#46465,
#46466,#46467,#46468,#46469,#46470,#46471,#46472,#46473,#46474,#46475,#46476,
#46477,#46478,#46479,#46480,#46481,#46482,#46483,#46484,#46485,#46486,#46487,
#46488,#46489,#46490,#46491,#46492,#46493,#46494,#46495,#46496,#46497,#46498,
#46499,#46500,#46501,#46502,#46503,#46504,#46505,#46506,#46507,#46508,#46509,
#46510,#46511,#46512,#46513,#46514,#46515,#46516,#46517,#46518,#46519,#46520,
#46521,#46522,#46523,#46524,#46525,#46526,#46527,#46528,#46529),
 .UNSPECIFIED.,.F.,.F.,(4,3,3,3,3,3,3,3,3,3,3,3,3,3,3,3,3,3,3,3,3,3,3,3,
3,3,3,3,3,3,3,3,3,3,3,3,3,3,3,3,3,4),(143.597933923764,143.696192318378,
143.794433373045,143.892686560447,143.991045348678,144.089461529939,144.188044091191,
144.247365346936,144.34596347194,144.444421254716,144.544643822489,144.642923380217,
144.741169959291,144.839413042329,144.941110230972,145.03949464439,145.142848220644,
145.246201796898,145.344799921902,145.443257704678,145.543480272451,145.641759830179,
145.740006409253,145.838249492291,145.939946680933,146.038331094352,146.141684670606,
146.24503824686,146.343636371864,146.442094154641,146.542316722413,146.640596280141,
146.738842859215,146.837085942253,146.938783130896,147.037167544314,147.140521120568,
147.243874696822,147.352569174392,147.460952550046,147.568802109382,147.654854305401),
 .UNSPECIFIED.);
#411=B_SPLINE_CURVE_WITH_KNOTS('',3,(#46535,#46536,#46537,#46538,#46539,
#46540,#46541,#46542,#46543,#46544,#46545,#46546,#46547,#46548,#46549,#46550,
#46551,#46552,#46553,#46554,#46555,#46556,#46557,#46558,#46559,#46560,#46561,
#46562,#46563,#46564,#46565,#46566,#46567,#46568,#46569,#46570,#46571,#46572,
#46573,#46574,#46575,#46576,#46577,#46578,#46579,#46580,#46581,#46582,#46583,
#46584,#46585,#46586,#46587,#46588,#46589,#46590,#46591,#46592,#46593,#46594,
#46595,#46596,#46597,#46598,#46599,#46600,#46601,#46602,#46603,#46604,#46605,
#46606,#46607,#46608,#46609,#46610,#46611,#46612,#46613,#46614,#46615,#46616,
#46617,#46618,#46619,#46620,#46621,#46622,#46623,#46624,#46625,#46626,#46627,
#46628,#46629,#46630,#46631,#46632,#46633,#46634,#46635,#46636,#46637,#46638,
#46639,#46640,#46641,#46642,#46643,#46644,#46645,#46646,#46647,#46648,#46649,
#46650,#46651,#46652,#46653,#46654,#46655,#46656,#46657,#46658),
 .UNSPECIFIED.,.F.,.F.,(4,3,3,3,3,3,3,3,3,3,3,3,3,3,3,3,3,3,3,3,3,3,3,3,
3,3,3,3,3,3,3,3,3,3,3,3,3,3,3,3,3,4),(137.314044095319,137.41561230392,
137.513996943761,137.617156936742,137.720316929723,137.818915054727,137.917372837503,
138.017595405276,138.115874963004,138.214121542077,138.312364625116,138.414061813758,
138.512446227176,138.61579980343,138.719153379684,138.817751504688,138.916209287464,
139.016431855237,139.114711412965,139.212957992039,139.311201075077,139.412898263719,
139.511282677138,139.614636253392,139.717989829646,139.81658795465,139.915045737427,
140.015268305199,140.113547862927,140.211794442001,140.310037525039,140.411734713681,
140.5101191271,140.613472703354,140.716826279608,140.815569227393,140.914173010821,
141.012667061739,141.111081830931,141.209449097702,141.307822396312,141.371669411541),
 .UNSPECIFIED.);
#412=B_SPLINE_CURVE_WITH_KNOTS('',3,(#46659,#46660,#46661,#46662,#46663,
#46664,#46665,#46666,#46667,#46668,#46669,#46670,#46671,#46672,#46673,#46674,
#46675,#46676,#46677,#46678,#46679,#46680,#46681,#46682,#46683,#46684,#46685,
#46686,#46687,#46688,#46689,#46690,#46691,#46692,#46693,#46694,#46695,#46696,
#46697,#46698,#46699,#46700,#46701,#46702,#46703,#46704,#46705,#46706,#46707,
#46708,#46709,#46710,#46711,#46712,#46713,#46714,#46715,#46716,#46717,#46718,
#46719,#46720,#46721,#46722,#46723,#46724,#46725),.UNSPECIFIED.,.F.,.F.,
(4,3,3,3,3,3,3,3,3,3,3,3,3,3,3,3,3,3,3,3,3,3,4),(141.371669411768,141.485016004534,
141.600339367052,141.71566272957,141.814260854574,141.912718637351,142.012941205123,
142.111220762851,142.209467341925,142.307710424963,142.409407613605,142.507792027024,
142.611145603278,142.714499179532,142.813105314795,142.911543009964,143.009885026327,
143.108160960053,143.206400336867,143.304679404128,143.40297364966,143.501391759162,
143.597018510158),.UNSPECIFIED.);
#413=B_SPLINE_CURVE_WITH_KNOTS('',3,(#46727,#46728,#46729,#46730,#46731,
#46732,#46733,#46734,#46735,#46736,#46737,#46738,#46739,#46740,#46741,#46742,
#46743,#46744,#46745,#46746,#46747,#46748,#46749,#46750,#46751,#46752,#46753,
#46754,#46755,#46756,#46757,#46758,#46759,#46760,#46761,#46762,#46763,#46764,
#46765,#46766,#46767,#46768,#46769,#46770,#46771,#46772,#46773,#46774,#46775,
#46776,#46777,#46778,#46779,#46780,#46781,#46782,#46783,#46784,#46785,#46786,
#46787,#46788,#46789,#46790,#46791,#46792,#46793,#46794,#46795,#46796),
 .UNSPECIFIED.,.F.,.F.,(4,3,3,3,3,3,3,3,3,3,3,3,3,3,3,3,3,3,3,3,3,3,3,4),
(141.371669411541,141.468831254161,141.566438903267,141.66339620349,141.760311911022,
141.857216996242,141.955335858935,142.052368429038,142.151030438025,142.249692447012,
142.348290572016,142.446748354792,142.546970922565,142.645250480293,142.743497059367,
142.841740142405,142.943437331047,143.041821744466,143.14517532072,143.248528896974,
143.3471049557,143.445558136373,143.543900701709,143.597933923764),
 .UNSPECIFIED.);
#414=B_SPLINE_CURVE_WITH_KNOTS('',3,(#46797,#46798,#46799,#46800,#46801,
#46802,#46803,#46804),.UNSPECIFIED.,.F.,.F.,(4,1,1,1,1,4),(137.314688076936,
138.254346647165,139.253183097127,140.252019547089,141.25085599705,141.371669411541),
 .UNSPECIFIED.);
#415=B_SPLINE_CURVE_WITH_KNOTS('',3,(#46810,#46811,#46812,#46813,#46814,
#46815,#46816,#46817,#46818,#46819,#46820,#46821,#46822,#46823,#46824,#46825,
#46826,#46827,#46828,#46829,#46830,#46831,#46832,#46833,#46834,#46835,#46836,
#46837,#46838,#46839,#46840,#46841,#46842,#46843,#46844,#46845,#46846,#46847,
#46848,#46849,#46850,#46851,#46852,#46853,#46854,#46855,#46856,#46857,#46858,
#46859,#46860,#46861,#46862,#46863,#46864,#46865,#46866,#46867,#46868,#46869,
#46870,#46871,#46872,#46873,#46874,#46875,#46876,#46877,#46878,#46879,#46880,
#46881,#46882,#46883,#46884,#46885,#46886,#46887,#46888,#46889,#46890,#46891,
#46892,#46893,#46894,#46895,#46896,#46897,#46898,#46899,#46900,#46901,#46902,
#46903,#46904,#46905,#46906,#46907,#46908,#46909,#46910,#46911,#46912,#46913,
#46914,#46915,#46916,#46917,#46918,#46919,#46920,#46921,#46922,#46923,#46924,
#46925,#46926,#46927,#46928,#46929,#46930,#46931,#46932,#46933),
 .UNSPECIFIED.,.F.,.F.,(4,3,3,3,3,3,3,3,3,3,3,3,3,3,3,3,3,3,3,3,3,3,3,3,
3,3,3,3,3,3,3,3,3,3,3,3,3,3,3,3,3,4),(131.031654973638,131.129931712951,
131.228177248346,131.326421060941,131.426640353193,131.525027385579,131.626162807765,
131.727298229951,131.825896354955,131.924354137732,132.024576705504,132.122856263233,
132.221102842306,132.319345925345,132.421043113987,132.519427527405,132.622781103659,
132.726134679913,132.824732804917,132.923190587694,133.023413155466,133.121692713194,
133.219939292268,133.318182375306,133.419879563948,133.518263977367,133.621617553621,
133.724971129875,133.823569254879,133.922027037656,134.022249605428,134.120529163156,
134.21877574223,134.317018825268,134.418716013911,134.517100427329,134.620454003583,
134.723807579837,134.8363385207,134.948409000641,135.059693750754,135.088484104126),
 .UNSPECIFIED.);
#416=B_SPLINE_CURVE_WITH_KNOTS('',3,(#46934,#46935,#46936,#46937,#46938,
#46939,#46940,#46941,#46942,#46943,#46944,#46945,#46946,#46947,#46948,#46949,
#46950,#46951,#46952,#46953,#46954,#46955,#46956,#46957,#46958,#46959,#46960,
#46961,#46962,#46963,#46964,#46965,#46966,#46967,#46968,#46969,#46970,#46971,
#46972,#46973,#46974,#46975,#46976,#46977,#46978,#46979,#46980,#46981,#46982,
#46983,#46984,#46985,#46986,#46987,#46988,#46989,#46990,#46991,#46992,#46993,
#46994,#46995,#46996,#46997,#46998,#46999,#47000,#47001,#47002,#47003),
 .UNSPECIFIED.,.F.,.F.,(4,3,3,3,3,3,3,3,3,3,3,3,3,3,3,3,3,3,3,3,3,3,3,4),
(135.088484104361,135.187254556185,135.286029876604,135.384838499174,135.483776463585,
135.582788468008,135.681976179005,135.722644029799,135.821242154803,135.919699937579,
136.019922505352,136.11820206308,136.216448642154,136.314691725192,136.416388913834,
136.514773327253,136.618126903507,136.721480479761,136.82006725633,136.918521077985,
137.017401832319,137.115677672201,137.21486088376,137.314044095319),
 .UNSPECIFIED.);
#417=B_SPLINE_CURVE_WITH_KNOTS('',3,(#47005,#47006,#47007,#47008,#47009,
#47010,#47011),.UNSPECIFIED.,.F.,.F.,(4,1,1,1,4),(135.088484104361,135.257837297279,
136.256673747241,137.255510197203,137.314688076936),.UNSPECIFIED.);
#418=B_SPLINE_CURVE_WITH_KNOTS('',3,(#47012,#47013,#47014,#47015,#47016,
#47017,#47018,#47019,#47020,#47021,#47022,#47023,#47024,#47025,#47026,#47027,
#47028,#47029,#47030,#47031,#47032,#47033,#47034,#47035,#47036,#47037,#47038,
#47039,#47040,#47041,#47042,#47043,#47044,#47045,#47046,#47047,#47048,#47049,
#47050,#47051,#47052,#47053,#47054,#47055,#47056,#47057,#47058,#47059,#47060,
#47061,#47062,#47063,#47064,#47065,#47066,#47067,#47068,#47069,#47070,#47071,
#47072,#47073,#47074,#47075,#47076,#47077,#47078,#47079,#47080,#47081,#47082,
#47083,#47084,#47085,#47086,#47087,#47088,#47089,#47090,#47091,#47092,#47093,
#47094,#47095,#47096,#47097,#47098,#47099,#47100,#47101,#47102,#47103,#47104,
#47105,#47106,#47107,#47108,#47109,#47110,#47111,#47112,#47113,#47114,#47115,
#47116,#47117,#47118,#47119,#47120,#47121,#47122,#47123,#47124,#47125,#47126,
#47127,#47128,#47129,#47130,#47131,#47132,#47133,#47134,#47135,#47136,#47137,
#47138),.UNSPECIFIED.,.F.,.F.,(4,3,3,3,3,3,3,3,3,3,3,3,3,3,3,3,3,3,3,3,
3,3,3,3,3,3,3,3,3,3,3,3,3,3,3,3,3,3,3,3,3,3,4),(131.030544944991,131.128979440939,
131.227573133845,131.262491497432,131.361089622436,131.459547405212,131.559769972985,
131.658049530713,131.756296109787,131.854539192825,131.956236381467,132.054620794886,
132.15797437114,132.261327947394,132.359926072398,132.458383855174,132.558606422947,
132.656885980675,132.755132559748,132.853375642787,132.955072831429,133.053457244848,
133.156810821101,133.260164397355,133.358762522359,133.457220305135,133.557442872908,
133.655722430636,133.753969009709,133.852212092748,133.95390928139,134.052293694809,
134.155647271063,134.259000847317,134.356128675187,134.453094160804,134.549968416923,
134.6467826177,134.743567858739,134.84039997176,134.937256811787,135.034231214226,
135.088484104361),.UNSPECIFIED.);
#419=B_SPLINE_CURVE_WITH_KNOTS('',3,(#47144,#47145,#47146,#47147,#47148,
#47149,#47150,#47151),.UNSPECIFIED.,.F.,.F.,(4,1,1,1,1,4),(124.748033484277,
125.73427953018,126.733115980142,127.731952430104,128.730788880066,128.805298797182),
 .UNSPECIFIED.);
#420=B_SPLINE_CURVE_WITH_KNOTS('',3,(#47152,#47153,#47154,#47155,#47156,
#47157,#47158,#47159,#47160,#47161,#47162,#47163,#47164,#47165,#47166,#47167,
#47168,#47169,#47170,#47171,#47172,#47173,#47174,#47175,#47176,#47177,#47178,
#47179,#47180,#47181,#47182,#47183,#47184,#47185,#47186,#47187,#47188,#47189,
#47190,#47191,#47192,#47193,#47194,#47195,#47196,#47197,#47198,#47199,#47200,
#47201,#47202,#47203,#47204,#47205,#47206,#47207,#47208,#47209,#47210,#47211,
#47212,#47213,#47214,#47215,#47216,#47217,#47218,#47219,#47220,#47221),
 .UNSPECIFIED.,.F.,.F.,(4,3,3,3,3,3,3,3,3,3,3,3,3,3,3,3,3,3,3,3,3,3,3,4),
(128.805298797182,128.902840431273,129.000250613517,129.097560812666,129.194818343698,
129.292053887498,129.389298094495,129.486642967569,129.584044330746,129.681605924981,
129.729625330028,129.828223455032,129.926681237808,130.026903805581,130.125183363309,
130.223429942382,130.321673025421,130.423370214063,130.521754627482,130.625108203735,
130.728461779989,130.82704702784,130.929351000739,131.031654973638),
 .UNSPECIFIED.);
#421=B_SPLINE_CURVE_WITH_KNOTS('',3,(#47223,#47224,#47225,#47226,#47227,
#47228,#47229,#47230,#47231,#47232,#47233,#47234,#47235,#47236,#47237,#47238,
#47239,#47240,#47241,#47242,#47243,#47244,#47245,#47246,#47247,#47248,#47249,
#47250,#47251,#47252,#47253,#47254,#47255,#47256,#47257,#47258,#47259,#47260,
#47261,#47262,#47263,#47264,#47265,#47266,#47267,#47268,#47269,#47270,#47271,
#47272,#47273,#47274,#47275,#47276,#47277,#47278,#47279,#47280,#47281,#47282,
#47283,#47284,#47285,#47286,#47287,#47288,#47289,#47290,#47291,#47292),
 .UNSPECIFIED.,.F.,.F.,(4,3,3,3,3,3,3,3,3,3,3,3,3,3,3,3,3,3,3,3,3,3,3,4),
(128.805299011159,128.91008561987,129.01525575915,129.120630109632,129.226318351047,
129.264818597508,129.363416722512,129.461874505288,129.562097073061,129.660376630789,
129.758623209863,129.856866292901,129.958563481543,130.056947894962,130.160301471216,
130.26365504747,130.362225486655,130.460667523599,130.55901086589,130.657285118175,
130.755545076206,130.853792579363,130.952108672697,131.030544944991),
 .UNSPECIFIED.);
#422=B_SPLINE_CURVE_WITH_KNOTS('',3,(#47293,#47294,#47295,#47296,#47297,
#47298,#47299,#47300),.UNSPECIFIED.,.F.,.F.,(4,1,1,1,1,4),(124.748072441043,
125.26947279766,126.268309247622,127.267145697584,128.265982147546,128.805298797182),
 .UNSPECIFIED.);
#423=B_SPLINE_CURVE_WITH_KNOTS('',3,(#47306,#47307,#47308,#47309,#47310,
#47311,#47312,#47313,#47314,#47315,#47316,#47317,#47318,#47319,#47320,#47321,
#47322,#47323,#47324,#47325,#47326,#47327,#47328,#47329,#47330,#47331,#47332,
#47333,#47334,#47335,#47336,#47337,#47338,#47339,#47340,#47341,#47342,#47343,
#47344,#47345,#47346,#47347,#47348,#47349,#47350,#47351,#47352,#47353,#47354,
#47355,#47356,#47357,#47358,#47359,#47360,#47361,#47362,#47363,#47364,#47365,
#47366,#47367,#47368,#47369,#47370,#47371,#47372,#47373,#47374,#47375,#47376,
#47377,#47378,#47379,#47380,#47381,#47382,#47383,#47384,#47385,#47386,#47387,
#47388,#47389,#47390,#47391,#47392,#47393,#47394,#47395,#47396,#47397,#47398,
#47399,#47400,#47401,#47402,#47403,#47404,#47405,#47406,#47407,#47408,#47409,
#47410,#47411,#47412,#47413,#47414,#47415,#47416,#47417,#47418,#47419,#47420,
#47421,#47422,#47423,#47424,#47425,#47426,#47427,#47428,#47429),
 .UNSPECIFIED.,.F.,.F.,(4,3,3,3,3,3,3,3,3,3,3,3,3,3,3,3,3,3,3,3,3,3,3,3,
3,3,3,3,3,3,3,3,3,3,3,3,3,3,3,3,3,4),(118.464214608881,118.562615726968,
118.661189997389,118.742424380447,118.841022505451,118.939480288228,119.039702856,
119.137982413728,119.236228992802,119.33447207584,119.436169264482,119.534553677901,
119.637907254155,119.741260830409,119.839858955413,119.93831673819,120.038539305962,
120.136818863691,120.235065442764,120.333308525803,120.435005714445,120.533390127863,
120.636743704117,120.740097280371,120.838695405375,120.937153188151,121.037375755924,
121.135655313652,121.233901892726,121.332144975764,121.433842164406,121.532226577825,
121.635580154079,121.738933730333,121.836831200292,121.933909156543,122.030894120917,
122.127817176647,122.226391254986,122.323316910845,122.422715200423,122.522113490002),
 .UNSPECIFIED.);
#424=B_SPLINE_CURVE_WITH_KNOTS('',3,(#47430,#47431,#47432,#47433,#47434,
#47435,#47436),.UNSPECIFIED.,.F.,.F.,(4,1,1,1,4),(122.522113490002,122.737770180294,
123.736606630256,124.735443080218,124.748033484277),.UNSPECIFIED.);
#425=B_SPLINE_CURVE_WITH_KNOTS('',3,(#47438,#47439,#47440,#47441,#47442,
#47443),.UNSPECIFIED.,.F.,.F.,(4,1,1,4),(122.522113490002,123.271799897737,
124.270636347699,124.748072441043),.UNSPECIFIED.);
#426=B_SPLINE_CURVE_WITH_KNOTS('',3,(#47444,#47445,#47446,#47447,#47448,
#47449,#47450,#47451,#47452,#47453,#47454,#47455,#47456,#47457,#47458,#47459,
#47460,#47461,#47462,#47463,#47464,#47465,#47466,#47467,#47468,#47469,#47470,
#47471,#47472,#47473,#47474,#47475,#47476,#47477,#47478,#47479,#47480,#47481,
#47482,#47483,#47484,#47485,#47486,#47487,#47488,#47489,#47490,#47491,#47492,
#47493,#47494,#47495,#47496,#47497,#47498,#47499,#47500,#47501,#47502,#47503,
#47504,#47505,#47506,#47507,#47508,#47509,#47510,#47511,#47512,#47513,#47514,
#47515,#47516,#47517,#47518,#47519,#47520,#47521,#47522,#47523,#47524,#47525,
#47526,#47527,#47528,#47529,#47530,#47531,#47532,#47533,#47534,#47535,#47536,
#47537,#47538,#47539,#47540,#47541,#47542,#47543,#47544,#47545,#47546,#47547,
#47548,#47549,#47550,#47551,#47552,#47553,#47554,#47555,#47556,#47557,#47558,
#47559,#47560,#47561,#47562,#47563,#47564,#47565,#47566,#47567),
 .UNSPECIFIED.,.F.,.F.,(4,3,3,3,3,3,3,3,3,3,3,3,3,3,3,3,3,3,3,3,3,3,3,3,
3,3,3,3,3,3,3,3,3,3,3,3,3,3,3,3,3,4),(118.465360150378,118.566746893817,
118.665030509587,118.763278701368,118.861520954009,118.959786737651,119.058164566875,
119.156610035311,119.255210840485,119.276454097889,119.375052222893,119.47351000567,
119.573732573442,119.67201213117,119.770258710244,119.868501793282,119.970198981924,
120.068583395343,120.171936971597,120.275290547851,120.373888672855,120.472346455631,
120.572569023404,120.670848581132,120.769095160206,120.867338243244,120.969035431886,
121.067419845305,121.170773421559,121.274126997813,121.372725122817,121.471182905594,
121.571405473366,121.669685031094,121.767931610168,121.866174693206,121.967871881848,
122.066256295267,122.169609871521,122.272963447775,122.40085782982,122.522113389975),
 .UNSPECIFIED.);
#427=B_SPLINE_CURVE_WITH_KNOTS('',3,(#47573,#47574,#47575,#47576,#47577,
#47578,#47579,#47580,#47581,#47582,#47583,#47584,#47585,#47586,#47587,#47588,
#47589,#47590,#47591,#47592,#47593,#47594,#47595,#47596,#47597,#47598,#47599,
#47600,#47601,#47602,#47603,#47604,#47605,#47606,#47607,#47608,#47609,#47610,
#47611,#47612,#47613,#47614,#47615,#47616,#47617,#47618,#47619,#47620,#47621,
#47622,#47623,#47624,#47625,#47626,#47627,#47628,#47629,#47630,#47631,#47632,
#47633,#47634,#47635,#47636,#47637,#47638,#47639,#47640,#47641,#47642,#47643,
#47644,#47645,#47646,#47647,#47648,#47649,#47650,#47651,#47652,#47653,#47654,
#47655,#47656,#47657,#47658,#47659,#47660,#47661,#47662,#47663,#47664,#47665,
#47666,#47667,#47668,#47669,#47670,#47671,#47672,#47673,#47674,#47675,#47676,
#47677,#47678,#47679,#47680,#47681,#47682,#47683,#47684,#47685,#47686,#47687,
#47688,#47689,#47690,#47691,#47692,#47693,#47694,#47695,#47696),
 .UNSPECIFIED.,.F.,.F.,(4,3,3,3,3,3,3,3,3,3,3,3,3,3,3,3,3,3,3,3,3,3,3,3,
3,3,3,3,3,3,3,3,3,3,3,3,3,3,3,3,3,4),(112.18179093325,112.280032836003,
112.378281939794,112.476633715995,112.575038453655,112.673614632877,112.749405680676,
112.84800380568,112.946461588456,113.046684156229,113.144963713957,113.24321029303,
113.341453376069,113.443150564711,113.54153497813,113.644888554384,113.748242130638,
113.846840255641,113.945298038418,114.045520606191,114.143800163919,114.242046742992,
114.340289826031,114.441987014673,114.540371428091,114.643725004345,114.747078580599,
114.845676705603,114.944134488379,115.044357056152,115.14263661388,115.240883192953,
115.339126275992,115.440823464634,115.539207878053,115.642561454307,115.745915030561,
115.84988875933,115.953561696348,116.057054365164,116.160309146371,116.238928182547),
 .UNSPECIFIED.);
#428=B_SPLINE_CURVE_WITH_KNOTS('',3,(#47697,#47698,#47699,#47700,#47701,
#47702,#47703,#47704,#47705,#47706,#47707,#47708,#47709,#47710,#47711,#47712,
#47713,#47714,#47715,#47716,#47717,#47718,#47719,#47720,#47721,#47722,#47723,
#47724,#47725,#47726,#47727,#47728,#47729,#47730,#47731,#47732,#47733,#47734,
#47735,#47736,#47737,#47738,#47739,#47740,#47741,#47742,#47743,#47744,#47745,
#47746,#47747,#47748,#47749,#47750,#47751,#47752,#47753,#47754,#47755,#47756,
#47757,#47758,#47759,#47760,#47761,#47762,#47763,#47764,#47765,#47766),
 .UNSPECIFIED.,.F.,.F.,(4,3,3,3,3,3,3,3,3,3,3,3,3,3,3,3,3,3,3,3,3,3,3,4),
(116.238928182823,116.341566510357,116.44447107289,116.547509821617,116.650828963887,
116.744751480523,116.843349605527,116.941807388303,117.042029956076,117.140309513804,
117.238556092878,117.336799175916,117.438496364558,117.536880777977,117.640234354231,
117.743587930485,117.842162082216,117.940606624238,118.038951269659,118.137225626952,
118.235476585644,118.333714612383,118.431998836546,118.464214608881),
 .UNSPECIFIED.);
#429=B_SPLINE_CURVE_WITH_KNOTS('',3,(#47768,#47769,#47770,#47771,#47772,
#47773,#47774,#47775,#47776,#47777,#47778,#47779,#47780,#47781,#47782,#47783,
#47784,#47785,#47786,#47787,#47788,#47789,#47790,#47791,#47792,#47793,#47794,
#47795,#47796,#47797,#47798,#47799,#47800,#47801,#47802,#47803,#47804,#47805,
#47806,#47807,#47808,#47809,#47810,#47811,#47812,#47813,#47814,#47815,#47816,
#47817,#47818,#47819,#47820,#47821,#47822,#47823,#47824,#47825,#47826,#47827,
#47828,#47829,#47830,#47831,#47832,#47833,#47834,#47835,#47836,#47837),
 .UNSPECIFIED.,.F.,.F.,(4,3,3,3,3,3,3,3,3,3,3,3,3,3,3,3,3,3,3,3,3,3,3,4),
(116.238928182823,116.279944748004,116.378542873008,116.477000655784,116.577223223557,
116.675502781285,116.773749360358,116.871992443397,116.973689632039,117.072074045458,
117.175427621712,117.278781197966,117.37737932297,117.475837105746,117.576059673519,
117.674339231247,117.77258581032,117.870828893359,117.972526082001,118.07091049542,
118.174264071673,118.277617647927,118.376189313834,118.465360150378),
 .UNSPECIFIED.);
#430=B_SPLINE_CURVE_WITH_KNOTS('',3,(#47838,#47839,#47840,#47841,#47842,
#47843,#47844,#47845),.UNSPECIFIED.,.F.,.F.,(4,1,1,1,1,4),(112.180986328742,
112.284598948156,113.283435398118,114.28227184808,115.281108298042,116.2389227975),
 .UNSPECIFIED.);
#431=B_SPLINE_CURVE_WITH_KNOTS('',3,(#47851,#47852,#47853,#47854,#47855,
#47856,#47857,#47858,#47859,#47860,#47861,#47862,#47863,#47864,#47865,#47866,
#47867,#47868,#47869,#47870,#47871,#47872,#47873,#47874,#47875,#47876,#47877,
#47878,#47879,#47880,#47881,#47882,#47883,#47884,#47885,#47886,#47887,#47888,
#47889,#47890,#47891,#47892,#47893,#47894,#47895,#47896,#47897,#47898,#47899,
#47900,#47901,#47902,#47903,#47904,#47905,#47906,#47907,#47908,#47909,#47910,
#47911,#47912,#47913,#47914,#47915,#47916,#47917,#47918,#47919,#47920,#47921,
#47922,#47923,#47924,#47925,#47926,#47927,#47928,#47929,#47930,#47931,#47932,
#47933,#47934,#47935,#47936,#47937,#47938,#47939,#47940,#47941,#47942,#47943,
#47944,#47945,#47946,#47947,#47948,#47949,#47950,#47951,#47952,#47953,#47954,
#47955,#47956,#47957,#47958,#47959,#47960,#47961,#47962,#47963,#47964,#47965,
#47966,#47967,#47968,#47969,#47970,#47971,#47972,#47973,#47974),
 .UNSPECIFIED.,.F.,.F.,(4,3,3,3,3,3,3,3,3,3,3,3,3,3,3,3,3,3,3,3,3,3,3,3,
3,3,3,3,3,3,3,3,3,3,3,3,3,3,3,3,3,4),(105.898938929587,105.99734597658,
106.095658484987,106.193920762289,106.292162310713,106.390412604461,106.488766496703,
106.587174737975,106.685752817441,106.756386980904,106.854985105908,106.953442888684,
107.053665456457,107.151945014185,107.250191593259,107.348434676297,107.450131864939,
107.548516278358,107.651869854612,107.755223430866,107.85382155587,107.952279338646,
108.052501906419,108.150781464147,108.249028043221,108.347271126259,108.448968314902,
108.54735272832,108.650706304574,108.754059880828,108.852658005832,108.951115788608,
109.051338356381,109.149617914109,109.247864493183,109.346107576221,109.447804764863,
109.546189178282,109.649542754536,109.75289633079,109.893212936358,109.955742875643),
 .UNSPECIFIED.);
#432=B_SPLINE_CURVE_WITH_KNOTS('',3,(#47975,#47976,#47977,#47978,#47979,
#47980,#47981,#47982,#47983,#47984,#47985,#47986,#47987,#47988,#47989,#47990,
#47991,#47992,#47993,#47994,#47995,#47996,#47997,#47998,#47999,#48000,#48001,
#48002,#48003,#48004,#48005,#48006,#48007,#48008,#48009,#48010,#48011,#48012,
#48013,#48014,#48015,#48016,#48017,#48018,#48019,#48020,#48021,#48022,#48023,
#48024,#48025,#48026,#48027,#48028,#48029,#48030,#48031,#48032,#48033,#48034,
#48035,#48036,#48037,#48038,#48039,#48040,#48041,#48042,#48043,#48044,#48045,
#48046,#48047),.UNSPECIFIED.,.F.,.F.,(4,3,3,3,3,3,3,3,3,3,3,3,3,3,3,3,3,
3,3,3,3,3,3,3,4),(109.955742875951,110.055241614051,110.152151423466,110.249014842069,
110.345862894414,110.447330365999,110.544300028994,110.641334438529,110.738518045248,
110.751732780752,110.850330905756,110.948788688532,111.049011256305,111.147290814033,
111.245537393107,111.343780476145,111.445477664787,111.543862078206,111.64721565446,
111.750569230714,111.849176820414,111.947618966285,112.045965736407,112.144240689691,
112.18179093325),.UNSPECIFIED.);
#433=B_SPLINE_CURVE_WITH_KNOTS('',3,(#48049,#48050,#48051,#48052,#48053,
#48054),.UNSPECIFIED.,.F.,.F.,(4,1,1,4),(109.955750010087,110.286926048232,
111.285762498194,112.180986328742),.UNSPECIFIED.);
#434=B_SPLINE_CURVE_WITH_KNOTS('',3,(#48055,#48056,#48057,#48058,#48059,
#48060,#48061,#48062,#48063,#48064,#48065,#48066,#48067,#48068,#48069,#48070,
#48071,#48072,#48073,#48074,#48075,#48076,#48077,#48078,#48079,#48080,#48081,
#48082,#48083,#48084,#48085,#48086,#48087,#48088,#48089,#48090,#48091,#48092,
#48093,#48094,#48095,#48096,#48097,#48098,#48099,#48100,#48101,#48102,#48103,
#48104,#48105,#48106,#48107,#48108,#48109,#48110,#48111,#48112,#48113,#48114,
#48115,#48116,#48117,#48118,#48119,#48120,#48121,#48122,#48123,#48124,#48125,
#48126,#48127,#48128,#48129,#48130,#48131,#48132,#48133,#48134,#48135,#48136,
#48137,#48138,#48139,#48140,#48141,#48142,#48143,#48144,#48145,#48146,#48147,
#48148,#48149,#48150,#48151,#48152,#48153,#48154,#48155,#48156,#48157,#48158,
#48159,#48160,#48161,#48162,#48163,#48164,#48165,#48166,#48167,#48168,#48169,
#48170,#48171,#48172,#48173,#48174,#48175,#48176,#48177,#48178),
 .UNSPECIFIED.,.F.,.F.,(4,3,3,3,3,3,3,3,3,3,3,3,3,3,3,3,3,3,3,3,3,3,3,3,
3,3,3,3,3,3,3,3,3,3,3,3,3,3,3,3,3,4),(105.898082546227,105.996456971766,
106.094847348914,106.193416319605,106.291580248385,106.390178373389,106.488636156165,
106.588858723938,106.687138281666,106.78538486074,106.883627943778,106.98532513242,
107.083709545839,107.187063122093,107.290416698347,107.389014823351,107.487472606128,
107.5876951739,107.685974731629,107.784221310702,107.882464393741,107.984161582383,
108.082545995802,108.185899572055,108.289253148309,108.387851273313,108.486309056089,
108.586531623862,108.68481118159,108.783057760664,108.881300843702,108.982998032345,
109.081382445763,109.184736022017,109.288089598271,109.386591328535,109.484956309733,
109.583214317042,109.681399820024,109.779540599734,109.877698313765,109.955742875643),
 .UNSPECIFIED.);
#435=B_SPLINE_CURVE_WITH_KNOTS('',3,(#48184,#48185,#48186,#48187,#48188,
#48189,#48190,#48191),.UNSPECIFIED.,.F.,.F.,(4,1,1,1,1,4),(99.6144332342635,
99.7645318311714,100.763368281133,101.762204731095,102.761041181057,103.672548858934),
 .UNSPECIFIED.);
#436=B_SPLINE_CURVE_WITH_KNOTS('',3,(#48192,#48193,#48194,#48195,#48196,
#48197,#48198,#48199,#48200,#48201,#48202,#48203,#48204,#48205,#48206,#48207,
#48208,#48209,#48210,#48211,#48212,#48213,#48214,#48215,#48216,#48217,#48218,
#48219,#48220,#48221,#48222,#48223,#48224,#48225,#48226,#48227,#48228,#48229,
#48230,#48231,#48232,#48233,#48234,#48235,#48236,#48237,#48238,#48239,#48240,
#48241,#48242,#48243,#48244,#48245,#48246,#48247,#48248,#48249,#48250,#48251,
#48252,#48253,#48254,#48255,#48256,#48257,#48258,#48259,#48260,#48261),
 .UNSPECIFIED.,.F.,.F.,(4,3,3,3,3,3,3,3,3,3,3,3,3,3,3,3,3,3,3,3,3,3,3,4),
(103.672557568463,103.759877631019,103.858475756023,103.9569335388,104.057156106572,
104.1554356643,104.253682243374,104.351925326412,104.453622515055,104.552006928473,
104.655360504727,104.758714080981,104.857312205985,104.955769988761,105.055992556534,
105.154272114262,105.252518693336,105.350761776374,105.452458965016,105.550843378435,
105.654196954689,105.757550530943,105.856140410584,105.898938929587),
 .UNSPECIFIED.);
#437=B_SPLINE_CURVE_WITH_KNOTS('',3,(#48263,#48264,#48265,#48266,#48267,
#48268,#48269,#48270,#48271,#48272,#48273,#48274,#48275,#48276,#48277,#48278,
#48279,#48280,#48281,#48282,#48283,#48284,#48285,#48286,#48287,#48288,#48289,
#48290,#48291,#48292,#48293,#48294,#48295,#48296,#48297,#48298,#48299,#48300,
#48301,#48302,#48303,#48304,#48305,#48306,#48307,#48308,#48309,#48310,#48311,
#48312,#48313,#48314,#48315,#48316,#48317,#48318,#48319,#48320,#48321,#48322,
#48323,#48324,#48325,#48326,#48327,#48328,#48329,#48330,#48331,#48332,#48333,
#48334,#48335),.UNSPECIFIED.,.F.,.F.,(4,3,3,3,3,3,3,3,3,3,3,3,3,3,3,3,3,
3,3,3,3,3,3,3,4),(103.672557568463,103.771601702603,103.870660322484,103.96976131202,
104.06899945985,104.168318657834,104.267812431338,104.293907348461,104.392505473465,
104.490963256242,104.591185824014,104.689465381742,104.787711960816,104.885955043854,
104.987652232497,105.086036645915,105.189390222169,105.292743798423,105.39132916073,
105.489781902009,105.591857063063,105.690131969833,105.788367325292,105.886604359629,
105.898082546227),.UNSPECIFIED.);
#438=B_SPLINE_CURVE_WITH_KNOTS('',3,(#48336,#48337,#48338,#48339,#48340,
#48341,#48342,#48343),.UNSPECIFIED.,.F.,.F.,(4,1,1,1,1,4),(99.6160278953699,
100.298561548614,101.297397998576,102.296234448537,103.295070898499,103.672550060693),
 .UNSPECIFIED.);
#439=B_SPLINE_CURVE_WITH_KNOTS('',3,(#48349,#48350,#48351,#48352,#48353,
#48354,#48355,#48356,#48357,#48358,#48359,#48360,#48361,#48362,#48363,#48364,
#48365,#48366,#48367,#48368,#48369,#48370,#48371,#48372,#48373,#48374,#48375,
#48376,#48377,#48378,#48379,#48380,#48381,#48382,#48383,#48384,#48385,#48386,
#48387,#48388,#48389,#48390,#48391,#48392,#48393,#48394,#48395,#48396,#48397,
#48398,#48399,#48400,#48401,#48402,#48403,#48404,#48405,#48406,#48407,#48408,
#48409,#48410,#48411,#48412,#48413,#48414,#48415,#48416,#48417,#48418,#48419,
#48420,#48421,#48422,#48423,#48424,#48425,#48426,#48427,#48428,#48429,#48430,
#48431,#48432,#48433,#48434,#48435,#48436,#48437,#48438,#48439,#48440,#48441,
#48442,#48443,#48444,#48445,#48446,#48447,#48448,#48449,#48450,#48451,#48452,
#48453,#48454,#48455,#48456,#48457,#48458,#48459,#48460,#48461,#48462,#48463,
#48464,#48465,#48466,#48467,#48468,#48469,#48470,#48471,#48472,#48473,#48474,
#48475),.UNSPECIFIED.,.F.,.F.,(4,3,3,3,3,3,3,3,3,3,3,3,3,3,3,3,3,3,3,3,
3,3,3,3,3,3,3,3,3,3,3,3,3,3,3,3,3,3,3,3,3,3,4),(93.3318434563844,93.4301005392899,
93.5284655236451,93.6268914765217,93.7254798512049,93.7715131314001,93.8701112564038,
93.9685690391806,94.0687916069533,94.1670711646814,94.2653177437548,94.3635608267931,
94.4652580154354,94.5636424288541,94.6669960051081,94.770349581362,94.8689477063657,
94.9674054891425,95.0676280569152,95.1659076146434,95.2641541937167,95.3623972767553,
95.4640944653975,95.5624788788163,95.6658324550701,95.7691860313239,95.8677841563277,
95.9662419391043,96.066464506877,96.1647440646051,96.2629906436786,96.3612337267171,
96.4629309153592,96.561315328778,96.6646689050319,96.7680224812857,96.867499372579,
96.9668292609829,97.0660403563902,97.1651524247998,97.264207533224,97.3632407686273,
97.3893722612837),.UNSPECIFIED.);
#440=B_SPLINE_CURVE_WITH_KNOTS('',3,(#48476,#48477,#48478,#48479,#48480,
#48481),.UNSPECIFIED.,.F.,.F.,(4,1,1,4),(97.389379769506,97.7668589312476,
98.7656953812095,99.6144332342635),.UNSPECIFIED.);
#441=B_SPLINE_CURVE_WITH_KNOTS('',3,(#48483,#48484,#48485,#48486,#48487,
#48488),.UNSPECIFIED.,.F.,.F.,(4,1,1,4),(97.3893809713061,98.3008886486899,
99.2997250986518,99.6160278953699),.UNSPECIFIED.);
#442=B_SPLINE_CURVE_WITH_KNOTS('',3,(#48489,#48490,#48491,#48492,#48493,
#48494,#48495,#48496,#48497,#48498,#48499,#48500,#48501,#48502,#48503,#48504,
#48505,#48506,#48507,#48508,#48509,#48510,#48511,#48512,#48513,#48514,#48515,
#48516,#48517,#48518,#48519,#48520,#48521,#48522,#48523,#48524,#48525,#48526,
#48527,#48528,#48529,#48530,#48531,#48532,#48533,#48534,#48535,#48536,#48537,
#48538,#48539,#48540,#48541,#48542,#48543,#48544,#48545,#48546,#48547,#48548,
#48549,#48550,#48551,#48552,#48553,#48554,#48555,#48556,#48557,#48558,#48559,
#48560,#48561,#48562,#48563,#48564,#48565,#48566,#48567,#48568,#48569,#48570,
#48571,#48572,#48573,#48574,#48575,#48576,#48577,#48578,#48579,#48580,#48581,
#48582,#48583,#48584,#48585,#48586,#48587,#48588,#48589,#48590,#48591,#48592,
#48593,#48594,#48595,#48596,#48597,#48598,#48599,#48600,#48601,#48602,#48603,
#48604,#48605,#48606,#48607,#48608,#48609,#48610,#48611,#48612),
 .UNSPECIFIED.,.F.,.F.,(4,3,3,3,3,3,3,3,3,3,3,3,3,3,3,3,3,3,3,3,3,3,3,3,
3,3,3,3,3,3,3,3,3,3,3,3,3,3,3,3,3,4),(93.3321733281741,93.4307320743328,
93.5291589655597,93.627483394628,93.7257523855544,93.8239954482649,93.9222420599768,
94.020589121044,94.1189858625401,94.2175579041604,94.3055428488424,94.4041409738461,
94.5025987566229,94.6028213243956,94.7011008821237,94.7993474611971,94.8975905442356,
94.9992877328778,95.0976721462966,95.2010257225505,95.3043792988043,95.402977423808,
95.5014352065847,95.6016577743574,95.6999373320855,95.7981839111589,95.8964269941973,
95.9981241828395,96.0965085962583,96.1998621725122,96.3032157487661,96.4018138737698,
96.5002716565465,96.6004942243192,96.6987737820473,96.7970203611207,96.8952634441592,
96.9969606328014,97.0953450462202,97.1986986224741,97.302052198728,97.3893722612837),
 .UNSPECIFIED.);
#443=B_SPLINE_CURVE_WITH_KNOTS('',3,(#48618,#48619,#48620,#48621,#48622,
#48623,#48624,#48625),.UNSPECIFIED.,.F.,.F.,(4,1,1,1,1,4),(87.0497429340083,
87.7784944316289,88.7773308815907,89.7761673315526,90.7750037815145,91.1061798190739),
 .UNSPECIFIED.);
#444=B_SPLINE_CURVE_WITH_KNOTS('',3,(#48626,#48627,#48628,#48629,#48630,
#48631,#48632,#48633,#48634,#48635,#48636,#48637,#48638,#48639,#48640,#48641,
#48642,#48643,#48644,#48645,#48646,#48647,#48648,#48649,#48650,#48651,#48652,
#48653,#48654,#48655,#48656,#48657,#48658,#48659,#48660,#48661,#48662,#48663,
#48664,#48665,#48666,#48667,#48668,#48669,#48670,#48671,#48672,#48673,#48674,
#48675,#48676,#48677,#48678,#48679,#48680,#48681,#48682,#48683,#48684,#48685,
#48686,#48687,#48688,#48689,#48690,#48691,#48692,#48693,#48694,#48695),
 .UNSPECIFIED.,.F.,.F.,(4,3,3,3,3,3,3,3,3,3,3,3,3,3,3,3,3,3,3,3,3,3,3,4),
(91.1061869541041,91.2043419644769,91.3024795334306,91.4006291648835,91.4988897541851,
91.5972075103073,91.6957053368608,91.7738402314764,91.8724383564801,91.9708961392569,
92.0711187070296,92.1693982647577,92.2676448438311,92.3658879268697,92.4675851155119,
92.5659695289307,92.6693231051844,92.7726766814382,92.8712673172517,92.9697241251225,
93.0680663331336,93.16634103844,93.2645927043654,93.3318434563844),
 .UNSPECIFIED.);
#445=B_SPLINE_CURVE_WITH_KNOTS('',3,(#48697,#48698,#48699,#48700,#48701,
#48702,#48703,#48704,#48705,#48706,#48707,#48708,#48709,#48710,#48711,#48712,
#48713,#48714,#48715,#48716,#48717,#48718,#48719,#48720,#48721,#48722,#48723,
#48724,#48725,#48726,#48727,#48728,#48729,#48730,#48731,#48732,#48733,#48734,
#48735,#48736,#48737,#48738,#48739,#48740,#48741,#48742,#48743,#48744,#48745,
#48746,#48747,#48748,#48749,#48750,#48751,#48752,#48753,#48754,#48755,#48756,
#48757,#48758,#48759,#48760,#48761,#48762,#48763,#48764,#48765,#48766),
 .UNSPECIFIED.,.F.,.F.,(4,3,3,3,3,3,3,3,3,3,3,3,3,3,3,3,3,3,3,3,3,3,3,4),
(91.1061869541041,91.2465035596788,91.3090334989568,91.4076316239605,91.5060894067373,
91.6063119745099,91.7045915322381,91.8028381113114,91.90108119435,92.0027783829921,
92.1011627964109,92.2045163726648,92.3078699489186,92.4064680739223,92.5049258566991,
92.6051484244718,92.7034279821999,92.8016745612734,92.8999176443119,93.001614832954,
93.0999992463728,93.2033528226267,93.3067063988805,93.3321733281741),
 .UNSPECIFIED.);
#446=B_SPLINE_CURVE_WITH_KNOTS('',3,(#48767,#48768,#48769,#48770,#48771,
#48772,#48773,#48774,#48775,#48776,#48777,#48778,#48779,#48780,#48781,#48782,
#48783,#48784,#48785,#48786,#48787,#48788,#48789,#48790,#48791,#48792,#48793,
#48794,#48795,#48796,#48797,#48798,#48799,#48800,#48801,#48802,#48803,#48804,
#48805,#48806,#48807,#48808,#48809,#48810,#48811,#48812,#48813,#48814,#48815,
#48816,#48817,#48818,#48819,#48820,#48821,#48822,#48823,#48824,#48825,#48826,
#48827,#48828,#48829,#48830,#48831,#48832,#48833,#48834,#48835,#48836,#48837,
#48838,#48839,#48840,#48841,#48842,#48843,#48844,#48845,#48846,#48847,#48848,
#48849,#48850,#48851,#48852,#48853,#48854,#48855,#48856,#48857,#48858,#48859,
#48860,#48861,#48862,#48863,#48864,#48865,#48866,#48867,#48868,#48869,#48870,
#48871,#48872,#48873,#48874,#48875,#48876,#48877,#48878,#48879,#48880,#48881,
#48882,#48883,#48884,#48885,#48886,#48887,#48888,#48889,#48890,#48891,#48892,
#48893),.UNSPECIFIED.,.F.,.F.,(4,3,3,3,3,3,3,3,3,3,3,3,3,3,3,3,3,3,3,3,
3,3,3,3,3,3,3,3,3,3,3,3,3,3,3,3,3,3,3,3,3,3,4),(87.0482730717182,87.1466828354347,
87.2452617559357,87.3136876991093,87.412285824113,87.5107436068897,87.6109661746624,
87.7092457323906,87.807492311464,87.9057353945024,88.0074325831446,88.1058169965634,
88.2091705728173,88.3125241490712,88.4111222740749,88.5095800568517,88.6098026246243,
88.7080821823525,88.8063287614258,88.9045718444643,89.0062690331065,89.1046534465253,
89.2080070227792,89.311360599033,89.4099587240367,89.5084165068134,89.6086390745861,
89.7069186323142,89.8051652113876,89.9034082944261,90.0051054830683,90.1034898964871,
90.206843472741,90.3101970489949,90.409695787095,90.5067185530535,90.6036495481492,
90.70051989818,90.801936662084,90.8988156754798,90.9957205549588,91.0927209416413,
91.1061869537961),.UNSPECIFIED.);
#447=B_SPLINE_CURVE_WITH_KNOTS('',3,(#48899,#48900,#48901,#48902,#48903,
#48904,#48905,#48906,#48907,#48908,#48909,#48910,#48911,#48912,#48913,#48914,
#48915,#48916,#48917,#48918,#48919,#48920,#48921,#48922,#48923,#48924,#48925,
#48926,#48927,#48928,#48929,#48930,#48931,#48932,#48933,#48934,#48935,#48936,
#48937,#48938,#48939,#48940,#48941,#48942,#48943,#48944,#48945,#48946,#48947,
#48948,#48949,#48950,#48951,#48952,#48953,#48954,#48955,#48956,#48957,#48958,
#48959,#48960,#48961,#48962,#48963,#48964,#48965,#48966,#48967,#48968,#48969,
#48970,#48971,#48972,#48973,#48974,#48975,#48976,#48977,#48978,#48979,#48980,
#48981,#48982,#48983,#48984,#48985,#48986,#48987,#48988,#48989,#48990,#48991,
#48992,#48993,#48994,#48995,#48996,#48997,#48998,#48999,#49000,#49001,#49002,
#49003,#49004,#49005,#49006,#49007,#49008,#49009,#49010,#49011,#49012,#49013,
#49014,#49015,#49016,#49017,#49018,#49019,#49020,#49021,#49022,#49023,#49024,
#49025),.UNSPECIFIED.,.F.,.F.,(4,3,3,3,3,3,3,3,3,3,3,3,3,3,3,3,3,3,3,3,
3,3,3,3,3,3,3,3,3,3,3,3,3,3,3,3,3,3,3,3,3,3,4),(80.7655329641705,80.7866392818957,
80.8852374068994,80.9836951896762,81.0839177574489,81.182197315177,81.2804438942504,
81.3786869772889,81.4803841659311,81.5787685793499,81.6821221556037,81.7854757318576,
81.8840738568613,81.982531639638,82.0827542074107,82.1810337651389,82.2792803442123,
82.3775234272508,82.4792206158929,82.5776050293117,82.6809586055656,82.7843121818195,
82.8829103068232,82.9813680896,83.0815906573726,83.1798702151008,83.2781167941742,
83.3763598772127,83.4780570658549,83.5764414792737,83.6797950555275,83.7831486317814,
83.8817467567851,83.9802045395617,84.0804271073344,84.1787066650626,84.276953244136,
84.3751963271744,84.4768935158166,84.5752779292354,84.6786315054893,84.7819850817432,
84.8230016469246),.UNSPECIFIED.);
#448=B_SPLINE_CURVE_WITH_KNOTS('',3,(#49026,#49027,#49028,#49029,#49030,
#49031),.UNSPECIFIED.,.F.,.F.,(4,1,1,4),(84.8230070319889,85.7808215317051,
86.779657981667,87.0497429340083),.UNSPECIFIED.);
#449=B_SPLINE_CURVE_WITH_KNOTS('',3,(#49033,#49034,#49035,#49036,#49037,
#49038,#49039,#49040,#49041,#49042,#49043,#49044,#49045,#49046,#49047,#49048,
#49049,#49050,#49051,#49052,#49053,#49054,#49055,#49056,#49057,#49058,#49059,
#49060,#49061,#49062,#49063,#49064,#49065,#49066,#49067,#49068,#49069,#49070,
#49071,#49072,#49073,#49074,#49075,#49076,#49077,#49078,#49079,#49080,#49081,
#49082,#49083,#49084,#49085,#49086,#49087,#49088,#49089,#49090,#49091,#49092,
#49093,#49094,#49095,#49096,#49097,#49098,#49099,#49100,#49101,#49102),
 .UNSPECIFIED.,.F.,.F.,(4,3,3,3,3,3,3,3,3,3,3,3,3,3,3,3,3,3,3,3,3,3,3,4),
(84.8230016472006,84.9261861619503,85.029664796698,85.133294590709,85.2372126194223,
85.3160147991855,85.4146129241892,85.513070706966,85.6132932747387,85.7115728324668,
85.8098194115402,85.9080624945788,86.0097596832209,86.1081440966398,86.2114976728936,
86.3148512491474,86.4134243290379,86.5118681332251,86.6102123732651,86.7084866565464,
86.8067399239172,86.9049803913521,87.003272709464,87.0482730717182),
 .UNSPECIFIED.);
#450=B_SPLINE_CURVE_WITH_KNOTS('',3,(#49103,#49104,#49105,#49106,#49107,
#49108,#49109,#49110,#49111,#49112,#49113,#49114,#49115,#49116,#49117,#49118,
#49119,#49120,#49121,#49122,#49123,#49124,#49125,#49126,#49127,#49128,#49129,
#49130,#49131,#49132,#49133,#49134,#49135,#49136,#49137,#49138,#49139,#49140,
#49141,#49142,#49143,#49144,#49145,#49146,#49147,#49148,#49149,#49150,#49151,
#49152,#49153,#49154,#49155,#49156,#49157,#49158,#49159,#49160,#49161,#49162,
#49163,#49164,#49165,#49166,#49167,#49168,#49169,#49170,#49171,#49172,#49173,
#49174,#49175,#49176,#49177,#49178,#49179,#49180,#49181,#49182,#49183,#49184,
#49185,#49186,#49187,#49188,#49189,#49190,#49191,#49192,#49193,#49194,#49195,
#49196,#49197,#49198,#49199,#49200,#49201,#49202,#49203,#49204,#49205,#49206,
#49207,#49208,#49209,#49210,#49211,#49212,#49213,#49214,#49215,#49216,#49217,
#49218,#49219,#49220,#49221,#49222,#49223,#49224,#49225,#49226),
 .UNSPECIFIED.,.F.,.F.,(4,3,3,3,3,3,3,3,3,3,3,3,3,3,3,3,3,3,3,3,3,3,3,3,
3,3,3,3,3,3,3,3,3,3,3,3,3,3,3,3,3,4),(80.7658264823238,80.8640676547198,
80.9623198591735,81.0606770182082,81.1590905811291,81.2576716388607,81.320668999338,
81.4192671243417,81.5177249071185,81.6179474748912,81.7162270326193,81.8144736116927,
81.9127166947311,82.0144138833733,82.1127982967922,82.216151873046,82.3195054492999,
82.4181035743036,82.5165613570806,82.6167839248532,82.7150634825814,82.8133100616548,
82.9115531446933,83.0132503333354,83.1116347467542,83.214988323008,83.3183418992618,
83.4169400242655,83.5153978070425,83.6156203748152,83.7138999325434,83.8121465116168,
83.9103895946552,84.0120867832973,84.1104711967161,84.2138247729699,84.3171783492237,
84.420557830251,84.523654386749,84.6265834813182,84.7292989065994,84.8230016469246),
 .UNSPECIFIED.);
#451=B_SPLINE_CURVE_WITH_KNOTS('',3,(#49232,#49233,#49234,#49235,#49236,
#49237,#49238,#49239),.UNSPECIFIED.,.F.,.F.,(4,1,1,1,1,4),(74.4816441296696,
74.7936205821245,75.7924570320864,76.7912934820482,77.7901299320101,78.539816339745),
 .UNSPECIFIED.);
#452=B_SPLINE_CURVE_WITH_KNOTS('',3,(#49240,#49241,#49242,#49243,#49244,
#49245,#49246,#49247,#49248,#49249,#49250,#49251,#49252,#49253,#49254,#49255,
#49256,#49257,#49258,#49259,#49260,#49261,#49262,#49263,#49264,#49265,#49266,
#49267,#49268,#49269,#49270,#49271,#49272,#49273,#49274,#49275,#49276,#49277,
#49278,#49279,#49280,#49281,#49282,#49283,#49284,#49285,#49286,#49287,#49288,
#49289,#49290,#49291,#49292,#49293,#49294,#49295,#49296,#49297,#49298,#49299,
#49300,#49301,#49302,#49303,#49304,#49305,#49306),.UNSPECIFIED.,.F.,.F.,
(4,3,3,3,3,3,3,3,3,3,3,3,3,3,3,3,3,3,3,3,3,3,4),(78.5398164398184,78.6677108218573,
78.788966381972,78.8875645069757,78.9860222897524,79.0862448575251,79.1845244152533,
79.2827709943266,79.3810140773651,79.4827112660073,79.5810956794261,79.68444925568,
79.7878028319339,79.8864023576699,79.9848611556885,80.0832042043516,80.1814836418339,
80.2797289912675,80.3779697355309,80.4762993937765,80.5746716764702,80.6732109328371,
80.7655329641705),.UNSPECIFIED.);
#453=B_SPLINE_CURVE_WITH_KNOTS('',3,(#49308,#49309,#49310,#49311,#49312,
#49313,#49314,#49315,#49316,#49317,#49318,#49319,#49320,#49321,#49322,#49323,
#49324,#49325,#49326,#49327,#49328,#49329,#49330,#49331,#49332,#49333,#49334,
#49335,#49336,#49337,#49338,#49339,#49340,#49341,#49342,#49343,#49344,#49345,
#49346,#49347,#49348,#49349,#49350,#49351,#49352,#49353,#49354,#49355,#49356,
#49357,#49358,#49359,#49360,#49361,#49362,#49363,#49364,#49365,#49366,#49367,
#49368,#49369,#49370,#49371,#49372,#49373,#49374,#49375,#49376,#49377),
 .UNSPECIFIED.,.F.,.F.,(4,3,3,3,3,3,3,3,3,3,3,3,3,3,3,3,3,3,3,3,3,3,3,4),
(78.539816339745,78.6377138097037,78.7346673304385,78.831578691398,78.9284788661294,
79.0271081744506,79.1241353185128,79.2235657089636,79.3229960994143,79.4215942244181,
79.5200520071948,79.6202745749675,79.7185541326956,79.816800711769,79.9150437948075,
80.0167409834497,80.1151253968684,80.2184789731223,80.3218325493762,80.4204382921282,
80.5188792313131,80.6172249291316,80.7155010605353,80.7658264823238),
 .UNSPECIFIED.);
#454=B_SPLINE_CURVE_WITH_KNOTS('',3,(#49378,#49379,#49380,#49381,#49382,
#49383,#49384,#49385),.UNSPECIFIED.,.F.,.F.,(4,1,1,1,1,4),(74.48326306339,
75.3276502995668,76.3264867495287,77.3253231994905,78.3241596494524,78.539816339745),
 .UNSPECIFIED.);
#455=B_SPLINE_CURVE_WITH_KNOTS('',3,(#49391,#49392,#49393,#49394,#49395,
#49396,#49397,#49398,#49399,#49400,#49401,#49402,#49403,#49404,#49405,#49406,
#49407,#49408,#49409,#49410,#49411,#49412,#49413,#49414,#49415,#49416,#49417,
#49418,#49419,#49420,#49421,#49422,#49423,#49424,#49425,#49426,#49427,#49428,
#49429,#49430,#49431,#49432,#49433,#49434,#49435,#49436,#49437,#49438,#49439,
#49440,#49441,#49442,#49443,#49444,#49445,#49446,#49447,#49448,#49449,#49450,
#49451,#49452,#49453,#49454,#49455,#49456,#49457,#49458,#49459,#49460,#49461,
#49462,#49463,#49464,#49465,#49466,#49467,#49468,#49469,#49470,#49471,#49472,
#49473,#49474,#49475,#49476,#49477,#49478,#49479,#49480,#49481,#49482,#49483,
#49484,#49485,#49486,#49487,#49488,#49489,#49490,#49491,#49492,#49493,#49494,
#49495,#49496,#49497,#49498,#49499,#49500,#49501,#49502,#49503,#49504,#49505,
#49506,#49507,#49508,#49509,#49510,#49511,#49512,#49513,#49514),
 .UNSPECIFIED.,.F.,.F.,(4,3,3,3,3,3,3,3,3,3,3,3,3,3,3,3,3,3,3,3,3,3,3,3,
3,3,3,3,3,3,3,3,3,3,3,3,3,3,3,3,3,4),(68.1995885950359,68.2978347616174,
68.3960781115758,68.4972090542702,68.595594464771,68.6980981735621,68.8006018823532,
68.8992000073568,68.9976577901334,69.0978803579061,69.1961599156343,69.2944064947077,
69.3926495777462,69.4943467663884,69.5927311798071,69.6960847560611,69.7994383323151,
69.8980364573188,69.9964942400959,70.0967168078685,70.1949963655966,70.29324294467,
70.3914860277084,70.4931832163506,70.5915676297695,70.6949212060232,70.798274782277,
70.8968729072807,70.9953306900577,71.0955532578304,71.1938328155586,71.292079394632,
71.3903224776701,71.4920196663123,71.5904040797311,71.693757655985,71.7971112322389,
71.9028340905511,72.0081993817375,72.1133399321499,72.2181701837239,72.2566308185779),
 .UNSPECIFIED.);
#456=B_SPLINE_CURVE_WITH_KNOTS('',3,(#49515,#49516,#49517,#49518,#49519,
#49520),.UNSPECIFIED.,.F.,.F.,(4,1,1,4),(72.2566310325654,72.7959476822007,
73.7947841321626,74.4816441296696),.UNSPECIFIED.);
#457=B_SPLINE_CURVE_WITH_KNOTS('',3,(#49522,#49523,#49524,#49525,#49526,
#49527,#49528),.UNSPECIFIED.,.F.,.F.,(4,1,1,1,4),(72.2566310325654,72.3311409496812,
73.329977399643,74.3288138496049,74.48326306339),.UNSPECIFIED.);
#458=B_SPLINE_CURVE_WITH_KNOTS('',3,(#49529,#49530,#49531,#49532,#49533,
#49534,#49535,#49536,#49537,#49538,#49539,#49540,#49541,#49542,#49543,#49544,
#49545,#49546,#49547,#49548,#49549,#49550,#49551,#49552,#49553,#49554,#49555,
#49556,#49557,#49558,#49559,#49560,#49561,#49562,#49563,#49564,#49565,#49566,
#49567,#49568,#49569,#49570,#49571,#49572,#49573,#49574,#49575,#49576,#49577,
#49578,#49579,#49580,#49581,#49582,#49583,#49584,#49585,#49586,#49587,#49588,
#49589,#49590,#49591,#49592,#49593,#49594,#49595,#49596,#49597,#49598,#49599,
#49600,#49601,#49602,#49603,#49604,#49605,#49606,#49607,#49608,#49609,#49610,
#49611,#49612,#49613,#49614,#49615,#49616,#49617,#49618,#49619,#49620,#49621,
#49622,#49623,#49624,#49625,#49626,#49627,#49628,#49629,#49630,#49631,#49632,
#49633,#49634,#49635,#49636,#49637,#49638,#49639,#49640,#49641,#49642,#49643,
#49644,#49645,#49646,#49647,#49648,#49649,#49650,#49651,#49652,#49653,#49654,
#49655),.UNSPECIFIED.,.F.,.F.,(4,3,3,3,3,3,3,3,3,3,3,3,3,3,3,3,3,3,3,3,
3,3,3,3,3,3,3,3,3,3,3,3,3,3,3,3,3,3,3,3,3,3,4),(68.1987515094134,68.2973434667343,
68.3357951498337,68.4343932748374,68.5328510576141,68.6330736253868,68.7313531831149,
68.8295997621883,68.9278428452268,69.029540033869,69.1279244472877,69.2312780235416,
69.3346315997955,69.4332297247992,69.5316875075759,69.6319100753486,69.7301896330768,
69.8284362121502,69.9266792951887,70.0283764838308,70.1267608972497,70.2301144735035,
70.3334680497574,70.4320661747611,70.5305239575378,70.6307465253105,70.7290260830386,
70.827272662112,70.9255157451505,71.0272129337927,71.1255973472115,71.2289509234654,
71.3323044997193,71.4298807240688,71.5273176349421,71.6246428433669,71.721908115062,
71.8191441424516,71.9163815796695,72.013708783522,72.1110862397604,72.2086145464311,
72.2566310325654),.UNSPECIFIED.);
#459=B_SPLINE_CURVE_WITH_KNOTS('',3,(#49661,#49662,#49663,#49664,#49665,
#49666,#49667,#49668),.UNSPECIFIED.,.F.,.F.,(4,1,1,1,1,4),(61.9167164919525,
62.807583182582,63.8064196325439,64.8052560825058,65.8040925324676,65.9734457253857),
 .UNSPECIFIED.);
#460=B_SPLINE_CURVE_WITH_KNOTS('',3,(#49669,#49670,#49671,#49672,#49673,
#49674,#49675,#49676,#49677,#49678,#49679,#49680,#49681,#49682,#49683,#49684,
#49685,#49686,#49687,#49688,#49689,#49690,#49691,#49692,#49693,#49694,#49695,
#49696,#49697,#49698,#49699,#49700,#49701,#49702,#49703,#49704,#49705,#49706,
#49707,#49708,#49709,#49710,#49711,#49712,#49713,#49714,#49715,#49716,#49717,
#49718,#49719,#49720,#49721,#49722,#49723,#49724,#49725,#49726,#49727,#49728,
#49729,#49730,#49731,#49732,#49733,#49734,#49735,#49736,#49737,#49738),
 .UNSPECIFIED.,.F.,.F.,(4,3,3,3,3,3,3,3,3,3,3,3,3,3,3,3,3,3,3,3,3,3,3,4),
(65.9734457253857,66.0704340596177,66.1673127975357,66.2641328887558,66.3609254267909,
66.4577214670338,66.5546134226801,66.6515579893416,66.7486626585398,66.8029289824295,
66.9015271074333,66.9999848902101,67.1002074579827,67.1984870157109,67.2967335947843,
67.3949766778227,67.4966738664648,67.5950582798836,67.6984118561375,67.8017654323914,
67.9012212230525,67.9996662408954,68.0996274179656,68.1995885950359),
 .UNSPECIFIED.);
#461=B_SPLINE_CURVE_WITH_KNOTS('',3,(#49740,#49741,#49742,#49743,#49744,
#49745,#49746,#49747,#49748,#49749,#49750,#49751,#49752,#49753,#49754,#49755,
#49756,#49757,#49758,#49759,#49760,#49761,#49762,#49763,#49764,#49765,#49766,
#49767,#49768,#49769,#49770,#49771,#49772,#49773,#49774,#49775,#49776,#49777,
#49778,#49779,#49780,#49781,#49782,#49783,#49784,#49785,#49786,#49787,#49788,
#49789,#49790,#49791,#49792,#49793,#49794,#49795,#49796,#49797,#49798,#49799,
#49800,#49801,#49802,#49803,#49804,#49805,#49806,#49807,#49808,#49809),
 .UNSPECIFIED.,.F.,.F.,(4,3,3,3,3,3,3,3,3,3,3,3,3,3,3,3,3,3,3,3,3,3,3,4),
(65.9734457256204,66.0848798050741,66.1968635637043,66.309495782683,66.3381222499099,
66.4367203749136,66.5351781576904,66.6354007254631,66.7336802831912,66.8319268622647,
66.9301699453032,67.0318671339453,67.1302515473642,67.233605123618,67.3369586998718,
67.4355663370597,67.5340045943449,67.6323466348068,67.7306220560096,67.828860384381,
67.9271329658739,68.0254205103649,68.1238183935028,68.1987515094134),
 .UNSPECIFIED.);
#462=B_SPLINE_CURVE_WITH_KNOTS('',3,(#49810,#49811,#49812,#49813,#49814,
#49815,#49816,#49817,#49818,#49819,#49820,#49821,#49822,#49823,#49824,#49825,
#49826,#49827,#49828,#49829,#49830,#49831,#49832,#49833,#49834,#49835,#49836,
#49837,#49838,#49839,#49840,#49841,#49842,#49843,#49844,#49845,#49846,#49847,
#49848,#49849,#49850,#49851,#49852,#49853,#49854,#49855,#49856,#49857,#49858,
#49859,#49860,#49861,#49862,#49863,#49864,#49865,#49866,#49867,#49868,#49869,
#49870,#49871,#49872,#49873,#49874,#49875,#49876,#49877,#49878,#49879,#49880,
#49881,#49882,#49883,#49884,#49885,#49886,#49887,#49888,#49889,#49890,#49891,
#49892,#49893,#49894,#49895,#49896,#49897,#49898,#49899,#49900,#49901,#49902,
#49903,#49904,#49905,#49906,#49907,#49908,#49909,#49910,#49911,#49912,#49913,
#49914,#49915,#49916,#49917,#49918,#49919,#49920,#49921,#49922,#49923,#49924,
#49925,#49926,#49927,#49928,#49929,#49930,#49931,#49932,#49933,#49934,#49935,
#49936),.UNSPECIFIED.,.F.,.F.,(4,3,3,3,3,3,3,3,3,3,3,3,3,3,3,3,3,3,3,3,
3,3,3,3,3,3,3,3,3,3,3,3,3,3,3,3,3,3,3,3,3,3,4),(61.9158792692003,62.0141406113804,
62.1125120186739,62.2109478385454,62.3095423735334,62.3427764500624,62.4413745750661,
62.5398323578429,62.6400549256156,62.7383344833437,62.8365810624171,62.9348241454556,
63.0365213340978,63.1349057475167,63.2382593237705,63.3416129000243,63.440211025028,
63.5386688078047,63.6388913755774,63.7371709333055,63.835417512379,63.9336605954173,
64.0353577840595,64.1337421974783,64.2370957737322,64.3404493499862,64.43904747499,
64.5375052577664,64.6377278255391,64.7360073832672,64.8342539623404,64.9324970453787,
65.0341942340211,65.1325786474399,65.235932223694,65.339285799948,65.4384637976082,
65.53749807745,65.6364173808604,65.7352455972605,65.8340208922139,65.932784900221,
65.9734457253857),.UNSPECIFIED.);
#463=B_SPLINE_CURVE_WITH_KNOTS('',3,(#49942,#49943,#49944,#49945,#49946,
#49947,#49948,#49949,#49950,#49951,#49952,#49953,#49954,#49955,#49956,#49957,
#49958,#49959,#49960,#49961,#49962,#49963,#49964,#49965,#49966,#49967,#49968,
#49969,#49970,#49971,#49972,#49973,#49974,#49975,#49976,#49977,#49978,#49979,
#49980,#49981,#49982,#49983,#49984,#49985,#49986,#49987,#49988,#49989,#49990,
#49991,#49992,#49993,#49994,#49995,#49996,#49997,#49998,#49999,#50000,#50001,
#50002,#50003,#50004,#50005,#50006,#50007,#50008,#50009,#50010,#50011,#50012,
#50013,#50014,#50015,#50016,#50017,#50018,#50019,#50020,#50021,#50022,#50023,
#50024,#50025,#50026,#50027,#50028,#50029,#50030,#50031,#50032,#50033,#50034,
#50035,#50036,#50037,#50038,#50039,#50040,#50041,#50042,#50043,#50044,#50045,
#50046,#50047,#50048,#50049,#50050,#50051,#50052,#50053,#50054,#50055,#50056,
#50057,#50058,#50059,#50060,#50061,#50062,#50063,#50064,#50065),
 .UNSPECIFIED.,.F.,.F.,(4,3,3,3,3,3,3,3,3,3,3,3,3,3,3,3,3,3,3,3,3,3,3,3,
3,3,3,3,3,3,3,3,3,3,3,3,3,3,3,3,3,4),(55.6323252039848,55.7308982682604,
55.8157280328489,55.9143261578526,56.0127839406293,56.113006508402,56.2112860661301,
56.3095326452035,56.407775728242,56.5094729168842,56.607857330303,56.7112109065569,
56.8145644828108,56.9131626078145,57.0116203905912,57.1118429583639,57.2101225160921,
57.3083690951655,57.4066121782039,57.5083093668461,57.6066937802649,57.7100473565188,
57.8134009327726,57.9119990577763,58.010456840553,58.1106794083257,58.2089589660538,
58.3072055451272,58.4054486281657,58.5071458168079,58.6055302302267,58.7088838064806,
58.8122373827345,58.9094791608007,59.0070768179764,59.1040671063404,59.2009981633325,
59.2979009849178,59.3959908432399,59.4929780422907,59.5916192302484,59.6902604182062),
 .UNSPECIFIED.);
#464=B_SPLINE_CURVE_WITH_KNOTS('',3,(#50066,#50067,#50068,#50069,#50070,
#50071,#50072),.UNSPECIFIED.,.F.,.F.,(4,1,1,1,4),(59.6902604182062,59.8110738326964,
60.8099102826583,61.8087467326201,61.9167164919525),.UNSPECIFIED.);
#465=B_SPLINE_CURVE_WITH_KNOTS('',3,(#50074,#50075,#50076,#50077,#50078,
#50079,#50080,#50081,#50082,#50083,#50084,#50085,#50086,#50087,#50088,#50089,
#50090,#50091,#50092,#50093,#50094,#50095,#50096,#50097,#50098,#50099,#50100,
#50101,#50102,#50103,#50104,#50105,#50106,#50107,#50108,#50109,#50110,#50111,
#50112,#50113,#50114,#50115,#50116,#50117,#50118,#50119,#50120,#50121,#50122,
#50123,#50124,#50125,#50126,#50127,#50128,#50129,#50130,#50131,#50132,#50133,
#50134,#50135,#50136,#50137,#50138,#50139,#50140,#50141,#50142,#50143),
 .UNSPECIFIED.,.F.,.F.,(4,3,3,3,3,3,3,3,3,3,3,3,3,3,3,3,3,3,3,3,3,3,3,4),
(59.6902604182062,59.7886341730559,59.8869985815967,59.985382791999,60.0838846667639,
60.182449929213,60.2811933482967,60.3451035501387,60.4437016751424,60.5421594579193,
60.6423820256919,60.74066158342,60.8389081624934,60.9371512455319,61.038848434174,
61.1372328475928,61.2405864238467,61.3439400001005,61.4425291322752,61.5409847704257,
61.6393272818741,61.7376024228517,61.8358589218591,61.9158792692003),
 .UNSPECIFIED.);
#466=B_SPLINE_CURVE_WITH_KNOTS('',3,(#50144,#50145,#50146,#50147,#50148,
#50149,#50150,#50151,#50152,#50153,#50154,#50155,#50156,#50157,#50158,#50159,
#50160,#50161,#50162,#50163,#50164,#50165,#50166,#50167,#50168,#50169,#50170,
#50171,#50172,#50173,#50174,#50175,#50176,#50177,#50178,#50179,#50180,#50181,
#50182,#50183,#50184,#50185,#50186,#50187,#50188,#50189,#50190,#50191,#50192,
#50193,#50194,#50195,#50196,#50197,#50198,#50199,#50200,#50201,#50202,#50203,
#50204,#50205,#50206,#50207,#50208,#50209,#50210,#50211,#50212,#50213,#50214,
#50215,#50216,#50217,#50218,#50219,#50220,#50221,#50222,#50223,#50224,#50225,
#50226,#50227,#50228,#50229,#50230,#50231,#50232,#50233,#50234,#50235,#50236,
#50237,#50238,#50239,#50240,#50241,#50242,#50243,#50244,#50245,#50246,#50247,
#50248,#50249,#50250,#50251,#50252,#50253,#50254,#50255,#50256,#50257,#50258,
#50259,#50260,#50261,#50262,#50263,#50264,#50265,#50266,#50267),
 .UNSPECIFIED.,.F.,.F.,(4,3,3,3,3,3,3,3,3,3,3,3,3,3,3,3,3,3,3,3,3,3,3,3,
3,3,3,3,3,3,3,3,3,3,3,3,3,3,3,3,3,4),(55.6334625497945,55.7317495942871,
55.8299992378273,55.9282409671961,56.0265042526908,56.1248784994769,56.2233186098339,
56.3219159047901,56.3497577502912,56.4483558752948,56.5468136580714,56.6470362258441,
56.7453157835723,56.8435623626456,56.9418054456839,57.0435026343262,57.141887047745,
57.245240623999,57.348594200253,57.4471923252566,57.5456501080335,57.6458726758062,
57.7441522335342,57.8423988126075,57.9406418956461,58.0423390842883,58.1407234977071,
58.244077073961,58.3474306502149,58.4460287752185,58.5444865579957,58.6447091257683,
58.7429886834964,58.8412352625698,58.9394783456081,59.0411755342503,59.1395599476692,
59.242913523923,59.3462671001768,59.4608829140302,59.5755716660047,59.6902604179793),
 .UNSPECIFIED.);
#467=B_SPLINE_CURVE_WITH_KNOTS('',3,(#50273,#50274,#50275,#50276,#50277,
#50278,#50279,#50280),.UNSPECIFIED.,.F.,.F.,(4,1,1,1,1,4),(49.3495871973939,
49.8227093330776,50.8215457830395,51.8203822330014,52.8192186829633,53.4070751110266),
 .UNSPECIFIED.);
#468=B_SPLINE_CURVE_WITH_KNOTS('',3,(#50281,#50282,#50283,#50284,#50285,
#50286,#50287,#50288,#50289,#50290,#50291,#50292,#50293,#50294,#50295,#50296,
#50297,#50298,#50299,#50300,#50301,#50302,#50303,#50304,#50305,#50306,#50307,
#50308,#50309,#50310,#50311,#50312,#50313,#50314,#50315,#50316,#50317,#50318,
#50319,#50320,#50321,#50322,#50323,#50324,#50325,#50326,#50327,#50328,#50329,
#50330,#50331,#50332,#50333,#50334,#50335,#50336,#50337,#50338,#50339,#50340,
#50341,#50342,#50343,#50344,#50345,#50346,#50347,#50348,#50349,#50350),
 .UNSPECIFIED.,.F.,.F.,(4,3,3,3,3,3,3,3,3,3,3,3,3,3,3,3,3,3,3,3,3,3,3,4),
(53.4070755243672,53.5149520672774,53.6231638610727,53.7318758460234,53.8180551329251,
53.9166532579288,54.0151110407056,54.1153336084783,54.2136131662065,54.3118597452798,
54.4101028283184,54.5118000169606,54.6101844303794,54.7135380066332,54.816891582887,
54.9188207855242,55.0172568627063,55.1155965180651,55.2138693495665,55.3121048834225,
55.4103643248623,55.5086391375978,55.6069975898681,55.6323252039848),
 .UNSPECIFIED.);
#469=B_SPLINE_CURVE_WITH_KNOTS('',3,(#50352,#50353,#50354,#50355,#50356,
#50357,#50358,#50359,#50360,#50361,#50362,#50363,#50364,#50365,#50366,#50367,
#50368,#50369,#50370,#50371,#50372,#50373,#50374,#50375,#50376,#50377,#50378,
#50379,#50380,#50381,#50382,#50383,#50384,#50385,#50386,#50387,#50388,#50389,
#50390,#50391,#50392,#50393,#50394,#50395,#50396,#50397,#50398,#50399,#50400,
#50401,#50402,#50403,#50404,#50405,#50406,#50407,#50408,#50409,#50410,#50411,
#50412,#50413,#50414,#50415,#50416,#50417,#50418,#50419,#50420,#50421),
 .UNSPECIFIED.,.F.,.F.,(4,3,3,3,3,3,3,3,3,3,3,3,3,3,3,3,3,3,3,3,3,3,3,4),
(53.4070751110266,53.5048543854907,53.602498370777,53.7000367768844,53.7975186210123,
53.894974367796,53.9924344477701,54.0899931990352,54.1876041339862,54.2853815723757,
54.3520848503674,54.4506829753711,54.5491407581478,54.6493633259204,54.7476428836486,
54.8458894627221,54.9441325457606,55.0458297344028,55.1442141478216,55.2475677240754,
55.3509213003293,55.4495112354527,55.5479503969119,55.6334625497945),
 .UNSPECIFIED.);
#470=B_SPLINE_CURVE_WITH_KNOTS('',3,(#50422,#50423,#50424,#50425,#50426,
#50427,#50428,#50429,#50430),.UNSPECIFIED.,.F.,.F.,(4,1,1,1,1,1,4),(49.3496771194667,
49.3579026005581,50.3567390505199,51.3555755004818,52.3544119504437,53.3532484004055,
53.4070751110266),.UNSPECIFIED.);
#471=B_SPLINE_CURVE_WITH_KNOTS('',3,(#50436,#50437,#50438,#50439,#50440,
#50441,#50442,#50443,#50444,#50445,#50446,#50447,#50448,#50449,#50450,#50451,
#50452,#50453,#50454,#50455,#50456,#50457,#50458,#50459,#50460,#50461,#50462,
#50463,#50464,#50465,#50466,#50467,#50468,#50469,#50470,#50471,#50472,#50473,
#50474,#50475,#50476,#50477,#50478,#50479,#50480,#50481,#50482,#50483,#50484,
#50485,#50486,#50487,#50488,#50489,#50490,#50491,#50492,#50493,#50494,#50495,
#50496,#50497,#50498,#50499,#50500,#50501,#50502,#50503,#50504,#50505,#50506,
#50507,#50508,#50509,#50510,#50511,#50512,#50513,#50514,#50515,#50516,#50517,
#50518,#50519,#50520,#50521,#50522,#50523,#50524,#50525,#50526,#50527,#50528,
#50529,#50530,#50531,#50532,#50533,#50534,#50535,#50536,#50537,#50538,#50539,
#50540,#50541,#50542,#50543,#50544,#50545,#50546,#50547,#50548,#50549,#50550,
#50551,#50552,#50553,#50554,#50555,#50556,#50557,#50558,#50559),
 .UNSPECIFIED.,.F.,.F.,(4,3,3,3,3,3,3,3,3,3,3,3,3,3,3,3,3,3,3,3,3,3,3,3,
3,3,3,3,3,3,3,3,3,3,3,3,3,3,3,3,3,4),(43.0671358448511,43.1654506943593,
43.263714257863,43.3619560390805,43.4602055127591,43.5585579544468,43.6569637991359,
43.755540573341,43.8296906333064,43.9282887583115,44.0267465410897,44.126969108862,
44.2252486665916,44.3234952456664,44.4217383287064,44.5234355173468,44.6218199307671,
44.7251735070177,44.8285270832683,44.9271252082715,45.0255829910477,45.1258055588205,
45.2240851165482,45.3223316956211,45.4205747786592,45.5222719673019,45.6206563807203,
45.7240099569752,45.8273635332301,45.9259616582337,46.0244194410103,46.124642008783,
46.222921566511,46.3211681455842,46.4194112286227,46.521108417265,46.6194928306837,
46.7228464069379,46.826199983192,46.9466622822371,47.0654828012677,47.1238896269617),
 .UNSPECIFIED.);
#472=B_SPLINE_CURVE_WITH_KNOTS('',3,(#50560,#50561,#50562,#50563,#50564,
#50565),.UNSPECIFIED.,.F.,.F.,(4,1,1,4),(47.123889803847,47.8250364331539,
48.8238728831158,49.3495871973939),.UNSPECIFIED.);
#473=B_SPLINE_CURVE_WITH_KNOTS('',3,(#50567,#50568,#50569,#50570,#50571,
#50572),.UNSPECIFIED.,.F.,.F.,(4,1,1,4),(47.1238901027736,47.3602297006343,
48.3590661505962,49.3496771194667),.UNSPECIFIED.);
#474=B_SPLINE_CURVE_WITH_KNOTS('',3,(#50573,#50574,#50575,#50576,#50577,
#50578,#50579,#50580,#50581,#50582,#50583,#50584,#50585,#50586,#50587,#50588,
#50589,#50590,#50591,#50592,#50593,#50594,#50595,#50596,#50597,#50598,#50599,
#50600,#50601,#50602,#50603,#50604,#50605,#50606,#50607,#50608,#50609,#50610,
#50611,#50612,#50613,#50614,#50615,#50616,#50617,#50618,#50619,#50620,#50621,
#50622,#50623,#50624,#50625,#50626,#50627,#50628,#50629,#50630,#50631,#50632,
#50633,#50634,#50635,#50636,#50637,#50638,#50639,#50640,#50641,#50642,#50643,
#50644,#50645,#50646,#50647,#50648,#50649,#50650,#50651,#50652,#50653,#50654,
#50655,#50656,#50657,#50658,#50659,#50660,#50661,#50662,#50663,#50664,#50665,
#50666,#50667,#50668,#50669,#50670,#50671,#50672,#50673,#50674,#50675,#50676,
#50677,#50678,#50679,#50680,#50681,#50682,#50683,#50684,#50685,#50686,#50687,
#50688,#50689,#50690,#50691,#50692,#50693,#50694,#50695,#50696),
 .UNSPECIFIED.,.F.,.F.,(4,3,3,3,3,3,3,3,3,3,3,3,3,3,3,3,3,3,3,3,3,3,3,3,
3,3,3,3,3,3,3,3,3,3,3,3,3,3,3,3,3,4),(43.0660207895399,43.1644088973725,
43.2646463990797,43.3648839007868,43.4634820258002,43.5619398085866,43.6621623763569,
43.7604419340951,43.8586885131787,43.9569315962275,44.0586287848578,44.157013198287,
44.2603667745178,44.3637203507487,44.4623184757498,44.5607762585239,44.6609988262972,
44.7592783840226,44.8575249630933,44.955768046129,45.0574652347744,45.1558496481904,
45.2592032244505,45.3625568007106,45.4611549257132,45.5596127084887,45.6598352762616,
45.7581148339886,45.8563614130607,45.9546044960983,46.0563016847418,46.1546860981594,
46.2580396744159,46.3613932506724,46.4587199838046,46.5559210250953,46.6530274701202,
46.750070296518,46.8471124553623,46.9441490048067,47.0412721236587,47.123889803847),
 .UNSPECIFIED.);
#475=B_SPLINE_CURVE_WITH_KNOTS('',3,(#50702,#50703,#50704,#50705,#50706,
#50707,#50708,#50709,#50710,#50711,#50712,#50713,#50714,#50715,#50716,#50717,
#50718,#50719,#50720,#50721,#50722,#50723,#50724,#50725,#50726,#50727,#50728,
#50729,#50730,#50731,#50732,#50733,#50734,#50735,#50736,#50737,#50738,#50739,
#50740,#50741,#50742,#50743,#50744,#50745,#50746,#50747,#50748,#50749,#50750,
#50751,#50752,#50753,#50754,#50755,#50756,#50757,#50758,#50759,#50760,#50761,
#50762,#50763,#50764,#50765,#50766,#50767,#50768,#50769,#50770,#50771,#50772,
#50773,#50774,#50775,#50776,#50777,#50778,#50779,#50780,#50781,#50782,#50783,
#50784,#50785,#50786,#50787,#50788,#50789,#50790,#50791,#50792,#50793,#50794,
#50795,#50796,#50797,#50798,#50799,#50800,#50801,#50802,#50803,#50804,#50805,
#50806,#50807,#50808,#50809,#50810,#50811,#50812,#50813,#50814,#50815,#50816,
#50817,#50818,#50819,#50820,#50821,#50822,#50823,#50824,#50825,#50826,#50827,
#50828),.UNSPECIFIED.,.F.,.F.,(4,3,3,3,3,3,3,3,3,3,3,3,3,3,3,3,3,3,3,3,
3,3,3,3,3,3,3,3,3,3,3,3,3,3,3,3,3,3,3,3,3,3,4),(36.7830721323901,36.8378354835733,
36.9364336084865,37.034891391171,37.1351139589666,37.2333935165987,37.3316400955749,
37.4298831785151,37.5315803672701,37.629964780589,37.7333183570621,37.8366719335352,
37.9352700586078,38.0337278414543,38.1339504092097,38.2322299670095,38.3304765461551,
38.4287196292662,38.5304168178239,38.6288012313158,38.7321548074064,38.835508383497,
38.9341065084864,39.0325642912488,39.1327868590251,39.2310664167388,39.3293129957978,
39.4275560788219,39.5292532674811,39.6276376808858,39.7309912571723,39.8343448334589,
39.9329429584521,40.0314007412181,40.1316233089935,40.2299028667104,40.3281494457725,
40.4263925287994,40.5280897174548,40.6264741308618,40.7298277071413,40.8331812834208,
40.8407044966674),.UNSPECIFIED.);
#476=B_SPLINE_CURVE_WITH_KNOTS('',3,(#50829,#50830,#50831,#50832,#50833,
#50834,#50835,#50836,#50837,#50838,#50839,#50840,#50841,#50842,#50843,#50844,
#50845,#50846,#50847,#50848,#50849,#50850,#50851,#50852,#50853,#50854,#50855,
#50856,#50857,#50858,#50859,#50860,#50861,#50862,#50863,#50864,#50865,#50866,
#50867,#50868,#50869,#50870,#50871,#50872,#50873,#50874,#50875,#50876,#50877,
#50878,#50879,#50880,#50881,#50882,#50883,#50884,#50885,#50886,#50887,#50888,
#50889,#50890,#50891,#50892,#50893,#50894,#50895,#50896,#50897,#50898),
 .UNSPECIFIED.,.F.,.F.,(4,3,3,3,3,3,3,3,3,3,3,3,3,3,3,3,3,3,3,3,3,3,3,4),
(40.8407044969197,40.93917053872,41.0374964280042,41.1368115911765,41.2349607512895,
41.3330774110131,41.4311912274065,41.5313978539005,41.6296531901077,41.7308354617452,
41.8320177333826,41.9306158583837,42.029073641158,42.1292962089313,42.2275757666567,
42.3258223457274,42.4240654287631,42.5257626174084,42.6241470308245,42.7275006070845,
42.8308541833445,42.9294559188132,43.0279051778277,43.0671358448511),
 .UNSPECIFIED.);
#477=B_SPLINE_CURVE_WITH_KNOTS('',3,(#50900,#50901,#50902,#50903,#50904,
#50905,#50906,#50907,#50908,#50909,#50910,#50911,#50912,#50913,#50914,#50915,
#50916,#50917,#50918,#50919,#50920,#50921,#50922,#50923,#50924,#50925,#50926,
#50927,#50928,#50929,#50930,#50931,#50932,#50933,#50934,#50935,#50936,#50937,
#50938,#50939,#50940,#50941,#50942,#50943,#50944,#50945,#50946,#50947,#50948,
#50949,#50950,#50951,#50952,#50953,#50954,#50955,#50956,#50957,#50958,#50959,
#50960,#50961,#50962,#50963,#50964,#50965,#50966,#50967,#50968,#50969),
 .UNSPECIFIED.,.F.,.F.,(4,3,3,3,3,3,3,3,3,3,3,3,3,3,3,3,3,3,3,3,3,3,3,4),
(40.8407044966674,40.942531041993,41.0487010317105,41.1508691915792,41.2531658485542,
41.3556785603229,41.3672110008631,41.4658091258526,41.5642669086151,41.6644894763913,
41.7627690341051,41.8610156131642,41.9592586961886,42.0609558848477,42.1593402982525,
42.2626938745387,42.3660474508249,42.46462340533,42.5630692109006,42.6614145831978,
42.7625661347833,42.8608128972949,42.9634168434174,43.0660207895399),
 .UNSPECIFIED.);
#478=B_SPLINE_CURVE_WITH_KNOTS('',3,(#50970,#50971,#50972,#50973,#50974,
#50975,#50976,#50977),.UNSPECIFIED.,.F.,.F.,(4,1,1,1,1,4),(36.7838197976209,
37.3718652010156,38.3707016509774,39.3695381009393,40.3683745509012,40.8407024149681),
 .UNSPECIFIED.);
#479=B_SPLINE_CURVE_WITH_KNOTS('',3,(#50983,#50984,#50985,#50986,#50987,
#50988,#50989,#50990,#50991,#50992,#50993,#50994,#50995,#50996,#50997,#50998,
#50999,#51000,#51001,#51002,#51003,#51004,#51005,#51006,#51007,#51008,#51009,
#51010,#51011,#51012,#51013,#51014,#51015,#51016,#51017,#51018,#51019,#51020,
#51021,#51022,#51023,#51024,#51025,#51026,#51027,#51028,#51029,#51030,#51031,
#51032,#51033,#51034,#51035,#51036,#51037,#51038,#51039,#51040,#51041,#51042,
#51043,#51044,#51045,#51046,#51047,#51048,#51049,#51050,#51051,#51052,#51053,
#51054,#51055,#51056,#51057,#51058,#51059,#51060,#51061,#51062,#51063,#51064,
#51065,#51066,#51067,#51068,#51069,#51070,#51071,#51072,#51073,#51074,#51075,
#51076,#51077,#51078,#51079,#51080,#51081,#51082,#51083,#51084,#51085,#51086,
#51087,#51088,#51089,#51090,#51091,#51092,#51093,#51094,#51095,#51096,#51097,
#51098,#51099,#51100,#51101,#51102,#51103,#51104,#51105,#51106,#51107,#51108,
#51109),.UNSPECIFIED.,.F.,.F.,(4,3,3,3,3,3,3,3,3,3,3,3,3,3,3,3,3,3,3,3,
3,3,3,3,3,3,3,3,3,3,3,3,3,3,3,3,3,3,3,3,3,3,4),(30.499739219623,30.5981024448967,
30.696525650912,30.7951123611512,30.844816783802,30.9434149029152,31.041872679698,
31.1420952489563,31.2403748004794,31.3386213732825,31.4368644499935,31.5385616459361,
31.6369460529487,31.7402996433563,31.8436532337639,31.9422513619745,32.0407091479983,
32.1409317149643,32.2392112760146,32.3374578584309,32.4357009448286,32.5373981295529,
32.6357825463377,32.7391361150317,32.8424896837258,32.9410878085145,33.0395455910813,
33.1397681589071,33.2380477164403,33.3362942953245,33.4345373781801,33.536234567057,
33.6346189803103,33.737972556999,33.8413261336877,33.9390973941501,34.0367388270535,
34.1342810926874,34.2317547370029,34.3292101035722,34.4266554953253,34.5241539309012,
34.5575191894878),.UNSPECIFIED.);
#480=B_SPLINE_CURVE_WITH_KNOTS('',3,(#51110,#51111,#51112,#51113,#51114,
#51115,#51116,#51117,#51118,#51119,#51120,#51121,#51122,#51123,#51124,#51125,
#51126,#51127,#51128,#51129,#51130,#51131,#51132,#51133,#51134,#51135,#51136,
#51137,#51138,#51139,#51140,#51141,#51142,#51143,#51144,#51145,#51146,#51147,
#51148,#51149,#51150,#51151,#51152,#51153,#51154,#51155,#51156,#51157,#51158,
#51159,#51160,#51161,#51162,#51163,#51164,#51165,#51166,#51167,#51168,#51169,
#51170,#51171,#51172,#51173,#51174,#51175,#51176,#51177,#51178,#51179),
 .UNSPECIFIED.,.F.,.F.,(4,3,3,3,3,3,3,3,3,3,3,3,3,3,3,3,3,3,3,3,3,3,3,4),
(34.5575191897594,34.6782345503606,34.8009387396023,34.8401625836495,34.9387607091287,
35.0372184923872,35.1374410600402,35.2357206182622,35.3339671978328,35.4322102813714,
35.5339074694314,35.6322918833521,35.7356454584817,35.8389990336114,35.9376008413508,
36.0360613066033,36.1344037647036,36.2326817408433,36.3309247589448,36.4291623016121,
36.5274785677211,36.6258371036476,36.7243383500819,36.7830721323901),
 .UNSPECIFIED.);
#481=B_SPLINE_CURVE_WITH_KNOTS('',3,(#51181,#51182,#51183,#51184,#51185,
#51186),.UNSPECIFIED.,.F.,.F.,(4,1,1,4),(34.5575241472562,35.3741923010918,
36.3730287510537,36.7838197976209),.UNSPECIFIED.);
#482=B_SPLINE_CURVE_WITH_KNOTS('',3,(#51187,#51188,#51189,#51190,#51191,
#51192,#51193,#51194,#51195,#51196,#51197,#51198,#51199,#51200,#51201,#51202,
#51203,#51204,#51205,#51206,#51207,#51208,#51209,#51210,#51211,#51212,#51213,
#51214,#51215,#51216,#51217,#51218,#51219,#51220,#51221,#51222,#51223,#51224,
#51225,#51226,#51227,#51228,#51229,#51230,#51231,#51232,#51233,#51234,#51235,
#51236,#51237,#51238,#51239,#51240,#51241,#51242,#51243,#51244,#51245,#51246,
#51247,#51248,#51249,#51250,#51251,#51252,#51253,#51254,#51255,#51256,#51257,
#51258,#51259,#51260,#51261,#51262,#51263,#51264,#51265,#51266,#51267,#51268,
#51269,#51270,#51271,#51272,#51273,#51274,#51275,#51276,#51277,#51278,#51279,
#51280,#51281,#51282,#51283,#51284,#51285,#51286,#51287,#51288,#51289,#51290,
#51291,#51292,#51293,#51294,#51295,#51296,#51297,#51298,#51299,#51300,#51301,
#51302,#51303,#51304,#51305,#51306,#51307,#51308,#51309,#51310),
 .UNSPECIFIED.,.F.,.F.,(4,3,3,3,3,3,3,3,3,3,3,3,3,3,3,3,3,3,3,3,3,3,3,3,
3,3,3,3,3,3,3,3,3,3,3,3,3,3,3,3,3,4),(30.5006744564005,30.5991052602797,
30.6974320559243,30.7957024047894,30.8939458184504,30.9921917748654,31.0905375599031,
31.1889321215594,31.2875030626886,31.3788465012443,31.4774446472214,31.5759024512158,
31.6761250137146,31.7744045931048,31.8726511939587,31.9708942988676,32.0725914619522,
32.170975897242,32.2743294242241,32.3776829512062,32.4762810765974,32.5747388598281,
32.6749614274956,32.7732409858386,32.8714875655859,32.9697306493566,33.0714278373095,
33.1698122515998,33.2731658263839,33.3765194011681,33.4751175203064,33.5735752971148,
33.6737978663667,33.7720774179164,33.8703239907463,33.9685670674843,34.0702642633957,
34.1686486704357,34.2720022607828,34.3753558511299,34.52385598093,34.5575191894878),
 .UNSPECIFIED.);
#483=B_SPLINE_CURVE_WITH_KNOTS('',3,(#51316,#51317,#51318,#51319,#51320,
#51321,#51322,#51323),.UNSPECIFIED.,.F.,.F.,(4,1,1,1,1,4),(24.2176478200484,
24.8517980840308,25.8506345339927,26.8494709839545,27.8483074339164,28.2743284148063),
 .UNSPECIFIED.);
#484=B_SPLINE_CURVE_WITH_KNOTS('',3,(#51324,#51325,#51326,#51327,#51328,
#51329,#51330,#51331,#51332,#51333,#51334,#51335,#51336,#51337,#51338,#51339,
#51340,#51341,#51342,#51343,#51344,#51345,#51346,#51347,#51348,#51349,#51350,
#51351,#51352,#51353,#51354,#51355,#51356,#51357,#51358,#51359,#51360,#51361,
#51362,#51363,#51364,#51365,#51366,#51367,#51368,#51369,#51370,#51371,#51372,
#51373,#51374,#51375,#51376,#51377,#51378,#51379,#51380,#51381,#51382,#51383,
#51384,#51385,#51386,#51387,#51388,#51389,#51390,#51391,#51392,#51393),
 .UNSPECIFIED.,.F.,.F.,(4,3,3,3,3,3,3,3,3,3,3,3,3,3,3,3,3,3,3,3,3,3,3,4),
(28.2743338823082,28.3746245106389,28.4749734038845,28.5754886320393,28.6760922702991,
28.7769068624285,28.8471438838783,28.9457420299505,29.044199834041,29.1444223965159,
29.2427019760043,29.3409485769571,29.4391916819651,29.5408888449339,29.6392732803231,
29.7426268070816,29.8459803338402,29.9445606477207,30.0430096057647,30.1413569295324,
30.2396381186448,30.3378792535309,30.4361386871605,30.499739219623),
 .UNSPECIFIED.);
#485=B_SPLINE_CURVE_WITH_KNOTS('',3,(#51395,#51396,#51397,#51398,#51399,
#51400,#51401,#51402,#51403,#51404,#51405,#51406,#51407,#51408,#51409,#51410,
#51411,#51412,#51413,#51414,#51415,#51416,#51417,#51418,#51419,#51420,#51421,
#51422,#51423,#51424,#51425,#51426,#51427,#51428,#51429,#51430,#51431,#51432,
#51433,#51434,#51435,#51436,#51437,#51438,#51439,#51440,#51441,#51442,#51443,
#51444,#51445,#51446,#51447,#51448,#51449,#51450,#51451,#51452,#51453,#51454,
#51455,#51456,#51457,#51458,#51459,#51460,#51461,#51462,#51463,#51464),
 .UNSPECIFIED.,.F.,.F.,(4,3,3,3,3,3,3,3,3,3,3,3,3,3,3,3,3,3,3,3,3,3,3,4),
(28.2743338823082,28.3823371513587,28.480935409995,28.5793933278136,28.679615862002,
28.7778955572416,28.8761422744467,28.9743854960547,29.0760825223712,29.1744670740333,
29.277820337677,29.3811736013206,29.479771742719,29.5782295425603,29.6784521061506,
29.7767316824742,29.8749782806757,29.9732213833518,30.0749185503344,30.1733029844702,
30.2766565178763,30.3800100512824,30.4786103666909,30.5006744564005),
 .UNSPECIFIED.);
#486=B_SPLINE_CURVE_WITH_KNOTS('',3,(#51465,#51466,#51467,#51468,#51469,
#51470,#51471,#51472,#51473,#51474,#51475,#51476,#51477,#51478,#51479,#51480,
#51481,#51482,#51483,#51484,#51485,#51486,#51487,#51488,#51489,#51490,#51491,
#51492,#51493,#51494,#51495,#51496,#51497,#51498,#51499,#51500,#51501,#51502,
#51503,#51504,#51505,#51506,#51507,#51508,#51509,#51510,#51511,#51512,#51513,
#51514,#51515,#51516,#51517,#51518,#51519,#51520,#51521,#51522,#51523,#51524,
#51525,#51526,#51527,#51528,#51529,#51530,#51531,#51532,#51533,#51534,#51535,
#51536,#51537,#51538,#51539,#51540,#51541,#51542,#51543,#51544,#51545,#51546,
#51547,#51548,#51549,#51550,#51551,#51552,#51553,#51554,#51555,#51556,#51557,
#51558,#51559,#51560,#51561,#51562,#51563,#51564,#51565,#51566,#51567,#51568,
#51569,#51570,#51571,#51572,#51573,#51574,#51575,#51576,#51577,#51578,#51579,
#51580,#51581,#51582,#51583,#51584,#51585,#51586,#51587,#51588,#51589,#51590,
#51591),.UNSPECIFIED.,.F.,.F.,(4,3,3,3,3,3,3,3,3,3,3,3,3,3,3,3,3,3,3,3,
3,3,3,3,3,3,3,3,3,3,3,3,3,3,3,3,3,3,3,3,3,3,4),(24.2164091248765,24.3149891714194,
24.3869913515112,24.4855869806887,24.584042229485,24.6842654259835,24.7825423743751,
24.8807863216562,24.9790267538739,25.0807270157737,25.1791087577961,25.2824682796346,
25.3858278014731,25.484426744909,25.5828853535715,25.6831077158044,25.781388111632,
25.8796355315209,25.9778794569755,26.0795756555903,26.1779609067728,26.2813125791038,
26.3846642514349,26.4832625887837,26.5817205899964,26.6819431039214,26.7802228935229,
26.8784697089924,26.9767130326531,27.078409949839,27.1767946120345,27.2801476567156,
27.3835007013968,27.4808124357131,27.5800026165089,27.6770619123618,27.7740624152157,
27.8710350591815,27.971859764906,28.0689211638456,28.1660361055543,28.2632831538734,
28.2743338820794),.UNSPECIFIED.);
#487=B_SPLINE_CURVE_WITH_KNOTS('',3,(#51597,#51598,#51599,#51600,#51601,
#51602),.UNSPECIFIED.,.F.,.F.,(4,1,1,4),(15.707963267949,16.3962997518162,
17.3951362017781,17.9335273566036),.UNSPECIFIED.);
#488=B_SPLINE_CURVE_WITH_KNOTS('',3,(#51604,#51605,#51606,#51607,#51608),
 .UNSPECIFIED.,.F.,.F.,(4,1,4),(14.3986268518925,15.3974633018543,15.707963267949),
 .UNSPECIFIED.);
#489=B_SPLINE_CURVE_WITH_KNOTS('',3,(#51612,#51613,#51614,#51615,#51616,
#51617,#51618,#51619,#51620,#51621,#51622,#51623,#51624,#51625,#51626,#51627,
#51628,#51629,#51630,#51631,#51632,#51633,#51634,#51635,#51636,#51637,#51638,
#51639,#51640,#51641,#51642,#51643,#51644,#51645,#51646,#51647,#51648,#51649,
#51650,#51651,#51652,#51653,#51654,#51655,#51656,#51657,#51658,#51659,#51660,
#51661,#51662,#51663,#51664,#51665,#51666,#51667,#51668,#51669),
 .UNSPECIFIED.,.F.,.F.,(4,3,3,3,3,3,3,3,3,3,3,3,3,3,3,3,3,3,3,4),(13.8757070305518,
13.9742335824856,14.0726198317922,14.1714715508697,14.2696802764454,14.3678558944916,
14.4660279816071,14.5653793823083,14.6636893819281,14.7635614831701,14.8634335844121,
14.9606976623845,15.0578044029831,15.1548229005499,15.2517842045426,15.3487192918042,
15.4457083561665,15.542724156859,15.6398692496992,15.707963267949),
 .UNSPECIFIED.);
#490=B_SPLINE_CURVE_WITH_KNOTS('',3,(#51670,#51671,#51672,#51673,#51674,
#51675,#51676),.UNSPECIFIED.,.F.,.F.,(4,1,1,1,4),(15.707963267949,15.8622700343739,
16.8611064843358,17.8599429342977,17.9342415884722),.UNSPECIFIED.);
#491=B_SPLINE_CURVE_WITH_KNOTS('',3,(#51682,#51683,#51684,#51685,#51686,
#51687,#51688,#51689),.UNSPECIFIED.,.F.,.F.,(4,1,1,1,1,4),(181.295997133577,
181.669120728045,182.667957178007,183.666793627969,184.665630077931,185.353966561798),
 .UNSPECIFIED.);
#492=B_SPLINE_CURVE_WITH_KNOTS('',3,(#51691,#51692,#51693,#51694,#51695),
 .UNSPECIFIED.,.F.,.F.,(4,1,4),(185.353966561798,185.664466527893,186.663302977854),
 .UNSPECIFIED.);
#493=B_SPLINE_CURVE_WITH_KNOTS('',3,(#51699,#51700,#51701,#51702,#51703,
#51704,#51705,#51706,#51707,#51708,#51709,#51710,#51711,#51712,#51713,#51714,
#51715,#51716,#51717,#51718,#51719,#51720,#51721,#51722,#51723,#51724,#51725,
#51726,#51727,#51728,#51729,#51730,#51731,#51732,#51733,#51734,#51735,#51736,
#51737,#51738,#51739,#51740,#51741,#51742,#51743,#51744,#51745,#51746,#51747,
#51748,#51749,#51750,#51751,#51752,#51753,#51754,#51755,#51756),
 .UNSPECIFIED.,.F.,.F.,(4,3,3,3,3,3,3,3,3,3,3,3,3,3,3,3,3,3,3,4),(185.353966561798,
185.451129857721,185.548173538225,185.645152135629,185.742096642157,185.839038005082,
185.936068670734,186.033145886574,186.130383559583,186.198496245335,186.297011743078,
186.39538923924,186.494243434233,186.592449062934,186.690623713446,186.78879696123,
186.88815342072,186.986469795236,187.086346297213,187.186222799189),
 .UNSPECIFIED.);
#494=B_SPLINE_CURVE_WITH_KNOTS('',3,(#51757,#51758,#51759,#51760,#51761,
#51762,#51763,#51764),.UNSPECIFIED.,.F.,.F.,(4,1,1,1,1,4),(181.2971675537,
182.203150445487,183.201986895449,184.200823345411,185.199659795373,185.353966561798),
 .UNSPECIFIED.);
#495=B_SPLINE_CURVE_WITH_KNOTS('',3,(#51770,#51771,#51772,#51773,#51774,
#51775,#51776,#51777,#51778,#51779,#51780,#51781,#51782,#51783,#51784,#51785,
#51786,#51787,#51788,#51789,#51790,#51791,#51792,#51793,#51794,#51795,#51796,
#51797,#51798,#51799,#51800,#51801,#51802,#51803,#51804,#51805,#51806,#51807,
#51808,#51809,#51810,#51811,#51812,#51813,#51814,#51815,#51816,#51817,#51818,
#51819,#51820,#51821,#51822,#51823,#51824,#51825,#51826,#51827,#51828,#51829,
#51830,#51831,#51832,#51833,#51834,#51835,#51836,#51837,#51838,#51839,#51840,
#51841,#51842,#51843,#51844,#51845,#51846,#51847,#51848,#51849,#51850,#51851,
#51852,#51853,#51854,#51855,#51856,#51857,#51858,#51859,#51860,#51861,#51862,
#51863,#51864,#51865,#51866,#51867,#51868,#51869,#51870,#51871,#51872,#51873,
#51874,#51875,#51876,#51877,#51878,#51879,#51880,#51881,#51882,#51883,#51884,
#51885,#51886,#51887,#51888,#51889,#51890,#51891,#51892,#51893),
 .UNSPECIFIED.,.F.,.F.,(4,3,3,3,3,3,3,3,3,3,3,3,3,3,3,3,3,3,3,3,3,3,3,3,
3,3,3,3,3,3,3,3,3,3,3,3,3,3,3,3,3,4),(175.013888660471,175.112152321306,
175.210394808164,175.308645594357,175.406999706945,175.50540776602,175.6039861128,
175.676102028274,175.774697485907,175.873152598171,175.973375833179,176.071652731782,
176.169896661679,176.268137108901,176.369837451234,176.468219288705,176.57157888347,
176.674938478236,176.77353909221,176.871999348327,176.972221295811,177.070503271432,
177.168752242674,177.266997689187,177.36869199894,177.467078681016,177.570426804607,
177.673774928198,177.772377764499,177.870840302866,177.971061687278,178.069346073991,
178.167597498754,178.265845437704,178.367536922818,178.465926167544,178.569268772851,
178.672611378159,178.782250111505,178.891545462336,179.000249339659,179.070781030153),
 .UNSPECIFIED.);
#496=B_SPLINE_CURVE_WITH_KNOTS('',3,(#51894,#51895,#51896,#51897,#51898,
#51899),.UNSPECIFIED.,.F.,.F.,(4,1,1,4),(179.070781254618,179.671447828121,
180.670284278083,181.295997133577),.UNSPECIFIED.);
#497=B_SPLINE_CURVE_WITH_KNOTS('',3,(#51901,#51902,#51903,#51904,#51905,
#51906,#51907),.UNSPECIFIED.,.F.,.F.,(4,1,1,1,4),(179.070781254618,179.206641095602,
180.205477545564,181.204313995525,181.2971675537),.UNSPECIFIED.);
#498=B_SPLINE_CURVE_WITH_KNOTS('',3,(#51908,#51909,#51910,#51911,#51912,
#51913,#51914,#51915),.UNSPECIFIED.,.F.,.F.,(4,1,1,1,1,4),(175.012544821303,
175.211295295754,176.210131745716,177.208968195678,178.20780464564,179.070781254618),
 .UNSPECIFIED.);
#499=B_SPLINE_CURVE_WITH_KNOTS('',3,(#51921,#51922,#51923,#51924,#51925,
#51926,#51927,#51928,#51929,#51930,#51931,#51932,#51933,#51934,#51935,#51936,
#51937,#51938,#51939,#51940,#51941,#51942,#51943,#51944,#51945,#51946,#51947,
#51948,#51949,#51950,#51951,#51952,#51953,#51954,#51955,#51956,#51957,#51958,
#51959,#51960,#51961,#51962,#51963,#51964,#51965,#51966,#51967,#51968,#51969,
#51970,#51971,#51972,#51973,#51974,#51975,#51976,#51977,#51978,#51979,#51980,
#51981,#51982,#51983,#51984,#51985,#51986,#51987,#51988,#51989,#51990,#51991,
#51992,#51993,#51994,#51995,#51996,#51997,#51998,#51999,#52000,#52001,#52002,
#52003,#52004,#52005,#52006,#52007,#52008,#52009,#52010,#52011,#52012,#52013,
#52014,#52015,#52016,#52017,#52018,#52019,#52020,#52021,#52022,#52023,#52024,
#52025,#52026,#52027,#52028,#52029,#52030,#52031,#52032,#52033,#52034,#52035,
#52036,#52037,#52038,#52039,#52040,#52041,#52042,#52043,#52044),
 .UNSPECIFIED.,.F.,.F.,(4,3,3,3,3,3,3,3,3,3,3,3,3,3,3,3,3,3,3,3,3,3,3,3,
3,3,3,3,3,3,3,3,3,3,3,3,3,3,3,3,3,4),(168.730499549008,168.829027791897,
168.927431101866,169.025741410082,169.124002504523,169.222243885976,169.320495028123,
169.41885037296,169.517260979166,169.615840378079,169.683083328503,169.781681404542,
169.880139138361,169.980361718374,170.078641227507,170.176887758226,170.27513079321,
170.376828039524,170.475212406123,170.578566092293,170.681919778464,170.780517924866,
170.878975728651,170.979198291123,171.077477868767,171.17572446731,171.273967569349,
171.375664734118,171.474049165187,171.577402696807,171.680756228426,171.779354490553,
171.877812411242,171.978034944635,172.076314641203,172.17456135916,172.272804580942,
172.374501605303,172.472886155702,172.576239417045,172.679592678388,172.787595947439),
 .UNSPECIFIED.);
#500=B_SPLINE_CURVE_WITH_KNOTS('',3,(#52045,#52046,#52047,#52048,#52049,
#52050,#52051,#52052,#52053,#52054,#52055,#52056,#52057,#52058,#52059,#52060,
#52061,#52062,#52063,#52064,#52065,#52066,#52067,#52068,#52069,#52070,#52071,
#52072,#52073,#52074,#52075,#52076,#52077,#52078,#52079,#52080,#52081,#52082,
#52083,#52084,#52085,#52086,#52087,#52088,#52089,#52090,#52091,#52092,#52093,
#52094,#52095,#52096,#52097,#52098,#52099,#52100,#52101,#52102,#52103,#52104,
#52105,#52106,#52107,#52108,#52109,#52110,#52111,#52112,#52113,#52114,#52115,
#52116,#52117),.UNSPECIFIED.,.F.,.F.,(4,3,3,3,3,3,3,3,3,3,3,3,3,3,3,3,3,
3,3,3,3,3,3,3,4),(172.787595947668,172.884841558603,172.984040004821,173.081071836984,
173.178059268517,173.275033212281,173.375882191298,173.472980624789,173.57014496826,
173.66745840562,173.67842912835,173.777027506535,173.875485539983,173.975708044774,
174.073987845308,174.172234663756,174.270477982445,174.372174881412,174.470559518906,
174.573912548609,174.677265578312,174.77584482842,174.874301068252,174.972645515065,
175.013888660471),.UNSPECIFIED.);
#501=B_SPLINE_CURVE_WITH_KNOTS('',3,(#52119,#52120,#52121,#52122,#52123,
#52124),.UNSPECIFIED.,.F.,.F.,(4,1,1,4),(172.787601414694,173.21362239583,
174.212458845792,175.012544821303),.UNSPECIFIED.);
#502=B_SPLINE_CURVE_WITH_KNOTS('',3,(#52125,#52126,#52127,#52128,#52129,
#52130,#52131,#52132,#52133,#52134,#52135,#52136,#52137,#52138,#52139,#52140,
#52141,#52142,#52143,#52144,#52145,#52146,#52147,#52148,#52149,#52150,#52151,
#52152,#52153,#52154,#52155,#52156,#52157,#52158,#52159,#52160,#52161,#52162,
#52163,#52164,#52165,#52166,#52167,#52168,#52169,#52170,#52171,#52172,#52173,
#52174,#52175,#52176,#52177,#52178,#52179,#52180,#52181,#52182,#52183,#52184,
#52185,#52186,#52187,#52188,#52189,#52190,#52191,#52192,#52193,#52194,#52195,
#52196,#52197,#52198,#52199,#52200,#52201,#52202,#52203,#52204,#52205,#52206,
#52207,#52208,#52209,#52210,#52211,#52212,#52213,#52214,#52215,#52216,#52217,
#52218,#52219,#52220,#52221,#52222,#52223,#52224,#52225,#52226,#52227,#52228,
#52229,#52230,#52231,#52232,#52233,#52234,#52235,#52236,#52237,#52238,#52239,
#52240,#52241,#52242,#52243,#52244,#52245,#52246,#52247,#52248),
 .UNSPECIFIED.,.F.,.F.,(4,3,3,3,3,3,3,3,3,3,3,3,3,3,3,3,3,3,3,3,3,3,3,3,
3,3,3,3,3,3,3,3,3,3,3,3,3,3,3,3,3,4),(168.73021510062,168.828460568105,
168.926805276369,169.025197909693,169.12376794625,169.218276595983,169.316874714607,
169.41533249101,169.515555060377,169.613834611791,169.712081184585,169.810324261387,
169.912021457527,170.01040586488,170.113759455413,170.217113045945,170.315711171923,
170.414168955615,170.514391523152,170.612671081648,170.710917661432,170.809160745125,
170.910857932821,171.009242346748,171.112595921327,171.215949495907,171.314547642568,
171.413005447104,171.513228009449,171.611507589026,171.709754189934,171.807997294764,
171.90969445754,172.008078892422,172.111432419146,172.214785945869,172.315617765325,
172.416285943672,172.516781875576,172.617176498836,172.717484580328,172.787595947439),
 .UNSPECIFIED.);
#503=B_SPLINE_CURVE_WITH_KNOTS('',3,(#52254,#52255,#52256,#52257,#52258,
#52259,#52260,#52261),.UNSPECIFIED.,.F.,.F.,(4,1,1,1,1,4),(162.446146734229,
162.691228178769,163.690064628731,164.688901078693,165.687737528655,166.504405683232),
 .UNSPECIFIED.);
#504=B_SPLINE_CURVE_WITH_KNOTS('',3,(#52262,#52263,#52264,#52265,#52266,
#52267,#52268,#52269,#52270,#52271,#52272,#52273,#52274,#52275,#52276,#52277,
#52278,#52279,#52280,#52281,#52282,#52283,#52284,#52285,#52286,#52287,#52288,
#52289,#52290,#52291,#52292,#52293,#52294,#52295,#52296,#52297,#52298,#52299,
#52300,#52301,#52302,#52303,#52304,#52305,#52306,#52307,#52308,#52309,#52310,
#52311,#52312,#52313,#52314,#52315,#52316,#52317,#52318,#52319,#52320,#52321,
#52322,#52323,#52324,#52325,#52326,#52327,#52328,#52329,#52330,#52331),
 .UNSPECIFIED.,.F.,.F.,(4,3,3,3,3,3,3,3,3,3,3,3,3,3,3,3,3,3,3,3,3,3,3,4),
(166.504410640259,166.652910770227,166.686573978617,166.785172097216,166.883629873594,
166.983852442967,167.082131994355,167.180378567125,167.278621643903,167.380318840072,
167.478703247402,167.58205683799,167.685410428579,167.784008554554,167.882466338243,
167.98268890578,168.080968464272,168.179215044053,168.277458127742,168.379155315442,
168.477539729364,168.580893303952,168.684246878541,168.730499549008),
 .UNSPECIFIED.);
#505=B_SPLINE_CURVE_WITH_KNOTS('',3,(#52333,#52334,#52335,#52336,#52337,
#52338,#52339,#52340,#52341,#52342,#52343,#52344,#52345,#52346,#52347,#52348,
#52349,#52350,#52351,#52352,#52353,#52354,#52355,#52356,#52357,#52358,#52359,
#52360,#52361,#52362,#52363,#52364,#52365,#52366,#52367,#52368,#52369,#52370,
#52371,#52372,#52373,#52374,#52375,#52376,#52377,#52378,#52379,#52380,#52381,
#52382,#52383,#52384,#52385,#52386,#52387,#52388,#52389,#52390,#52391,#52392,
#52393,#52394,#52395,#52396,#52397,#52398,#52399,#52400,#52401,#52402,#52403,
#52404,#52405),.UNSPECIFIED.,.F.,.F.,(4,3,3,3,3,3,3,3,3,3,3,3,3,3,3,3,3,
3,3,3,3,3,3,3,4),(166.504410640259,166.6019131263,166.699371433809,166.79681599036,
166.894277201724,166.991846173228,167.089478292237,167.187269535439,167.220603696059,
167.319201820915,167.417659603535,167.517882171346,167.616161728898,167.714408307788,
167.812651390637,167.914348579483,168.012732992698,168.116086569359,168.219440146021,
168.318036793094,168.421081369976,168.519419921282,168.617691702015,168.715928374415,
168.73021510062),.UNSPECIFIED.);
#506=B_SPLINE_CURVE_WITH_KNOTS('',3,(#52406,#52407,#52408,#52409,#52410,
#52411,#52412,#52413,#52414,#52415,#52416,#52417,#52418,#52419,#52420,#52421,
#52422,#52423,#52424,#52425,#52426,#52427,#52428,#52429,#52430,#52431,#52432,
#52433,#52434,#52435,#52436,#52437,#52438,#52439,#52440,#52441,#52442,#52443,
#52444,#52445,#52446,#52447,#52448,#52449,#52450,#52451,#52452,#52453,#52454,
#52455,#52456,#52457,#52458,#52459,#52460,#52461,#52462,#52463,#52464,#52465,
#52466,#52467,#52468,#52469,#52470,#52471,#52472,#52473,#52474,#52475,#52476,
#52477,#52478,#52479,#52480,#52481,#52482,#52483,#52484,#52485,#52486,#52487,
#52488,#52489,#52490,#52491,#52492,#52493,#52494,#52495,#52496,#52497,#52498,
#52499,#52500,#52501,#52502,#52503,#52504,#52505,#52506,#52507,#52508,#52509,
#52510,#52511,#52512,#52513,#52514,#52515,#52516,#52517,#52518,#52519,#52520,
#52521,#52522,#52523,#52524,#52525,#52526,#52527,#52528,#52529),
 .UNSPECIFIED.,.F.,.F.,(4,3,3,3,3,3,3,3,3,3,3,3,3,3,3,3,3,3,3,3,3,3,3,3,
3,3,3,3,3,3,3,3,3,3,3,3,3,3,3,3,3,4),(162.447662236975,162.545987533319,
162.644257027658,162.742500230488,162.840746619266,162.939093233869,163.03748920276,
163.136060860489,163.225257896212,163.323856021116,163.422313803793,163.522536371591,
163.620815929221,163.719062508197,163.817305591139,163.919002779898,164.017387193223,
164.120740769699,164.224094346174,164.322692471118,164.421150253833,164.521372821621,
164.619652379285,164.717898958294,164.816142041267,164.917839229985,165.016223643337,
165.119577219737,165.222930796136,165.321528921635,165.419986704909,165.520209272558,
165.618488830783,165.716735410353,165.814978493886,165.916675681939,166.015060095843,
166.11841367097,166.221767246097,166.34459987441,166.465474953157,166.504410639987),
 .UNSPECIFIED.);
#507=B_SPLINE_CURVE_WITH_KNOTS('',3,(#52535,#52536,#52537,#52538,#52539,
#52540,#52541,#52542,#52543,#52544,#52545,#52546,#52547,#52548,#52549,#52550,
#52551,#52552,#52553,#52554,#52555,#52556,#52557,#52558,#52559,#52560,#52561,
#52562,#52563,#52564,#52565,#52566,#52567,#52568,#52569,#52570,#52571,#52572,
#52573,#52574,#52575,#52576,#52577,#52578,#52579,#52580,#52581,#52582,#52583,
#52584,#52585,#52586,#52587,#52588,#52589,#52590,#52591,#52592,#52593,#52594,
#52595,#52596,#52597,#52598,#52599,#52600,#52601,#52602,#52603,#52604,#52605,
#52606,#52607,#52608,#52609,#52610,#52611,#52612,#52613,#52614,#52615,#52616,
#52617,#52618,#52619,#52620,#52621,#52622,#52623,#52624,#52625,#52626,#52627,
#52628,#52629,#52630,#52631,#52632,#52633,#52634,#52635,#52636,#52637,#52638,
#52639,#52640,#52641,#52642,#52643,#52644,#52645,#52646,#52647,#52648,#52649,
#52650,#52651,#52652,#52653,#52654,#52655,#52656,#52657,#52658,#52659,#52660,
#52661),.UNSPECIFIED.,.F.,.F.,(4,3,3,3,3,3,3,3,3,3,3,3,3,3,3,3,3,3,3,3,
3,3,3,3,3,3,3,3,3,3,3,3,3,3,3,3,3,3,3,3,3,3,4),(156.163987595307,156.262228639747,
156.360486901622,156.458853695073,156.557282451664,156.655872548919,156.698209478998,
156.796807604012,156.895265386799,156.995487954569,157.093767512308,157.192014091392,
157.29025717444,157.39195436307,157.490338776499,157.59369235273,157.69704592896,
157.795644053952,157.894101836717,157.994324404493,158.092603962209,158.190850541271,
158.289093624298,158.390790812954,158.489175226362,158.592528802642,158.695882378922,
158.794480503912,158.892938286675,158.993160854451,159.091440412165,159.189686991224,
159.287930074247,159.389627262907,159.488011676311,159.591365252598,159.694718828884,
159.797216560019,159.903218753284,160.005303397592,160.107256278837,160.209067828956,
160.22122533308),.UNSPECIFIED.);
#508=B_SPLINE_CURVE_WITH_KNOTS('',3,(#52662,#52663,#52664,#52665,#52666,
#52667),.UNSPECIFIED.,.F.,.F.,(4,1,1,4),(160.221227414878,160.693555278846,
161.692391728808,162.446146734229),.UNSPECIFIED.);
#509=B_SPLINE_CURVE_WITH_KNOTS('',3,(#52669,#52670,#52671,#52672,#52673,
#52674,#52675,#52676,#52677,#52678,#52679,#52680,#52681,#52682,#52683,#52684,
#52685,#52686,#52687,#52688,#52689,#52690,#52691,#52692,#52693,#52694,#52695,
#52696,#52697,#52698,#52699,#52700,#52701,#52702,#52703,#52704,#52705,#52706,
#52707,#52708,#52709,#52710,#52711,#52712,#52713,#52714,#52715,#52716,#52717,
#52718,#52719,#52720,#52721,#52722,#52723,#52724,#52725,#52726,#52727,#52728,
#52729,#52730,#52731,#52732,#52733,#52734,#52735,#52736,#52737,#52738,#52739,
#52740,#52741),.UNSPECIFIED.,.F.,.F.,(4,3,3,3,3,3,3,3,3,3,3,3,3,3,3,3,3,
3,3,3,3,3,3,3,4),(160.22122533308,160.228748546326,160.327346671318,160.425804454083,
160.526027021859,160.624306579575,160.722553158637,160.820796241665,160.92249343032,
161.020877843728,161.124231420008,161.227584996288,161.326183121278,161.424640904041,
161.524863471817,161.623143029531,161.72138960859,161.819632691614,161.921329880273,
162.019714293678,162.123067869964,162.22642144625,162.325027405982,162.423481500059,
162.447662236975),.UNSPECIFIED.);
#510=B_SPLINE_CURVE_WITH_KNOTS('',3,(#52742,#52743,#52744,#52745,#52746,
#52747,#52748,#52749,#52750,#52751,#52752,#52753,#52754,#52755,#52756,#52757,
#52758,#52759,#52760,#52761,#52762,#52763,#52764,#52765,#52766,#52767,#52768,
#52769,#52770,#52771,#52772,#52773,#52774,#52775,#52776,#52777,#52778,#52779,
#52780,#52781,#52782,#52783,#52784,#52785,#52786,#52787,#52788,#52789,#52790,
#52791,#52792,#52793,#52794,#52795,#52796,#52797,#52798,#52799,#52800,#52801,
#52802,#52803,#52804,#52805,#52806,#52807,#52808,#52809,#52810,#52811,#52812,
#52813,#52814,#52815,#52816,#52817,#52818,#52819,#52820,#52821,#52822,#52823,
#52824,#52825,#52826,#52827,#52828,#52829,#52830,#52831,#52832,#52833,#52834,
#52835,#52836,#52837,#52838,#52839,#52840,#52841,#52842,#52843,#52844,#52845,
#52846,#52847,#52848,#52849,#52850,#52851,#52852,#52853,#52854,#52855,#52856,
#52857,#52858,#52859,#52860,#52861,#52862,#52863,#52864,#52865),
 .UNSPECIFIED.,.F.,.F.,(4,3,3,3,3,3,3,3,3,3,3,3,3,3,3,3,3,3,3,3,3,3,3,3,
3,3,3,3,3,3,3,3,3,3,3,3,3,3,3,3,3,4),(156.163531931712,156.233402746479,
156.332000871484,156.430458654262,156.530681222035,156.628960779764,156.727207358839,
156.825450441879,156.927147630519,157.025532043939,157.12888562019,157.232239196441,
157.330837321443,157.429295104219,157.529517671992,157.627797229718,157.72604380879,
157.824286891828,157.925984080471,158.024368493889,158.127722070145,158.231075646402,
158.329673771403,158.428131554177,158.528354121951,158.626633679676,158.724880258747,
158.823123341783,158.924820530428,159.023204943844,159.126558520104,159.229912096364,
159.328378576654,159.426704810661,159.526019875932,159.624169149678,159.722285836342,
159.820399593048,159.920606027993,160.018861091251,160.120043212039,160.221225332828),
 .UNSPECIFIED.);
#511=B_SPLINE_CURVE_WITH_KNOTS('',3,(#52871,#52872,#52873,#52874,#52875,
#52876,#52877,#52878),.UNSPECIFIED.,.F.,.F.,(4,1,1,1,1,4),(149.881541704413,
150.705190779227,151.704027229189,152.702863679151,153.701700129113,153.938039726298),
 .UNSPECIFIED.);
#512=B_SPLINE_CURVE_WITH_KNOTS('',3,(#52879,#52880,#52881,#52882,#52883,
#52884,#52885,#52886,#52887,#52888,#52889,#52890,#52891,#52892,#52893,#52894,
#52895,#52896,#52897,#52898,#52899,#52900,#52901,#52902,#52903,#52904,#52905,
#52906,#52907,#52908,#52909,#52910,#52911,#52912,#52913,#52914,#52915,#52916,
#52917,#52918,#52919,#52920,#52921,#52922,#52923,#52924,#52925,#52926,#52927,
#52928,#52929,#52930,#52931,#52932,#52933,#52934,#52935,#52936,#52937,#52938,
#52939,#52940,#52941,#52942,#52943,#52944,#52945,#52946,#52947,#52948),
 .UNSPECIFIED.,.F.,.F.,(4,3,3,3,3,3,3,3,3,3,3,3,3,3,3,3,3,3,3,3,3,3,3,4),
(153.9380400259,154.035163898234,154.132222574363,154.229246955324,154.326267897773,
154.423381488606,154.520541056366,154.617870832504,154.700536579074,154.799134704076,
154.897592486852,154.997815054625,155.096094612352,155.194341191424,155.292584274461,
155.394281463105,155.492665876522,155.596019452779,155.699373029036,155.79797586222,
155.89641514303,155.9947593991,156.093038592392,156.163987595307),
 .UNSPECIFIED.);
#513=B_SPLINE_CURVE_WITH_KNOTS('',3,(#52950,#52951,#52952,#52953,#52954,
#52955,#52956,#52957,#52958,#52959,#52960,#52961,#52962,#52963,#52964,#52965,
#52966,#52967,#52968,#52969,#52970,#52971,#52972,#52973,#52974,#52975,#52976,
#52977,#52978,#52979,#52980,#52981,#52982,#52983,#52984,#52985,#52986,#52987,
#52988,#52989,#52990,#52991,#52992,#52993,#52994,#52995,#52996,#52997,#52998,
#52999,#53000,#53001,#53002,#53003,#53004,#53005,#53006,#53007,#53008,#53009,
#53010,#53011,#53012,#53013,#53014,#53015,#53016,#53017,#53018,#53019),
 .UNSPECIFIED.,.F.,.F.,(4,3,3,3,3,3,3,3,3,3,3,3,3,3,3,3,3,3,3,3,3,3,3,4),
(153.938040202766,154.056659980235,154.176963650991,154.235729846555,154.334327971559,
154.432785754335,154.533008322108,154.631287879836,154.729534458909,154.827777541948,
154.92947473059,155.027859144009,155.131212720263,155.234566296517,155.33316914801,
155.431630381046,155.529972651698,155.628250049481,155.726492098718,155.82472828193,
155.923038846793,156.021391522283,156.119876942737,156.163531931712),
 .UNSPECIFIED.);
#514=B_SPLINE_CURVE_WITH_KNOTS('',3,(#53020,#53021,#53022,#53023,#53024,
#53025,#53026,#53027),.UNSPECIFIED.,.F.,.F.,(4,1,1,1,1,4),(149.880018495728,
150.240384046707,151.239220496669,152.238056946631,153.236893396593,153.9380400259),
 .UNSPECIFIED.);
#515=B_SPLINE_CURVE_WITH_KNOTS('',3,(#53033,#53034,#53035,#53036,#53037,
#53038,#53039,#53040,#53041,#53042,#53043,#53044,#53045,#53046,#53047,#53048,
#53049,#53050,#53051,#53052,#53053,#53054,#53055,#53056,#53057,#53058,#53059,
#53060,#53061,#53062,#53063,#53064,#53065,#53066,#53067,#53068,#53069,#53070,
#53071,#53072,#53073,#53074,#53075,#53076,#53077,#53078,#53079,#53080,#53081,
#53082,#53083,#53084,#53085,#53086,#53087,#53088,#53089,#53090,#53091,#53092,
#53093,#53094,#53095,#53096,#53097,#53098,#53099,#53100,#53101,#53102,#53103,
#53104,#53105,#53106,#53107,#53108,#53109,#53110,#53111,#53112,#53113,#53114,
#53115,#53116,#53117,#53118,#53119,#53120,#53121,#53122,#53123,#53124,#53125,
#53126,#53127,#53128,#53129,#53130,#53131,#53132,#53133,#53134,#53135,#53136,
#53137,#53138,#53139,#53140,#53141,#53142,#53143,#53144,#53145,#53146,#53147,
#53148,#53149,#53150,#53151,#53152,#53153,#53154,#53155,#53156,#53157,#53158,
#53159),.UNSPECIFIED.,.F.,.F.,(4,3,3,3,3,3,3,3,3,3,3,3,3,3,3,3,3,3,3,3,
3,3,3,3,3,3,3,3,3,3,3,3,3,3,3,3,3,3,3,3,3,3,4),(143.597018511536,143.695621253918,
143.713335629494,143.811933754498,143.910391537274,144.010614105047,144.108893662775,
144.207140241849,144.305383324887,144.407080513529,144.505464926948,144.608818503202,
144.712172079456,144.81077020446,144.909227987236,145.009450555009,145.107730112737,
145.205976691811,145.304219774849,145.405916963491,145.50430137691,145.607654953164,
145.711008529418,145.809606654422,145.908064437198,146.008287004971,146.106566562699,
146.204813141772,146.303056224811,146.404753413453,146.503137826872,146.606491403125,
146.709844979379,146.807643480436,146.905302408374,147.002849316603,147.100335701354,
147.197792033696,147.295248746519,147.3927980835,147.490396206244,147.588155506493,
147.65485471872),.UNSPECIFIED.);
#516=B_SPLINE_CURVE_WITH_KNOTS('',3,(#53160,#53161,#53162,#53163,#53164,
#53165,#53166),.UNSPECIFIED.,.F.,.F.,(4,1,1,1,4),(147.65485471872,147.708681429341,
148.707517879303,149.706354329265,149.881541704413),.UNSPECIFIED.);
#517=B_SPLINE_CURVE_WITH_KNOTS('',3,(#53168,#53169,#53170,#53171,#53172,
#53173),.UNSPECIFIED.,.F.,.F.,(4,1,1,4),(147.65485471872,148.242711146784,
149.241547596746,149.880018495728),.UNSPECIFIED.);
#518=B_SPLINE_CURVE_WITH_KNOTS('',3,(#53174,#53175,#53176,#53177,#53178,
#53179,#53180,#53181,#53182,#53183,#53184,#53185,#53186,#53187,#53188,#53189,
#53190,#53191,#53192,#53193,#53194,#53195,#53196,#53197,#53198,#53199,#53200,
#53201,#53202,#53203,#53204,#53205,#53206,#53207,#53208,#53209,#53210,#53211,
#53212,#53213,#53214,#53215,#53216,#53217,#53218,#53219,#53220,#53221,#53222,
#53223,#53224,#53225,#53226,#53227,#53228,#53229,#53230,#53231,#53232,#53233,
#53234,#53235,#53236,#53237,#53238,#53239,#53240,#53241,#53242,#53243,#53244,
#53245,#53246,#53247,#53248,#53249,#53250,#53251,#53252,#53253,#53254,#53255,
#53256,#53257,#53258,#53259,#53260,#53261,#53262,#53263,#53264,#53265,#53266,
#53267,#53268,#53269,#53270,#53271,#53272,#53273,#53274,#53275,#53276,#53277,
#53278,#53279,#53280,#53281,#53282,#53283,#53284,#53285,#53286,#53287,#53288,
#53289,#53290,#53291,#53292,#53293,#53294,#53295,#53296,#53297),
 .UNSPECIFIED.,.F.,.F.,(4,3,3,3,3,3,3,3,3,3,3,3,3,3,3,3,3,3,3,3,3,3,3,3,
3,3,3,3,3,3,3,3,3,3,3,3,3,3,3,3,3,4),(143.597933925136,143.69619231975,
143.794433374417,143.892686561819,143.99104535005,144.089461531313,144.188044092565,
144.247365346936,144.34596347194,144.444421254716,144.544643822489,144.642923380217,
144.741169959291,144.839413042329,144.941110230972,145.03949464439,145.142848220644,
145.246201796898,145.344799921902,145.443257704679,145.543480272451,145.64175983018,
145.740006409253,145.838249492292,145.939946680934,146.038331094352,146.141684670606,
146.24503824686,146.343636371864,146.442094154641,146.542316722413,146.640596280141,
146.738842859215,146.837085942254,146.938783130896,147.037167544314,147.140521120568,
147.243874696822,147.352569174392,147.460952550046,147.568802109382,147.654854305399),
 .UNSPECIFIED.);
#519=B_SPLINE_CURVE_WITH_KNOTS('',3,(#53303,#53304,#53305,#53306,#53307,
#53308,#53309,#53310,#53311,#53312,#53313,#53314,#53315,#53316,#53317,#53318,
#53319,#53320,#53321,#53322,#53323,#53324,#53325,#53326,#53327,#53328,#53329,
#53330,#53331,#53332,#53333,#53334,#53335,#53336,#53337,#53338,#53339,#53340,
#53341,#53342,#53343,#53344,#53345,#53346,#53347,#53348,#53349,#53350,#53351,
#53352,#53353,#53354,#53355,#53356,#53357,#53358,#53359,#53360,#53361,#53362,
#53363,#53364,#53365,#53366,#53367,#53368,#53369,#53370,#53371,#53372,#53373,
#53374,#53375,#53376,#53377,#53378,#53379,#53380,#53381,#53382,#53383,#53384,
#53385,#53386,#53387,#53388,#53389,#53390,#53391,#53392,#53393,#53394,#53395,
#53396,#53397,#53398,#53399,#53400,#53401,#53402,#53403,#53404,#53405,#53406,
#53407,#53408,#53409,#53410,#53411,#53412,#53413,#53414,#53415,#53416,#53417,
#53418,#53419,#53420,#53421,#53422,#53423,#53424,#53425,#53426),
 .UNSPECIFIED.,.F.,.F.,(4,3,3,3,3,3,3,3,3,3,3,3,3,3,3,3,3,3,3,3,3,3,3,3,
3,3,3,3,3,3,3,3,3,3,3,3,3,3,3,3,3,4),(137.314044096691,137.415612304949,
137.51399694479,137.617156937256,137.720316929723,137.818915054726,137.917372837503,
138.017595405276,138.115874963004,138.214121542077,138.312364625116,138.414061813758,
138.512446227177,138.61579980343,138.719153379684,138.817751504688,138.916209287465,
139.016431855237,139.114711412965,139.212957992039,139.311201075077,139.412898263719,
139.511282677138,139.614636253392,139.717989829646,139.81658795465,139.915045737427,
140.015268305199,140.113547862927,140.211794442001,140.310037525039,140.411734713681,
140.5101191271,140.613472703354,140.716826279608,140.815569227393,140.914173010821,
141.012667061738,141.11108183093,141.209449097701,141.307822396311,141.371669411541),
 .UNSPECIFIED.);
#520=B_SPLINE_CURVE_WITH_KNOTS('',3,(#53427,#53428,#53429,#53430,#53431,
#53432,#53433,#53434,#53435,#53436,#53437,#53438,#53439,#53440,#53441,#53442,
#53443,#53444,#53445,#53446,#53447,#53448,#53449,#53450,#53451,#53452,#53453,
#53454,#53455,#53456,#53457,#53458,#53459,#53460,#53461,#53462,#53463,#53464,
#53465,#53466,#53467,#53468,#53469,#53470,#53471,#53472,#53473,#53474,#53475,
#53476,#53477,#53478,#53479,#53480,#53481,#53482,#53483,#53484,#53485,#53486,
#53487,#53488,#53489,#53490,#53491,#53492,#53493),.UNSPECIFIED.,.F.,.F.,
(4,3,3,3,3,3,3,3,3,3,3,3,3,3,3,3,3,3,3,3,3,3,4),(141.371669411768,141.485016004534,
141.600339367052,141.71566272957,141.814260854574,141.91271863735,142.012941205123,
142.111220762851,142.209467341925,142.307710424963,142.409407613605,142.507792027024,
142.611145603278,142.714499179532,142.813105314795,142.911543009964,143.009885026327,
143.108160960053,143.206400336867,143.304679404128,143.402973649661,143.501391759164,
143.597018511536),.UNSPECIFIED.);
#521=B_SPLINE_CURVE_WITH_KNOTS('',3,(#53495,#53496,#53497,#53498,#53499,
#53500,#53501,#53502,#53503,#53504,#53505,#53506,#53507,#53508,#53509,#53510,
#53511,#53512,#53513,#53514,#53515,#53516,#53517,#53518,#53519,#53520,#53521,
#53522,#53523,#53524,#53525,#53526,#53527,#53528,#53529,#53530,#53531,#53532,
#53533,#53534,#53535,#53536,#53537,#53538,#53539,#53540,#53541,#53542,#53543,
#53544,#53545,#53546,#53547,#53548,#53549,#53550,#53551,#53552,#53553,#53554,
#53555,#53556,#53557,#53558,#53559,#53560,#53561,#53562,#53563,#53564),
 .UNSPECIFIED.,.F.,.F.,(4,3,3,3,3,3,3,3,3,3,3,3,3,3,3,3,3,3,3,3,3,3,3,4),
(141.371669411541,141.468831254161,141.566438903267,141.66339620349,141.760311911022,
141.857216996242,141.955335858934,142.052368429038,142.151030438025,142.249692447012,
142.348290572016,142.446748354792,142.546970922565,142.645250480293,142.743497059367,
142.841740142405,142.943437331047,143.041821744466,143.14517532072,143.248528896974,
143.347104955699,143.445558136373,143.543900701708,143.597933925136),
 .UNSPECIFIED.);
#522=B_SPLINE_CURVE_WITH_KNOTS('',3,(#53565,#53566,#53567,#53568,#53569,
#53570,#53571,#53572),.UNSPECIFIED.,.F.,.F.,(4,1,1,1,1,4),(137.314688078281,
138.254346647165,139.253183097127,140.252019547089,141.250855997051,141.371669411541),
 .UNSPECIFIED.);
#523=B_SPLINE_CURVE_WITH_KNOTS('',3,(#53578,#53579,#53580,#53581,#53582,
#53583,#53584,#53585,#53586,#53587,#53588,#53589,#53590,#53591,#53592,#53593,
#53594,#53595,#53596,#53597,#53598,#53599,#53600,#53601,#53602,#53603,#53604,
#53605,#53606,#53607,#53608,#53609,#53610,#53611,#53612,#53613,#53614,#53615,
#53616,#53617,#53618,#53619,#53620,#53621,#53622,#53623,#53624,#53625,#53626,
#53627,#53628,#53629,#53630,#53631,#53632,#53633,#53634,#53635,#53636,#53637,
#53638,#53639,#53640,#53641,#53642,#53643,#53644,#53645,#53646,#53647,#53648,
#53649,#53650,#53651,#53652,#53653,#53654,#53655,#53656,#53657,#53658,#53659,
#53660,#53661,#53662,#53663,#53664,#53665,#53666,#53667,#53668,#53669,#53670,
#53671,#53672,#53673,#53674,#53675,#53676,#53677,#53678,#53679,#53680,#53681,
#53682,#53683,#53684,#53685,#53686,#53687,#53688,#53689,#53690,#53691,#53692,
#53693,#53694,#53695,#53696,#53697,#53698,#53699,#53700,#53701),
 .UNSPECIFIED.,.F.,.F.,(4,3,3,3,3,3,3,3,3,3,3,3,3,3,3,3,3,3,3,3,3,3,3,3,
3,3,3,3,3,3,3,3,3,3,3,3,3,3,3,3,3,4),(131.031654975012,131.129931714323,
131.228177249718,131.326421062313,131.426640354222,131.525027386608,131.62616280828,
131.727298229951,131.825896354955,131.924354137731,132.024576705504,132.122856263232,
132.221102842306,132.319345925344,132.421043113987,132.519427527405,132.622781103659,
132.726134679913,132.824732804917,132.923190587693,133.023413155466,133.121692713194,
133.219939292268,133.318182375306,133.419879563948,133.518263977367,133.621617553621,
133.724971129875,133.823569254879,133.922027037656,134.022249605428,134.120529163156,
134.21877574223,134.317018825268,134.41871601391,134.517100427329,134.620454003583,
134.723807579837,134.8363385207,134.948409000641,135.059693750753,135.088484104126),
 .UNSPECIFIED.);
#524=B_SPLINE_CURVE_WITH_KNOTS('',3,(#53702,#53703,#53704,#53705,#53706,
#53707,#53708,#53709,#53710,#53711,#53712,#53713,#53714,#53715,#53716,#53717,
#53718,#53719,#53720,#53721,#53722,#53723,#53724,#53725,#53726,#53727,#53728,
#53729,#53730,#53731,#53732,#53733,#53734,#53735,#53736,#53737,#53738,#53739,
#53740,#53741,#53742,#53743,#53744,#53745,#53746,#53747,#53748,#53749,#53750,
#53751,#53752,#53753,#53754,#53755,#53756,#53757,#53758,#53759,#53760,#53761,
#53762,#53763,#53764,#53765,#53766,#53767,#53768,#53769,#53770,#53771),
 .UNSPECIFIED.,.F.,.F.,(4,3,3,3,3,3,3,3,3,3,3,3,3,3,3,3,3,3,3,3,3,3,3,4),
(135.088484104361,135.187254556185,135.286029876603,135.384838499173,135.483776463585,
135.582788468008,135.681976179006,135.722644029799,135.821242154803,135.919699937579,
136.019922505352,136.11820206308,136.216448642154,136.314691725192,136.416388913835,
136.514773327253,136.618126903507,136.721480479761,136.820067256329,136.918521077985,
137.017401832662,137.115677672543,137.214860884617,137.314044096691),
 .UNSPECIFIED.);
#525=B_SPLINE_CURVE_WITH_KNOTS('',3,(#53773,#53774,#53775,#53776,#53777,
#53778,#53779),.UNSPECIFIED.,.F.,.F.,(4,1,1,1,4),(135.088484104361,135.257837297279,
136.256673747241,137.255510197203,137.314688078281),.UNSPECIFIED.);
#526=B_SPLINE_CURVE_WITH_KNOTS('',3,(#53780,#53781,#53782,#53783,#53784,
#53785,#53786,#53787,#53788,#53789,#53790,#53791,#53792,#53793,#53794,#53795,
#53796,#53797,#53798,#53799,#53800,#53801,#53802,#53803,#53804,#53805,#53806,
#53807,#53808,#53809,#53810,#53811,#53812,#53813,#53814,#53815,#53816,#53817,
#53818,#53819,#53820,#53821,#53822,#53823,#53824,#53825,#53826,#53827,#53828,
#53829,#53830,#53831,#53832,#53833,#53834,#53835,#53836,#53837,#53838,#53839,
#53840,#53841,#53842,#53843,#53844,#53845,#53846,#53847,#53848,#53849,#53850,
#53851,#53852,#53853,#53854,#53855,#53856,#53857,#53858,#53859,#53860,#53861,
#53862,#53863,#53864,#53865,#53866,#53867,#53868,#53869,#53870,#53871,#53872,
#53873,#53874,#53875,#53876,#53877,#53878,#53879,#53880,#53881,#53882,#53883,
#53884,#53885,#53886,#53887,#53888,#53889,#53890,#53891,#53892,#53893,#53894,
#53895,#53896,#53897,#53898,#53899,#53900,#53901,#53902,#53903,#53904,#53905,
#53906),.UNSPECIFIED.,.F.,.F.,(4,3,3,3,3,3,3,3,3,3,3,3,3,3,3,3,3,3,3,3,
3,3,3,3,3,3,3,3,3,3,3,3,3,3,3,3,3,3,3,3,3,3,4),(131.030544946366,131.128979442315,
131.227573135221,131.262491497432,131.361089622436,131.459547405213,131.559769972985,
131.658049530713,131.756296109787,131.854539192825,131.956236381468,132.054620794886,
132.15797437114,132.261327947394,132.359926072398,132.458383855174,132.558606422947,
132.656885980675,132.755132559749,132.853375642787,132.955072831429,133.053457244848,
133.156810821102,133.260164397356,133.35876252236,133.457220305136,133.557442872909,
133.655722430637,133.75396900971,133.852212092749,133.953909281391,134.05229369481,
134.155647271063,134.259000847317,134.356128675186,134.453094160804,134.549968416922,
134.646782617699,134.743567858737,134.840399971759,134.937256811785,135.034231214224,
135.088484104361),.UNSPECIFIED.);
#527=B_SPLINE_CURVE_WITH_KNOTS('',3,(#53912,#53913,#53914,#53915,#53916,
#53917,#53918,#53919),.UNSPECIFIED.,.F.,.F.,(4,1,1,1,1,4),(124.74803348566,
125.73427953018,126.733115980142,127.731952430104,128.730788880066,128.805298797182),
 .UNSPECIFIED.);
#528=B_SPLINE_CURVE_WITH_KNOTS('',3,(#53920,#53921,#53922,#53923,#53924,
#53925,#53926,#53927,#53928,#53929,#53930,#53931,#53932,#53933,#53934,#53935,
#53936,#53937,#53938,#53939,#53940,#53941,#53942,#53943,#53944,#53945,#53946,
#53947,#53948,#53949,#53950,#53951,#53952,#53953,#53954,#53955,#53956,#53957,
#53958,#53959,#53960,#53961,#53962,#53963,#53964,#53965,#53966,#53967,#53968,
#53969,#53970,#53971,#53972,#53973,#53974,#53975,#53976,#53977,#53978,#53979,
#53980,#53981,#53982,#53983,#53984,#53985,#53986,#53987,#53988,#53989),
 .UNSPECIFIED.,.F.,.F.,(4,3,3,3,3,3,3,3,3,3,3,3,3,3,3,3,3,3,3,3,3,3,3,4),
(128.805298797182,128.902840431273,129.000250613517,129.097560812666,129.194818343698,
129.292053887497,129.389298094495,129.486642967568,129.584044330746,129.68160592498,
129.729625330028,129.828223455032,129.926681237808,130.026903805581,130.125183363309,
130.223429942382,130.321673025421,130.423370214063,130.521754627482,130.625108203735,
130.728461779989,130.82704702784,130.929351001426,131.031654975012),
 .UNSPECIFIED.);
#529=B_SPLINE_CURVE_WITH_KNOTS('',3,(#53991,#53992,#53993,#53994,#53995,
#53996,#53997,#53998,#53999,#54000,#54001,#54002,#54003,#54004,#54005,#54006,
#54007,#54008,#54009,#54010,#54011,#54012,#54013,#54014,#54015,#54016,#54017,
#54018,#54019,#54020,#54021,#54022,#54023,#54024,#54025,#54026,#54027,#54028,
#54029,#54030,#54031,#54032,#54033,#54034,#54035,#54036,#54037,#54038,#54039,
#54040,#54041,#54042,#54043,#54044,#54045,#54046,#54047,#54048,#54049,#54050,
#54051,#54052,#54053,#54054,#54055,#54056,#54057,#54058,#54059,#54060),
 .UNSPECIFIED.,.F.,.F.,(4,3,3,3,3,3,3,3,3,3,3,3,3,3,3,3,3,3,3,3,3,3,3,4),
(128.80529901116,128.910085619871,129.015255759151,129.120630109632,129.226318351047,
129.264818597508,129.363416722512,129.461874505288,129.562097073061,129.660376630789,
129.758623209863,129.856866292901,129.958563481543,130.056947894962,130.160301471216,
130.26365504747,130.362225486655,130.460667523599,130.55901086589,130.657285118175,
130.755545076206,130.853792579363,130.952108672699,131.030544946366),
 .UNSPECIFIED.);
#530=B_SPLINE_CURVE_WITH_KNOTS('',3,(#54061,#54062,#54063,#54064,#54065,
#54066,#54067,#54068),.UNSPECIFIED.,.F.,.F.,(4,1,1,1,1,4),(124.748072442403,
125.269472797661,126.268309247622,127.267145697584,128.265982147546,128.805298797182),
 .UNSPECIFIED.);
#531=B_SPLINE_CURVE_WITH_KNOTS('',3,(#54074,#54075,#54076,#54077,#54078,
#54079,#54080,#54081,#54082,#54083,#54084,#54085,#54086,#54087,#54088,#54089,
#54090,#54091,#54092,#54093,#54094,#54095,#54096,#54097,#54098,#54099,#54100,
#54101,#54102,#54103,#54104,#54105,#54106,#54107,#54108,#54109,#54110,#54111,
#54112,#54113,#54114,#54115,#54116,#54117,#54118,#54119,#54120,#54121,#54122,
#54123,#54124,#54125,#54126,#54127,#54128,#54129,#54130,#54131,#54132,#54133,
#54134,#54135,#54136,#54137,#54138,#54139,#54140,#54141,#54142,#54143,#54144,
#54145,#54146,#54147,#54148,#54149,#54150,#54151,#54152,#54153,#54154,#54155,
#54156,#54157,#54158,#54159,#54160,#54161,#54162,#54163,#54164,#54165,#54166,
#54167,#54168,#54169,#54170,#54171,#54172,#54173,#54174,#54175,#54176,#54177,
#54178,#54179,#54180,#54181,#54182,#54183,#54184,#54185,#54186,#54187,#54188,
#54189,#54190,#54191,#54192,#54193,#54194,#54195,#54196,#54197),
 .UNSPECIFIED.,.F.,.F.,(4,3,3,3,3,3,3,3,3,3,3,3,3,3,3,3,3,3,3,3,3,3,3,3,
3,3,3,3,3,3,3,3,3,3,3,3,3,3,3,3,3,4),(118.464214610255,118.562615728343,
118.661189998764,118.742424380447,118.841022505451,118.939480288228,119.039702856,
119.137982413728,119.236228992802,119.33447207584,119.436169264482,119.534553677901,
119.637907254155,119.741260830409,119.839858955413,119.93831673819,120.038539305963,
120.136818863691,120.235065442764,120.333308525802,120.435005714445,120.533390127863,
120.636743704117,120.740097280371,120.838695405375,120.937153188151,121.037375755924,
121.135655313652,121.233901892726,121.332144975764,121.433842164407,121.532226577825,
121.635580154079,121.738933730333,121.836831200292,121.933909156543,122.030894120917,
122.127817176647,122.226391254986,122.323316910845,122.422715200424,122.522113490002),
 .UNSPECIFIED.);
#532=B_SPLINE_CURVE_WITH_KNOTS('',3,(#54198,#54199,#54200,#54201,#54202,
#54203,#54204),.UNSPECIFIED.,.F.,.F.,(4,1,1,1,4),(122.522113490002,122.737770180294,
123.736606630256,124.735443080218,124.74803348566),.UNSPECIFIED.);
#533=B_SPLINE_CURVE_WITH_KNOTS('',3,(#54206,#54207,#54208,#54209,#54210,
#54211),.UNSPECIFIED.,.F.,.F.,(4,1,1,4),(122.522113490002,123.271799897737,
124.270636347699,124.748072442403),.UNSPECIFIED.);
#534=B_SPLINE_CURVE_WITH_KNOTS('',3,(#54212,#54213,#54214,#54215,#54216,
#54217,#54218,#54219,#54220,#54221,#54222,#54223,#54224,#54225,#54226,#54227,
#54228,#54229,#54230,#54231,#54232,#54233,#54234,#54235,#54236,#54237,#54238,
#54239,#54240,#54241,#54242,#54243,#54244,#54245,#54246,#54247,#54248,#54249,
#54250,#54251,#54252,#54253,#54254,#54255,#54256,#54257,#54258,#54259,#54260,
#54261,#54262,#54263,#54264,#54265,#54266,#54267,#54268,#54269,#54270,#54271,
#54272,#54273,#54274,#54275,#54276,#54277,#54278,#54279,#54280,#54281,#54282,
#54283,#54284,#54285,#54286,#54287,#54288,#54289,#54290,#54291,#54292,#54293,
#54294,#54295,#54296,#54297,#54298,#54299,#54300,#54301,#54302,#54303,#54304,
#54305,#54306,#54307,#54308,#54309,#54310,#54311,#54312,#54313,#54314,#54315,
#54316,#54317,#54318,#54319,#54320,#54321,#54322,#54323,#54324,#54325,#54326,
#54327,#54328,#54329,#54330,#54331,#54332,#54333,#54334,#54335),
 .UNSPECIFIED.,.F.,.F.,(4,3,3,3,3,3,3,3,3,3,3,3,3,3,3,3,3,3,3,3,3,3,3,3,
3,3,3,3,3,3,3,3,3,3,3,3,3,3,3,3,3,4),(118.465360151754,118.566746895021,
118.66503051079,118.763278702571,118.861520955212,118.959786738854,119.05816456808,
119.156610036517,119.255210841691,119.276454097889,119.375052222893,119.47351000567,
119.573732573442,119.67201213117,119.770258710244,119.868501793282,119.970198981925,
120.068583395343,120.171936971597,120.275290547851,120.373888672855,120.472346455631,
120.572569023404,120.670848581132,120.769095160206,120.867338243244,120.969035431886,
121.067419845305,121.170773421559,121.274126997813,121.372725122817,121.471182905593,
121.571405473366,121.669685031094,121.767931610168,121.866174693206,121.967871881848,
122.066256295267,122.169609871521,122.272963447775,122.400857829821,122.52211338997),
 .UNSPECIFIED.);
#535=B_SPLINE_CURVE_WITH_KNOTS('',3,(#54341,#54342,#54343,#54344,#54345,
#54346,#54347,#54348,#54349,#54350,#54351,#54352,#54353,#54354,#54355,#54356,
#54357,#54358,#54359,#54360,#54361,#54362,#54363,#54364,#54365,#54366,#54367,
#54368,#54369,#54370,#54371,#54372,#54373,#54374,#54375,#54376,#54377,#54378,
#54379,#54380,#54381,#54382,#54383,#54384,#54385,#54386,#54387,#54388,#54389,
#54390,#54391,#54392,#54393,#54394,#54395,#54396,#54397,#54398,#54399,#54400,
#54401,#54402,#54403,#54404,#54405,#54406,#54407,#54408,#54409,#54410,#54411,
#54412,#54413,#54414,#54415,#54416,#54417,#54418,#54419,#54420,#54421,#54422,
#54423,#54424,#54425,#54426,#54427,#54428,#54429,#54430,#54431,#54432,#54433,
#54434,#54435,#54436,#54437,#54438,#54439,#54440,#54441,#54442,#54443,#54444,
#54445,#54446,#54447,#54448,#54449,#54450,#54451,#54452,#54453,#54454,#54455,
#54456,#54457,#54458,#54459,#54460,#54461,#54462,#54463,#54464),
 .UNSPECIFIED.,.F.,.F.,(4,3,3,3,3,3,3,3,3,3,3,3,3,3,3,3,3,3,3,3,3,3,3,3,
3,3,3,3,3,3,3,3,3,3,3,3,3,3,3,3,3,4),(112.181790934622,112.280032837375,
112.378281941166,112.476633717368,112.575038455028,112.673614634251,112.749405680676,
112.84800380568,112.946461588457,113.046684156229,113.144963713957,113.243210293031,
113.341453376069,113.443150564711,113.54153497813,113.644888554384,113.748242130638,
113.846840255642,113.945298038418,114.045520606191,114.143800163919,114.242046742992,
114.34028982603,114.441987014673,114.540371428091,114.643725004345,114.747078580599,
114.845676705603,114.944134488379,115.044357056152,115.14263661388,115.240883192953,
115.339126275992,115.440823464634,115.539207878053,115.642561454307,115.745915030561,
115.849888759331,115.953561696348,116.057054365164,116.160309146371,116.238928182547),
 .UNSPECIFIED.);
#536=B_SPLINE_CURVE_WITH_KNOTS('',3,(#54465,#54466,#54467,#54468,#54469,
#54470,#54471,#54472,#54473,#54474,#54475,#54476,#54477,#54478,#54479,#54480,
#54481,#54482,#54483,#54484,#54485,#54486,#54487,#54488,#54489,#54490,#54491,
#54492,#54493,#54494,#54495,#54496,#54497,#54498,#54499,#54500,#54501,#54502,
#54503,#54504,#54505,#54506,#54507,#54508,#54509,#54510,#54511,#54512,#54513,
#54514,#54515,#54516,#54517,#54518,#54519,#54520,#54521,#54522,#54523,#54524,
#54525,#54526,#54527,#54528,#54529,#54530,#54531,#54532,#54533,#54534),
 .UNSPECIFIED.,.F.,.F.,(4,3,3,3,3,3,3,3,3,3,3,3,3,3,3,3,3,3,3,3,3,3,3,4),
(116.238928182823,116.341566510357,116.44447107289,116.547509821617,116.650828963887,
116.744751480523,116.843349605527,116.941807388303,117.042029956076,117.140309513804,
117.238556092877,117.336799175916,117.438496364558,117.536880777977,117.640234354231,
117.743587930485,117.842162082216,117.940606624237,118.038951269659,118.137225626952,
118.235476585644,118.333714612383,118.431998836548,118.464214610255),
 .UNSPECIFIED.);
#537=B_SPLINE_CURVE_WITH_KNOTS('',3,(#54536,#54537,#54538,#54539,#54540,
#54541,#54542,#54543,#54544,#54545,#54546,#54547,#54548,#54549,#54550,#54551,
#54552,#54553,#54554,#54555,#54556,#54557,#54558,#54559,#54560,#54561,#54562,
#54563,#54564,#54565,#54566,#54567,#54568,#54569,#54570,#54571,#54572,#54573,
#54574,#54575,#54576,#54577,#54578,#54579,#54580,#54581,#54582,#54583,#54584,
#54585,#54586,#54587,#54588,#54589,#54590,#54591,#54592,#54593,#54594,#54595,
#54596,#54597,#54598,#54599,#54600,#54601,#54602,#54603,#54604,#54605),
 .UNSPECIFIED.,.F.,.F.,(4,3,3,3,3,3,3,3,3,3,3,3,3,3,3,3,3,3,3,3,3,3,3,4),
(116.238928182823,116.279944748004,116.378542873008,116.477000655784,116.577223223557,
116.675502781285,116.773749360358,116.871992443397,116.973689632039,117.072074045458,
117.175427621712,117.278781197966,117.37737932297,117.475837105746,117.576059673519,
117.674339231247,117.77258581032,117.870828893359,117.972526082001,118.07091049542,
118.174264071673,118.277617647927,118.376189313834,118.465360151754),
 .UNSPECIFIED.);
#538=B_SPLINE_CURVE_WITH_KNOTS('',3,(#54606,#54607,#54608,#54609,#54610,
#54611,#54612,#54613),.UNSPECIFIED.,.F.,.F.,(4,1,1,1,1,4),(112.180986330182,
112.284598948156,113.283435398118,114.28227184808,115.281108298042,116.238922797526),
 .UNSPECIFIED.);
#539=B_SPLINE_CURVE_WITH_KNOTS('',3,(#54619,#54620,#54621,#54622,#54623,
#54624,#54625,#54626,#54627,#54628,#54629,#54630,#54631,#54632,#54633,#54634,
#54635,#54636,#54637,#54638,#54639,#54640,#54641,#54642,#54643,#54644,#54645,
#54646,#54647,#54648,#54649,#54650,#54651,#54652,#54653,#54654,#54655,#54656,
#54657,#54658,#54659,#54660,#54661,#54662,#54663,#54664,#54665,#54666,#54667,
#54668,#54669,#54670,#54671,#54672,#54673,#54674,#54675,#54676,#54677,#54678,
#54679,#54680,#54681,#54682,#54683,#54684,#54685,#54686,#54687,#54688,#54689,
#54690,#54691,#54692,#54693,#54694,#54695,#54696,#54697,#54698,#54699,#54700,
#54701,#54702,#54703,#54704,#54705,#54706,#54707,#54708,#54709,#54710,#54711,
#54712,#54713,#54714,#54715,#54716,#54717,#54718,#54719,#54720,#54721,#54722,
#54723,#54724,#54725,#54726,#54727,#54728,#54729,#54730,#54731,#54732,#54733,
#54734,#54735,#54736,#54737,#54738,#54739,#54740,#54741,#54742),
 .UNSPECIFIED.,.F.,.F.,(4,3,3,3,3,3,3,3,3,3,3,3,3,3,3,3,3,3,3,3,3,3,3,3,
3,3,3,3,3,3,3,3,3,3,3,3,3,3,3,3,3,4),(105.898938930965,105.997345977956,
106.095658486362,106.193920763664,106.292162312088,106.390412605836,106.488766498079,
106.587174739352,106.685752818818,106.756386980905,106.854985105909,106.953442888685,
107.053665456458,107.151945014186,107.250191593259,107.348434676298,107.45013186494,
107.548516278359,107.651869854612,107.755223430866,107.85382155587,107.952279338646,
108.052501906419,108.150781464147,108.24902804322,108.347271126259,108.448968314901,
108.54735272832,108.650706304574,108.754059880828,108.852658005832,108.951115788608,
109.051338356381,109.149617914109,109.247864493183,109.346107576221,109.447804764863,
109.546189178282,109.649542754536,109.75289633079,109.893212936346,109.955742875643),
 .UNSPECIFIED.);
#540=B_SPLINE_CURVE_WITH_KNOTS('',3,(#54743,#54744,#54745,#54746,#54747,
#54748,#54749,#54750,#54751,#54752,#54753,#54754,#54755,#54756,#54757,#54758,
#54759,#54760,#54761,#54762,#54763,#54764,#54765,#54766,#54767,#54768,#54769,
#54770,#54771,#54772,#54773,#54774,#54775,#54776,#54777,#54778,#54779,#54780,
#54781,#54782,#54783,#54784,#54785,#54786,#54787,#54788,#54789,#54790,#54791,
#54792,#54793,#54794,#54795,#54796,#54797,#54798,#54799,#54800,#54801,#54802,
#54803,#54804,#54805,#54806,#54807,#54808,#54809,#54810,#54811,#54812,#54813,
#54814,#54815),.UNSPECIFIED.,.F.,.F.,(4,3,3,3,3,3,3,3,3,3,3,3,3,3,3,3,3,
3,3,3,3,3,3,3,4),(109.955742875951,110.055241614051,110.152151423466,110.249014842069,
110.345862894414,110.447330365999,110.544300028994,110.641334438529,110.738518045248,
110.751732780752,110.850330905756,110.948788688533,111.049011256305,111.147290814034,
111.245537393107,111.343780476145,111.445477664788,111.543862078206,111.64721565446,
111.750569230714,111.849176820414,111.947618966285,112.045965736407,112.144240689691,
112.181790934622),.UNSPECIFIED.);
#541=B_SPLINE_CURVE_WITH_KNOTS('',3,(#54817,#54818,#54819,#54820,#54821,
#54822),.UNSPECIFIED.,.F.,.F.,(4,1,1,4),(109.955750010146,110.286926048232,
111.285762498194,112.180986330182),.UNSPECIFIED.);
#542=B_SPLINE_CURVE_WITH_KNOTS('',3,(#54823,#54824,#54825,#54826,#54827,
#54828,#54829,#54830,#54831,#54832,#54833,#54834,#54835,#54836,#54837,#54838,
#54839,#54840,#54841,#54842,#54843,#54844,#54845,#54846,#54847,#54848,#54849,
#54850,#54851,#54852,#54853,#54854,#54855,#54856,#54857,#54858,#54859,#54860,
#54861,#54862,#54863,#54864,#54865,#54866,#54867,#54868,#54869,#54870,#54871,
#54872,#54873,#54874,#54875,#54876,#54877,#54878,#54879,#54880,#54881,#54882,
#54883,#54884,#54885,#54886,#54887,#54888,#54889,#54890,#54891,#54892,#54893,
#54894,#54895,#54896,#54897,#54898,#54899,#54900,#54901,#54902,#54903,#54904,
#54905,#54906,#54907,#54908,#54909,#54910,#54911,#54912,#54913,#54914,#54915,
#54916,#54917,#54918,#54919,#54920,#54921,#54922,#54923,#54924,#54925,#54926,
#54927,#54928,#54929,#54930,#54931,#54932,#54933,#54934,#54935,#54936,#54937,
#54938,#54939,#54940,#54941,#54942,#54943,#54944,#54945,#54946),
 .UNSPECIFIED.,.F.,.F.,(4,3,3,3,3,3,3,3,3,3,3,3,3,3,3,3,3,3,3,3,3,3,3,3,
3,3,3,3,3,3,3,3,3,3,3,3,3,3,3,3,3,4),(105.898082547599,105.996456972795,
106.094847349944,106.193416320635,106.291580248385,106.390178373389,106.488636156166,
106.588858723938,106.687138281666,106.78538486074,106.883627943778,106.985325132421,
107.083709545839,107.187063122093,107.290416698347,107.389014823351,107.487472606128,
107.5876951739,107.685974731629,107.784221310702,107.88246439374,107.984161582382,
108.082545995801,108.185899572055,108.289253148309,108.387851273313,108.486309056089,
108.586531623862,108.68481118159,108.783057760664,108.881300843702,108.982998032344,
109.081382445763,109.184736022017,109.288089598271,109.386591328535,109.484956309732,
109.583214317041,109.681399820023,109.779540599733,109.877698313764,109.955742875643),
 .UNSPECIFIED.);
#543=B_SPLINE_CURVE_WITH_KNOTS('',3,(#54952,#54953,#54954,#54955,#54956,
#54957,#54958,#54959),.UNSPECIFIED.,.F.,.F.,(4,1,1,1,1,4),(99.6144332356559,
99.7645318311714,100.763368281133,101.762204731095,102.761041181057,103.672548858943),
 .UNSPECIFIED.);
#544=B_SPLINE_CURVE_WITH_KNOTS('',3,(#54960,#54961,#54962,#54963,#54964,
#54965,#54966,#54967,#54968,#54969,#54970,#54971,#54972,#54973,#54974,#54975,
#54976,#54977,#54978,#54979,#54980,#54981,#54982,#54983,#54984,#54985,#54986,
#54987,#54988,#54989,#54990,#54991,#54992,#54993,#54994,#54995,#54996,#54997,
#54998,#54999,#55000,#55001,#55002,#55003,#55004,#55005,#55006,#55007,#55008,
#55009,#55010,#55011,#55012,#55013,#55014,#55015,#55016,#55017,#55018,#55019,
#55020,#55021,#55022,#55023,#55024,#55025,#55026,#55027,#55028,#55029),
 .UNSPECIFIED.,.F.,.F.,(4,3,3,3,3,3,3,3,3,3,3,3,3,3,3,3,3,3,3,3,3,3,3,4),
(103.672557568463,103.759877631019,103.858475756023,103.9569335388,104.057156106572,
104.1554356643,104.253682243374,104.351925326412,104.453622515054,104.552006928473,
104.655360504727,104.758714080981,104.857312205985,104.955769988762,105.055992556534,
105.154272114262,105.252518693336,105.350761776374,105.452458965017,105.550843378435,
105.654196954689,105.757550530943,105.856140410583,105.898938930965),
 .UNSPECIFIED.);
#545=B_SPLINE_CURVE_WITH_KNOTS('',3,(#55031,#55032,#55033,#55034,#55035,
#55036,#55037,#55038,#55039,#55040,#55041,#55042,#55043,#55044,#55045,#55046,
#55047,#55048,#55049,#55050,#55051,#55052,#55053,#55054,#55055,#55056,#55057,
#55058,#55059,#55060,#55061,#55062,#55063,#55064,#55065,#55066,#55067,#55068,
#55069,#55070,#55071,#55072,#55073,#55074,#55075,#55076,#55077,#55078,#55079,
#55080,#55081,#55082,#55083,#55084,#55085,#55086,#55087,#55088,#55089,#55090,
#55091,#55092,#55093,#55094,#55095,#55096,#55097,#55098,#55099,#55100,#55101,
#55102,#55103),.UNSPECIFIED.,.F.,.F.,(4,3,3,3,3,3,3,3,3,3,3,3,3,3,3,3,3,
3,3,3,3,3,3,3,4),(103.672557568463,103.771601702603,103.870660322484,103.96976131202,
104.06899945985,104.168318657834,104.267812431338,104.293907348461,104.392505473465,
104.490963256241,104.591185824014,104.689465381742,104.787711960816,104.885955043854,
104.987652232496,105.086036645915,105.189390222169,105.292743798423,105.39132916073,
105.489781902009,105.591857063406,105.690131970176,105.788367325635,105.886604359972,
105.898082547599),.UNSPECIFIED.);
#546=B_SPLINE_CURVE_WITH_KNOTS('',3,(#55104,#55105,#55106,#55107,#55108,
#55109,#55110,#55111),.UNSPECIFIED.,.F.,.F.,(4,1,1,1,1,4),(99.616027896677,
100.298561548614,101.297397998576,102.296234448537,103.295070898499,103.672550060648),
 .UNSPECIFIED.);
#547=B_SPLINE_CURVE_WITH_KNOTS('',3,(#55117,#55118,#55119,#55120,#55121,
#55122,#55123,#55124,#55125,#55126,#55127,#55128,#55129,#55130,#55131,#55132,
#55133,#55134,#55135,#55136,#55137,#55138,#55139,#55140,#55141,#55142,#55143,
#55144,#55145,#55146,#55147,#55148,#55149,#55150,#55151,#55152,#55153,#55154,
#55155,#55156,#55157,#55158,#55159,#55160,#55161,#55162,#55163,#55164,#55165,
#55166,#55167,#55168,#55169,#55170,#55171,#55172,#55173,#55174,#55175,#55176,
#55177,#55178,#55179,#55180,#55181,#55182,#55183,#55184,#55185,#55186,#55187,
#55188,#55189,#55190,#55191,#55192,#55193,#55194,#55195,#55196,#55197,#55198,
#55199,#55200,#55201,#55202,#55203,#55204,#55205,#55206,#55207,#55208,#55209,
#55210,#55211,#55212,#55213,#55214,#55215,#55216,#55217,#55218,#55219,#55220,
#55221,#55222,#55223,#55224,#55225,#55226,#55227,#55228,#55229,#55230,#55231,
#55232,#55233,#55234,#55235,#55236,#55237,#55238,#55239,#55240,#55241,#55242,
#55243),.UNSPECIFIED.,.F.,.F.,(4,3,3,3,3,3,3,3,3,3,3,3,3,3,3,3,3,3,3,3,
3,3,3,3,3,3,3,3,3,3,3,3,3,3,3,3,3,3,3,3,3,3,4),(93.3318434577557,93.430100540662,
93.5284655250177,93.6268914778956,93.7254798525794,93.7715131314001,93.8701112564038,
93.9685690391807,94.0687916069534,94.1670711646815,94.2653177437549,94.3635608267937,
94.4652580154358,94.5636424288546,94.6669960051083,94.770349581362,94.8689477063657,
94.9674054891427,95.0676280569154,95.1659076146435,95.264154193717,95.3623972767553,
95.4640944653975,95.5624788788163,95.6658324550701,95.7691860313239,95.8677841563275,
95.9662419391041,96.0664645068768,96.164744064605,96.2629906436783,96.361233726717,
96.4629309153592,96.5613153287781,96.6646689050319,96.7680224812858,96.8674993725788,
96.9668292609825,97.0660403563896,97.1651524247991,97.2642075332237,97.3632407686266,
97.3893722612837),.UNSPECIFIED.);
#548=B_SPLINE_CURVE_WITH_KNOTS('',3,(#55244,#55245,#55246,#55247,#55248,
#55249),.UNSPECIFIED.,.F.,.F.,(4,1,1,4),(97.3893797695142,97.7668589312476,
98.7656953812095,99.6144332356559),.UNSPECIFIED.);
#549=B_SPLINE_CURVE_WITH_KNOTS('',3,(#55251,#55252,#55253,#55254,#55255,
#55256),.UNSPECIFIED.,.F.,.F.,(4,1,1,4),(97.3893809712563,98.3008886486899,
99.2997250986518,99.616027896677),.UNSPECIFIED.);
#550=B_SPLINE_CURVE_WITH_KNOTS('',3,(#55257,#55258,#55259,#55260,#55261,
#55262,#55263,#55264,#55265,#55266,#55267,#55268,#55269,#55270,#55271,#55272,
#55273,#55274,#55275,#55276,#55277,#55278,#55279,#55280,#55281,#55282,#55283,
#55284,#55285,#55286,#55287,#55288,#55289,#55290,#55291,#55292,#55293,#55294,
#55295,#55296,#55297,#55298,#55299,#55300,#55301,#55302,#55303,#55304,#55305,
#55306,#55307,#55308,#55309,#55310,#55311,#55312,#55313,#55314,#55315,#55316,
#55317,#55318,#55319,#55320,#55321,#55322,#55323,#55324,#55325,#55326,#55327,
#55328,#55329,#55330,#55331,#55332,#55333,#55334,#55335,#55336,#55337,#55338,
#55339,#55340,#55341,#55342,#55343,#55344,#55345,#55346,#55347,#55348,#55349,
#55350,#55351,#55352,#55353,#55354,#55355,#55356,#55357,#55358,#55359,#55360,
#55361,#55362,#55363,#55364,#55365,#55366,#55367,#55368,#55369,#55370,#55371,
#55372,#55373,#55374,#55375,#55376,#55377,#55378,#55379,#55380),
 .UNSPECIFIED.,.F.,.F.,(4,3,3,3,3,3,3,3,3,3,3,3,3,3,3,3,3,3,3,3,3,3,3,3,
3,3,3,3,3,3,3,3,3,3,3,3,3,3,3,3,3,4),(93.3321733295568,93.4307320757135,
93.5291589669388,93.6274833960061,93.725752386932,93.8239954496423,93.9222420613545,
94.0205891224222,94.1189858639191,94.2175579055399,94.3055428488424,94.4041409738461,
94.5025987566229,94.6028213243955,94.7011008821237,94.7993474611971,94.8975905442356,
94.9992877328778,95.0976721462966,95.2010257225504,95.3043792988043,95.402977423808,
95.5014352065848,95.6016577743575,95.6999373320856,95.798183911159,95.8964269941974,
95.9981241828396,96.0965085962584,96.1998621725123,96.3032157487662,96.4018138737699,
96.5002716565466,96.6004942243193,96.6987737820475,96.7970203611208,96.8952634441593,
96.9969606328015,97.0953450462203,97.1986986224741,97.302052198728,97.3893722612837),
 .UNSPECIFIED.);
#551=B_SPLINE_CURVE_WITH_KNOTS('',3,(#55386,#55387,#55388,#55389,#55390,
#55391,#55392,#55393),.UNSPECIFIED.,.F.,.F.,(4,1,1,1,1,4),(87.049742935369,
87.7784944316289,88.7773308815908,89.7761673315526,90.7750037815145,91.1061798190633),
 .UNSPECIFIED.);
#552=B_SPLINE_CURVE_WITH_KNOTS('',3,(#55394,#55395,#55396,#55397,#55398,
#55399,#55400,#55401,#55402,#55403,#55404,#55405,#55406,#55407,#55408,#55409,
#55410,#55411,#55412,#55413,#55414,#55415,#55416,#55417,#55418,#55419,#55420,
#55421,#55422,#55423,#55424,#55425,#55426,#55427,#55428,#55429,#55430,#55431,
#55432,#55433,#55434,#55435,#55436,#55437,#55438,#55439,#55440,#55441,#55442,
#55443,#55444,#55445,#55446,#55447,#55448,#55449,#55450,#55451,#55452,#55453,
#55454,#55455,#55456,#55457,#55458,#55459,#55460,#55461,#55462,#55463),
 .UNSPECIFIED.,.F.,.F.,(4,3,3,3,3,3,3,3,3,3,3,3,3,3,3,3,3,3,3,3,3,3,3,4),
(91.1061869541041,91.204341964477,91.3024795334307,91.4006291648839,91.4988897541856,
91.5972075103077,91.6957053368613,91.7738402314764,91.8724383564801,91.9708961392568,
92.0711187070294,92.1693982647576,92.2676448438311,92.3658879268697,92.4675851155119,
92.5659695289307,92.6693231051845,92.7726766814383,92.8712673172515,92.9697241251222,
93.0680663331333,93.1663410384397,93.2645927043656,93.3318434577557),
 .UNSPECIFIED.);
#553=B_SPLINE_CURVE_WITH_KNOTS('',3,(#55465,#55466,#55467,#55468,#55469,
#55470,#55471,#55472,#55473,#55474,#55475,#55476,#55477,#55478,#55479,#55480,
#55481,#55482,#55483,#55484,#55485,#55486,#55487,#55488,#55489,#55490,#55491,
#55492,#55493,#55494,#55495,#55496,#55497,#55498,#55499,#55500,#55501,#55502,
#55503,#55504,#55505,#55506,#55507,#55508,#55509,#55510,#55511,#55512,#55513,
#55514,#55515,#55516,#55517,#55518,#55519,#55520,#55521,#55522,#55523,#55524,
#55525,#55526,#55527,#55528,#55529,#55530,#55531,#55532,#55533,#55534),
 .UNSPECIFIED.,.F.,.F.,(4,3,3,3,3,3,3,3,3,3,3,3,3,3,3,3,3,3,3,3,3,3,3,4),
(91.1061869541041,91.246503559673,91.3090334989568,91.4076316239605,91.5060894067373,
91.6063119745099,91.7045915322381,91.8028381113116,91.9010811943501,92.0027783829923,
92.101162796411,92.2045163726649,92.3078699489187,92.4064680739224,92.5049258566991,
92.6051484244718,92.7034279822,92.8016745612733,92.8999176443118,93.001614832954,
93.0999992463728,93.2033528226267,93.3067063988806,93.3321733295568),
 .UNSPECIFIED.);
#554=B_SPLINE_CURVE_WITH_KNOTS('',3,(#55535,#55536,#55537,#55538,#55539,
#55540,#55541,#55542,#55543,#55544,#55545,#55546,#55547,#55548,#55549,#55550,
#55551,#55552,#55553,#55554,#55555,#55556,#55557,#55558,#55559,#55560,#55561,
#55562,#55563,#55564,#55565,#55566,#55567,#55568,#55569,#55570,#55571,#55572,
#55573,#55574,#55575,#55576,#55577,#55578,#55579,#55580,#55581,#55582,#55583,
#55584,#55585,#55586,#55587,#55588,#55589,#55590,#55591,#55592,#55593,#55594,
#55595,#55596,#55597,#55598,#55599,#55600,#55601,#55602,#55603,#55604,#55605,
#55606,#55607,#55608,#55609,#55610,#55611,#55612,#55613,#55614,#55615,#55616,
#55617,#55618,#55619,#55620,#55621,#55622,#55623,#55624,#55625,#55626,#55627,
#55628,#55629,#55630,#55631,#55632,#55633,#55634,#55635,#55636,#55637,#55638,
#55639,#55640,#55641,#55642,#55643,#55644,#55645,#55646,#55647,#55648,#55649,
#55650,#55651,#55652,#55653,#55654,#55655,#55656,#55657,#55658,#55659,#55660,
#55661),.UNSPECIFIED.,.F.,.F.,(4,3,3,3,3,3,3,3,3,3,3,3,3,3,3,3,3,3,3,3,
3,3,3,3,3,3,3,3,3,3,3,3,3,3,3,3,3,3,3,3,3,3,4),(87.0482730730921,87.1466828368096,
87.2452617573112,87.3136876991093,87.412285824113,87.5107436068897,87.6109661746624,
87.7092457323906,87.807492311464,87.9057353945025,88.0074325831447,88.1058169965635,
88.2091705728173,88.3125241490712,88.4111222740749,88.5095800568516,88.6098026246243,
88.7080821823524,88.8063287614258,88.9045718444643,89.0062690331065,89.1046534465253,
89.2080070227792,89.3113605990331,89.4099587240368,89.5084165068135,89.6086390745862,
89.7069186323143,89.8051652113877,89.9034082944262,90.0051054830684,90.1034898964872,
90.206843472741,90.3101970489949,90.409695787095,90.5067185530535,90.6036495481491,
90.7005198981799,90.801936662084,90.8988156754797,90.9957205549586,91.0927209416412,
91.1061869537961),.UNSPECIFIED.);
#555=B_SPLINE_CURVE_WITH_KNOTS('',3,(#55667,#55668,#55669,#55670,#55671,
#55672,#55673,#55674,#55675,#55676,#55677,#55678,#55679,#55680,#55681,#55682,
#55683,#55684,#55685,#55686,#55687,#55688,#55689,#55690,#55691,#55692,#55693,
#55694,#55695,#55696,#55697,#55698,#55699,#55700,#55701,#55702,#55703,#55704,
#55705,#55706,#55707,#55708,#55709,#55710,#55711,#55712,#55713,#55714,#55715,
#55716,#55717,#55718,#55719,#55720,#55721,#55722,#55723,#55724,#55725,#55726,
#55727,#55728,#55729,#55730,#55731,#55732,#55733,#55734,#55735,#55736,#55737,
#55738,#55739,#55740,#55741,#55742,#55743,#55744,#55745,#55746,#55747,#55748,
#55749,#55750,#55751,#55752,#55753,#55754,#55755,#55756,#55757,#55758,#55759,
#55760,#55761,#55762,#55763,#55764,#55765,#55766,#55767,#55768,#55769,#55770,
#55771,#55772,#55773,#55774,#55775,#55776,#55777,#55778,#55779,#55780,#55781,
#55782,#55783,#55784,#55785,#55786,#55787,#55788,#55789,#55790,#55791,#55792,
#55793),.UNSPECIFIED.,.F.,.F.,(4,3,3,3,3,3,3,3,3,3,3,3,3,3,3,3,3,3,3,3,
3,3,3,3,3,3,3,3,3,3,3,3,3,3,3,3,3,3,3,3,3,3,4),(80.7655329655535,80.7866392818958,
80.8852374068995,80.9836951896763,81.0839177574489,81.1821973151771,81.2804438942505,
81.378686977289,81.4803841659311,81.57876857935,81.6821221556038,81.7854757318576,
81.8840738568613,81.982531639638,82.0827542074107,82.1810337651388,82.2792803442122,
82.3775234272507,82.4792206158929,82.5776050293117,82.6809586055656,82.7843121818195,
82.8829103068232,82.9813680895999,83.0815906573726,83.1798702151008,83.2781167941742,
83.3763598772127,83.4780570658549,83.5764414792737,83.6797950555275,83.7831486317814,
83.8817467567851,83.9802045395618,84.0804271073345,84.1787066650627,84.2769532441361,
84.3751963271746,84.4768935158168,84.5752779292356,84.6786315054894,84.7819850817433,
84.8230016469246),.UNSPECIFIED.);
#556=B_SPLINE_CURVE_WITH_KNOTS('',3,(#55794,#55795,#55796,#55797,#55798,
#55799),.UNSPECIFIED.,.F.,.F.,(4,1,1,4),(84.8230070319842,85.7808215317051,
86.779657981667,87.049742935369),.UNSPECIFIED.);
#557=B_SPLINE_CURVE_WITH_KNOTS('',3,(#55801,#55802,#55803,#55804,#55805,
#55806,#55807,#55808,#55809,#55810,#55811,#55812,#55813,#55814,#55815,#55816,
#55817,#55818,#55819,#55820,#55821,#55822,#55823,#55824,#55825,#55826,#55827,
#55828,#55829,#55830,#55831,#55832,#55833,#55834,#55835,#55836,#55837,#55838,
#55839,#55840,#55841,#55842,#55843,#55844,#55845,#55846,#55847,#55848,#55849,
#55850,#55851,#55852,#55853,#55854,#55855,#55856,#55857,#55858,#55859,#55860,
#55861,#55862,#55863,#55864,#55865,#55866,#55867,#55868,#55869,#55870),
 .UNSPECIFIED.,.F.,.F.,(4,3,3,3,3,3,3,3,3,3,3,3,3,3,3,3,3,3,3,3,3,3,3,4),
(84.8230016472006,84.9261861619504,85.0296647966981,85.1332945907092,85.2372126194224,
85.3160147991856,85.4146129241893,85.513070706966,85.6132932747387,85.7115728324668,
85.8098194115402,85.9080624945786,86.0097596832208,86.1081440966396,86.2114976728935,
86.3148512491474,86.4134243290378,86.5118681332248,86.6102123732649,86.7084866565461,
86.8067399239172,86.9049803913524,87.0032727094652,87.0482730730921),
 .UNSPECIFIED.);
#558=B_SPLINE_CURVE_WITH_KNOTS('',3,(#55871,#55872,#55873,#55874,#55875,
#55876,#55877,#55878,#55879,#55880,#55881,#55882,#55883,#55884,#55885,#55886,
#55887,#55888,#55889,#55890,#55891,#55892,#55893,#55894,#55895,#55896,#55897,
#55898,#55899,#55900,#55901,#55902,#55903,#55904,#55905,#55906,#55907,#55908,
#55909,#55910,#55911,#55912,#55913,#55914,#55915,#55916,#55917,#55918,#55919,
#55920,#55921,#55922,#55923,#55924,#55925,#55926,#55927,#55928,#55929,#55930,
#55931,#55932,#55933,#55934,#55935,#55936,#55937,#55938,#55939,#55940,#55941,
#55942,#55943,#55944,#55945,#55946,#55947,#55948,#55949,#55950,#55951,#55952,
#55953,#55954,#55955,#55956,#55957,#55958,#55959,#55960,#55961,#55962,#55963,
#55964,#55965,#55966,#55967,#55968,#55969,#55970,#55971,#55972,#55973,#55974,
#55975,#55976,#55977,#55978,#55979,#55980,#55981,#55982,#55983,#55984,#55985,
#55986,#55987,#55988,#55989,#55990,#55991,#55992,#55993,#55994),
 .UNSPECIFIED.,.F.,.F.,(4,3,3,3,3,3,3,3,3,3,3,3,3,3,3,3,3,3,3,3,3,3,3,3,
3,3,3,3,3,3,3,3,3,3,3,3,3,3,3,3,3,4),(80.7658264836951,80.8640676560909,
80.9623198605447,81.06067701958,81.1590905825019,81.2576716402341,81.3206689993381,
81.4192671243418,81.5177249071184,81.6179474748911,81.7162270326193,81.8144736116926,
81.9127166947313,82.0144138833734,82.1127982967922,82.2161518730461,82.3195054492999,
82.4181035743036,82.5165613570801,82.6167839248528,82.7150634825809,82.8133100616544,
82.9115531446928,83.0132503333351,83.1116347467539,83.2149883230078,83.3183418992618,
83.4169400242654,83.5153978070421,83.6156203748148,83.7138999325429,83.8121465116161,
83.9103895946545,84.0120867832968,84.1104711967157,84.2138247729697,84.3171783492237,
84.4205578302506,84.5236543867486,84.626583481318,84.7292989065995,84.8230016469246),
 .UNSPECIFIED.);
#559=B_SPLINE_CURVE_WITH_KNOTS('',3,(#56000,#56001,#56002,#56003,#56004,
#56005,#56006,#56007),.UNSPECIFIED.,.F.,.F.,(4,1,1,1,1,4),(74.4816441310534,
74.7936205821245,75.7924570320864,76.7912934820483,77.7901299320101,78.539816339745),
 .UNSPECIFIED.);
#560=B_SPLINE_CURVE_WITH_KNOTS('',3,(#56008,#56009,#56010,#56011,#56012,
#56013,#56014,#56015,#56016,#56017,#56018,#56019,#56020,#56021,#56022,#56023,
#56024,#56025,#56026,#56027,#56028,#56029,#56030,#56031,#56032,#56033,#56034,
#56035,#56036,#56037,#56038,#56039,#56040,#56041,#56042,#56043,#56044,#56045,
#56046,#56047,#56048,#56049,#56050,#56051,#56052,#56053,#56054,#56055,#56056,
#56057,#56058,#56059,#56060,#56061,#56062,#56063,#56064,#56065,#56066,#56067,
#56068,#56069,#56070,#56071,#56072,#56073,#56074),.UNSPECIFIED.,.F.,.F.,
(4,3,3,3,3,3,3,3,3,3,3,3,3,3,3,3,3,3,3,3,3,3,4),(78.5398164398193,78.6677108218625,
78.788966381972,78.8875645069757,78.9860222897523,79.086244857525,79.1845244152531,
79.2827709943266,79.3810140773651,79.4827112660073,79.5810956794261,79.68444925568,
79.7878028319339,79.8864023576698,79.9848611556883,80.0832042043514,80.1814836418338,
80.2797289912676,80.3779697355311,80.4762993937773,80.5746716764715,80.6732109328401,
80.7655329655535),.UNSPECIFIED.);
#561=B_SPLINE_CURVE_WITH_KNOTS('',3,(#56076,#56077,#56078,#56079,#56080,
#56081,#56082,#56083,#56084,#56085,#56086,#56087,#56088,#56089,#56090,#56091,
#56092,#56093,#56094,#56095,#56096,#56097,#56098,#56099,#56100,#56101,#56102,
#56103,#56104,#56105,#56106,#56107,#56108,#56109,#56110,#56111,#56112,#56113,
#56114,#56115,#56116,#56117,#56118,#56119,#56120,#56121,#56122,#56123,#56124,
#56125,#56126,#56127,#56128,#56129,#56130,#56131,#56132,#56133,#56134,#56135,
#56136,#56137,#56138,#56139,#56140,#56141,#56142,#56143,#56144,#56145),
 .UNSPECIFIED.,.F.,.F.,(4,3,3,3,3,3,3,3,3,3,3,3,3,3,3,3,3,3,3,3,3,3,3,4),
(78.539816339745,78.6377138097037,78.7346673304386,78.8315786913981,78.9284788661295,
79.0271081744507,79.1241353185129,79.2235657089636,79.3229960994143,79.421594224418,
79.5200520071949,79.6202745749675,79.7185541326957,79.816800711769,79.9150437948074,
80.0167409834496,80.1151253968684,80.2184789731223,80.3218325493762,80.4204382921282,
80.518879231313,80.6172249291312,80.7155010605349,80.7658264836951),
 .UNSPECIFIED.);
#562=B_SPLINE_CURVE_WITH_KNOTS('',3,(#56146,#56147,#56148,#56149,#56150,
#56151,#56152,#56153),.UNSPECIFIED.,.F.,.F.,(4,1,1,1,1,4),(74.4832630646979,
75.3276502995668,76.3264867495287,77.3253231994906,78.3241596494524,78.539816339745),
 .UNSPECIFIED.);
#563=B_SPLINE_CURVE_WITH_KNOTS('',3,(#56159,#56160,#56161,#56162,#56163,
#56164,#56165,#56166,#56167,#56168,#56169,#56170,#56171,#56172,#56173,#56174,
#56175,#56176,#56177,#56178,#56179,#56180,#56181,#56182,#56183,#56184,#56185,
#56186,#56187,#56188,#56189,#56190,#56191,#56192,#56193,#56194,#56195,#56196,
#56197,#56198,#56199,#56200,#56201,#56202,#56203,#56204,#56205,#56206,#56207,
#56208,#56209,#56210,#56211,#56212,#56213,#56214,#56215,#56216,#56217,#56218,
#56219,#56220,#56221,#56222,#56223,#56224,#56225,#56226,#56227,#56228,#56229,
#56230,#56231,#56232,#56233,#56234,#56235,#56236,#56237,#56238,#56239,#56240,
#56241,#56242,#56243,#56244,#56245,#56246,#56247,#56248,#56249,#56250,#56251,
#56252,#56253,#56254,#56255,#56256,#56257,#56258,#56259,#56260,#56261,#56262,
#56263,#56264,#56265,#56266,#56267,#56268,#56269,#56270,#56271,#56272,#56273,
#56274,#56275,#56276,#56277,#56278,#56279,#56280,#56281,#56282),
 .UNSPECIFIED.,.F.,.F.,(4,3,3,3,3,3,3,3,3,3,3,3,3,3,3,3,3,3,3,3,3,3,3,3,
3,3,3,3,3,3,3,3,3,3,3,3,3,3,3,3,3,4),(68.1995885964076,68.297834762989,
68.3960781129469,68.4972090552985,68.5955944658001,68.6980981740767,68.8006018823533,
68.899200007357,68.9976577901338,69.0978803579064,69.1961599156345,69.2944064947077,
69.3926495777462,69.4943467663884,69.5927311798072,69.6960847560611,69.7994383323151,
69.8980364573188,69.9964942400956,70.0967168078682,70.1949963655964,70.2932429446698,
70.3914860277084,70.4931832163505,70.5915676297693,70.6949212060232,70.798274782277,
70.8968729072806,70.9953306900575,71.0955532578301,71.1938328155582,71.2920793946317,
71.39032247767,71.4920196663122,71.590404079731,71.693757655985,71.7971112322389,
71.902834090551,72.0081993817376,72.1133399321502,72.2181701837246,72.2566308185778),
 .UNSPECIFIED.);
#564=B_SPLINE_CURVE_WITH_KNOTS('',3,(#56283,#56284,#56285,#56286,#56287,
#56288),.UNSPECIFIED.,.F.,.F.,(4,1,1,4),(72.2566310325654,72.7959476822008,
73.7947841321626,74.4816441310534),.UNSPECIFIED.);
#565=B_SPLINE_CURVE_WITH_KNOTS('',3,(#56290,#56291,#56292,#56293,#56294,
#56295,#56296),.UNSPECIFIED.,.F.,.F.,(4,1,1,1,4),(72.2566310325654,72.3311409496812,
73.3299773996431,74.3288138496049,74.4832630646979),.UNSPECIFIED.);
#566=B_SPLINE_CURVE_WITH_KNOTS('',3,(#56297,#56298,#56299,#56300,#56301,
#56302,#56303,#56304,#56305,#56306,#56307,#56308,#56309,#56310,#56311,#56312,
#56313,#56314,#56315,#56316,#56317,#56318,#56319,#56320,#56321,#56322,#56323,
#56324,#56325,#56326,#56327,#56328,#56329,#56330,#56331,#56332,#56333,#56334,
#56335,#56336,#56337,#56338,#56339,#56340,#56341,#56342,#56343,#56344,#56345,
#56346,#56347,#56348,#56349,#56350,#56351,#56352,#56353,#56354,#56355,#56356,
#56357,#56358,#56359,#56360,#56361,#56362,#56363,#56364,#56365,#56366,#56367,
#56368,#56369,#56370,#56371,#56372,#56373,#56374,#56375,#56376,#56377,#56378,
#56379,#56380,#56381,#56382,#56383,#56384,#56385,#56386,#56387,#56388,#56389,
#56390,#56391,#56392,#56393,#56394,#56395,#56396,#56397,#56398,#56399,#56400,
#56401,#56402,#56403,#56404,#56405,#56406,#56407,#56408,#56409,#56410,#56411,
#56412,#56413,#56414,#56415,#56416,#56417,#56418,#56419,#56420,#56421,#56422,
#56423),.UNSPECIFIED.,.F.,.F.,(4,3,3,3,3,3,3,3,3,3,3,3,3,3,3,3,3,3,3,3,
3,3,3,3,3,3,3,3,3,3,3,3,3,3,3,3,3,3,3,3,3,3,4),(68.1987515107913,68.2973434681129,
68.3357951498337,68.4343932748374,68.5328510576141,68.6330736253868,68.7313531831149,
68.8295997621883,68.9278428452268,69.029540033869,69.1279244472878,69.2312780235417,
69.3346315997956,69.4332297247993,69.531687507576,69.6319100753487,69.7301896330768,
69.8284362121502,69.9266792951887,70.0283764838309,70.1267608972497,70.2301144735035,
70.3334680497574,70.4320661747611,70.5305239575379,70.6307465253105,70.7290260830387,
70.8272726621121,70.9255157451506,71.0272129337928,71.1255973472116,71.2289509234654,
71.3323044997193,71.4298807240688,71.527317634942,71.6246428433669,71.7219081150619,
71.8191441424516,71.9163815796695,72.013708783522,72.1110862397604,72.208614546431,
72.2566310325654),.UNSPECIFIED.);
#567=B_SPLINE_CURVE_WITH_KNOTS('',3,(#56429,#56430,#56431,#56432,#56433,
#56434,#56435,#56436),.UNSPECIFIED.,.F.,.F.,(4,1,1,1,1,4),(61.9167164933236,
62.807583182582,63.8064196325439,64.8052560825058,65.8040925324676,65.9734457253857),
 .UNSPECIFIED.);
#568=B_SPLINE_CURVE_WITH_KNOTS('',3,(#56437,#56438,#56439,#56440,#56441,
#56442,#56443,#56444,#56445,#56446,#56447,#56448,#56449,#56450,#56451,#56452,
#56453,#56454,#56455,#56456,#56457,#56458,#56459,#56460,#56461,#56462,#56463,
#56464,#56465,#56466,#56467,#56468,#56469,#56470,#56471,#56472,#56473,#56474,
#56475,#56476,#56477,#56478,#56479,#56480,#56481,#56482,#56483,#56484,#56485,
#56486,#56487,#56488,#56489,#56490,#56491,#56492,#56493,#56494,#56495,#56496,
#56497,#56498,#56499,#56500,#56501,#56502,#56503,#56504,#56505,#56506),
 .UNSPECIFIED.,.F.,.F.,(4,3,3,3,3,3,3,3,3,3,3,3,3,3,3,3,3,3,3,3,3,3,3,4),
(65.9734457253857,66.0704340596178,66.1673127975358,66.264132888756,66.360925426791,
66.4577214670338,66.5546134226801,66.6515579893415,66.7486626585398,66.8029289824295,
66.9015271074332,66.9999848902101,67.1002074579828,67.198487015711,67.2967335947843,
67.3949766778228,67.496673866465,67.5950582798838,67.6984118561376,67.8017654323914,
67.9012212233955,67.9996662412379,68.0996274188227,68.1995885964076),
 .UNSPECIFIED.);
#569=B_SPLINE_CURVE_WITH_KNOTS('',3,(#56508,#56509,#56510,#56511,#56512,
#56513,#56514,#56515,#56516,#56517,#56518,#56519,#56520,#56521,#56522,#56523,
#56524,#56525,#56526,#56527,#56528,#56529,#56530,#56531,#56532,#56533,#56534,
#56535,#56536,#56537,#56538,#56539,#56540,#56541,#56542,#56543,#56544,#56545,
#56546,#56547,#56548,#56549,#56550,#56551,#56552,#56553,#56554,#56555,#56556,
#56557,#56558,#56559,#56560,#56561,#56562,#56563,#56564,#56565,#56566,#56567,
#56568,#56569,#56570,#56571,#56572,#56573,#56574,#56575,#56576,#56577),
 .UNSPECIFIED.,.F.,.F.,(4,3,3,3,3,3,3,3,3,3,3,3,3,3,3,3,3,3,3,3,3,3,3,4),
(65.9734457256204,66.0848798050736,66.1968635637033,66.3094957826818,66.3381222499099,
66.4367203749136,66.5351781576903,66.635400725463,66.7336802831912,66.8319268622646,
66.930169945303,67.0318671339452,67.130251547364,67.2336051236179,67.3369586998718,
67.4355663370596,67.5340045943448,67.6323466348067,67.7306220560095,67.828860384381,
67.9271329658743,68.0254205103658,68.123818393505,68.1987515107913),
 .UNSPECIFIED.);
#570=B_SPLINE_CURVE_WITH_KNOTS('',3,(#56578,#56579,#56580,#56581,#56582,
#56583,#56584,#56585,#56586,#56587,#56588,#56589,#56590,#56591,#56592,#56593,
#56594,#56595,#56596,#56597,#56598,#56599,#56600,#56601,#56602,#56603,#56604,
#56605,#56606,#56607,#56608,#56609,#56610,#56611,#56612,#56613,#56614,#56615,
#56616,#56617,#56618,#56619,#56620,#56621,#56622,#56623,#56624,#56625,#56626,
#56627,#56628,#56629,#56630,#56631,#56632,#56633,#56634,#56635,#56636,#56637,
#56638,#56639,#56640,#56641,#56642,#56643,#56644,#56645,#56646,#56647,#56648,
#56649,#56650,#56651,#56652,#56653,#56654,#56655,#56656,#56657,#56658,#56659,
#56660,#56661,#56662,#56663,#56664,#56665,#56666,#56667,#56668,#56669,#56670,
#56671,#56672,#56673,#56674,#56675,#56676,#56677,#56678,#56679,#56680,#56681,
#56682,#56683,#56684,#56685,#56686,#56687,#56688,#56689,#56690,#56691,#56692,
#56693,#56694,#56695,#56696,#56697,#56698,#56699,#56700,#56701,#56702,#56703,
#56704),.UNSPECIFIED.,.F.,.F.,(4,3,3,3,3,3,3,3,3,3,3,3,3,3,3,3,3,3,3,3,
3,3,3,3,3,3,3,3,3,3,3,3,3,3,3,3,3,3,3,3,3,3,4),(61.9158792705717,62.0141406127527,
62.1125120200468,62.2109478399191,62.3095423749078,62.3427764500624,62.4413745750661,
62.539832357843,62.6400549256157,62.7383344833438,62.8365810624172,62.9348241454557,
63.0365213340979,63.1349057475167,63.2382593237705,63.3416129000243,63.440211025028,
63.5386688078047,63.6388913755774,63.7371709333055,63.835417512379,63.9336605954174,
64.0353577840596,64.1337421974785,64.2370957737323,64.3404493499862,64.4390474749899,
64.5375052577665,64.6377278255392,64.7360073832674,64.8342539623408,64.9324970453791,
65.0341942340214,65.13257864744,65.2359322236941,65.3392857999481,65.4384637976085,
65.53749807745,65.6364173808604,65.7352455972606,65.8340208922139,65.932784900221,
65.9734457253857),.UNSPECIFIED.);
#571=B_SPLINE_CURVE_WITH_KNOTS('',3,(#56710,#56711,#56712,#56713,#56714,
#56715,#56716,#56717,#56718,#56719,#56720,#56721,#56722,#56723,#56724,#56725,
#56726,#56727,#56728,#56729,#56730,#56731,#56732,#56733,#56734,#56735,#56736,
#56737,#56738,#56739,#56740,#56741,#56742,#56743,#56744,#56745,#56746,#56747,
#56748,#56749,#56750,#56751,#56752,#56753,#56754,#56755,#56756,#56757,#56758,
#56759,#56760,#56761,#56762,#56763,#56764,#56765,#56766,#56767,#56768,#56769,
#56770,#56771,#56772,#56773,#56774,#56775,#56776,#56777,#56778,#56779,#56780,
#56781,#56782,#56783,#56784,#56785,#56786,#56787,#56788,#56789,#56790,#56791,
#56792,#56793,#56794,#56795,#56796,#56797,#56798,#56799,#56800,#56801,#56802,
#56803,#56804,#56805,#56806,#56807,#56808,#56809,#56810,#56811,#56812,#56813,
#56814,#56815,#56816,#56817,#56818,#56819,#56820,#56821,#56822,#56823,#56824,
#56825,#56826,#56827,#56828,#56829,#56830,#56831,#56832,#56833),
 .UNSPECIFIED.,.F.,.F.,(4,3,3,3,3,3,3,3,3,3,3,3,3,3,3,3,3,3,3,3,3,3,3,3,
3,3,3,3,3,3,3,3,3,3,3,3,3,3,3,3,3,4),(55.6323252053611,55.7308982696372,
55.8157280328489,55.9143261578526,56.0127839406294,56.1130065084021,56.2112860661302,
56.3095326452036,56.4077757282421,56.5094729168843,56.6078573303031,56.7112109065569,
56.8145644828108,56.9131626078145,57.0116203905912,57.1118429583639,57.210122516092,
57.3083690951654,57.4066121782039,57.5083093668461,57.6066937802649,57.7100473565188,
57.8134009327727,57.9119990577764,58.0104568405531,58.1106794083258,58.2089589660539,
58.3072055451273,58.4054486281658,58.5071458168079,58.6055302302267,58.7088838064806,
58.8122373827345,58.9094791608007,59.0070768179764,59.1040671063403,59.2009981633324,
59.2979009849176,59.3959908432397,59.4929780422904,59.5916192302483,59.6902604182062),
 .UNSPECIFIED.);
#572=B_SPLINE_CURVE_WITH_KNOTS('',3,(#56834,#56835,#56836,#56837,#56838,
#56839,#56840),.UNSPECIFIED.,.F.,.F.,(4,1,1,1,4),(59.6902604182062,59.8110738326964,
60.8099102826583,61.8087467326202,61.9167164933236),.UNSPECIFIED.);
#573=B_SPLINE_CURVE_WITH_KNOTS('',3,(#56842,#56843,#56844,#56845,#56846,
#56847,#56848,#56849,#56850,#56851,#56852,#56853,#56854,#56855,#56856,#56857,
#56858,#56859,#56860,#56861,#56862,#56863,#56864,#56865,#56866,#56867,#56868,
#56869,#56870,#56871,#56872,#56873,#56874,#56875,#56876,#56877,#56878,#56879,
#56880,#56881,#56882,#56883,#56884,#56885,#56886,#56887,#56888,#56889,#56890,
#56891,#56892,#56893,#56894,#56895,#56896,#56897,#56898,#56899,#56900,#56901,
#56902,#56903,#56904,#56905,#56906,#56907,#56908,#56909,#56910,#56911),
 .UNSPECIFIED.,.F.,.F.,(4,3,3,3,3,3,3,3,3,3,3,3,3,3,3,3,3,3,3,3,3,3,3,4),
(59.6902604182062,59.788634173056,59.886998581597,59.9853827919993,60.0838846667643,
60.1824499292137,60.2811933482975,60.3451035501387,60.4437016751424,60.542159457919,
60.6423820256917,60.7406615834199,60.8389081624932,60.9371512455317,61.0388484341739,
61.1372328475927,61.2405864238466,61.3439400001006,61.4425291322751,61.5409847704255,
61.639327281874,61.7376024228517,61.8358589218597,61.9158792705717),
 .UNSPECIFIED.);
#574=B_SPLINE_CURVE_WITH_KNOTS('',3,(#56912,#56913,#56914,#56915,#56916,
#56917,#56918,#56919,#56920,#56921,#56922,#56923,#56924,#56925,#56926,#56927,
#56928,#56929,#56930,#56931,#56932,#56933,#56934,#56935,#56936,#56937,#56938,
#56939,#56940,#56941,#56942,#56943,#56944,#56945,#56946,#56947,#56948,#56949,
#56950,#56951,#56952,#56953,#56954,#56955,#56956,#56957,#56958,#56959,#56960,
#56961,#56962,#56963,#56964,#56965,#56966,#56967,#56968,#56969,#56970,#56971,
#56972,#56973,#56974,#56975,#56976,#56977,#56978,#56979,#56980,#56981,#56982,
#56983,#56984,#56985,#56986,#56987,#56988,#56989,#56990,#56991,#56992,#56993,
#56994,#56995,#56996,#56997,#56998,#56999,#57000,#57001,#57002,#57003,#57004,
#57005,#57006,#57007,#57008,#57009,#57010,#57011,#57012,#57013,#57014,#57015,
#57016,#57017,#57018,#57019,#57020,#57021,#57022,#57023,#57024,#57025,#57026,
#57027,#57028,#57029,#57030,#57031,#57032,#57033,#57034,#57035),
 .UNSPECIFIED.,.F.,.F.,(4,3,3,3,3,3,3,3,3,3,3,3,3,3,3,3,3,3,3,3,3,3,3,3,
3,3,3,3,3,3,3,3,3,3,3,3,3,3,3,3,3,4),(55.633462551168,55.73174959566,55.8299992392,
55.9282409685686,56.0265042540639,56.1248785008508,56.2233186112086,56.3219159061656,
56.3497577502912,56.4483558752949,56.5468136580715,56.6470362258442,56.7453157835724,
56.8435623626458,56.9418054456843,57.0435026343265,57.1418870477454,57.2452406239993,
57.3485942002531,57.4471923252568,57.5456501080335,57.6458726758062,57.7441522335343,
57.8423988126077,57.9406418956462,58.0423390842884,58.1407234977072,58.244077073961,
58.3474306502149,58.4460287752184,58.5444865579953,58.644709125768,58.7429886834962,
58.8412352625695,58.9394783456081,59.0411755342503,59.1395599476691,59.242913523923,
59.3462671001768,59.4608829140295,59.5755716660044,59.6902604179793),
 .UNSPECIFIED.);
#575=B_SPLINE_CURVE_WITH_KNOTS('',3,(#57041,#57042,#57043,#57044,#57045,
#57046,#57047,#57048),.UNSPECIFIED.,.F.,.F.,(4,1,1,1,1,4),(49.3495871987639,
49.8227093330777,50.8215457830395,51.8203822330014,52.8192186829633,53.4070751110266),
 .UNSPECIFIED.);
#576=B_SPLINE_CURVE_WITH_KNOTS('',3,(#57049,#57050,#57051,#57052,#57053,
#57054,#57055,#57056,#57057,#57058,#57059,#57060,#57061,#57062,#57063,#57064,
#57065,#57066,#57067,#57068,#57069,#57070,#57071,#57072,#57073,#57074,#57075,
#57076,#57077,#57078,#57079,#57080,#57081,#57082,#57083,#57084,#57085,#57086,
#57087,#57088,#57089,#57090,#57091,#57092,#57093,#57094,#57095,#57096,#57097,
#57098,#57099,#57100,#57101,#57102,#57103,#57104,#57105,#57106,#57107,#57108,
#57109,#57110,#57111,#57112,#57113,#57114,#57115,#57116,#57117,#57118),
 .UNSPECIFIED.,.F.,.F.,(4,3,3,3,3,3,3,3,3,3,3,3,3,3,3,3,3,3,3,3,3,3,3,4),
(53.4070755243676,53.5149520672777,53.623163861073,53.7318758460237,53.8180551329252,
53.9166532579289,54.0151110407056,54.1153336084783,54.2136131662064,54.3118597452797,
54.4101028283182,54.5118000169604,54.6101844303792,54.7135380066331,54.816891582887,
54.9188207856963,55.0172568628781,55.1155965182368,55.2138693497382,55.3121048835941,
55.4103643250343,55.5086391377704,55.6069975900418,55.6323252053611),
 .UNSPECIFIED.);
#577=B_SPLINE_CURVE_WITH_KNOTS('',3,(#57120,#57121,#57122,#57123,#57124,
#57125,#57126,#57127,#57128,#57129,#57130,#57131,#57132,#57133,#57134,#57135,
#57136,#57137,#57138,#57139,#57140,#57141,#57142,#57143,#57144,#57145,#57146,
#57147,#57148,#57149,#57150,#57151,#57152,#57153,#57154,#57155,#57156,#57157,
#57158,#57159,#57160,#57161,#57162,#57163,#57164,#57165,#57166,#57167,#57168,
#57169,#57170,#57171,#57172,#57173,#57174,#57175,#57176,#57177,#57178,#57179,
#57180,#57181,#57182,#57183,#57184,#57185,#57186,#57187,#57188,#57189),
 .UNSPECIFIED.,.F.,.F.,(4,3,3,3,3,3,3,3,3,3,3,3,3,3,3,3,3,3,3,3,3,3,3,4),
(53.4070751110266,53.5048543854907,53.6024983707772,53.7000367768846,53.7975186210126,
53.8949743677963,53.9924344477706,54.0899931990358,54.1876041339868,54.2853815723763,
54.3520848503674,54.4506829753711,54.5491407581476,54.6493633259203,54.7476428836485,
54.8458894627219,54.9441325457605,55.0458297344027,55.1442141478214,55.2475677240754,
55.3509213003293,55.449511235452,55.5479503969111,55.633462551168),
 .UNSPECIFIED.);
#578=B_SPLINE_CURVE_WITH_KNOTS('',3,(#57190,#57191,#57192,#57193,#57194,
#57195,#57196,#57197,#57198),.UNSPECIFIED.,.F.,.F.,(4,1,1,1,1,1,4),(49.349677120857,
49.3579026005581,50.3567390505199,51.3555755004818,52.3544119504437,53.3532484004056,
53.4070751110266),.UNSPECIFIED.);
#579=B_SPLINE_CURVE_WITH_KNOTS('',3,(#57204,#57205,#57206,#57207,#57208,
#57209,#57210,#57211,#57212,#57213,#57214,#57215,#57216,#57217,#57218,#57219,
#57220,#57221,#57222,#57223,#57224,#57225,#57226,#57227,#57228,#57229,#57230,
#57231,#57232,#57233,#57234,#57235,#57236,#57237,#57238,#57239,#57240,#57241,
#57242,#57243,#57244,#57245,#57246,#57247,#57248,#57249,#57250,#57251,#57252,
#57253,#57254,#57255,#57256,#57257,#57258,#57259,#57260,#57261,#57262,#57263,
#57264,#57265,#57266,#57267,#57268,#57269,#57270,#57271,#57272,#57273,#57274,
#57275,#57276,#57277,#57278,#57279,#57280,#57281,#57282,#57283,#57284,#57285,
#57286,#57287,#57288,#57289,#57290,#57291,#57292,#57293,#57294,#57295,#57296,
#57297,#57298,#57299,#57300,#57301,#57302,#57303,#57304,#57305,#57306,#57307,
#57308,#57309,#57310,#57311,#57312,#57313,#57314,#57315,#57316,#57317,#57318,
#57319,#57320,#57321,#57322,#57323,#57324,#57325,#57326,#57327),
 .UNSPECIFIED.,.F.,.F.,(4,3,3,3,3,3,3,3,3,3,3,3,3,3,3,3,3,3,3,3,3,3,3,3,
3,3,3,3,3,3,3,3,3,3,3,3,3,3,3,3,3,4),(43.0671358462258,43.1654506957331,
43.2637142592363,43.3619560404535,43.4602055141326,43.5585579558209,43.6569638005109,
43.7555405747165,43.8296906333064,43.9282887583114,44.0267465410897,44.126969108862,
44.2252486665916,44.3234952456665,44.4217383287065,44.523435517347,44.6218199307672,
44.7251735070178,44.8285270832683,44.9271252082715,45.025582991048,45.1258055588207,
45.2240851165484,45.3223316956214,45.4205747786595,45.5222719673022,45.6206563807206,
45.7240099569754,45.8273635332302,45.9259616582337,46.0244194410101,46.1246420087828,
46.2229215665108,46.3211681455839,46.4194112286225,46.5211084172648,46.6194928306836,
46.7228464069378,46.826199983192,46.9466622822351,47.0654828012647,47.1238896269613),
 .UNSPECIFIED.);
#580=B_SPLINE_CURVE_WITH_KNOTS('',3,(#57328,#57329,#57330,#57331,#57332,
#57333),.UNSPECIFIED.,.F.,.F.,(4,1,1,4),(47.123889803847,47.8250364331539,
48.8238728831158,49.3495871987639),.UNSPECIFIED.);
#581=B_SPLINE_CURVE_WITH_KNOTS('',3,(#57335,#57336,#57337,#57338,#57339,
#57340),.UNSPECIFIED.,.F.,.F.,(4,1,1,4),(47.1238901028405,47.3602297006343,
48.3590661505962,49.349677120857),.UNSPECIFIED.);
#582=B_SPLINE_CURVE_WITH_KNOTS('',3,(#57341,#57342,#57343,#57344,#57345,
#57346,#57347,#57348,#57349,#57350,#57351,#57352,#57353,#57354,#57355,#57356,
#57357,#57358,#57359,#57360,#57361,#57362,#57363,#57364,#57365,#57366,#57367,
#57368,#57369,#57370,#57371,#57372,#57373,#57374,#57375,#57376,#57377,#57378,
#57379,#57380,#57381,#57382,#57383,#57384,#57385,#57386,#57387,#57388,#57389,
#57390,#57391,#57392,#57393,#57394,#57395,#57396,#57397,#57398,#57399,#57400,
#57401,#57402,#57403,#57404,#57405,#57406,#57407,#57408,#57409,#57410,#57411,
#57412,#57413,#57414,#57415,#57416,#57417,#57418,#57419,#57420,#57421,#57422,
#57423,#57424,#57425,#57426,#57427,#57428,#57429,#57430,#57431,#57432,#57433,
#57434,#57435,#57436,#57437,#57438,#57439,#57440,#57441,#57442,#57443,#57444,
#57445,#57446,#57447,#57448,#57449,#57450,#57451,#57452,#57453,#57454,#57455,
#57456,#57457,#57458,#57459,#57460,#57461,#57462,#57463,#57464),
 .UNSPECIFIED.,.F.,.F.,(4,3,3,3,3,3,3,3,3,3,3,3,3,3,3,3,3,3,3,3,3,3,3,3,
3,3,3,3,3,3,3,3,3,3,3,3,3,3,3,3,3,4),(43.0660207909132,43.1644088987463,
43.2646463997666,43.3648839007868,43.4634820258002,43.5619398085867,43.6621623763569,
43.7604419340952,43.8586885131787,43.9569315962273,44.0586287848577,44.1570131982869,
44.2603667745178,44.3637203507487,44.4623184757497,44.5607762585238,44.6609988262972,
44.7592783840227,44.8575249630933,44.955768046129,45.0574652347744,45.1558496481904,
45.2592032244505,45.3625568007106,45.4611549257133,45.5596127084892,45.6598352762621,
45.758114833989,45.8563614130613,45.9546044960985,46.056301684742,46.1546860981596,
46.258039674416,46.3613932506724,46.4587199838046,46.5559210250953,46.6530274701202,
46.7500702965176,46.8471124553619,46.9441490048062,47.0412721236582,47.123889803847),
 .UNSPECIFIED.);
#583=B_SPLINE_CURVE_WITH_KNOTS('',3,(#57470,#57471,#57472,#57473,#57474,
#57475,#57476,#57477,#57478,#57479,#57480,#57481,#57482,#57483,#57484,#57485,
#57486,#57487,#57488,#57489,#57490,#57491,#57492,#57493,#57494,#57495,#57496,
#57497,#57498,#57499,#57500,#57501,#57502,#57503,#57504,#57505,#57506,#57507,
#57508,#57509,#57510,#57511,#57512,#57513,#57514,#57515,#57516,#57517,#57518,
#57519,#57520,#57521,#57522,#57523,#57524,#57525,#57526,#57527,#57528,#57529,
#57530,#57531,#57532,#57533,#57534,#57535,#57536,#57537,#57538,#57539,#57540,
#57541,#57542,#57543,#57544,#57545,#57546,#57547,#57548,#57549,#57550,#57551,
#57552,#57553,#57554,#57555,#57556,#57557,#57558,#57559,#57560,#57561,#57562,
#57563,#57564,#57565,#57566,#57567,#57568,#57569,#57570,#57571,#57572,#57573,
#57574,#57575,#57576,#57577,#57578,#57579,#57580,#57581,#57582,#57583,#57584,
#57585,#57586,#57587,#57588,#57589,#57590,#57591,#57592,#57593,#57594,#57595,
#57596),.UNSPECIFIED.,.F.,.F.,(4,3,3,3,3,3,3,3,3,3,3,3,3,3,3,3,3,3,3,3,
3,3,3,3,3,3,3,3,3,3,3,3,3,3,3,3,3,3,3,3,3,3,4),(36.7830721337714,36.8378354835733,
36.9364336084865,37.034891391171,37.1351139589665,37.2333935165987,37.3316400955748,
37.429883178515,37.5315803672701,37.6299647805889,37.7333183570621,37.8366719335352,
37.9352700586078,38.0337278414544,38.1339504092097,38.2322299670096,38.3304765461552,
38.4287196292664,38.530416817824,38.6288012313159,38.7321548074064,38.835508383497,
38.9341065084864,39.0325642912487,39.132786859025,39.2310664167387,39.3293129957976,
39.4275560788218,39.5292532674811,39.6276376808857,39.7309912571723,39.8343448334589,
39.9329429584521,40.0314007412181,40.1316233089935,40.2299028667104,40.3281494457725,
40.4263925287994,40.5280897174548,40.6264741308618,40.7298277071413,40.8331812834208,
40.8407044966674),.UNSPECIFIED.);
#584=B_SPLINE_CURVE_WITH_KNOTS('',3,(#57597,#57598,#57599,#57600,#57601,
#57602,#57603,#57604,#57605,#57606,#57607,#57608,#57609,#57610,#57611,#57612,
#57613,#57614,#57615,#57616,#57617,#57618,#57619,#57620,#57621,#57622,#57623,
#57624,#57625,#57626,#57627,#57628,#57629,#57630,#57631,#57632,#57633,#57634,
#57635,#57636,#57637,#57638,#57639,#57640,#57641,#57642,#57643,#57644,#57645,
#57646,#57647,#57648,#57649,#57650,#57651,#57652,#57653,#57654,#57655,#57656,
#57657,#57658,#57659,#57660,#57661,#57662,#57663,#57664,#57665,#57666),
 .UNSPECIFIED.,.F.,.F.,(4,3,3,3,3,3,3,3,3,3,3,3,3,3,3,3,3,3,3,3,3,3,3,4),
(40.8407044969197,40.9391705387199,41.0374964280042,41.1368115911765,41.2349607512895,
41.3330774110131,41.4311912274066,41.5313978539006,41.6296531901077,41.7308354617452,
41.8320177333827,41.9306158583837,42.0290736411578,42.1292962089311,42.2275757666566,
42.3258223457272,42.4240654287629,42.5257626174083,42.6241470308245,42.7275006070845,
42.8308541833445,42.929455918813,43.027905177827,43.0671358462258),
 .UNSPECIFIED.);
#585=B_SPLINE_CURVE_WITH_KNOTS('',3,(#57668,#57669,#57670,#57671,#57672,
#57673,#57674,#57675,#57676,#57677,#57678,#57679,#57680,#57681,#57682,#57683,
#57684,#57685,#57686,#57687,#57688,#57689,#57690,#57691,#57692,#57693,#57694,
#57695,#57696,#57697,#57698,#57699,#57700,#57701,#57702,#57703,#57704,#57705,
#57706,#57707,#57708,#57709,#57710,#57711,#57712,#57713,#57714,#57715,#57716,
#57717,#57718,#57719,#57720,#57721,#57722,#57723,#57724,#57725,#57726,#57727,
#57728,#57729,#57730,#57731,#57732,#57733,#57734,#57735,#57736,#57737),
 .UNSPECIFIED.,.F.,.F.,(4,3,3,3,3,3,3,3,3,3,3,3,3,3,3,3,3,3,3,3,3,3,3,4),
(40.8407044966674,40.9425310419931,41.0487010317106,41.1508691915794,41.2531658485544,
41.3556785603232,41.3672110008631,41.4658091258525,41.5642669086152,41.6644894763914,
41.7627690341051,41.8610156131643,41.9592586961885,42.0609558848476,42.1593402982524,
42.2626938745386,42.3660474508249,42.4646234053299,42.5630692109005,42.6614145831975,
42.7625661351264,42.8608128976382,42.9634168442757,43.0660207909132),
 .UNSPECIFIED.);
#586=B_SPLINE_CURVE_WITH_KNOTS('',3,(#57738,#57739,#57740,#57741,#57742,
#57743,#57744,#57745),.UNSPECIFIED.,.F.,.F.,(4,1,1,1,1,4),(36.7838197989548,
37.3718652010156,38.3707016509774,39.3695381009393,40.3683745509012,40.8407024149584),
 .UNSPECIFIED.);
#587=B_SPLINE_CURVE_WITH_KNOTS('',3,(#57751,#57752,#57753,#57754,#57755,
#57756,#57757,#57758,#57759,#57760,#57761,#57762,#57763,#57764,#57765,#57766,
#57767,#57768,#57769,#57770,#57771,#57772,#57773,#57774,#57775,#57776,#57777,
#57778,#57779,#57780,#57781,#57782,#57783,#57784,#57785,#57786,#57787,#57788,
#57789,#57790,#57791,#57792,#57793,#57794,#57795,#57796,#57797,#57798,#57799,
#57800,#57801,#57802,#57803,#57804,#57805,#57806,#57807,#57808,#57809,#57810,
#57811,#57812,#57813,#57814,#57815,#57816,#57817,#57818,#57819,#57820,#57821,
#57822,#57823,#57824,#57825,#57826,#57827,#57828,#57829,#57830,#57831,#57832,
#57833,#57834,#57835,#57836,#57837,#57838,#57839,#57840,#57841,#57842,#57843,
#57844,#57845,#57846,#57847,#57848,#57849,#57850,#57851,#57852,#57853,#57854,
#57855,#57856,#57857,#57858,#57859,#57860,#57861,#57862,#57863,#57864,#57865,
#57866,#57867,#57868,#57869,#57870,#57871,#57872,#57873,#57874,#57875,#57876,
#57877),.UNSPECIFIED.,.F.,.F.,(4,3,3,3,3,3,3,3,3,3,3,3,3,3,3,3,3,3,3,3,
3,3,3,3,3,3,3,3,3,3,3,3,3,3,3,3,3,3,3,3,3,3,4),(30.4997392209955,30.59810244627,
30.6965256522857,30.7951123625252,30.844816783802,30.9434149029147,31.041872679697,
31.1420952489554,31.240374800478,31.3386213732805,31.4368644499908,31.5385616459341,
31.636946052946,31.7402996433549,31.8436532337639,31.9422513619748,32.040709147999,
32.1409317149648,32.2392112760154,32.3374578584321,32.4357009448303,32.5373981295542,
32.6357825463393,32.7391361150326,32.8424896837258,32.9410878085143,33.0395455910813,
33.1397681589071,33.2380477164402,33.3362942953243,33.4345373781799,33.5362345670568,
33.6346189803102,33.737972556999,33.8413261336877,33.93909739415,34.0367388270534,
34.1342810926871,34.2317547370018,34.3292101035708,34.426655495324,34.5241539308998,
34.5575191894878),.UNSPECIFIED.);
#588=B_SPLINE_CURVE_WITH_KNOTS('',3,(#57878,#57879,#57880,#57881,#57882,
#57883,#57884,#57885,#57886,#57887,#57888,#57889,#57890,#57891,#57892,#57893,
#57894,#57895,#57896,#57897,#57898,#57899,#57900,#57901,#57902,#57903,#57904,
#57905,#57906,#57907,#57908,#57909,#57910,#57911,#57912,#57913,#57914,#57915,
#57916,#57917,#57918,#57919,#57920,#57921,#57922,#57923,#57924,#57925,#57926,
#57927,#57928,#57929,#57930,#57931,#57932,#57933,#57934,#57935,#57936,#57937,
#57938,#57939,#57940,#57941,#57942,#57943,#57944,#57945,#57946,#57947),
 .UNSPECIFIED.,.F.,.F.,(4,3,3,3,3,3,3,3,3,3,3,3,3,3,3,3,3,3,3,3,3,3,3,4),
(34.5575191897594,34.6782345503608,34.8009387396036,34.8401625836495,34.9387607091287,
35.0372184923873,35.1374410600403,35.2357206182623,35.333967197833,35.4322102813716,
35.5339074694315,35.6322918833522,35.7356454584818,35.8389990336114,35.9376008413507,
36.036061306603,36.1344037647034,36.2326817408431,36.3309247589446,36.429162301612,
36.5274785677215,36.6258371036485,36.7243383500844,36.7830721337714),
 .UNSPECIFIED.);
#589=B_SPLINE_CURVE_WITH_KNOTS('',3,(#57949,#57950,#57951,#57952,#57953,
#57954),.UNSPECIFIED.,.F.,.F.,(4,1,1,4),(34.5575241471828,35.3741923010918,
36.3730287510537,36.7838197989548),.UNSPECIFIED.);
#590=B_SPLINE_CURVE_WITH_KNOTS('',3,(#57955,#57956,#57957,#57958,#57959,
#57960,#57961,#57962,#57963,#57964,#57965,#57966,#57967,#57968,#57969,#57970,
#57971,#57972,#57973,#57974,#57975,#57976,#57977,#57978,#57979,#57980,#57981,
#57982,#57983,#57984,#57985,#57986,#57987,#57988,#57989,#57990,#57991,#57992,
#57993,#57994,#57995,#57996,#57997,#57998,#57999,#58000,#58001,#58002,#58003,
#58004,#58005,#58006,#58007,#58008,#58009,#58010,#58011,#58012,#58013,#58014,
#58015,#58016,#58017,#58018,#58019,#58020,#58021,#58022,#58023,#58024,#58025,
#58026,#58027,#58028,#58029,#58030,#58031,#58032,#58033,#58034,#58035,#58036,
#58037,#58038,#58039,#58040,#58041,#58042,#58043,#58044,#58045,#58046,#58047,
#58048,#58049,#58050,#58051,#58052,#58053,#58054,#58055,#58056,#58057,#58058,
#58059,#58060,#58061,#58062,#58063,#58064,#58065,#58066,#58067,#58068,#58069,
#58070,#58071,#58072,#58073,#58074,#58075,#58076,#58077,#58078),
 .UNSPECIFIED.,.F.,.F.,(4,3,3,3,3,3,3,3,3,3,3,3,3,3,3,3,3,3,3,3,3,3,3,3,
3,3,3,3,3,3,3,3,3,3,3,3,3,3,3,3,3,4),(30.5006744577879,30.5991052616483,
30.6974320572743,30.7957024061211,30.893945819764,30.9921917761612,31.0905375611812,
31.1889321228201,31.2875030639315,31.3788465012443,31.4774446472309,31.575902451235,
31.6761250137314,31.7744045931314,31.8726511939953,31.9708942989141,32.0725914619871,
32.1709758972869,32.2743294242465,32.3776829512062,32.4762810765969,32.5747388598271,
32.6749614274947,32.7732409858373,32.871487565584,32.9697306493543,33.0714278373078,
33.1698122515977,33.2731658263829,33.3765194011681,33.4751175203039,33.5735752971096,
33.6737978663622,33.7720774179092,33.8703239907363,33.9685670674716,34.0702642633862,
34.1686486704234,34.2720022607767,34.37535585113,34.5238559809678,34.5575191894878),
 .UNSPECIFIED.);
#591=B_SPLINE_CURVE_WITH_KNOTS('',3,(#58084,#58085,#58086,#58087,#58088,
#58089,#58090,#58091),.UNSPECIFIED.,.F.,.F.,(4,1,1,1,1,4),(24.2176478214031,
24.8517980840308,25.8506345339927,26.8494709839545,27.8483074339164,28.2743284148014),
 .UNSPECIFIED.);
#592=B_SPLINE_CURVE_WITH_KNOTS('',3,(#58092,#58093,#58094,#58095,#58096,
#58097,#58098,#58099,#58100,#58101,#58102,#58103,#58104,#58105,#58106,#58107,
#58108,#58109,#58110,#58111,#58112,#58113,#58114,#58115,#58116,#58117,#58118,
#58119,#58120,#58121,#58122,#58123,#58124,#58125,#58126,#58127,#58128,#58129,
#58130,#58131,#58132,#58133,#58134,#58135,#58136,#58137,#58138,#58139,#58140,
#58141,#58142,#58143,#58144,#58145,#58146,#58147,#58148,#58149,#58150,#58151,
#58152,#58153,#58154,#58155,#58156,#58157,#58158,#58159,#58160,#58161),
 .UNSPECIFIED.,.F.,.F.,(4,3,3,3,3,3,3,3,3,3,3,3,3,3,3,3,3,3,3,3,3,3,3,4),
(28.2743338823082,28.3746245106346,28.4749734038757,28.575488632026,28.6760922702813,
28.7769068624063,28.8471438838783,28.9457420299521,29.0441998340446,29.144422396519,
29.2427019760093,29.340948576964,29.4391916819737,29.5408888449403,29.6392732803313,
29.7426268070858,29.8459803338402,29.9445606477205,30.0430096057643,30.1413569295321,
30.2396381186445,30.3378792535306,30.4361386871608,30.4997392209955),
 .UNSPECIFIED.);
#593=B_SPLINE_CURVE_WITH_KNOTS('',3,(#58163,#58164,#58165,#58166,#58167,
#58168,#58169,#58170,#58171,#58172,#58173,#58174,#58175,#58176,#58177,#58178,
#58179,#58180,#58181,#58182,#58183,#58184,#58185,#58186,#58187,#58188,#58189,
#58190,#58191,#58192,#58193,#58194,#58195,#58196,#58197,#58198,#58199,#58200,
#58201,#58202,#58203,#58204,#58205,#58206,#58207,#58208,#58209,#58210,#58211,
#58212,#58213,#58214,#58215,#58216,#58217,#58218,#58219,#58220,#58221,#58222,
#58223,#58224,#58225,#58226,#58227,#58228,#58229,#58230,#58231,#58232),
 .UNSPECIFIED.,.F.,.F.,(4,3,3,3,3,3,3,3,3,3,3,3,3,3,3,3,3,3,3,3,3,3,3,4),
(28.2743338823082,28.3823371513587,28.4809354100483,28.5793933279209,28.6796158620959,
28.7778955573906,28.876142274651,28.9743854963144,29.0760825225659,29.1744670742836,
29.2778203378021,29.3811736013206,29.47977174272,29.5782295425626,29.6784521061526,
29.7767316824779,29.8749782806812,29.9732213833591,30.07491855034,30.173302984478,
30.2766565178802,30.3800100512825,30.4786103666735,30.5006744577879),
 .UNSPECIFIED.);
#594=B_SPLINE_CURVE_WITH_KNOTS('',3,(#58233,#58234,#58235,#58236,#58237,
#58238,#58239,#58240,#58241,#58242,#58243,#58244,#58245,#58246,#58247,#58248,
#58249,#58250,#58251,#58252,#58253,#58254,#58255,#58256,#58257,#58258,#58259,
#58260,#58261,#58262,#58263,#58264,#58265,#58266,#58267,#58268,#58269,#58270,
#58271,#58272,#58273,#58274,#58275,#58276,#58277,#58278,#58279,#58280,#58281,
#58282,#58283,#58284,#58285,#58286,#58287,#58288,#58289,#58290,#58291,#58292,
#58293,#58294,#58295,#58296,#58297,#58298,#58299,#58300,#58301,#58302,#58303,
#58304,#58305,#58306,#58307,#58308,#58309,#58310,#58311,#58312,#58313,#58314,
#58315,#58316,#58317,#58318,#58319,#58320,#58321,#58322,#58323,#58324,#58325,
#58326,#58327,#58328,#58329,#58330,#58331,#58332,#58333,#58334,#58335,#58336,
#58337,#58338,#58339,#58340,#58341,#58342,#58343,#58344,#58345,#58346,#58347,
#58348,#58349,#58350,#58351,#58352,#58353,#58354,#58355,#58356,#58357,#58358,
#58359),.UNSPECIFIED.,.F.,.F.,(4,3,3,3,3,3,3,3,3,3,3,3,3,3,3,3,3,3,3,3,
3,3,3,3,3,3,3,3,3,3,3,3,3,3,3,3,3,3,3,3,3,3,4),(24.2164091264089,24.3149891732794,
24.3869913515112,24.4855869800636,24.5840422282253,24.6842654248812,24.7825423726193,
24.8807863192412,24.9790267507949,25.0807270134645,25.1791087548177,25.2824682781454,
25.3858278014731,25.4844267451928,25.5828853541422,25.6831077163038,25.7813881124234,
25.8796355326055,25.9778794583543,26.0795756566245,26.1779609081003,26.2813125797677,
26.384664251435,26.4832625888131,26.5817205900565,26.681943103974,26.780222893609,
26.8784697091132,26.9767130328096,27.0784099499564,27.1767946121896,27.2801476567932,
27.3835007013968,27.4808124356152,27.5800026164232,27.6770619121749,27.7740624149263,
27.8710350587886,27.9718597646113,28.0689211634457,28.1660361050485,28.2632831532614,
28.2743338820794),.UNSPECIFIED.);
#595=B_SPLINE_CURVE_WITH_KNOTS('',3,(#58365,#58366,#58367,#58368,#58369,
#58370),.UNSPECIFIED.,.F.,.F.,(4,1,1,4),(15.707963267949,16.3962997518162,
17.3951362017781,17.9335273553052),.UNSPECIFIED.);
#596=B_SPLINE_CURVE_WITH_KNOTS('',3,(#58372,#58373,#58374,#58375,#58376),
 .UNSPECIFIED.,.F.,.F.,(4,1,4),(14.3986268518925,15.3974633018543,15.707963267949),
 .UNSPECIFIED.);
#597=B_SPLINE_CURVE_WITH_KNOTS('',3,(#58380,#58381,#58382,#58383,#58384,
#58385,#58386,#58387,#58388,#58389,#58390,#58391,#58392,#58393,#58394,#58395,
#58396,#58397,#58398,#58399,#58400,#58401,#58402,#58403,#58404,#58405,#58406,
#58407,#58408,#58409,#58410,#58411,#58412,#58413,#58414,#58415,#58416,#58417,
#58418,#58419,#58420,#58421,#58422,#58423,#58424,#58425,#58426,#58427,#58428,
#58429,#58430,#58431,#58432,#58433,#58434,#58435,#58436,#58437),
 .UNSPECIFIED.,.F.,.F.,(4,3,3,3,3,3,3,3,3,3,3,3,3,3,3,3,3,3,3,4),(13.8757070305517,
13.9742335889647,14.072619844817,14.1714715622663,14.2696802945035,14.3678559192405,
14.4660280130677,14.5653794059038,14.6636894122209,14.7635614983165,14.8634335844121,
14.9606976622509,15.0578044027615,15.1548229002686,15.2517842042296,15.3487192914879,
15.4457083558909,15.5427241566488,15.6398692495935,15.707963267949),
 .UNSPECIFIED.);
#598=B_SPLINE_CURVE_WITH_KNOTS('',3,(#58438,#58439,#58440,#58441,#58442,
#58443,#58444),.UNSPECIFIED.,.F.,.F.,(4,1,1,1,4),(15.707963267949,15.8622700343739,
16.8611064843358,17.8599429342977,17.9342415897067),.UNSPECIFIED.);
#599=B_SPLINE_CURVE_WITH_KNOTS('',3,(#58450,#58451,#58452,#58453,#58454,
#58455,#58456,#58457),.UNSPECIFIED.,.F.,.F.,(4,1,1,1,1,4),(181.295997105629,
181.669120728045,182.667957178007,183.666793627969,184.665630077931,185.353966561798),
 .UNSPECIFIED.);
#600=B_SPLINE_CURVE_WITH_KNOTS('',3,(#58459,#58460,#58461,#58462,#58463),
 .UNSPECIFIED.,.F.,.F.,(4,1,4),(185.353966561798,185.664466527893,186.663302977854),
 .UNSPECIFIED.);
#601=B_SPLINE_CURVE_WITH_KNOTS('',3,(#58467,#58468,#58469,#58470,#58471,
#58472,#58473,#58474,#58475,#58476,#58477,#58478,#58479,#58480,#58481,#58482,
#58483,#58484,#58485,#58486,#58487,#58488,#58489,#58490,#58491,#58492,#58493,
#58494,#58495,#58496,#58497,#58498,#58499,#58500,#58501,#58502,#58503,#58504,
#58505,#58506,#58507,#58508,#58509,#58510,#58511,#58512,#58513,#58514,#58515,
#58516,#58517,#58518,#58519,#58520,#58521,#58522,#58523,#58524),
 .UNSPECIFIED.,.F.,.F.,(4,3,3,3,3,3,3,3,3,3,3,3,3,3,3,3,3,3,3,4),(185.353966561798,
185.451129862355,185.548173545581,185.645152144533,185.742096651447,185.839038013602,
185.93606867674,186.033145889087,186.130383557083,186.198496245335,186.297012011071,
186.39538977669,186.494243904503,186.592449804335,186.690624726039,186.788798244729,
186.888154383345,186.9864710254,187.086346912297,187.186222799194),
 .UNSPECIFIED.);
#602=B_SPLINE_CURVE_WITH_KNOTS('',3,(#58525,#58526,#58527,#58528,#58529,
#58530,#58531,#58532),.UNSPECIFIED.,.F.,.F.,(4,1,1,1,1,4),(181.297167536261,
182.203150445487,183.201986895449,184.200823345411,185.199659795373,185.353966561798),
 .UNSPECIFIED.);
#603=B_SPLINE_CURVE_WITH_KNOTS('',3,(#58538,#58539,#58540,#58541,#58542,
#58543,#58544,#58545,#58546,#58547,#58548,#58549,#58550,#58551,#58552,#58553,
#58554,#58555,#58556,#58557,#58558,#58559,#58560,#58561,#58562,#58563,#58564,
#58565,#58566,#58567,#58568,#58569,#58570,#58571,#58572,#58573,#58574,#58575,
#58576,#58577,#58578,#58579,#58580,#58581,#58582,#58583,#58584,#58585,#58586,
#58587,#58588,#58589,#58590,#58591,#58592,#58593,#58594,#58595,#58596,#58597,
#58598,#58599,#58600,#58601,#58602,#58603,#58604,#58605,#58606,#58607,#58608,
#58609,#58610,#58611,#58612,#58613,#58614,#58615,#58616,#58617,#58618,#58619,
#58620,#58621,#58622,#58623,#58624,#58625,#58626,#58627,#58628,#58629,#58630,
#58631,#58632,#58633,#58634,#58635,#58636,#58637,#58638,#58639,#58640,#58641,
#58642,#58643,#58644,#58645,#58646,#58647,#58648,#58649,#58650,#58651,#58652,
#58653,#58654,#58655,#58656,#58657,#58658,#58659,#58660,#58661),
 .UNSPECIFIED.,.F.,.F.,(4,3,3,3,3,3,3,3,3,3,3,3,3,3,3,3,3,3,3,3,3,3,3,3,
3,3,3,3,3,3,3,3,3,3,3,3,3,3,3,3,3,4),(175.013888639089,175.112152299112,
175.210394785152,175.308645570523,175.40699968229,175.505407740544,175.60398608652,
175.676102028274,175.774697487766,175.873152601892,175.973375836435,176.07165273689,
176.169896668633,176.268137117691,176.369837457827,176.468219297092,176.571578887664,
176.674938478236,176.773539091296,176.87199934651,176.972221294221,177.070503268971,
177.168752239357,177.266997685028,177.36869199582,177.4670786771,177.570426802649,
177.673774928198,177.772377760441,177.870840294725,177.971061680154,178.069346062747,
178.167597483387,178.265845418215,178.367536908201,178.465926148849,178.569268763504,
178.672611378159,178.782250126366,178.891545491967,179.000249383586,179.070781030157),
 .UNSPECIFIED.);
#604=B_SPLINE_CURVE_WITH_KNOTS('',3,(#58662,#58663,#58664,#58665,#58666,
#58667),.UNSPECIFIED.,.F.,.F.,(4,1,1,4),(179.070781254618,179.671447828121,
180.670284278083,181.295997105629),.UNSPECIFIED.);
#605=B_SPLINE_CURVE_WITH_KNOTS('',3,(#58669,#58670,#58671,#58672,#58673,
#58674,#58675),.UNSPECIFIED.,.F.,.F.,(4,1,1,1,4),(179.070781254618,179.206641095602,
180.205477545564,181.204313995525,181.297167536261),.UNSPECIFIED.);
#606=B_SPLINE_CURVE_WITH_KNOTS('',3,(#58676,#58677,#58678,#58679,#58680,
#58681,#58682,#58683),.UNSPECIFIED.,.F.,.F.,(4,1,1,1,1,4),(175.01254480072,
175.211295295754,176.210131745716,177.208968195678,178.20780464564,179.070781254618),
 .UNSPECIFIED.);
#607=B_SPLINE_CURVE_WITH_KNOTS('',3,(#58689,#58690,#58691,#58692,#58693,
#58694,#58695,#58696,#58697,#58698,#58699,#58700,#58701,#58702,#58703,#58704,
#58705,#58706,#58707,#58708,#58709,#58710,#58711,#58712,#58713,#58714,#58715,
#58716,#58717,#58718,#58719,#58720,#58721,#58722,#58723,#58724,#58725,#58726,
#58727,#58728,#58729,#58730,#58731,#58732,#58733,#58734,#58735,#58736,#58737,
#58738,#58739,#58740,#58741,#58742,#58743,#58744,#58745,#58746,#58747,#58748,
#58749,#58750,#58751,#58752,#58753,#58754,#58755,#58756,#58757,#58758,#58759,
#58760,#58761,#58762,#58763,#58764,#58765,#58766,#58767,#58768,#58769,#58770,
#58771,#58772,#58773,#58774,#58775,#58776,#58777,#58778,#58779,#58780,#58781,
#58782,#58783,#58784,#58785,#58786,#58787,#58788,#58789,#58790,#58791,#58792,
#58793,#58794,#58795,#58796,#58797,#58798,#58799,#58800,#58801,#58802,#58803,
#58804,#58805,#58806,#58807,#58808,#58809,#58810,#58811,#58812),
 .UNSPECIFIED.,.F.,.F.,(4,3,3,3,3,3,3,3,3,3,3,3,3,3,3,3,3,3,3,3,3,3,3,3,
3,3,3,3,3,3,3,3,3,3,3,3,3,3,3,3,3,4),(168.730499527606,168.829027770498,
168.927431080463,169.025741388665,169.124002483085,169.222243864512,169.320495006626,
169.418850351426,169.51726095759,169.615840356468,169.683083328503,169.781681404593,
169.880139138462,169.980361718462,170.078641227646,170.176887758415,170.275130793449,
170.376828039703,170.47521240635,170.578566092407,170.681919778464,170.780517924859,
170.878975728637,170.979198291111,171.07747786875,171.175724467288,171.273967569322,
171.375664734098,171.474049165163,171.577402696795,171.680756228426,171.7793544904,
171.877812410935,171.978034944366,172.07631464078,172.174561358581,172.272804580209,
172.374501604754,172.472886155,172.576239416694,172.679592678388,172.787595947439),
 .UNSPECIFIED.);
#608=B_SPLINE_CURVE_WITH_KNOTS('',3,(#58813,#58814,#58815,#58816,#58817,
#58818,#58819,#58820,#58821,#58822,#58823,#58824,#58825,#58826,#58827,#58828,
#58829,#58830,#58831,#58832,#58833,#58834,#58835,#58836,#58837,#58838,#58839,
#58840,#58841,#58842,#58843,#58844,#58845,#58846,#58847,#58848,#58849,#58850,
#58851,#58852,#58853,#58854,#58855,#58856,#58857,#58858,#58859,#58860,#58861,
#58862,#58863,#58864,#58865,#58866,#58867,#58868,#58869,#58870,#58871,#58872,
#58873,#58874,#58875,#58876,#58877,#58878,#58879,#58880,#58881,#58882,#58883,
#58884,#58885),.UNSPECIFIED.,.F.,.F.,(4,3,3,3,3,3,3,3,3,3,3,3,3,3,3,3,3,
3,3,3,3,3,3,3,4),(172.787595947668,172.884841558898,172.98404000508,173.081071837534,
173.178059269357,173.275033213409,173.375882192145,173.472980625916,173.570144969666,
173.667458407301,173.67842912835,173.777027506426,173.875485539767,173.975708044585,
174.073987845019,174.172234663368,174.270477981962,174.372174881049,174.470559518455,
174.573912548384,174.677265578312,174.775844827615,174.874301066636,174.972645512634,
175.013888639089),.UNSPECIFIED.);
#609=B_SPLINE_CURVE_WITH_KNOTS('',3,(#58887,#58888,#58889,#58890,#58891,
#58892),.UNSPECIFIED.,.F.,.F.,(4,1,1,4),(172.787601414895,173.21362239583,
174.212458845792,175.01254480072),.UNSPECIFIED.);
#610=B_SPLINE_CURVE_WITH_KNOTS('',3,(#58893,#58894,#58895,#58896,#58897,
#58898,#58899,#58900,#58901,#58902,#58903,#58904,#58905,#58906,#58907,#58908,
#58909,#58910,#58911,#58912,#58913,#58914,#58915,#58916,#58917,#58918,#58919,
#58920,#58921,#58922,#58923,#58924,#58925,#58926,#58927,#58928,#58929,#58930,
#58931,#58932,#58933,#58934,#58935,#58936,#58937,#58938,#58939,#58940,#58941,
#58942,#58943,#58944,#58945,#58946,#58947,#58948,#58949,#58950,#58951,#58952,
#58953,#58954,#58955,#58956,#58957,#58958,#58959,#58960,#58961,#58962,#58963,
#58964,#58965,#58966,#58967,#58968,#58969,#58970,#58971,#58972,#58973,#58974,
#58975,#58976,#58977,#58978,#58979,#58980,#58981,#58982,#58983,#58984,#58985,
#58986,#58987,#58988,#58989,#58990,#58991,#58992,#58993,#58994,#58995,#58996,
#58997,#58998,#58999,#59000,#59001,#59002,#59003,#59004,#59005,#59006,#59007,
#59008,#59009,#59010,#59011,#59012,#59013,#59014,#59015,#59016),
 .UNSPECIFIED.,.F.,.F.,(4,3,3,3,3,3,3,3,3,3,3,3,3,3,3,3,3,3,3,3,3,3,3,3,
3,3,3,3,3,3,3,3,3,3,3,3,3,3,3,3,3,4),(168.730215079385,168.828460546878,
168.926805255148,169.02519788847,169.123767925033,169.218276595983,169.316874714587,
169.41533249097,169.515555060342,169.613834611735,169.71208118451,169.810324261293,
169.912021457456,170.010405864791,170.113759455368,170.217113045945,170.31571117192,
170.41416895561,170.514391523147,170.61267108164,170.710917661422,170.809160745111,
170.91085793281,171.009242346733,171.11259592132,171.215949495907,171.314547642641,
171.413005447249,171.513228009576,171.611507589225,171.709754190205,171.807997295108,
171.909694457798,172.008078892752,172.11143241931,172.214785945869,172.315617765141,
172.416285943305,172.516781875028,172.617176498107,172.717484579422,172.787595947439),
 .UNSPECIFIED.);
#611=B_SPLINE_CURVE_WITH_KNOTS('',3,(#59022,#59023,#59024,#59025,#59026,
#59027,#59028,#59029),.UNSPECIFIED.,.F.,.F.,(4,1,1,1,1,4),(162.446146712717,
162.691228178769,163.690064628731,164.688901078693,165.687737528655,166.504405683028),
 .UNSPECIFIED.);
#612=B_SPLINE_CURVE_WITH_KNOTS('',3,(#59030,#59031,#59032,#59033,#59034,
#59035,#59036,#59037,#59038,#59039,#59040,#59041,#59042,#59043,#59044,#59045,
#59046,#59047,#59048,#59049,#59050,#59051,#59052,#59053,#59054,#59055,#59056,
#59057,#59058,#59059,#59060,#59061,#59062,#59063,#59064,#59065,#59066,#59067,
#59068,#59069,#59070,#59071,#59072,#59073,#59074,#59075,#59076,#59077,#59078,
#59079,#59080,#59081,#59082,#59083,#59084,#59085,#59086,#59087,#59088,#59089,
#59090,#59091,#59092,#59093,#59094,#59095,#59096,#59097,#59098,#59099),
 .UNSPECIFIED.,.F.,.F.,(4,3,3,3,3,3,3,3,3,3,3,3,3,3,3,3,3,3,3,3,3,3,3,4),
(166.504410640259,166.65291077017,166.686573978617,166.785172097224,166.883629873609,
166.983852442981,167.082131994377,167.180378567154,167.278621643939,167.380318840099,
167.478703247436,167.582056838008,167.685410428579,167.784008554555,167.882466338245,
167.982688905782,168.080968464275,168.179215044057,168.277458127747,168.379155315446,
168.477539729369,168.580893303955,168.684246878541,168.730499527606),
 .UNSPECIFIED.);
#613=B_SPLINE_CURVE_WITH_KNOTS('',3,(#59101,#59102,#59103,#59104,#59105,
#59106,#59107,#59108,#59109,#59110,#59111,#59112,#59113,#59114,#59115,#59116,
#59117,#59118,#59119,#59120,#59121,#59122,#59123,#59124,#59125,#59126,#59127,
#59128,#59129,#59130,#59131,#59132,#59133,#59134,#59135,#59136,#59137,#59138,
#59139,#59140,#59141,#59142,#59143,#59144,#59145,#59146,#59147,#59148,#59149,
#59150,#59151,#59152,#59153,#59154,#59155,#59156,#59157,#59158,#59159,#59160,
#59161,#59162,#59163,#59164,#59165,#59166,#59167,#59168,#59169,#59170,#59171,
#59172,#59173),.UNSPECIFIED.,.F.,.F.,(4,3,3,3,3,3,3,3,3,3,3,3,3,3,3,3,3,
3,3,3,3,3,3,3,4),(166.504410640259,166.601913126298,166.699371433805,166.796815990355,
166.894277201717,166.99184617322,167.089478292227,167.187269535427,167.220603696059,
167.319201820913,167.417659603532,167.517882171343,167.616161728894,167.714408307783,
167.81265139063,167.914348579478,168.012732992691,168.116086569356,168.219440146021,
168.31803679311,168.421081364679,168.519419916002,168.61769169675,168.715928369161,
168.730215079385),.UNSPECIFIED.);
#614=B_SPLINE_CURVE_WITH_KNOTS('',3,(#59174,#59175,#59176,#59177,#59178,
#59179,#59180,#59181,#59182,#59183,#59184,#59185,#59186,#59187,#59188,#59189,
#59190,#59191,#59192,#59193,#59194,#59195,#59196,#59197,#59198,#59199,#59200,
#59201,#59202,#59203,#59204,#59205,#59206,#59207,#59208,#59209,#59210,#59211,
#59212,#59213,#59214,#59215,#59216,#59217,#59218,#59219,#59220,#59221,#59222,
#59223,#59224,#59225,#59226,#59227,#59228,#59229,#59230,#59231,#59232,#59233,
#59234,#59235,#59236,#59237,#59238,#59239,#59240,#59241,#59242,#59243,#59244,
#59245,#59246,#59247,#59248,#59249,#59250,#59251,#59252,#59253,#59254,#59255,
#59256,#59257,#59258,#59259,#59260,#59261,#59262,#59263,#59264,#59265,#59266,
#59267,#59268,#59269,#59270,#59271,#59272,#59273,#59274,#59275,#59276,#59277,
#59278,#59279,#59280,#59281,#59282,#59283,#59284,#59285,#59286,#59287,#59288,
#59289,#59290,#59291,#59292,#59293,#59294,#59295,#59296,#59297),
 .UNSPECIFIED.,.F.,.F.,(4,3,3,3,3,3,3,3,3,3,3,3,3,3,3,3,3,3,3,3,3,3,3,3,
3,3,3,3,3,3,3,3,3,3,3,3,3,3,3,3,3,4),(162.447662215674,162.545987512034,
162.644257006383,162.742500209215,162.84074659799,162.939093212585,163.037489181463,
163.136060839186,163.225257896212,163.323856021116,163.422313803793,163.52253637159,
163.62081592922,163.719062508196,163.817305591137,163.919002779896,164.017387193222,
164.120740769698,164.224094346174,164.322692471117,164.421150253833,164.52137282162,
164.619652379284,164.717898958293,164.816142041266,164.917839229983,165.016223643335,
165.119577219736,165.222930796136,165.321528921637,165.419986704913,165.520209272561,
165.618488830789,165.71673541036,165.814978493895,165.916675681946,166.015060095852,
166.118413670974,166.221767246097,166.344599874398,166.465474953135,166.504410639987),
 .UNSPECIFIED.);
#615=B_SPLINE_CURVE_WITH_KNOTS('',3,(#59303,#59304,#59305,#59306,#59307,
#59308,#59309,#59310,#59311,#59312,#59313,#59314,#59315,#59316,#59317,#59318,
#59319,#59320,#59321,#59322,#59323,#59324,#59325,#59326,#59327,#59328,#59329,
#59330,#59331,#59332,#59333,#59334,#59335,#59336,#59337,#59338,#59339,#59340,
#59341,#59342,#59343,#59344,#59345,#59346,#59347,#59348,#59349,#59350,#59351,
#59352,#59353,#59354,#59355,#59356,#59357,#59358,#59359,#59360,#59361,#59362,
#59363,#59364,#59365,#59366,#59367,#59368,#59369,#59370,#59371,#59372,#59373,
#59374,#59375,#59376,#59377,#59378,#59379,#59380,#59381,#59382,#59383,#59384,
#59385,#59386,#59387,#59388,#59389,#59390,#59391,#59392,#59393,#59394,#59395,
#59396,#59397,#59398,#59399,#59400,#59401,#59402,#59403,#59404,#59405,#59406,
#59407,#59408,#59409,#59410,#59411,#59412,#59413,#59414,#59415,#59416,#59417,
#59418,#59419,#59420,#59421,#59422,#59423,#59424,#59425,#59426,#59427,#59428,
#59429),.UNSPECIFIED.,.F.,.F.,(4,3,3,3,3,3,3,3,3,3,3,3,3,3,3,3,3,3,3,3,
3,3,3,3,3,3,3,3,3,3,3,3,3,3,3,3,3,3,3,3,3,3,4),(156.163987574067,156.262228618507,
156.360486880375,156.458853673816,156.557282430391,156.655872527635,156.698209478998,
156.796807604012,156.895265386799,156.995487954569,157.093767512308,157.192014091391,
157.29025717444,157.39195436307,157.490338776499,157.593692352729,157.69704592896,
157.795644053952,157.894101836717,157.994324404492,158.092603962209,158.190850541271,
158.289093624298,158.390790812954,158.489175226362,158.592528802642,158.695882378922,
158.794480503912,158.892938286674,158.993160854451,159.091440412165,159.189686991223,
159.287930074248,159.389627262907,159.488011676311,159.591365252598,159.694718828884,
159.797216560019,159.903218753284,160.005303397592,160.107256278838,160.209067828957,
160.22122533308),.UNSPECIFIED.);
#616=B_SPLINE_CURVE_WITH_KNOTS('',3,(#59430,#59431,#59432,#59433,#59434,
#59435),.UNSPECIFIED.,.F.,.F.,(4,1,1,4),(160.221227414851,160.693555278846,
161.692391728808,162.446146712717),.UNSPECIFIED.);
#617=B_SPLINE_CURVE_WITH_KNOTS('',3,(#59437,#59438,#59439,#59440,#59441,
#59442,#59443,#59444,#59445,#59446,#59447,#59448,#59449,#59450,#59451,#59452,
#59453,#59454,#59455,#59456,#59457,#59458,#59459,#59460,#59461,#59462,#59463,
#59464,#59465,#59466,#59467,#59468,#59469,#59470,#59471,#59472,#59473,#59474,
#59475,#59476,#59477,#59478,#59479,#59480,#59481,#59482,#59483,#59484,#59485,
#59486,#59487,#59488,#59489,#59490,#59491,#59492,#59493,#59494,#59495,#59496,
#59497,#59498,#59499,#59500,#59501,#59502,#59503,#59504,#59505,#59506,#59507,
#59508,#59509),.UNSPECIFIED.,.F.,.F.,(4,3,3,3,3,3,3,3,3,3,3,3,3,3,3,3,3,
3,3,3,3,3,3,3,4),(160.22122533308,160.228748546326,160.327346671318,160.425804454083,
160.526027021859,160.624306579575,160.722553158637,160.820796241664,160.92249343032,
161.020877843728,161.124231420008,161.227584996288,161.326183121278,161.424640904041,
161.524863471817,161.623143029531,161.72138960859,161.819632691614,161.921329880273,
162.019714293677,162.123067869964,162.22642144625,162.325027405988,162.423481500074,
162.447662215674),.UNSPECIFIED.);
#618=B_SPLINE_CURVE_WITH_KNOTS('',3,(#59510,#59511,#59512,#59513,#59514,
#59515,#59516,#59517,#59518,#59519,#59520,#59521,#59522,#59523,#59524,#59525,
#59526,#59527,#59528,#59529,#59530,#59531,#59532,#59533,#59534,#59535,#59536,
#59537,#59538,#59539,#59540,#59541,#59542,#59543,#59544,#59545,#59546,#59547,
#59548,#59549,#59550,#59551,#59552,#59553,#59554,#59555,#59556,#59557,#59558,
#59559,#59560,#59561,#59562,#59563,#59564,#59565,#59566,#59567,#59568,#59569,
#59570,#59571,#59572,#59573,#59574,#59575,#59576,#59577,#59578,#59579,#59580,
#59581,#59582,#59583,#59584,#59585,#59586,#59587,#59588,#59589,#59590,#59591,
#59592,#59593,#59594,#59595,#59596,#59597,#59598,#59599,#59600,#59601,#59602,
#59603,#59604,#59605,#59606,#59607,#59608,#59609,#59610,#59611,#59612,#59613,
#59614,#59615,#59616,#59617,#59618,#59619,#59620,#59621,#59622,#59623,#59624,
#59625,#59626,#59627,#59628,#59629,#59630,#59631,#59632,#59633),
 .UNSPECIFIED.,.F.,.F.,(4,3,3,3,3,3,3,3,3,3,3,3,3,3,3,3,3,3,3,3,3,3,3,3,
3,3,3,3,3,3,3,3,3,3,3,3,3,3,3,3,3,4),(156.163531910326,156.233402746479,
156.332000871484,156.430458654262,156.530681222035,156.628960779764,156.727207358839,
156.825450441879,156.927147630519,157.02553204394,157.12888562019,157.232239196441,
157.330837321443,157.429295104219,157.529517671992,157.627797229718,157.72604380879,
157.824286891828,157.925984080471,158.024368493889,158.127722070145,158.231075646402,
158.329673771403,158.428131554177,158.52835412195,158.626633679676,158.724880258747,
158.823123341782,158.924820530428,159.023204943844,159.126558520104,159.229912096364,
159.328378576654,159.426704810661,159.526019875932,159.624169149678,159.722285836342,
159.820399593048,159.920606027993,160.018861091251,160.120043212039,160.221225332828),
 .UNSPECIFIED.);
#619=B_SPLINE_CURVE_WITH_KNOTS('',3,(#59639,#59640,#59641,#59642,#59643,
#59644,#59645,#59646),.UNSPECIFIED.,.F.,.F.,(4,1,1,1,1,4),(149.881541683267,
150.705190779227,151.704027229189,152.702863679151,153.701700129113,153.938039726484),
 .UNSPECIFIED.);
#620=B_SPLINE_CURVE_WITH_KNOTS('',3,(#59647,#59648,#59649,#59650,#59651,
#59652,#59653,#59654,#59655,#59656,#59657,#59658,#59659,#59660,#59661,#59662,
#59663,#59664,#59665,#59666,#59667,#59668,#59669,#59670,#59671,#59672,#59673,
#59674,#59675,#59676,#59677,#59678,#59679,#59680,#59681,#59682,#59683,#59684,
#59685,#59686,#59687,#59688,#59689,#59690,#59691,#59692,#59693,#59694,#59695,
#59696,#59697,#59698,#59699,#59700,#59701,#59702,#59703,#59704,#59705,#59706,
#59707,#59708,#59709,#59710,#59711,#59712,#59713,#59714,#59715,#59716),
 .UNSPECIFIED.,.F.,.F.,(4,3,3,3,3,3,3,3,3,3,3,3,3,3,3,3,3,3,3,3,3,3,3,4),
(153.9380400259,154.035163898234,154.132222574362,154.229246955324,154.326267897773,
154.423381488606,154.520541056366,154.617870832504,154.700536579074,154.799134704076,
154.897592486852,154.997815054625,155.096094612352,155.194341191424,155.292584274461,
155.394281463105,155.492665876522,155.596019452779,155.699373029036,155.797975862223,
155.896415143035,155.994759399106,156.093038592393,156.163987574067),
 .UNSPECIFIED.);
#621=B_SPLINE_CURVE_WITH_KNOTS('',3,(#59718,#59719,#59720,#59721,#59722,
#59723,#59724,#59725,#59726,#59727,#59728,#59729,#59730,#59731,#59732,#59733,
#59734,#59735,#59736,#59737,#59738,#59739,#59740,#59741,#59742,#59743,#59744,
#59745,#59746,#59747,#59748,#59749,#59750,#59751,#59752,#59753,#59754,#59755,
#59756,#59757,#59758,#59759,#59760,#59761,#59762,#59763,#59764,#59765,#59766,
#59767,#59768,#59769,#59770,#59771,#59772,#59773,#59774,#59775,#59776,#59777,
#59778,#59779,#59780,#59781,#59782,#59783,#59784,#59785,#59786,#59787),
 .UNSPECIFIED.,.F.,.F.,(4,3,3,3,3,3,3,3,3,3,3,3,3,3,3,3,3,3,3,3,3,3,3,4),
(153.938040202782,154.056659980249,154.176963651006,154.235729846555,154.334327971559,
154.432785754335,154.533008322108,154.631287879836,154.729534458909,154.827777541948,
154.92947473059,155.027859144009,155.131212720263,155.234566296517,155.333169148011,
155.431630381049,155.5299726517,155.628250049483,155.726492098718,155.824728281928,
155.923038846784,156.021391522265,156.119876942697,156.163531910326),
 .UNSPECIFIED.);
#622=B_SPLINE_CURVE_WITH_KNOTS('',3,(#59788,#59789,#59790,#59791,#59792,
#59793,#59794,#59795),.UNSPECIFIED.,.F.,.F.,(4,1,1,1,1,4),(149.880018474884,
150.240384046707,151.239220496669,152.238056946631,153.236893396593,153.9380400259),
 .UNSPECIFIED.);
#623=B_SPLINE_CURVE_WITH_KNOTS('',3,(#59801,#59802,#59803,#59804,#59805,
#59806,#59807,#59808,#59809,#59810,#59811,#59812,#59813,#59814,#59815,#59816,
#59817,#59818,#59819,#59820,#59821,#59822,#59823,#59824,#59825,#59826,#59827,
#59828,#59829,#59830,#59831,#59832,#59833,#59834,#59835,#59836,#59837,#59838,
#59839,#59840,#59841,#59842,#59843,#59844,#59845,#59846,#59847,#59848,#59849,
#59850,#59851,#59852,#59853,#59854,#59855,#59856,#59857,#59858,#59859,#59860,
#59861,#59862,#59863,#59864,#59865,#59866,#59867,#59868,#59869,#59870,#59871,
#59872,#59873,#59874,#59875,#59876,#59877,#59878,#59879,#59880,#59881,#59882,
#59883,#59884,#59885,#59886,#59887,#59888,#59889,#59890,#59891,#59892,#59893,
#59894,#59895,#59896,#59897,#59898,#59899,#59900,#59901,#59902,#59903,#59904,
#59905,#59906,#59907,#59908,#59909,#59910,#59911,#59912,#59913,#59914,#59915,
#59916,#59917,#59918,#59919,#59920,#59921,#59922,#59923,#59924,#59925,#59926,
#59927),.UNSPECIFIED.,.F.,.F.,(4,3,3,3,3,3,3,3,3,3,3,3,3,3,3,3,3,3,3,3,
3,3,3,3,3,3,3,3,3,3,3,3,3,3,3,3,3,3,3,3,3,3,4),(143.59701849018,143.69562123255,
143.713335629494,143.811933754498,143.910391537275,144.010614105047,144.108893662775,
144.207140241849,144.305383324887,144.40708051353,144.505464926948,144.608818503202,
144.712172079456,144.81077020446,144.909227987236,145.009450555009,145.107730112737,
145.205976691811,145.304219774849,145.405916963491,145.50430137691,145.607654953164,
145.711008529418,145.809606654422,145.908064437198,146.008287004971,146.106566562699,
146.204813141772,146.303056224811,146.404753413453,146.503137826872,146.606491403125,
146.709844979379,146.807643480436,146.905302408374,147.002849316603,147.100335701354,
147.197792033696,147.295248746519,147.3927980835,147.490396206244,147.588155506493,
147.65485471872),.UNSPECIFIED.);
#624=B_SPLINE_CURVE_WITH_KNOTS('',3,(#59928,#59929,#59930,#59931,#59932,
#59933,#59934),.UNSPECIFIED.,.F.,.F.,(4,1,1,1,4),(147.65485471872,147.708681429341,
148.707517879303,149.706354329265,149.881541683267),.UNSPECIFIED.);
#625=B_SPLINE_CURVE_WITH_KNOTS('',3,(#59936,#59937,#59938,#59939,#59940,
#59941),.UNSPECIFIED.,.F.,.F.,(4,1,1,4),(147.65485471872,148.242711146784,
149.241547596746,149.880018474884),.UNSPECIFIED.);
#626=B_SPLINE_CURVE_WITH_KNOTS('',3,(#59942,#59943,#59944,#59945,#59946,
#59947,#59948,#59949,#59950,#59951,#59952,#59953,#59954,#59955,#59956,#59957,
#59958,#59959,#59960,#59961,#59962,#59963,#59964,#59965,#59966,#59967,#59968,
#59969,#59970,#59971,#59972,#59973,#59974,#59975,#59976,#59977,#59978,#59979,
#59980,#59981,#59982,#59983,#59984,#59985,#59986,#59987,#59988,#59989,#59990,
#59991,#59992,#59993,#59994,#59995,#59996,#59997,#59998,#59999,#60000,#60001,
#60002,#60003,#60004,#60005,#60006,#60007,#60008,#60009,#60010,#60011,#60012,
#60013,#60014,#60015,#60016,#60017,#60018,#60019,#60020,#60021,#60022,#60023,
#60024,#60025,#60026,#60027,#60028,#60029,#60030,#60031,#60032,#60033,#60034,
#60035,#60036,#60037,#60038,#60039,#60040,#60041,#60042,#60043,#60044,#60045,
#60046,#60047,#60048,#60049,#60050,#60051,#60052,#60053,#60054,#60055,#60056,
#60057,#60058,#60059,#60060,#60061,#60062,#60063,#60064,#60065),
 .UNSPECIFIED.,.F.,.F.,(4,3,3,3,3,3,3,3,3,3,3,3,3,3,3,3,3,3,3,3,3,3,3,3,
3,3,3,3,3,3,3,3,3,3,3,3,3,3,3,3,3,4),(143.597933903879,143.6961922985,143.794433353168,
143.892686540564,143.991045328786,144.089461510033,144.188044071276,144.247365346936,
144.34596347194,144.444421254717,144.544643822489,144.642923380217,144.741169959291,
144.839413042329,144.941110230972,145.03949464439,145.142848220644,145.246201796898,
145.344799921902,145.443257704678,145.543480272451,145.641759830179,145.740006409253,
145.838249492291,145.939946680933,146.038331094352,146.141684670606,146.24503824686,
146.343636371864,146.44209415464,146.542316722413,146.640596280141,146.738842859215,
146.837085942253,146.938783130895,147.037167544314,147.140521120568,147.243874696822,
147.352569174392,147.460952550046,147.568802109382,147.654854305383),
 .UNSPECIFIED.);
#627=B_SPLINE_CURVE_WITH_KNOTS('',3,(#60071,#60072,#60073,#60074,#60075,
#60076,#60077,#60078,#60079,#60080,#60081,#60082,#60083,#60084,#60085,#60086,
#60087,#60088,#60089,#60090,#60091,#60092,#60093,#60094,#60095,#60096,#60097,
#60098,#60099,#60100,#60101,#60102,#60103,#60104,#60105,#60106,#60107,#60108,
#60109,#60110,#60111,#60112,#60113,#60114,#60115,#60116,#60117,#60118,#60119,
#60120,#60121,#60122,#60123,#60124,#60125,#60126,#60127,#60128,#60129,#60130,
#60131,#60132,#60133,#60134,#60135,#60136,#60137,#60138,#60139,#60140,#60141,
#60142,#60143,#60144,#60145,#60146,#60147,#60148,#60149,#60150,#60151,#60152,
#60153,#60154,#60155,#60156,#60157,#60158,#60159,#60160,#60161,#60162,#60163,
#60164,#60165,#60166,#60167,#60168,#60169,#60170,#60171,#60172,#60173,#60174,
#60175,#60176,#60177,#60178,#60179,#60180,#60181,#60182,#60183,#60184,#60185,
#60186,#60187,#60188,#60189,#60190,#60191,#60192,#60193,#60194),
 .UNSPECIFIED.,.F.,.F.,(4,3,3,3,3,3,3,3,3,3,3,3,3,3,3,3,3,3,3,3,3,3,3,3,
3,3,3,3,3,3,3,3,3,3,3,3,3,3,3,3,3,4),(137.314044075445,137.415612289014,
137.513996928846,137.617156929285,137.720316929723,137.818915054727,137.917372837503,
138.017595405276,138.115874963004,138.214121542077,138.312364625116,138.414061813758,
138.512446227177,138.61579980343,138.719153379684,138.817751504687,138.916209287464,
139.016431855237,139.114711412965,139.212957992038,139.311201075077,139.412898263719,
139.511282677138,139.614636253392,139.717989829646,139.81658795465,139.915045737426,
140.015268305199,140.113547862927,140.211794442001,140.310037525039,140.411734713681,
140.5101191271,140.613472703354,140.716826279608,140.815569227393,140.914173010821,
141.012667061739,141.111081830931,141.209449097701,141.307822396311,141.371669411541),
 .UNSPECIFIED.);
#628=B_SPLINE_CURVE_WITH_KNOTS('',3,(#60195,#60196,#60197,#60198,#60199,
#60200,#60201,#60202,#60203,#60204,#60205,#60206,#60207,#60208,#60209,#60210,
#60211,#60212,#60213,#60214,#60215,#60216,#60217,#60218,#60219,#60220,#60221,
#60222,#60223,#60224,#60225,#60226,#60227,#60228,#60229,#60230,#60231,#60232,
#60233,#60234,#60235,#60236,#60237,#60238,#60239,#60240,#60241,#60242,#60243,
#60244,#60245,#60246,#60247,#60248,#60249,#60250,#60251,#60252,#60253,#60254,
#60255,#60256,#60257,#60258,#60259,#60260,#60261),.UNSPECIFIED.,.F.,.F.,
(4,3,3,3,3,3,3,3,3,3,3,3,3,3,3,3,3,3,3,3,3,3,4),(141.371669411768,141.485016004535,
141.600339367052,141.71566272957,141.814260854574,141.912718637351,142.012941205123,
142.111220762851,142.209467341925,142.307710424963,142.409407613606,142.507792027024,
142.611145603278,142.714499179532,142.813105314796,142.911543009966,143.009885026329,
143.108160960054,143.206400336867,143.304679404122,143.402973649647,143.501391759129,
143.59701849018),.UNSPECIFIED.);
#629=B_SPLINE_CURVE_WITH_KNOTS('',3,(#60263,#60264,#60265,#60266,#60267,
#60268,#60269,#60270,#60271,#60272,#60273,#60274,#60275,#60276,#60277,#60278,
#60279,#60280,#60281,#60282,#60283,#60284,#60285,#60286,#60287,#60288,#60289,
#60290,#60291,#60292,#60293,#60294,#60295,#60296,#60297,#60298,#60299,#60300,
#60301,#60302,#60303,#60304,#60305,#60306,#60307,#60308,#60309,#60310,#60311,
#60312,#60313,#60314,#60315,#60316,#60317,#60318,#60319,#60320,#60321,#60322,
#60323,#60324,#60325,#60326,#60327,#60328,#60329,#60330,#60331,#60332),
 .UNSPECIFIED.,.F.,.F.,(4,3,3,3,3,3,3,3,3,3,3,3,3,3,3,3,3,3,3,3,3,3,3,4),
(141.371669411541,141.46883125416,141.566438903267,141.66339620349,141.760311911022,
141.857216996242,141.955335858935,142.052368429038,142.151030438025,142.249692447012,
142.348290572016,142.446748354793,142.546970922565,142.645250480293,142.743497059367,
142.841740142405,142.943437331047,143.041821744466,143.14517532072,143.248528896974,
143.347104955703,143.44555813638,143.543900701717,143.597933903879),
 .UNSPECIFIED.);
#630=B_SPLINE_CURVE_WITH_KNOTS('',3,(#60333,#60334,#60335,#60336,#60337,
#60338,#60339,#60340),.UNSPECIFIED.,.F.,.F.,(4,1,1,1,1,4),(137.314688056577,
138.254346647165,139.253183097127,140.252019547089,141.250855997051,141.371669411541),
 .UNSPECIFIED.);
#631=B_SPLINE_CURVE_WITH_KNOTS('',3,(#60346,#60347,#60348,#60349,#60350,
#60351,#60352,#60353,#60354,#60355,#60356,#60357,#60358,#60359,#60360,#60361,
#60362,#60363,#60364,#60365,#60366,#60367,#60368,#60369,#60370,#60371,#60372,
#60373,#60374,#60375,#60376,#60377,#60378,#60379,#60380,#60381,#60382,#60383,
#60384,#60385,#60386,#60387,#60388,#60389,#60390,#60391,#60392,#60393,#60394,
#60395,#60396,#60397,#60398,#60399,#60400,#60401,#60402,#60403,#60404,#60405,
#60406,#60407,#60408,#60409,#60410,#60411,#60412,#60413,#60414,#60415,#60416,
#60417,#60418,#60419,#60420,#60421,#60422,#60423,#60424,#60425,#60426,#60427,
#60428,#60429,#60430,#60431,#60432,#60433,#60434,#60435,#60436,#60437,#60438,
#60439,#60440,#60441,#60442,#60443,#60444,#60445,#60446,#60447,#60448,#60449,
#60450,#60451,#60452,#60453,#60454,#60455,#60456,#60457,#60458,#60459,#60460,
#60461,#60462,#60463,#60464,#60465,#60466,#60467,#60468,#60469),
 .UNSPECIFIED.,.F.,.F.,(4,3,3,3,3,3,3,3,3,3,3,3,3,3,3,3,3,3,3,3,3,3,3,3,
3,3,3,3,3,3,3,3,3,3,3,3,3,3,3,3,3,4),(131.031654953742,131.129931693063,
131.228177228462,131.326421041054,131.426640338278,131.525027370655,131.626162800303,
131.727298229951,131.825896354955,131.924354137731,132.024576705504,132.122856263232,
132.221102842306,132.319345925344,132.421043113987,132.519427527405,132.622781103659,
132.726134679913,132.824732804917,132.923190587694,133.023413155466,133.121692713194,
133.219939292268,133.318182375306,133.419879563948,133.518263977367,133.621617553621,
133.724971129875,133.823569254879,133.922027037655,134.022249605428,134.120529163156,
134.218775742229,134.317018825268,134.41871601391,134.517100427329,134.620454003583,
134.723807579837,134.836338520701,134.948409000642,135.059693750752,135.088484104126),
 .UNSPECIFIED.);
#632=B_SPLINE_CURVE_WITH_KNOTS('',3,(#60470,#60471,#60472,#60473,#60474,
#60475,#60476,#60477,#60478,#60479,#60480,#60481,#60482,#60483,#60484,#60485,
#60486,#60487,#60488,#60489,#60490,#60491,#60492,#60493,#60494,#60495,#60496,
#60497,#60498,#60499,#60500,#60501,#60502,#60503,#60504,#60505,#60506,#60507,
#60508,#60509,#60510,#60511,#60512,#60513,#60514,#60515,#60516,#60517,#60518,
#60519,#60520,#60521,#60522,#60523,#60524,#60525,#60526,#60527,#60528,#60529,
#60530,#60531,#60532,#60533,#60534,#60535,#60536,#60537,#60538,#60539),
 .UNSPECIFIED.,.F.,.F.,(4,3,3,3,3,3,3,3,3,3,3,3,3,3,3,3,3,3,3,3,3,3,3,4),
(135.088484104361,135.187254556185,135.286029876603,135.384838499173,135.483776463585,
135.582788468007,135.681976179005,135.722644029799,135.821242154803,135.91969993758,
136.019922505352,136.11820206308,136.216448642154,136.314691725192,136.416388913834,
136.514773327253,136.618126903507,136.721480479761,136.820067256332,136.918521077989,
137.017401827353,137.115677667237,137.214860871341,137.314044075445),
 .UNSPECIFIED.);
#633=B_SPLINE_CURVE_WITH_KNOTS('',3,(#60541,#60542,#60543,#60544,#60545,
#60546,#60547),.UNSPECIFIED.,.F.,.F.,(4,1,1,1,4),(135.088484104361,135.257837297279,
136.256673747241,137.255510197203,137.314688056577),.UNSPECIFIED.);
#634=B_SPLINE_CURVE_WITH_KNOTS('',3,(#60548,#60549,#60550,#60551,#60552,
#60553,#60554,#60555,#60556,#60557,#60558,#60559,#60560,#60561,#60562,#60563,
#60564,#60565,#60566,#60567,#60568,#60569,#60570,#60571,#60572,#60573,#60574,
#60575,#60576,#60577,#60578,#60579,#60580,#60581,#60582,#60583,#60584,#60585,
#60586,#60587,#60588,#60589,#60590,#60591,#60592,#60593,#60594,#60595,#60596,
#60597,#60598,#60599,#60600,#60601,#60602,#60603,#60604,#60605,#60606,#60607,
#60608,#60609,#60610,#60611,#60612,#60613,#60614,#60615,#60616,#60617,#60618,
#60619,#60620,#60621,#60622,#60623,#60624,#60625,#60626,#60627,#60628,#60629,
#60630,#60631,#60632,#60633,#60634,#60635,#60636,#60637,#60638,#60639,#60640,
#60641,#60642,#60643,#60644,#60645,#60646,#60647,#60648,#60649,#60650,#60651,
#60652,#60653,#60654,#60655,#60656,#60657,#60658,#60659,#60660,#60661,#60662,
#60663,#60664,#60665,#60666,#60667,#60668,#60669,#60670,#60671,#60672,#60673,
#60674),.UNSPECIFIED.,.F.,.F.,(4,3,3,3,3,3,3,3,3,3,3,3,3,3,3,3,3,3,3,3,
3,3,3,3,3,3,3,3,3,3,3,3,3,3,3,3,3,3,3,3,3,3,4),(131.03054492507,131.128979421002,
131.227573113898,131.262491497432,131.361089622436,131.459547405213,131.559769972985,
131.658049530713,131.756296109787,131.854539192826,131.956236381468,132.054620794887,
132.15797437114,132.261327947394,132.359926072398,132.458383855174,132.558606422947,
132.656885980675,132.755132559748,132.853375642787,132.955072831429,133.053457244848,
133.156810821102,133.260164397356,133.35876252236,133.457220305136,133.557442872909,
133.655722430637,133.75396900971,133.852212092749,133.953909281391,134.05229369481,
134.155647271063,134.259000847317,134.356128675186,134.453094160804,134.549968416923,
134.646782617699,134.743567858738,134.84039997176,134.937256811786,135.034231214225,
135.088484104361),.UNSPECIFIED.);
#635=B_SPLINE_CURVE_WITH_KNOTS('',3,(#60680,#60681,#60682,#60683,#60684,
#60685,#60686,#60687),.UNSPECIFIED.,.F.,.F.,(4,1,1,1,1,4),(124.748033464244,
125.73427953018,126.733115980142,127.731952430104,128.730788880066,128.805298797182),
 .UNSPECIFIED.);
#636=B_SPLINE_CURVE_WITH_KNOTS('',3,(#60688,#60689,#60690,#60691,#60692,
#60693,#60694,#60695,#60696,#60697,#60698,#60699,#60700,#60701,#60702,#60703,
#60704,#60705,#60706,#60707,#60708,#60709,#60710,#60711,#60712,#60713,#60714,
#60715,#60716,#60717,#60718,#60719,#60720,#60721,#60722,#60723,#60724,#60725,
#60726,#60727,#60728,#60729,#60730,#60731,#60732,#60733,#60734,#60735,#60736,
#60737,#60738,#60739,#60740,#60741,#60742,#60743,#60744,#60745,#60746,#60747,
#60748,#60749,#60750,#60751,#60752,#60753,#60754,#60755,#60756,#60757),
 .UNSPECIFIED.,.F.,.F.,(4,3,3,3,3,3,3,3,3,3,3,3,3,3,3,3,3,3,3,3,3,3,3,4),
(128.805298797182,128.902840431273,129.000250613517,129.097560812666,129.194818343698,
129.292053887498,129.389298094495,129.486642967569,129.584044330746,129.681605924981,
129.729625330028,129.828223455032,129.926681237808,130.026903805581,130.125183363309,
130.223429942382,130.321673025421,130.423370214063,130.521754627482,130.625108203735,
130.728461779989,130.827047027845,130.929350990793,131.031654953742),
 .UNSPECIFIED.);
#637=B_SPLINE_CURVE_WITH_KNOTS('',3,(#60759,#60760,#60761,#60762,#60763,
#60764,#60765,#60766,#60767,#60768,#60769,#60770,#60771,#60772,#60773,#60774,
#60775,#60776,#60777,#60778,#60779,#60780,#60781,#60782,#60783,#60784,#60785,
#60786,#60787,#60788,#60789,#60790,#60791,#60792,#60793,#60794,#60795,#60796,
#60797,#60798,#60799,#60800,#60801,#60802,#60803,#60804,#60805,#60806,#60807,
#60808,#60809,#60810,#60811,#60812,#60813,#60814,#60815,#60816,#60817,#60818,
#60819,#60820,#60821,#60822,#60823,#60824,#60825,#60826,#60827,#60828),
 .UNSPECIFIED.,.F.,.F.,(4,3,3,3,3,3,3,3,3,3,3,3,3,3,3,3,3,3,3,3,3,3,3,4),
(128.805299011168,128.910085619878,129.015255759158,129.12063010964,129.226318351055,
129.264818597508,129.363416722512,129.461874505288,129.562097073061,129.660376630789,
129.758623209863,129.856866292901,129.958563481543,130.056947894962,130.160301471216,
130.26365504747,130.362225486657,130.460667523602,130.559010865893,130.657285118178,
130.755545076205,130.853792579357,130.952108672676,131.03054492507),
 .UNSPECIFIED.);
#638=B_SPLINE_CURVE_WITH_KNOTS('',3,(#60829,#60830,#60831,#60832,#60833,
#60834,#60835,#60836),.UNSPECIFIED.,.F.,.F.,(4,1,1,1,1,4),(124.748072421146,
125.269472797661,126.268309247622,127.267145697584,128.265982147546,128.805298797182),
 .UNSPECIFIED.);
#639=B_SPLINE_CURVE_WITH_KNOTS('',3,(#60842,#60843,#60844,#60845,#60846,
#60847,#60848,#60849,#60850,#60851,#60852,#60853,#60854,#60855,#60856,#60857,
#60858,#60859,#60860,#60861,#60862,#60863,#60864,#60865,#60866,#60867,#60868,
#60869,#60870,#60871,#60872,#60873,#60874,#60875,#60876,#60877,#60878,#60879,
#60880,#60881,#60882,#60883,#60884,#60885,#60886,#60887,#60888,#60889,#60890,
#60891,#60892,#60893,#60894,#60895,#60896,#60897,#60898,#60899,#60900,#60901,
#60902,#60903,#60904,#60905,#60906,#60907,#60908,#60909,#60910,#60911,#60912,
#60913,#60914,#60915,#60916,#60917,#60918,#60919,#60920,#60921,#60922,#60923,
#60924,#60925,#60926,#60927,#60928,#60929,#60930,#60931,#60932,#60933,#60934,
#60935,#60936,#60937,#60938,#60939,#60940,#60941,#60942,#60943,#60944,#60945,
#60946,#60947,#60948,#60949,#60950,#60951,#60952,#60953,#60954,#60955,#60956,
#60957,#60958,#60959,#60960,#60961,#60962,#60963,#60964,#60965),
 .UNSPECIFIED.,.F.,.F.,(4,3,3,3,3,3,3,3,3,3,3,3,3,3,3,3,3,3,3,3,3,3,3,3,
3,3,3,3,3,3,3,3,3,3,3,3,3,3,3,3,3,4),(118.464214588977,118.562615707051,
118.661189977465,118.742424380447,118.841022505451,118.939480288228,119.039702856,
119.137982413728,119.236228992802,119.33447207584,119.436169264482,119.534553677901,
119.637907254155,119.741260830409,119.839858955413,119.93831673819,120.038539305962,
120.136818863691,120.235065442764,120.333308525802,120.435005714445,120.533390127863,
120.636743704117,120.740097280371,120.838695405375,120.937153188151,121.037375755924,
121.135655313652,121.233901892725,121.332144975764,121.433842164406,121.532226577825,
121.635580154079,121.738933730333,121.836831200292,121.933909156543,122.030894120917,
122.127817176648,122.226391254986,122.323316910845,122.422715200424,122.522113490002),
 .UNSPECIFIED.);
#640=B_SPLINE_CURVE_WITH_KNOTS('',3,(#60966,#60967,#60968,#60969,#60970,
#60971,#60972),.UNSPECIFIED.,.F.,.F.,(4,1,1,1,4),(122.522113490002,122.737770180294,
123.736606630256,124.735443080218,124.748033464244),.UNSPECIFIED.);
#641=B_SPLINE_CURVE_WITH_KNOTS('',3,(#60974,#60975,#60976,#60977,#60978,
#60979),.UNSPECIFIED.,.F.,.F.,(4,1,1,4),(122.522113490002,123.271799897737,
124.270636347699,124.748072421146),.UNSPECIFIED.);
#642=B_SPLINE_CURVE_WITH_KNOTS('',3,(#60980,#60981,#60982,#60983,#60984,
#60985,#60986,#60987,#60988,#60989,#60990,#60991,#60992,#60993,#60994,#60995,
#60996,#60997,#60998,#60999,#61000,#61001,#61002,#61003,#61004,#61005,#61006,
#61007,#61008,#61009,#61010,#61011,#61012,#61013,#61014,#61015,#61016,#61017,
#61018,#61019,#61020,#61021,#61022,#61023,#61024,#61025,#61026,#61027,#61028,
#61029,#61030,#61031,#61032,#61033,#61034,#61035,#61036,#61037,#61038,#61039,
#61040,#61041,#61042,#61043,#61044,#61045,#61046,#61047,#61048,#61049,#61050,
#61051,#61052,#61053,#61054,#61055,#61056,#61057,#61058,#61059,#61060,#61061,
#61062,#61063,#61064,#61065,#61066,#61067,#61068,#61069,#61070,#61071,#61072,
#61073,#61074,#61075,#61076,#61077,#61078,#61079,#61080,#61081,#61082,#61083,
#61084,#61085,#61086,#61087,#61088,#61089,#61090,#61091,#61092,#61093,#61094,
#61095,#61096,#61097,#61098,#61099,#61100,#61101,#61102,#61103),
 .UNSPECIFIED.,.F.,.F.,(4,3,3,3,3,3,3,3,3,3,3,3,3,3,3,3,3,3,3,3,3,3,3,3,
3,3,3,3,3,3,3,3,3,3,3,3,3,3,3,3,3,4),(118.465360130437,118.566746876369,
118.665030492148,118.763278683933,118.861520936572,118.959786720207,119.058164549422,
119.156610017844,119.255210823008,119.276454097889,119.375052222893,119.47351000567,
119.573732573442,119.67201213117,119.770258710244,119.868501793282,119.970198981924,
120.068583395343,120.171936971597,120.275290547851,120.373888672855,120.472346455632,
120.572569023404,120.670848581132,120.769095160206,120.867338243244,120.969035431886,
121.067419845305,121.170773421559,121.274126997813,121.372725122817,121.471182905593,
121.571405473366,121.669685031094,121.767931610168,121.866174693206,121.967871881848,
122.066256295267,122.169609871521,122.272963447775,122.400857829824,122.522113389936),
 .UNSPECIFIED.);
#643=B_SPLINE_CURVE_WITH_KNOTS('',3,(#61109,#61110,#61111,#61112,#61113,
#61114,#61115,#61116,#61117,#61118,#61119,#61120,#61121,#61122,#61123,#61124,
#61125,#61126,#61127,#61128,#61129,#61130,#61131,#61132,#61133,#61134,#61135,
#61136,#61137,#61138,#61139,#61140,#61141,#61142,#61143,#61144,#61145,#61146,
#61147,#61148,#61149,#61150,#61151,#61152,#61153,#61154,#61155,#61156,#61157,
#61158,#61159,#61160,#61161,#61162,#61163,#61164,#61165,#61166,#61167,#61168,
#61169,#61170,#61171,#61172,#61173,#61174,#61175,#61176,#61177,#61178,#61179,
#61180,#61181,#61182,#61183,#61184,#61185,#61186,#61187,#61188,#61189,#61190,
#61191,#61192,#61193,#61194,#61195,#61196,#61197,#61198,#61199,#61200,#61201,
#61202,#61203,#61204,#61205,#61206,#61207,#61208,#61209,#61210,#61211,#61212,
#61213,#61214,#61215,#61216,#61217,#61218,#61219,#61220,#61221,#61222,#61223,
#61224,#61225,#61226,#61227,#61228,#61229,#61230,#61231,#61232),
 .UNSPECIFIED.,.F.,.F.,(4,3,3,3,3,3,3,3,3,3,3,3,3,3,3,3,3,3,3,3,3,3,3,3,
3,3,3,3,3,3,3,3,3,3,3,3,3,3,3,3,3,4),(112.181790913379,112.280032816134,
112.37828191992,112.476633696113,112.575038433759,112.673614612974,112.749405680676,
112.84800380568,112.946461588456,113.046684156229,113.144963713957,113.243210293031,
113.341453376069,113.443150564711,113.54153497813,113.644888554384,113.748242130638,
113.846840255642,113.945298038418,114.045520606191,114.143800163919,114.242046742992,
114.340289826031,114.441987014673,114.540371428091,114.643725004345,114.747078580599,
114.845676705603,114.944134488379,115.044357056152,115.14263661388,115.240883192954,
115.339126275992,115.440823464634,115.539207878053,115.642561454307,115.745915030561,
115.84988875933,115.953561696348,116.057054365165,116.160309146372,116.238928182547),
 .UNSPECIFIED.);
#644=B_SPLINE_CURVE_WITH_KNOTS('',3,(#61233,#61234,#61235,#61236,#61237,
#61238,#61239,#61240,#61241,#61242,#61243,#61244,#61245,#61246,#61247,#61248,
#61249,#61250,#61251,#61252,#61253,#61254,#61255,#61256,#61257,#61258,#61259,
#61260,#61261,#61262,#61263,#61264,#61265,#61266,#61267,#61268,#61269,#61270,
#61271,#61272,#61273,#61274,#61275,#61276,#61277,#61278,#61279,#61280,#61281,
#61282,#61283,#61284,#61285,#61286,#61287,#61288,#61289,#61290,#61291,#61292,
#61293,#61294,#61295,#61296,#61297,#61298,#61299,#61300,#61301,#61302),
 .UNSPECIFIED.,.F.,.F.,(4,3,3,3,3,3,3,3,3,3,3,3,3,3,3,3,3,3,3,3,3,3,3,4),
(116.238928182823,116.341566510357,116.44447107289,116.547509821617,116.650828963887,
116.744751480523,116.843349605527,116.941807388303,117.042029956076,117.140309513804,
117.238556092878,117.336799175916,117.438496364558,117.536880777977,117.640234354231,
117.743587930485,117.842162082218,117.940606624241,118.038951269663,118.137225626956,
118.235476585645,118.33371461238,118.431998836531,118.464214588977),
 .UNSPECIFIED.);
#645=B_SPLINE_CURVE_WITH_KNOTS('',3,(#61304,#61305,#61306,#61307,#61308,
#61309,#61310,#61311,#61312,#61313,#61314,#61315,#61316,#61317,#61318,#61319,
#61320,#61321,#61322,#61323,#61324,#61325,#61326,#61327,#61328,#61329,#61330,
#61331,#61332,#61333,#61334,#61335,#61336,#61337,#61338,#61339,#61340,#61341,
#61342,#61343,#61344,#61345,#61346,#61347,#61348,#61349,#61350,#61351,#61352,
#61353,#61354,#61355,#61356,#61357,#61358,#61359,#61360,#61361,#61362,#61363,
#61364,#61365,#61366,#61367,#61368,#61369,#61370,#61371,#61372,#61373),
 .UNSPECIFIED.,.F.,.F.,(4,3,3,3,3,3,3,3,3,3,3,3,3,3,3,3,3,3,3,3,3,3,3,4),
(116.238928182823,116.279944748004,116.378542873008,116.477000655784,116.577223223557,
116.675502781285,116.773749360358,116.871992443397,116.973689632039,117.072074045458,
117.175427621712,117.278781197966,117.37737932297,117.475837105746,117.576059673519,
117.674339231247,117.77258581032,117.870828893359,117.972526082001,118.07091049542,
118.174264071673,118.277617647927,118.37618931384,118.465360130437),
 .UNSPECIFIED.);
#646=B_SPLINE_CURVE_WITH_KNOTS('',3,(#61374,#61375,#61376,#61377,#61378,
#61379,#61380,#61381),.UNSPECIFIED.,.F.,.F.,(4,1,1,1,1,4),(112.180986309197,
112.284598948156,113.283435398118,114.28227184808,115.281108298042,116.238922797716),
 .UNSPECIFIED.);
#647=B_SPLINE_CURVE_WITH_KNOTS('',3,(#61387,#61388,#61389,#61390,#61391,
#61392,#61393,#61394,#61395,#61396,#61397,#61398,#61399,#61400,#61401,#61402,
#61403,#61404,#61405,#61406,#61407,#61408,#61409,#61410,#61411,#61412,#61413,
#61414,#61415,#61416,#61417,#61418,#61419,#61420,#61421,#61422,#61423,#61424,
#61425,#61426,#61427,#61428,#61429,#61430,#61431,#61432,#61433,#61434,#61435,
#61436,#61437,#61438,#61439,#61440,#61441,#61442,#61443,#61444,#61445,#61446,
#61447,#61448,#61449,#61450,#61451,#61452,#61453,#61454,#61455,#61456,#61457,
#61458,#61459,#61460,#61461,#61462,#61463,#61464,#61465,#61466,#61467,#61468,
#61469,#61470,#61471,#61472,#61473,#61474,#61475,#61476,#61477,#61478,#61479,
#61480,#61481,#61482,#61483,#61484,#61485,#61486,#61487,#61488,#61489,#61490,
#61491,#61492,#61493,#61494,#61495,#61496,#61497,#61498,#61499,#61500,#61501,
#61502,#61503,#61504,#61505,#61506,#61507,#61508,#61509,#61510),
 .UNSPECIFIED.,.F.,.F.,(4,3,3,3,3,3,3,3,3,3,3,3,3,3,3,3,3,3,3,3,3,3,3,3,
3,3,3,3,3,3,3,3,3,3,3,3,3,3,3,3,3,4),(105.898938909624,105.997345956639,
106.095658465059,106.193920742369,106.292162290793,106.390412584537,106.488766476771,
106.58717471803,106.685752797487,106.756386980905,106.854985105909,106.953442888685,
107.053665456458,107.151945014186,107.250191593259,107.348434676298,107.45013186494,
107.548516278359,107.651869854612,107.755223430866,107.85382155587,107.952279338646,
108.052501906419,108.150781464147,108.24902804322,108.347271126259,108.448968314901,
108.54735272832,108.650706304574,108.754059880828,108.852658005832,108.951115788609,
109.051338356381,109.149617914109,109.247864493183,109.346107576221,109.447804764864,
109.546189178282,109.649542754536,109.75289633079,109.893212936346,109.955742875643),
 .UNSPECIFIED.);
#648=B_SPLINE_CURVE_WITH_KNOTS('',3,(#61511,#61512,#61513,#61514,#61515,
#61516,#61517,#61518,#61519,#61520,#61521,#61522,#61523,#61524,#61525,#61526,
#61527,#61528,#61529,#61530,#61531,#61532,#61533,#61534,#61535,#61536,#61537,
#61538,#61539,#61540,#61541,#61542,#61543,#61544,#61545,#61546,#61547,#61548,
#61549,#61550,#61551,#61552,#61553,#61554,#61555,#61556,#61557,#61558,#61559,
#61560,#61561,#61562,#61563,#61564,#61565,#61566,#61567,#61568,#61569,#61570,
#61571,#61572,#61573,#61574,#61575,#61576,#61577,#61578,#61579,#61580,#61581,
#61582,#61583),.UNSPECIFIED.,.F.,.F.,(4,3,3,3,3,3,3,3,3,3,3,3,3,3,3,3,3,
3,3,3,3,3,3,3,4),(109.955742875951,110.055241614051,110.152151423466,110.249014842069,
110.345862894414,110.447330365998,110.544300028994,110.641334438528,110.738518045248,
110.751732780752,110.850330905756,110.948788688532,111.049011256305,111.147290814033,
111.245537393107,111.343780476145,111.445477664787,111.543862078206,111.64721565446,
111.750569230714,111.849176820417,111.947618966289,112.045965736414,112.144240689696,
112.181790913379),.UNSPECIFIED.);
#649=B_SPLINE_CURVE_WITH_KNOTS('',3,(#61585,#61586,#61587,#61588,#61589,
#61590),.UNSPECIFIED.,.F.,.F.,(4,1,1,4),(109.955750010575,110.286926048232,
111.285762498194,112.180986309197),.UNSPECIFIED.);
#650=B_SPLINE_CURVE_WITH_KNOTS('',3,(#61591,#61592,#61593,#61594,#61595,
#61596,#61597,#61598,#61599,#61600,#61601,#61602,#61603,#61604,#61605,#61606,
#61607,#61608,#61609,#61610,#61611,#61612,#61613,#61614,#61615,#61616,#61617,
#61618,#61619,#61620,#61621,#61622,#61623,#61624,#61625,#61626,#61627,#61628,
#61629,#61630,#61631,#61632,#61633,#61634,#61635,#61636,#61637,#61638,#61639,
#61640,#61641,#61642,#61643,#61644,#61645,#61646,#61647,#61648,#61649,#61650,
#61651,#61652,#61653,#61654,#61655,#61656,#61657,#61658,#61659,#61660,#61661,
#61662,#61663,#61664,#61665,#61666,#61667,#61668,#61669,#61670,#61671,#61672,
#61673,#61674,#61675,#61676,#61677,#61678,#61679,#61680,#61681,#61682,#61683,
#61684,#61685,#61686,#61687,#61688,#61689,#61690,#61691,#61692,#61693,#61694,
#61695,#61696,#61697,#61698,#61699,#61700,#61701,#61702,#61703,#61704,#61705,
#61706,#61707,#61708,#61709,#61710,#61711,#61712,#61713,#61714),
 .UNSPECIFIED.,.F.,.F.,(4,3,3,3,3,3,3,3,3,3,3,3,3,3,3,3,3,3,3,3,3,3,3,3,
3,3,3,3,3,3,3,3,3,3,3,3,3,3,3,3,3,4),(105.898082526351,105.996456956859,
106.094847333998,106.193416304684,106.291580248385,106.390178373389,106.488636156165,
106.588858723938,106.687138281666,106.78538486074,106.883627943778,106.98532513242,
107.083709545839,107.187063122093,107.290416698347,107.389014823351,107.487472606127,
107.5876951739,107.685974731628,107.784221310702,107.88246439374,107.984161582382,
108.082545995801,108.185899572055,108.289253148309,108.387851273313,108.48630905609,
108.586531623862,108.68481118159,108.783057760664,108.881300843702,108.982998032344,
109.081382445763,109.184736022017,109.288089598271,109.386591328536,109.484956309732,
109.583214317042,109.681399820024,109.779540599734,109.877698313765,109.955742875643),
 .UNSPECIFIED.);
#651=B_SPLINE_CURVE_WITH_KNOTS('',3,(#61720,#61721,#61722,#61723,#61724,
#61725,#61726,#61727),.UNSPECIFIED.,.F.,.F.,(4,1,1,1,1,4),(99.6144332140862,
99.7645318311714,100.763368281133,101.762204731095,102.761041181057,103.672548858805),
 .UNSPECIFIED.);
#652=B_SPLINE_CURVE_WITH_KNOTS('',3,(#61728,#61729,#61730,#61731,#61732,
#61733,#61734,#61735,#61736,#61737,#61738,#61739,#61740,#61741,#61742,#61743,
#61744,#61745,#61746,#61747,#61748,#61749,#61750,#61751,#61752,#61753,#61754,
#61755,#61756,#61757,#61758,#61759,#61760,#61761,#61762,#61763,#61764,#61765,
#61766,#61767,#61768,#61769,#61770,#61771,#61772,#61773,#61774,#61775,#61776,
#61777,#61778,#61779,#61780,#61781,#61782,#61783,#61784,#61785,#61786,#61787,
#61788,#61789,#61790,#61791,#61792,#61793,#61794,#61795,#61796,#61797),
 .UNSPECIFIED.,.F.,.F.,(4,3,3,3,3,3,3,3,3,3,3,3,3,3,3,3,3,3,3,3,3,3,3,4),
(103.672557568463,103.759877631019,103.858475756023,103.956933538799,104.057156106572,
104.1554356643,104.253682243374,104.351925326412,104.453622515054,104.552006928473,
104.655360504727,104.758714080981,104.857312205985,104.955769988762,105.055992556534,
105.154272114262,105.252518693336,105.350761776374,105.452458965017,105.550843378435,
105.654196954689,105.757550530943,105.856140410593,105.898938909624),
 .UNSPECIFIED.);
#653=B_SPLINE_CURVE_WITH_KNOTS('',3,(#61799,#61800,#61801,#61802,#61803,
#61804,#61805,#61806,#61807,#61808,#61809,#61810,#61811,#61812,#61813,#61814,
#61815,#61816,#61817,#61818,#61819,#61820,#61821,#61822,#61823,#61824,#61825,
#61826,#61827,#61828,#61829,#61830,#61831,#61832,#61833,#61834,#61835,#61836,
#61837,#61838,#61839,#61840,#61841,#61842,#61843,#61844,#61845,#61846,#61847,
#61848,#61849,#61850,#61851,#61852,#61853,#61854,#61855,#61856,#61857,#61858,
#61859,#61860,#61861,#61862,#61863,#61864,#61865,#61866,#61867,#61868,#61869,
#61870,#61871),.UNSPECIFIED.,.F.,.F.,(4,3,3,3,3,3,3,3,3,3,3,3,3,3,3,3,3,
3,3,3,3,3,3,3,4),(103.672557568463,103.771601702603,103.870660322484,103.96976131202,
104.06899945985,104.168318657834,104.267812431338,104.293907348461,104.392505473465,
104.490963256241,104.591185824014,104.689465381742,104.787711960816,104.885955043854,
104.987652232496,105.086036645915,105.189390222169,105.292743798423,105.391329160732,
105.489781902013,105.591857058097,105.690131964868,105.788367320327,105.886604354657,
105.898082526351),.UNSPECIFIED.);
#654=B_SPLINE_CURVE_WITH_KNOTS('',3,(#61872,#61873,#61874,#61875,#61876,
#61877,#61878,#61879),.UNSPECIFIED.,.F.,.F.,(4,1,1,1,1,4),(99.616027874956,
100.298561548614,101.297397998576,102.296234448537,103.295070898499,103.672550060316),
 .UNSPECIFIED.);
#655=B_SPLINE_CURVE_WITH_KNOTS('',3,(#61885,#61886,#61887,#61888,#61889,
#61890,#61891,#61892,#61893,#61894,#61895,#61896,#61897,#61898,#61899,#61900,
#61901,#61902,#61903,#61904,#61905,#61906,#61907,#61908,#61909,#61910,#61911,
#61912,#61913,#61914,#61915,#61916,#61917,#61918,#61919,#61920,#61921,#61922,
#61923,#61924,#61925,#61926,#61927,#61928,#61929,#61930,#61931,#61932,#61933,
#61934,#61935,#61936,#61937,#61938,#61939,#61940,#61941,#61942,#61943,#61944,
#61945,#61946,#61947,#61948,#61949,#61950,#61951,#61952,#61953,#61954,#61955,
#61956,#61957,#61958,#61959,#61960,#61961,#61962,#61963,#61964,#61965,#61966,
#61967,#61968,#61969,#61970,#61971,#61972,#61973,#61974,#61975,#61976,#61977,
#61978,#61979,#61980,#61981,#61982,#61983,#61984,#61985,#61986,#61987,#61988,
#61989,#61990,#61991,#61992,#61993,#61994,#61995,#61996,#61997,#61998,#61999,
#62000,#62001,#62002,#62003,#62004,#62005,#62006,#62007,#62008,#62009,#62010,
#62011),.UNSPECIFIED.,.F.,.F.,(4,3,3,3,3,3,3,3,3,3,3,3,3,3,3,3,3,3,3,3,
3,3,3,3,3,3,3,3,3,3,3,3,3,3,3,3,3,3,3,3,3,3,4),(93.3318434365138,93.4301005194132,
93.5284655037585,93.6268914566206,93.7254798312946,93.7715131314001,93.8701112564038,
93.9685690391803,94.068791606953,94.1670711646811,94.2653177437544,94.3635608267929,
94.4652580154352,94.5636424288539,94.666996005108,94.770349581362,94.8689477063657,
94.9674054891425,95.0676280569152,95.1659076146433,95.2641541937166,95.3623972767552,
95.4640944653974,95.5624788788163,95.6658324550701,95.7691860313239,95.8677841563277,
95.9662419391043,96.066464506877,96.1647440646052,96.2629906436784,96.3612337267171,
96.4629309153592,96.5613153287781,96.6646689050319,96.7680224812858,96.8674993725789,
96.9668292609827,97.0660403563899,97.1651524247994,97.2642075332238,97.3632407686269,
97.3893722612837),.UNSPECIFIED.);
#656=B_SPLINE_CURVE_WITH_KNOTS('',3,(#62012,#62013,#62014,#62015,#62016,
#62017),.UNSPECIFIED.,.F.,.F.,(4,1,1,4),(97.3893797693875,97.7668589312476,
98.7656953812095,99.6144332140862),.UNSPECIFIED.);
#657=B_SPLINE_CURVE_WITH_KNOTS('',3,(#62019,#62020,#62021,#62022,#62023,
#62024),.UNSPECIFIED.,.F.,.F.,(4,1,1,4),(97.3893809708947,98.3008886486899,
99.2997250986518,99.616027874956),.UNSPECIFIED.);
#658=B_SPLINE_CURVE_WITH_KNOTS('',3,(#62025,#62026,#62027,#62028,#62029,
#62030,#62031,#62032,#62033,#62034,#62035,#62036,#62037,#62038,#62039,#62040,
#62041,#62042,#62043,#62044,#62045,#62046,#62047,#62048,#62049,#62050,#62051,
#62052,#62053,#62054,#62055,#62056,#62057,#62058,#62059,#62060,#62061,#62062,
#62063,#62064,#62065,#62066,#62067,#62068,#62069,#62070,#62071,#62072,#62073,
#62074,#62075,#62076,#62077,#62078,#62079,#62080,#62081,#62082,#62083,#62084,
#62085,#62086,#62087,#62088,#62089,#62090,#62091,#62092,#62093,#62094,#62095,
#62096,#62097,#62098,#62099,#62100,#62101,#62102,#62103,#62104,#62105,#62106,
#62107,#62108,#62109,#62110,#62111,#62112,#62113,#62114,#62115,#62116,#62117,
#62118,#62119,#62120,#62121,#62122,#62123,#62124,#62125,#62126,#62127,#62128,
#62129,#62130,#62131,#62132,#62133,#62134,#62135,#62136,#62137,#62138,#62139,
#62140,#62141,#62142,#62143,#62144,#62145,#62146,#62147,#62148),
 .UNSPECIFIED.,.F.,.F.,(4,3,3,3,3,3,3,3,3,3,3,3,3,3,3,3,3,3,3,3,3,3,3,3,
3,3,3,3,3,3,3,3,3,3,3,3,3,3,3,3,3,4),(93.3321733081382,93.4307320543271,
93.5291589455774,93.62748337466,93.7257523655947,93.8239954283074,93.9222420400156,
94.0205891010754,94.1189858425587,94.2175578841727,94.3055428488424,94.4041409738461,
94.5025987566228,94.6028213243955,94.7011008821237,94.7993474611971,94.8975905442356,
94.9992877328777,95.0976721462965,95.2010257225504,95.3043792988043,95.402977423808,
95.5014352065847,95.6016577743574,95.6999373320856,95.798183911159,95.8964269941975,
95.9981241828397,96.0965085962585,96.1998621725124,96.3032157487662,96.4018138737699,
96.5002716565467,96.6004942243194,96.6987737820475,96.7970203611209,96.8952634441594,
96.9969606328015,97.0953450462203,97.1986986224742,97.302052198728,97.3893722612837),
 .UNSPECIFIED.);
#659=B_SPLINE_CURVE_WITH_KNOTS('',3,(#62154,#62155,#62156,#62157,#62158,
#62159,#62160,#62161),.UNSPECIFIED.,.F.,.F.,(4,1,1,1,1,4),(87.0497429142915,
87.7784944316289,88.7773308815908,89.7761673315526,90.7750037815145,91.1061798192275),
 .UNSPECIFIED.);
#660=B_SPLINE_CURVE_WITH_KNOTS('',3,(#62162,#62163,#62164,#62165,#62166,
#62167,#62168,#62169,#62170,#62171,#62172,#62173,#62174,#62175,#62176,#62177,
#62178,#62179,#62180,#62181,#62182,#62183,#62184,#62185,#62186,#62187,#62188,
#62189,#62190,#62191,#62192,#62193,#62194,#62195,#62196,#62197,#62198,#62199,
#62200,#62201,#62202,#62203,#62204,#62205,#62206,#62207,#62208,#62209,#62210,
#62211,#62212,#62213,#62214,#62215,#62216,#62217,#62218,#62219,#62220,#62221,
#62222,#62223,#62224,#62225,#62226,#62227,#62228,#62229,#62230,#62231),
 .UNSPECIFIED.,.F.,.F.,(4,3,3,3,3,3,3,3,3,3,3,3,3,3,3,3,3,3,3,3,3,3,3,4),
(91.1061869541041,91.204341964477,91.3024795334308,91.400629164884,91.4988897541857,
91.5972075103079,91.6957053368615,91.7738402314764,91.8724383564801,91.9708961392567,
92.0711187070294,92.1693982647576,92.267644843831,92.3658879268695,92.4675851155117,
92.5659695289305,92.6693231051844,92.7726766814383,92.871267317254,92.9697241251268,
93.0680663331376,93.1663410384432,93.2645927043616,93.3318434365138),
 .UNSPECIFIED.);
#661=B_SPLINE_CURVE_WITH_KNOTS('',3,(#62233,#62234,#62235,#62236,#62237,
#62238,#62239,#62240,#62241,#62242,#62243,#62244,#62245,#62246,#62247,#62248,
#62249,#62250,#62251,#62252,#62253,#62254,#62255,#62256,#62257,#62258,#62259,
#62260,#62261,#62262,#62263,#62264,#62265,#62266,#62267,#62268,#62269,#62270,
#62271,#62272,#62273,#62274,#62275,#62276,#62277,#62278,#62279,#62280,#62281,
#62282,#62283,#62284,#62285,#62286,#62287,#62288,#62289,#62290,#62291,#62292,
#62293,#62294,#62295,#62296,#62297,#62298,#62299,#62300,#62301,#62302),
 .UNSPECIFIED.,.F.,.F.,(4,3,3,3,3,3,3,3,3,3,3,3,3,3,3,3,3,3,3,3,3,3,3,4),
(91.1061869541041,91.2465035596771,91.3090334989568,91.4076316239605,91.5060894067374,
91.60631197451,91.7045915322382,91.8028381113116,91.9010811943501,92.0027783829923,
92.101162796411,92.2045163726649,92.3078699489187,92.4064680739224,92.5049258566991,
92.6051484244718,92.7034279822,92.8016745612733,92.8999176443118,93.001614832954,
93.0999992463728,93.2033528226267,93.3067063988806,93.3321733081382),
 .UNSPECIFIED.);
#662=B_SPLINE_CURVE_WITH_KNOTS('',3,(#62303,#62304,#62305,#62306,#62307,
#62308,#62309,#62310,#62311,#62312,#62313,#62314,#62315,#62316,#62317,#62318,
#62319,#62320,#62321,#62322,#62323,#62324,#62325,#62326,#62327,#62328,#62329,
#62330,#62331,#62332,#62333,#62334,#62335,#62336,#62337,#62338,#62339,#62340,
#62341,#62342,#62343,#62344,#62345,#62346,#62347,#62348,#62349,#62350,#62351,
#62352,#62353,#62354,#62355,#62356,#62357,#62358,#62359,#62360,#62361,#62362,
#62363,#62364,#62365,#62366,#62367,#62368,#62369,#62370,#62371,#62372,#62373,
#62374,#62375,#62376,#62377,#62378,#62379,#62380,#62381,#62382,#62383,#62384,
#62385,#62386,#62387,#62388,#62389,#62390,#62391,#62392,#62393,#62394,#62395,
#62396,#62397,#62398,#62399,#62400,#62401,#62402,#62403,#62404,#62405,#62406,
#62407,#62408,#62409,#62410,#62411,#62412,#62413,#62414,#62415,#62416,#62417,
#62418,#62419,#62420,#62421,#62422,#62423,#62424,#62425,#62426,#62427,#62428,
#62429),.UNSPECIFIED.,.F.,.F.,(4,3,3,3,3,3,3,3,3,3,3,3,3,3,3,3,3,3,3,3,
3,3,3,3,3,3,3,3,3,3,3,3,3,3,3,3,3,3,3,3,3,3,4),(87.0482730518095,87.1466828155122,
87.2452617360055,87.3136876991093,87.412285824113,87.5107436068898,87.6109661746624,
87.7092457323906,87.807492311464,87.9057353945025,88.0074325831446,88.1058169965635,
88.2091705728173,88.3125241490712,88.4111222740749,88.5095800568516,88.6098026246243,
88.7080821823525,88.8063287614259,88.9045718444644,89.0062690331065,89.1046534465253,
89.2080070227792,89.3113605990331,89.4099587240368,89.5084165068135,89.6086390745861,
89.7069186323143,89.8051652113877,89.9034082944262,90.0051054830683,90.1034898964871,
90.206843472741,90.3101970489949,90.409695787095,90.5067185530535,90.6036495481491,
90.7005198981798,90.8019366620839,90.8988156754796,90.9957205549586,91.0927209416411,
91.1061869537961),.UNSPECIFIED.);
#663=B_SPLINE_CURVE_WITH_KNOTS('',3,(#62435,#62436,#62437,#62438,#62439,
#62440,#62441,#62442,#62443,#62444,#62445,#62446,#62447,#62448,#62449,#62450,
#62451,#62452,#62453,#62454,#62455,#62456,#62457,#62458,#62459,#62460,#62461,
#62462,#62463,#62464,#62465,#62466,#62467,#62468,#62469,#62470,#62471,#62472,
#62473,#62474,#62475,#62476,#62477,#62478,#62479,#62480,#62481,#62482,#62483,
#62484,#62485,#62486,#62487,#62488,#62489,#62490,#62491,#62492,#62493,#62494,
#62495,#62496,#62497,#62498,#62499,#62500,#62501,#62502,#62503,#62504,#62505,
#62506,#62507,#62508,#62509,#62510,#62511,#62512,#62513,#62514,#62515,#62516,
#62517,#62518,#62519,#62520,#62521,#62522,#62523,#62524,#62525,#62526,#62527,
#62528,#62529,#62530,#62531,#62532,#62533,#62534,#62535,#62536,#62537,#62538,
#62539,#62540,#62541,#62542,#62543,#62544,#62545,#62546,#62547,#62548,#62549,
#62550,#62551,#62552,#62553,#62554,#62555,#62556,#62557,#62558,#62559,#62560,
#62561),.UNSPECIFIED.,.F.,.F.,(4,3,3,3,3,3,3,3,3,3,3,3,3,3,3,3,3,3,3,3,
3,3,3,3,3,3,3,3,3,3,3,3,3,3,3,3,3,3,3,3,3,3,4),(80.7655329441315,80.7866392818958,
80.8852374068995,80.9836951896762,81.0839177574489,81.182197315177,81.2804438942504,
81.3786869772889,81.4803841659311,81.5787685793499,81.6821221556038,81.7854757318576,
81.8840738568613,81.9825316396381,82.0827542074107,82.1810337651388,82.2792803442122,
82.3775234272507,82.4792206158929,82.5776050293117,82.6809586055656,82.7843121818195,
82.8829103068232,82.9813680896,83.0815906573726,83.1798702151008,83.2781167941742,
83.3763598772127,83.4780570658549,83.5764414792737,83.6797950555275,83.7831486317814,
83.8817467567851,83.9802045395617,84.0804271073344,84.1787066650625,84.2769532441359,
84.3751963271743,84.4768935158166,84.5752779292353,84.6786315054893,84.7819850817433,
84.8230016469246),.UNSPECIFIED.);
#664=B_SPLINE_CURVE_WITH_KNOTS('',3,(#62562,#62563,#62564,#62565,#62566,
#62567),.UNSPECIFIED.,.F.,.F.,(4,1,1,4),(84.8230070320566,85.7808215317051,
86.779657981667,87.0497429142915),.UNSPECIFIED.);
#665=B_SPLINE_CURVE_WITH_KNOTS('',3,(#62569,#62570,#62571,#62572,#62573,
#62574,#62575,#62576,#62577,#62578,#62579,#62580,#62581,#62582,#62583,#62584,
#62585,#62586,#62587,#62588,#62589,#62590,#62591,#62592,#62593,#62594,#62595,
#62596,#62597,#62598,#62599,#62600,#62601,#62602,#62603,#62604,#62605,#62606,
#62607,#62608,#62609,#62610,#62611,#62612,#62613,#62614,#62615,#62616,#62617,
#62618,#62619,#62620,#62621,#62622,#62623,#62624,#62625,#62626,#62627,#62628,
#62629,#62630,#62631,#62632,#62633,#62634,#62635,#62636,#62637,#62638),
 .UNSPECIFIED.,.F.,.F.,(4,3,3,3,3,3,3,3,3,3,3,3,3,3,3,3,3,3,3,3,3,3,3,4),
(84.8230016472006,84.9261861619506,85.0296647966982,85.1332945907094,85.2372126194226,
85.3160147991856,85.4146129241893,85.5130707069661,85.6132932747388,85.7115728324669,
85.8098194115403,85.9080624945788,86.0097596832209,86.1081440966397,86.2114976728936,
86.3148512491474,86.4134243290395,86.5118681332278,86.6102123732684,86.7084866565498,
86.8067399239169,86.9049803913479,87.0032727094468,87.0482730518095),
 .UNSPECIFIED.);
#666=B_SPLINE_CURVE_WITH_KNOTS('',3,(#62639,#62640,#62641,#62642,#62643,
#62644,#62645,#62646,#62647,#62648,#62649,#62650,#62651,#62652,#62653,#62654,
#62655,#62656,#62657,#62658,#62659,#62660,#62661,#62662,#62663,#62664,#62665,
#62666,#62667,#62668,#62669,#62670,#62671,#62672,#62673,#62674,#62675,#62676,
#62677,#62678,#62679,#62680,#62681,#62682,#62683,#62684,#62685,#62686,#62687,
#62688,#62689,#62690,#62691,#62692,#62693,#62694,#62695,#62696,#62697,#62698,
#62699,#62700,#62701,#62702,#62703,#62704,#62705,#62706,#62707,#62708,#62709,
#62710,#62711,#62712,#62713,#62714,#62715,#62716,#62717,#62718,#62719,#62720,
#62721,#62722,#62723,#62724,#62725,#62726,#62727,#62728,#62729,#62730,#62731,
#62732,#62733,#62734,#62735,#62736,#62737,#62738,#62739,#62740,#62741,#62742,
#62743,#62744,#62745,#62746,#62747,#62748,#62749,#62750,#62751,#62752,#62753,
#62754,#62755,#62756,#62757,#62758,#62759,#62760,#62761,#62762),
 .UNSPECIFIED.,.F.,.F.,(4,3,3,3,3,3,3,3,3,3,3,3,3,3,3,3,3,3,3,3,3,3,3,3,
3,3,3,3,3,3,3,3,3,3,3,3,3,3,3,3,3,4),(80.7658264624535,80.8640676348504,
80.9623198392987,81.0606769983247,81.1590905612312,81.2576716189549,81.3206689993381,
81.4192671243418,81.5177249071187,81.6179474748913,81.7162270326195,81.8144736116928,
81.9127166947314,82.0144138833735,82.1127982967923,82.2161518730461,82.3195054492999,
82.4181035743036,82.5165613570802,82.6167839248529,82.7150634825809,82.8133100616542,
82.9115531446927,83.013250333335,83.1116347467538,83.2149883230078,83.3183418992618,
83.4169400242654,83.5153978070423,83.615620374815,83.7138999325431,83.8121465116164,
83.9103895946548,84.0120867832971,84.1104711967158,84.2138247729698,84.3171783492237,
84.4205578302504,84.5236543867486,84.6265834813177,84.7292989065991,84.8230016469246),
 .UNSPECIFIED.);
#667=B_SPLINE_CURVE_WITH_KNOTS('',3,(#62768,#62769,#62770,#62771,#62772,
#62773,#62774,#62775),.UNSPECIFIED.,.F.,.F.,(4,1,1,1,1,4),(74.4816441096174,
74.7936205821245,75.7924570320864,76.7912934820483,77.7901299320101,78.539816339745),
 .UNSPECIFIED.);
#668=B_SPLINE_CURVE_WITH_KNOTS('',3,(#62776,#62777,#62778,#62779,#62780,
#62781,#62782,#62783,#62784,#62785,#62786,#62787,#62788,#62789,#62790,#62791,
#62792,#62793,#62794,#62795,#62796,#62797,#62798,#62799,#62800,#62801,#62802,
#62803,#62804,#62805,#62806,#62807,#62808,#62809,#62810,#62811,#62812,#62813,
#62814,#62815,#62816,#62817,#62818,#62819,#62820,#62821,#62822,#62823,#62824,
#62825,#62826,#62827,#62828,#62829,#62830,#62831,#62832,#62833,#62834,#62835,
#62836,#62837,#62838,#62839,#62840,#62841,#62842),.UNSPECIFIED.,.F.,.F.,
(4,3,3,3,3,3,3,3,3,3,3,3,3,3,3,3,3,3,3,3,3,3,4),(78.5398164398063,78.6677108218491,
78.788966381972,78.8875645069757,78.9860222897523,79.086244857525,79.1845244152532,
79.2827709943266,79.3810140773651,79.4827112660073,79.5810956794261,79.68444925568,
79.7878028319339,79.8864023576712,79.9848611556908,80.0832042043534,80.1814836418347,
80.2797289912669,80.3779697355283,80.4762993937657,80.5746716764509,80.673210932794,
80.7655329441315),.UNSPECIFIED.);
#669=B_SPLINE_CURVE_WITH_KNOTS('',3,(#62844,#62845,#62846,#62847,#62848,
#62849,#62850,#62851,#62852,#62853,#62854,#62855,#62856,#62857,#62858,#62859,
#62860,#62861,#62862,#62863,#62864,#62865,#62866,#62867,#62868,#62869,#62870,
#62871,#62872,#62873,#62874,#62875,#62876,#62877,#62878,#62879,#62880,#62881,
#62882,#62883,#62884,#62885,#62886,#62887,#62888,#62889,#62890,#62891,#62892,
#62893,#62894,#62895,#62896,#62897,#62898,#62899,#62900,#62901,#62902,#62903,
#62904,#62905,#62906,#62907,#62908,#62909,#62910,#62911,#62912,#62913),
 .UNSPECIFIED.,.F.,.F.,(4,3,3,3,3,3,3,3,3,3,3,3,3,3,3,3,3,3,3,3,3,3,3,4),
(78.539816339745,78.6377138097037,78.7346673304386,78.8315786913982,78.9284788661298,
79.0271081744509,79.1241353185132,79.2235657089638,79.3229960994143,79.421594224418,
79.5200520071948,79.6202745749675,79.7185541326956,79.8168007117689,79.9150437948075,
80.0167409834497,80.1151253968685,80.2184789731223,80.3218325493762,80.420438292131,
80.5188792313176,80.617224929138,80.7155010605394,80.7658264624535),
 .UNSPECIFIED.);
#670=B_SPLINE_CURVE_WITH_KNOTS('',3,(#62914,#62915,#62916,#62917,#62918,
#62919,#62920,#62921),.UNSPECIFIED.,.F.,.F.,(4,1,1,1,1,4),(74.4832630428072,
75.3276502995668,76.3264867495287,77.3253231994906,78.3241596494524,78.539816339745),
 .UNSPECIFIED.);
#671=B_SPLINE_CURVE_WITH_KNOTS('',3,(#62927,#62928,#62929,#62930,#62931,
#62932,#62933,#62934,#62935,#62936,#62937,#62938,#62939,#62940,#62941,#62942,
#62943,#62944,#62945,#62946,#62947,#62948,#62949,#62950,#62951,#62952,#62953,
#62954,#62955,#62956,#62957,#62958,#62959,#62960,#62961,#62962,#62963,#62964,
#62965,#62966,#62967,#62968,#62969,#62970,#62971,#62972,#62973,#62974,#62975,
#62976,#62977,#62978,#62979,#62980,#62981,#62982,#62983,#62984,#62985,#62986,
#62987,#62988,#62989,#62990,#62991,#62992,#62993,#62994,#62995,#62996,#62997,
#62998,#62999,#63000,#63001,#63002,#63003,#63004,#63005,#63006,#63007,#63008,
#63009,#63010,#63011,#63012,#63013,#63014,#63015,#63016,#63017,#63018,#63019,
#63020,#63021,#63022,#63023,#63024,#63025,#63026,#63027,#63028,#63029,#63030,
#63031,#63032,#63033,#63034,#63035,#63036,#63037,#63038,#63039,#63040,#63041,
#63042,#63043,#63044,#63045,#63046,#63047,#63048,#63049,#63050),
 .UNSPECIFIED.,.F.,.F.,(4,3,3,3,3,3,3,3,3,3,3,3,3,3,3,3,3,3,3,3,3,3,3,3,
3,3,3,3,3,3,3,3,3,3,3,3,3,3,3,3,3,4),(68.1995885751602,68.2978347417454,
68.3960780917011,68.4972090393642,68.5955944498561,68.6980981661047,68.8006018823533,
68.8992000073569,68.9976577901337,69.0978803579063,69.1961599156345,69.2944064947079,
69.3926495777462,69.4943467663884,69.5927311798072,69.6960847560611,69.7994383323151,
69.8980364573188,69.9964942400957,70.0967168078684,70.1949963655966,70.2932429446699,
70.3914860277088,70.4931832163508,70.5915676297697,70.6949212060233,70.798274782277,
70.8968729072808,70.9953306900575,71.0955532578301,71.1938328155584,71.2920793946318,
71.3903224776704,71.4920196663125,71.5904040797312,71.6937576559851,71.7971112322389,
71.9028340905518,72.0081993817383,72.1133399321502,72.2181701837247,72.2566308185806),
 .UNSPECIFIED.);
#672=B_SPLINE_CURVE_WITH_KNOTS('',3,(#63051,#63052,#63053,#63054,#63055,
#63056),.UNSPECIFIED.,.F.,.F.,(4,1,1,4),(72.2566310325654,72.7959476822008,
73.7947841321626,74.4816441096174),.UNSPECIFIED.);
#673=B_SPLINE_CURVE_WITH_KNOTS('',3,(#63058,#63059,#63060,#63061,#63062,
#63063,#63064),.UNSPECIFIED.,.F.,.F.,(4,1,1,1,4),(72.2566310325654,72.3311409496812,
73.3299773996431,74.3288138496049,74.4832630428072),.UNSPECIFIED.);
#674=B_SPLINE_CURVE_WITH_KNOTS('',3,(#63065,#63066,#63067,#63068,#63069,
#63070,#63071,#63072,#63073,#63074,#63075,#63076,#63077,#63078,#63079,#63080,
#63081,#63082,#63083,#63084,#63085,#63086,#63087,#63088,#63089,#63090,#63091,
#63092,#63093,#63094,#63095,#63096,#63097,#63098,#63099,#63100,#63101,#63102,
#63103,#63104,#63105,#63106,#63107,#63108,#63109,#63110,#63111,#63112,#63113,
#63114,#63115,#63116,#63117,#63118,#63119,#63120,#63121,#63122,#63123,#63124,
#63125,#63126,#63127,#63128,#63129,#63130,#63131,#63132,#63133,#63134,#63135,
#63136,#63137,#63138,#63139,#63140,#63141,#63142,#63143,#63144,#63145,#63146,
#63147,#63148,#63149,#63150,#63151,#63152,#63153,#63154,#63155,#63156,#63157,
#63158,#63159,#63160,#63161,#63162,#63163,#63164,#63165,#63166,#63167,#63168,
#63169,#63170,#63171,#63172,#63173,#63174,#63175,#63176,#63177,#63178,#63179,
#63180,#63181,#63182,#63183,#63184,#63185,#63186,#63187,#63188,#63189,#63190,
#63191),.UNSPECIFIED.,.F.,.F.,(4,3,3,3,3,3,3,3,3,3,3,3,3,3,3,3,3,3,3,3,
3,3,3,3,3,3,3,3,3,3,3,3,3,3,3,3,3,3,3,3,3,3,4),(68.1987514894476,68.2973434467588,
68.3357951498337,68.4343932748374,68.5328510576141,68.6330736253868,68.731353183115,
68.8295997621883,68.9278428452268,69.029540033869,69.1279244472878,69.2312780235417,
69.3346315997956,69.4332297247993,69.5316875075761,69.6319100753487,69.7301896330769,
69.8284362121503,69.9266792951887,70.0283764838309,70.1267608972497,70.2301144735036,
70.3334680497574,70.4320661747611,70.5305239575378,70.6307465253105,70.7290260830387,
70.8272726621121,70.9255157451505,71.0272129337927,71.1255973472115,71.2289509234654,
71.3323044997193,71.4298807240689,71.5273176349422,71.6246428433671,71.7219081150621,
71.8191441424517,71.9163815796695,72.013708783522,72.1110862397604,72.2086145464311,
72.2566310325654),.UNSPECIFIED.);
#675=B_SPLINE_CURVE_WITH_KNOTS('',3,(#63197,#63198,#63199,#63200,#63201,
#63202,#63203,#63204),.UNSPECIFIED.,.F.,.F.,(4,1,1,1,1,4),(61.9167164720863,
62.807583182582,63.8064196325439,64.8052560825058,65.8040925324676,65.9734457253857),
 .UNSPECIFIED.);
#676=B_SPLINE_CURVE_WITH_KNOTS('',3,(#63205,#63206,#63207,#63208,#63209,
#63210,#63211,#63212,#63213,#63214,#63215,#63216,#63217,#63218,#63219,#63220,
#63221,#63222,#63223,#63224,#63225,#63226,#63227,#63228,#63229,#63230,#63231,
#63232,#63233,#63234,#63235,#63236,#63237,#63238,#63239,#63240,#63241,#63242,
#63243,#63244,#63245,#63246,#63247,#63248,#63249,#63250,#63251,#63252,#63253,
#63254,#63255,#63256,#63257,#63258,#63259,#63260,#63261,#63262,#63263,#63264,
#63265,#63266,#63267,#63268,#63269,#63270,#63271,#63272,#63273,#63274),
 .UNSPECIFIED.,.F.,.F.,(4,3,3,3,3,3,3,3,3,3,3,3,3,3,3,3,3,3,3,3,3,3,3,4),
(65.9734457253857,66.0704340596178,66.1673127975358,66.264132888756,66.360925426791,
66.4577214670338,66.5546134226801,66.6515579893416,66.7486626585399,66.8029289824295,
66.9015271074332,66.99998489021,67.1002074579827,67.1984870157108,67.2967335947842,
67.3949766778227,67.4966738664649,67.5950582798838,67.6984118561376,67.8017654323914,
67.9012212180836,67.9996662359346,68.0996274055474,68.1995885751602),
 .UNSPECIFIED.);
#677=B_SPLINE_CURVE_WITH_KNOTS('',3,(#63276,#63277,#63278,#63279,#63280,
#63281,#63282,#63283,#63284,#63285,#63286,#63287,#63288,#63289,#63290,#63291,
#63292,#63293,#63294,#63295,#63296,#63297,#63298,#63299,#63300,#63301,#63302,
#63303,#63304,#63305,#63306,#63307,#63308,#63309,#63310,#63311,#63312,#63313,
#63314,#63315,#63316,#63317,#63318,#63319,#63320,#63321,#63322,#63323,#63324,
#63325,#63326,#63327,#63328,#63329,#63330,#63331,#63332,#63333,#63334,#63335,
#63336,#63337,#63338,#63339,#63340,#63341,#63342,#63343,#63344,#63345),
 .UNSPECIFIED.,.F.,.F.,(4,3,3,3,3,3,3,3,3,3,3,3,3,3,3,3,3,3,3,3,3,3,3,4),
(65.9734457256204,66.084879805074,66.1968635637049,66.3094957826842,66.3381222499099,
66.4367203749136,66.5351781576905,66.6354007254632,66.7336802831913,66.8319268622647,
66.9301699453032,67.0318671339454,67.1302515473642,67.233605123618,67.3369586998718,
67.4355663370611,67.534004594347,67.632346634809,67.7306220560113,67.8288603843819,
67.9271329658687,68.0254205103534,68.1238183934725,68.1987514894476),
 .UNSPECIFIED.);
#678=B_SPLINE_CURVE_WITH_KNOTS('',3,(#63346,#63347,#63348,#63349,#63350,
#63351,#63352,#63353,#63354,#63355,#63356,#63357,#63358,#63359,#63360,#63361,
#63362,#63363,#63364,#63365,#63366,#63367,#63368,#63369,#63370,#63371,#63372,
#63373,#63374,#63375,#63376,#63377,#63378,#63379,#63380,#63381,#63382,#63383,
#63384,#63385,#63386,#63387,#63388,#63389,#63390,#63391,#63392,#63393,#63394,
#63395,#63396,#63397,#63398,#63399,#63400,#63401,#63402,#63403,#63404,#63405,
#63406,#63407,#63408,#63409,#63410,#63411,#63412,#63413,#63414,#63415,#63416,
#63417,#63418,#63419,#63420,#63421,#63422,#63423,#63424,#63425,#63426,#63427,
#63428,#63429,#63430,#63431,#63432,#63433,#63434,#63435,#63436,#63437,#63438,
#63439,#63440,#63441,#63442,#63443,#63444,#63445,#63446,#63447,#63448,#63449,
#63450,#63451,#63452,#63453,#63454,#63455,#63456,#63457,#63458,#63459,#63460,
#63461,#63462,#63463,#63464,#63465,#63466,#63467,#63468,#63469,#63470,#63471,
#63472),.UNSPECIFIED.,.F.,.F.,(4,3,3,3,3,3,3,3,3,3,3,3,3,3,3,3,3,3,3,3,
3,3,3,3,3,3,3,3,3,3,3,3,3,3,3,3,3,3,3,3,3,3,4),(61.9158792493284,62.0141405915021,
62.1125119987853,62.2109478186409,62.309542353619,62.3427764500624,62.4413745750661,
62.5398323578427,62.6400549256154,62.7383344833436,62.8365810624171,62.9348241454556,
63.0365213340977,63.1349057475165,63.2382593237704,63.3416129000243,63.440211025028,
63.5386688078045,63.6388913755772,63.7371709333053,63.8354175123787,63.9336605954171,
64.0353577840594,64.1337421974782,64.2370957737322,64.3404493499862,64.4390474749898,
64.5375052577665,64.6377278255392,64.7360073832672,64.8342539623407,64.9324970453793,
65.0341942340215,65.1325786474403,65.2359322236942,65.3392857999481,65.4384637976084,
65.5374980774502,65.6364173808603,65.7352455972603,65.8340208922133,65.9327849002203,
65.9734457253857),.UNSPECIFIED.);
#679=B_SPLINE_CURVE_WITH_KNOTS('',3,(#63478,#63479,#63480,#63481,#63482,
#63483,#63484,#63485,#63486,#63487,#63488,#63489,#63490,#63491,#63492,#63493,
#63494,#63495,#63496,#63497,#63498,#63499,#63500,#63501,#63502,#63503,#63504,
#63505,#63506,#63507,#63508,#63509,#63510,#63511,#63512,#63513,#63514,#63515,
#63516,#63517,#63518,#63519,#63520,#63521,#63522,#63523,#63524,#63525,#63526,
#63527,#63528,#63529,#63530,#63531,#63532,#63533,#63534,#63535,#63536,#63537,
#63538,#63539,#63540,#63541,#63542,#63543,#63544,#63545,#63546,#63547,#63548,
#63549,#63550,#63551,#63552,#63553,#63554,#63555,#63556,#63557,#63558,#63559,
#63560,#63561,#63562,#63563,#63564,#63565,#63566,#63567,#63568,#63569,#63570,
#63571,#63572,#63573,#63574,#63575,#63576,#63577,#63578,#63579,#63580,#63581,
#63582,#63583,#63584,#63585,#63586,#63587,#63588,#63589,#63590,#63591,#63592,
#63593,#63594,#63595,#63596,#63597,#63598,#63599,#63600,#63601),
 .UNSPECIFIED.,.F.,.F.,(4,3,3,3,3,3,3,3,3,3,3,3,3,3,3,3,3,3,3,3,3,3,3,3,
3,3,3,3,3,3,3,3,3,3,3,3,3,3,3,3,3,4),(55.6323251840425,55.7308982483116,
55.8157280328489,55.9143261578526,56.0127839406294,56.1130065084021,56.2112860661302,
56.3095326452036,56.4077757282421,56.5094729168843,56.6078573303031,56.7112109065569,
56.8145644828108,56.9131626078145,57.0116203905912,57.1118429583639,57.2101225160921,
57.3083690951655,57.406612178204,57.5083093668461,57.606693780265,57.7100473565188,
57.8134009327727,57.9119990577764,58.010456840553,58.1106794083257,58.2089589660538,
58.3072055451272,58.4054486281657,58.5071458168079,58.6055302302267,58.7088838064806,
58.8122373827345,58.9094791608007,59.0070768179764,59.1040671063403,59.2009981633323,
59.2979009849174,59.3959908432396,59.4929780422902,59.5916192302482,59.6902604182062),
 .UNSPECIFIED.);
#680=B_SPLINE_CURVE_WITH_KNOTS('',3,(#63602,#63603,#63604,#63605,#63606,
#63607,#63608),.UNSPECIFIED.,.F.,.F.,(4,1,1,1,4),(59.6902604182062,59.8110738326964,
60.8099102826583,61.8087467326202,61.9167164720863),.UNSPECIFIED.);
#681=B_SPLINE_CURVE_WITH_KNOTS('',3,(#63610,#63611,#63612,#63613,#63614,
#63615,#63616,#63617,#63618,#63619,#63620,#63621,#63622,#63623,#63624,#63625,
#63626,#63627,#63628,#63629,#63630,#63631,#63632,#63633,#63634,#63635,#63636,
#63637,#63638,#63639,#63640,#63641,#63642,#63643,#63644,#63645,#63646,#63647,
#63648,#63649,#63650,#63651,#63652,#63653,#63654,#63655,#63656,#63657,#63658,
#63659,#63660,#63661,#63662,#63663,#63664,#63665,#63666,#63667,#63668,#63669,
#63670,#63671,#63672,#63673,#63674,#63675,#63676,#63677,#63678,#63679),
 .UNSPECIFIED.,.F.,.F.,(4,3,3,3,3,3,3,3,3,3,3,3,3,3,3,3,3,3,3,3,3,3,3,4),
(59.6902604182062,59.788634173056,59.8869985815969,59.9853827919993,60.0838846667642,
60.1824499292134,60.2811933482972,60.3451035501387,60.4437016751424,60.5421594579191,
60.6423820256918,60.7406615834199,60.8389081624934,60.937151245532,61.0388484341741,
61.1372328475929,61.2405864238468,61.3439400001006,61.4425291322775,61.5409847704297,
61.6393272818776,61.7376024228545,61.835858921854,61.9158792493284),
 .UNSPECIFIED.);
#682=B_SPLINE_CURVE_WITH_KNOTS('',3,(#63680,#63681,#63682,#63683,#63684,
#63685,#63686,#63687,#63688,#63689,#63690,#63691,#63692,#63693,#63694,#63695,
#63696,#63697,#63698,#63699,#63700,#63701,#63702,#63703,#63704,#63705,#63706,
#63707,#63708,#63709,#63710,#63711,#63712,#63713,#63714,#63715,#63716,#63717,
#63718,#63719,#63720,#63721,#63722,#63723,#63724,#63725,#63726,#63727,#63728,
#63729,#63730,#63731,#63732,#63733,#63734,#63735,#63736,#63737,#63738,#63739,
#63740,#63741,#63742,#63743,#63744,#63745,#63746,#63747,#63748,#63749,#63750,
#63751,#63752,#63753,#63754,#63755,#63756,#63757,#63758,#63759,#63760,#63761,
#63762,#63763,#63764,#63765,#63766,#63767,#63768,#63769,#63770,#63771,#63772,
#63773,#63774,#63775,#63776,#63777,#63778,#63779,#63780,#63781,#63782,#63783,
#63784,#63785,#63786,#63787,#63788,#63789,#63790,#63791,#63792,#63793,#63794,
#63795,#63796,#63797,#63798,#63799,#63800,#63801,#63802,#63803),
 .UNSPECIFIED.,.F.,.F.,(4,3,3,3,3,3,3,3,3,3,3,3,3,3,3,3,3,3,3,3,3,3,3,3,
3,3,3,3,3,3,3,3,3,3,3,3,3,3,3,3,3,4),(55.6334625298916,55.7317495743948,
55.8299992179396,55.9282409473069,56.0265042327944,56.12487847957,56.2233185899107,
56.3219158848567,56.3497577502912,56.4483558752948,56.5468136580713,56.6470362258441,
56.7453157835722,56.8435623626454,56.941805445684,57.0435026343263,57.1418870477452,
57.2452406239991,57.3485942002531,57.4471923252568,57.5456501080334,57.6458726758061,
57.7441522335343,57.8423988126077,57.9406418956461,58.0423390842883,58.1407234977071,
58.244077073961,58.3474306502149,58.4460287752186,58.5444865579954,58.644709125768,
58.7429886834962,58.8412352625695,58.939478345608,59.0411755342502,59.1395599476691,
59.242913523923,59.3462671001768,59.4608829140306,59.5755716660049,59.6902604179793),
 .UNSPECIFIED.);
#683=B_SPLINE_CURVE_WITH_KNOTS('',3,(#63809,#63810,#63811,#63812,#63813,
#63814,#63815,#63816),.UNSPECIFIED.,.F.,.F.,(4,1,1,1,1,4),(49.3495871775425,
49.8227093330777,50.8215457830395,51.8203822330014,52.8192186829633,53.4070751110266),
 .UNSPECIFIED.);
#684=B_SPLINE_CURVE_WITH_KNOTS('',3,(#63817,#63818,#63819,#63820,#63821,
#63822,#63823,#63824,#63825,#63826,#63827,#63828,#63829,#63830,#63831,#63832,
#63833,#63834,#63835,#63836,#63837,#63838,#63839,#63840,#63841,#63842,#63843,
#63844,#63845,#63846,#63847,#63848,#63849,#63850,#63851,#63852,#63853,#63854,
#63855,#63856,#63857,#63858,#63859,#63860,#63861,#63862,#63863,#63864,#63865,
#63866,#63867,#63868,#63869,#63870,#63871,#63872,#63873,#63874,#63875,#63876,
#63877,#63878,#63879,#63880,#63881,#63882,#63883,#63884,#63885,#63886),
 .UNSPECIFIED.,.F.,.F.,(4,3,3,3,3,3,3,3,3,3,3,3,3,3,3,3,3,3,3,3,3,3,3,4),
(53.4070755243615,53.5149520672712,53.6231638610662,53.7318758460164,53.8180551329252,
53.9166532579289,54.0151110407057,54.1153336084784,54.2136131662065,54.3118597452799,
54.4101028283183,54.5118000169605,54.6101844303793,54.7135380066332,54.816891582887,
54.9188207830314,55.0172568602171,55.1155965155782,55.2138693470808,55.3121048809365,
55.410364322371,55.5086391351003,55.6069975873545,55.6323251840425),
 .UNSPECIFIED.);
#685=B_SPLINE_CURVE_WITH_KNOTS('',3,(#63888,#63889,#63890,#63891,#63892,
#63893,#63894,#63895,#63896,#63897,#63898,#63899,#63900,#63901,#63902,#63903,
#63904,#63905,#63906,#63907,#63908,#63909,#63910,#63911,#63912,#63913,#63914,
#63915,#63916,#63917,#63918,#63919,#63920,#63921,#63922,#63923,#63924,#63925,
#63926,#63927,#63928,#63929,#63930,#63931,#63932,#63933,#63934,#63935,#63936,
#63937,#63938,#63939,#63940,#63941,#63942,#63943,#63944,#63945,#63946,#63947,
#63948,#63949,#63950,#63951,#63952,#63953,#63954,#63955,#63956,#63957),
 .UNSPECIFIED.,.F.,.F.,(4,3,3,3,3,3,3,3,3,3,3,3,3,3,3,3,3,3,3,3,3,3,3,4),
(53.4070751110266,53.5048543854907,53.6024983707769,53.7000367768843,53.7975186210124,
53.8949743677959,53.9924344477701,54.0899931990353,54.1876041339863,54.2853815723758,
54.3520848503674,54.4506829753712,54.549140758148,54.6493633259206,54.7476428836488,
54.8458894627222,54.9441325457609,55.045829734403,55.1442141478217,55.2475677240755,
55.3509213003293,55.4495112354575,55.5479503969195,55.6334625298916),
 .UNSPECIFIED.);
#686=B_SPLINE_CURVE_WITH_KNOTS('',3,(#63958,#63959,#63960,#63961,#63962,
#63963,#63964,#63965,#63966),.UNSPECIFIED.,.F.,.F.,(4,1,1,1,1,1,4),(49.3496770994594,
49.3579026005581,50.3567390505199,51.3555755004818,52.3544119504437,53.3532484004056,
53.4070751110266),.UNSPECIFIED.);
#687=B_SPLINE_CURVE_WITH_KNOTS('',3,(#63972,#63973,#63974,#63975,#63976,
#63977,#63978,#63979,#63980,#63981,#63982,#63983,#63984,#63985,#63986,#63987,
#63988,#63989,#63990,#63991,#63992,#63993,#63994,#63995,#63996,#63997,#63998,
#63999,#64000,#64001,#64002,#64003,#64004,#64005,#64006,#64007,#64008,#64009,
#64010,#64011,#64012,#64013,#64014,#64015,#64016,#64017,#64018,#64019,#64020,
#64021,#64022,#64023,#64024,#64025,#64026,#64027,#64028,#64029,#64030,#64031,
#64032,#64033,#64034,#64035,#64036,#64037,#64038,#64039,#64040,#64041,#64042,
#64043,#64044,#64045,#64046,#64047,#64048,#64049,#64050,#64051,#64052,#64053,
#64054,#64055,#64056,#64057,#64058,#64059,#64060,#64061,#64062,#64063,#64064,
#64065,#64066,#64067,#64068,#64069,#64070,#64071,#64072,#64073,#64074,#64075,
#64076,#64077,#64078,#64079,#64080,#64081,#64082,#64083,#64084,#64085,#64086,
#64087,#64088,#64089,#64090,#64091,#64092,#64093,#64094,#64095),
 .UNSPECIFIED.,.F.,.F.,(4,3,3,3,3,3,3,3,3,3,3,3,3,3,3,3,3,3,3,3,3,3,3,3,
3,3,3,3,3,3,3,3,3,3,3,3,3,3,3,3,3,4),(43.0671358249316,43.1654506744533,
43.2637142379643,43.3619560191833,43.4602054928574,43.558557934537,43.6569637792126,
43.7555405534103,43.8296906333064,43.9282887583115,44.0267465410897,44.126969108862,
44.2252486665916,44.3234952456663,44.4217383287061,44.5234355173466,44.6218199307669,
44.7251735070176,44.8285270832683,44.9271252082716,45.0255829910478,45.1258055588206,
45.2240851165483,45.3223316956211,45.4205747786593,45.5222719673021,45.6206563807204,
45.7240099569753,45.8273635332302,45.9259616582338,46.0244194410105,46.1246420087832,
46.2229215665111,46.3211681455844,46.4194112286225,46.5211084172649,46.6194928306835,
46.7228464069377,46.826199983192,46.9466622822341,47.0654828012636,47.1238896269672),
 .UNSPECIFIED.);
#688=B_SPLINE_CURVE_WITH_KNOTS('',3,(#64096,#64097,#64098,#64099,#64100,
#64101),.UNSPECIFIED.,.F.,.F.,(4,1,1,4),(47.123889803847,47.8250364331539,
48.8238728831158,49.3495871775425),.UNSPECIFIED.);
#689=B_SPLINE_CURVE_WITH_KNOTS('',3,(#64103,#64104,#64105,#64106,#64107,
#64108),.UNSPECIFIED.,.F.,.F.,(4,1,1,4),(47.1238901033263,47.3602297006343,
48.3590661505962,49.3496770994594),.UNSPECIFIED.);
#690=B_SPLINE_CURVE_WITH_KNOTS('',3,(#64109,#64110,#64111,#64112,#64113,
#64114,#64115,#64116,#64117,#64118,#64119,#64120,#64121,#64122,#64123,#64124,
#64125,#64126,#64127,#64128,#64129,#64130,#64131,#64132,#64133,#64134,#64135,
#64136,#64137,#64138,#64139,#64140,#64141,#64142,#64143,#64144,#64145,#64146,
#64147,#64148,#64149,#64150,#64151,#64152,#64153,#64154,#64155,#64156,#64157,
#64158,#64159,#64160,#64161,#64162,#64163,#64164,#64165,#64166,#64167,#64168,
#64169,#64170,#64171,#64172,#64173,#64174,#64175,#64176,#64177,#64178,#64179,
#64180,#64181,#64182,#64183,#64184,#64185,#64186,#64187,#64188,#64189,#64190,
#64191,#64192,#64193,#64194,#64195,#64196,#64197,#64198,#64199,#64200,#64201,
#64202,#64203,#64204,#64205,#64206,#64207,#64208,#64209,#64210,#64211,#64212,
#64213,#64214,#64215,#64216,#64217,#64218,#64219,#64220,#64221,#64222,#64223,
#64224,#64225,#64226,#64227,#64228,#64229,#64230,#64231,#64232),
 .UNSPECIFIED.,.F.,.F.,(4,3,3,3,3,3,3,3,3,3,3,3,3,3,3,3,3,3,3,3,3,3,3,3,
3,3,3,3,3,3,3,3,3,3,3,3,3,3,3,3,3,4),(43.0660207696421,43.1644088774625,
43.2646463891246,43.3648839007868,43.4634820258003,43.5619398085869,43.6621623763571,
43.7604419340954,43.858688513179,43.956931596228,44.0586287848581,44.1570131982874,
44.260366774518,44.3637203507487,44.4623184757497,44.5607762585235,44.6609988262969,
44.7592783840224,44.8575249630931,44.9557680461289,45.0574652347743,45.1558496481904,
45.2592032244505,45.3625568007106,45.4611549257132,45.5596127084888,45.6598352762618,
45.7581148339887,45.856361413061,45.9546044960978,46.0563016847414,46.1546860981589,
46.2580396744157,46.3613932506724,46.4587199838046,46.5559210250952,46.6530274701203,
46.7500702965179,46.8471124553621,46.9441490048064,47.0412721236584,47.123889803847),
 .UNSPECIFIED.);
#691=B_SPLINE_CURVE_WITH_KNOTS('',3,(#64238,#64239,#64240,#64241,#64242,
#64243,#64244,#64245,#64246,#64247,#64248,#64249,#64250,#64251,#64252,#64253,
#64254,#64255,#64256,#64257,#64258,#64259,#64260,#64261,#64262,#64263,#64264,
#64265,#64266,#64267,#64268,#64269,#64270,#64271,#64272,#64273,#64274,#64275,
#64276,#64277,#64278,#64279,#64280,#64281,#64282,#64283,#64284,#64285,#64286,
#64287,#64288,#64289,#64290,#64291,#64292,#64293,#64294,#64295,#64296,#64297,
#64298,#64299,#64300,#64301,#64302,#64303,#64304,#64305,#64306,#64307,#64308,
#64309,#64310,#64311,#64312,#64313,#64314,#64315,#64316,#64317,#64318,#64319,
#64320,#64321,#64322,#64323,#64324,#64325,#64326,#64327,#64328,#64329,#64330,
#64331,#64332,#64333,#64334,#64335,#64336,#64337,#64338,#64339,#64340,#64341,
#64342,#64343,#64344,#64345,#64346,#64347,#64348,#64349,#64350,#64351,#64352,
#64353,#64354,#64355,#64356,#64357,#64358,#64359,#64360,#64361,#64362,#64363,
#64364),.UNSPECIFIED.,.F.,.F.,(4,3,3,3,3,3,3,3,3,3,3,3,3,3,3,3,3,3,3,3,
3,3,3,3,3,3,3,3,3,3,3,3,3,3,3,3,3,3,3,3,3,3,4),(36.7830721123744,36.8378354835733,
36.9364336084867,37.0348913911713,37.1351139589668,37.2333935165991,37.3316400955754,
37.4298831785158,37.5315803672706,37.6299647805896,37.7333183570624,37.8366719335352,
37.9352700586076,38.0337278414541,38.1339504092095,38.2322299670092,38.3304765461547,
38.4287196292657,38.5304168178235,38.6288012313153,38.7321548074061,38.835508383497,
38.9341065084864,39.0325642912488,39.132786859025,39.2310664167388,39.3293129957978,
39.4275560788219,39.5292532674812,39.6276376808859,39.7309912571724,39.8343448334589,
39.9329429584521,40.0314007412181,40.1316233089934,40.2299028667104,40.3281494457725,
40.4263925287995,40.5280897174548,40.6264741308619,40.7298277071414,40.8331812834208,
40.8407044966674),.UNSPECIFIED.);
#692=B_SPLINE_CURVE_WITH_KNOTS('',3,(#64365,#64366,#64367,#64368,#64369,
#64370,#64371,#64372,#64373,#64374,#64375,#64376,#64377,#64378,#64379,#64380,
#64381,#64382,#64383,#64384,#64385,#64386,#64387,#64388,#64389,#64390,#64391,
#64392,#64393,#64394,#64395,#64396,#64397,#64398,#64399,#64400,#64401,#64402,
#64403,#64404,#64405,#64406,#64407,#64408,#64409,#64410,#64411,#64412,#64413,
#64414,#64415,#64416,#64417,#64418,#64419,#64420,#64421,#64422,#64423,#64424,
#64425,#64426,#64427,#64428,#64429,#64430,#64431,#64432,#64433,#64434),
 .UNSPECIFIED.,.F.,.F.,(4,3,3,3,3,3,3,3,3,3,3,3,3,3,3,3,3,3,3,3,3,3,3,4),
(40.8407044969197,40.9391705387198,41.037496428004,41.1368115911763,41.2349607512892,
41.3330774110127,41.4311912274061,41.5313978539003,41.6296531901072,41.730835461745,
41.8320177333827,41.9306158583838,42.029073641158,42.1292962089313,42.2275757666567,
42.3258223457274,42.4240654287631,42.5257626174084,42.6241470308246,42.7275006070845,
42.8308541833445,42.9294559188181,43.0279051778381,43.0671358249316),
 .UNSPECIFIED.);
#693=B_SPLINE_CURVE_WITH_KNOTS('',3,(#64436,#64437,#64438,#64439,#64440,
#64441,#64442,#64443,#64444,#64445,#64446,#64447,#64448,#64449,#64450,#64451,
#64452,#64453,#64454,#64455,#64456,#64457,#64458,#64459,#64460,#64461,#64462,
#64463,#64464,#64465,#64466,#64467,#64468,#64469,#64470,#64471,#64472,#64473,
#64474,#64475,#64476,#64477,#64478,#64479,#64480,#64481,#64482,#64483,#64484,
#64485,#64486,#64487,#64488,#64489,#64490,#64491,#64492,#64493,#64494,#64495,
#64496,#64497,#64498,#64499,#64500,#64501,#64502,#64503,#64504,#64505),
 .UNSPECIFIED.,.F.,.F.,(4,3,3,3,3,3,3,3,3,3,3,3,3,3,3,3,3,3,3,3,3,3,3,4),
(40.8407044966674,40.9425310419933,41.0487010317108,41.1508691915798,41.2531658485548,
41.3556785603237,41.3672110008631,41.4658091258525,41.5642669086149,41.6644894763912,
41.7627690341049,41.8610156131639,41.959258696188,42.0609558848472,42.159340298252,
42.2626938745384,42.3660474508249,42.4646234053317,42.5630692109038,42.6614145832016,
42.7625661298117,42.8608128923214,42.9634168309817,43.0660207696421),
 .UNSPECIFIED.);
#694=B_SPLINE_CURVE_WITH_KNOTS('',3,(#64506,#64507,#64508,#64509,#64510,
#64511,#64512,#64513),.UNSPECIFIED.,.F.,.F.,(4,1,1,1,1,4),(36.7838197774947,
37.3718652010156,38.3707016509774,39.3695381009393,40.3683745509012,40.8407024148877),
 .UNSPECIFIED.);
#695=B_SPLINE_CURVE_WITH_KNOTS('',3,(#64519,#64520,#64521,#64522,#64523,
#64524,#64525,#64526,#64527,#64528,#64529,#64530,#64531,#64532,#64533,#64534,
#64535,#64536,#64537,#64538,#64539,#64540,#64541,#64542,#64543,#64544,#64545,
#64546,#64547,#64548,#64549,#64550,#64551,#64552,#64553,#64554,#64555,#64556,
#64557,#64558,#64559,#64560,#64561,#64562,#64563,#64564,#64565,#64566,#64567,
#64568,#64569,#64570,#64571,#64572,#64573,#64574,#64575,#64576,#64577,#64578,
#64579,#64580,#64581,#64582,#64583,#64584,#64585,#64586,#64587,#64588,#64589,
#64590,#64591,#64592,#64593,#64594,#64595,#64596,#64597,#64598,#64599,#64600,
#64601,#64602,#64603,#64604,#64605,#64606,#64607,#64608,#64609,#64610,#64611,
#64612,#64613,#64614,#64615,#64616,#64617,#64618,#64619,#64620,#64621,#64622,
#64623,#64624,#64625,#64626,#64627,#64628,#64629,#64630,#64631,#64632,#64633,
#64634,#64635,#64636,#64637,#64638,#64639,#64640,#64641,#64642,#64643,#64644,
#64645),.UNSPECIFIED.,.F.,.F.,(4,3,3,3,3,3,3,3,3,3,3,3,3,3,3,3,3,3,3,3,
3,3,3,3,3,3,3,3,3,3,3,3,3,3,3,3,3,3,3,3,3,3,4),(30.4997391997366,30.5981024250019,
30.6965256310033,30.7951123412346,30.844816783802,30.9434149029217,31.0418726797114,
31.1420952489679,31.240374800498,31.3386213733081,31.4368644500261,31.5385616459606,
31.6369460529803,31.7402996433721,31.8436532337639,31.9422513619701,32.0407091479896,
32.1409317149566,32.2392112760025,32.3374578584144,32.4357009448076,32.5373981295371,
32.6357825463172,32.7391361150215,32.8424896837258,32.941087808515,33.0395455910825,
33.1397681589082,33.2380477164417,33.3362942953263,33.4345373781827,33.5362345670589,
33.6346189803128,33.7379725570002,33.8413261336877,33.9390973941506,34.0367388270547,
34.1342810926888,34.2317547370042,34.3292101035739,34.4266554953284,34.5241539309046,
34.5575191894878),.UNSPECIFIED.);
#696=B_SPLINE_CURVE_WITH_KNOTS('',3,(#64646,#64647,#64648,#64649,#64650,
#64651,#64652,#64653,#64654,#64655,#64656,#64657,#64658,#64659,#64660,#64661,
#64662,#64663,#64664,#64665,#64666,#64667,#64668,#64669,#64670,#64671,#64672,
#64673,#64674,#64675,#64676,#64677,#64678,#64679,#64680,#64681,#64682,#64683,
#64684,#64685,#64686,#64687,#64688,#64689,#64690,#64691,#64692,#64693,#64694,
#64695,#64696,#64697,#64698,#64699,#64700,#64701,#64702,#64703,#64704,#64705,
#64706,#64707,#64708,#64709,#64710,#64711,#64712,#64713,#64714,#64715),
 .UNSPECIFIED.,.F.,.F.,(4,3,3,3,3,3,3,3,3,3,3,3,3,3,3,3,3,3,3,3,3,3,3,4),
(34.5575191897594,34.6782345503652,34.8009387396128,34.8401625836495,34.938760709128,
35.0372184923859,35.1374410600391,35.2357206182603,35.3339671978303,35.4322102813681,
35.5339074694289,35.6322918833488,35.7356454584801,35.8389990336114,35.9376008413523,
36.0360613066058,36.1344037647061,36.2326817408451,36.3309247589454,36.4291623016109,
36.5274785677124,36.625837103631,36.724338350044,36.7830721123744),
 .UNSPECIFIED.);
#697=B_SPLINE_CURVE_WITH_KNOTS('',3,(#64717,#64718,#64719,#64720,#64721,
#64722),.UNSPECIFIED.,.F.,.F.,(4,1,1,4),(34.5575241466493,35.3741923010918,
36.3730287510537,36.7838197774947),.UNSPECIFIED.);
#698=B_SPLINE_CURVE_WITH_KNOTS('',3,(#64723,#64724,#64725,#64726,#64727,
#64728,#64729,#64730,#64731,#64732,#64733,#64734,#64735,#64736,#64737,#64738,
#64739,#64740,#64741,#64742,#64743,#64744,#64745,#64746,#64747,#64748,#64749,
#64750,#64751,#64752,#64753,#64754,#64755,#64756,#64757,#64758,#64759,#64760,
#64761,#64762,#64763,#64764,#64765,#64766,#64767,#64768,#64769,#64770,#64771,
#64772,#64773,#64774,#64775,#64776,#64777,#64778,#64779,#64780,#64781,#64782,
#64783,#64784,#64785,#64786,#64787,#64788,#64789,#64790,#64791,#64792,#64793,
#64794,#64795,#64796,#64797,#64798,#64799,#64800,#64801,#64802,#64803,#64804,
#64805,#64806,#64807,#64808,#64809,#64810,#64811,#64812,#64813,#64814,#64815,
#64816,#64817,#64818,#64819,#64820,#64821,#64822,#64823,#64824,#64825,#64826,
#64827,#64828,#64829,#64830,#64831,#64832,#64833,#64834,#64835,#64836,#64837,
#64838,#64839,#64840,#64841,#64842,#64843,#64844,#64845,#64846),
 .UNSPECIFIED.,.F.,.F.,(4,3,3,3,3,3,3,3,3,3,3,3,3,3,3,3,3,3,3,3,3,3,3,3,
3,3,3,3,3,3,3,3,3,3,3,3,3,3,3,3,3,4),(30.5006744364989,30.5991052402592,
30.6974320357731,30.7957023845,30.8939457980153,30.9921917542775,31.0905375391577,
31.1889321006504,31.2875030416228,31.3788465012443,31.4774446473005,31.575902451375,
31.6761250138539,31.7744045933259,31.8726511942622,31.9708942992537,32.0725914622418,
32.1709758976143,32.2743294244103,32.3776829512062,32.4762810765929,32.5747388598192,
32.6749614274878,32.7732409858268,32.8714875655702,32.9697306493373,33.071427837295,
33.169812251582,33.2731658263751,33.3765194011681,33.4751175202855,33.5735752970726,
33.6737978663298,33.7720774178574,33.8703239906649,33.9685670673804,34.0702642633178,
34.1686486703349,34.2720022607324,34.37535585113,34.5238559810743,34.5575191894878),
 .UNSPECIFIED.);
#699=B_SPLINE_CURVE_WITH_KNOTS('',3,(#64852,#64853,#64854,#64855,#64856,
#64857,#64858,#64859),.UNSPECIFIED.,.F.,.F.,(4,1,1,1,1,4),(24.2176478004184,
24.8517980840308,25.8506345339927,26.8494709839545,27.8483074339164,28.2743284148783),
 .UNSPECIFIED.);
#700=B_SPLINE_CURVE_WITH_KNOTS('',3,(#64860,#64861,#64862,#64863,#64864,
#64865,#64866,#64867,#64868,#64869,#64870,#64871,#64872,#64873,#64874,#64875,
#64876,#64877,#64878,#64879,#64880,#64881,#64882,#64883,#64884,#64885,#64886,
#64887,#64888,#64889,#64890,#64891,#64892,#64893,#64894,#64895,#64896,#64897,
#64898,#64899,#64900,#64901,#64902,#64903,#64904,#64905,#64906,#64907,#64908,
#64909,#64910,#64911,#64912,#64913,#64914,#64915,#64916,#64917,#64918,#64919,
#64920,#64921,#64922,#64923,#64924,#64925,#64926,#64927,#64928,#64929),
 .UNSPECIFIED.,.F.,.F.,(4,3,3,3,3,3,3,3,3,3,3,3,3,3,3,3,3,3,3,3,3,3,3,4),
(28.2743338823082,28.3746245107026,28.4749734040128,28.5754886322331,28.6760922705589,
28.7769068627545,28.8471438838783,28.9457420299255,29.0441998339908,29.144422396472,
29.2427019759346,29.3409485768615,29.4391916818436,29.5408888448427,29.6392732802058,
29.742626807023,29.8459803338402,29.9445606477241,30.0430096057709,30.1413569295411,
30.2396381186526,30.3378792535374,30.4361386871576,30.4997391997366),
 .UNSPECIFIED.);
#701=B_SPLINE_CURVE_WITH_KNOTS('',3,(#64931,#64932,#64933,#64934,#64935,
#64936,#64937,#64938,#64939,#64940,#64941,#64942,#64943,#64944,#64945,#64946,
#64947,#64948,#64949,#64950,#64951,#64952,#64953,#64954,#64955,#64956,#64957,
#64958,#64959,#64960,#64961,#64962,#64963,#64964,#64965,#64966,#64967,#64968,
#64969,#64970,#64971,#64972,#64973,#64974,#64975,#64976,#64977,#64978,#64979,
#64980,#64981,#64982,#64983,#64984,#64985,#64986,#64987,#64988,#64989,#64990,
#64991,#64992,#64993,#64994,#64995,#64996,#64997,#64998,#64999,#65000),
 .UNSPECIFIED.,.F.,.F.,(4,3,3,3,3,3,3,3,3,3,3,3,3,3,3,3,3,3,3,3,3,3,3,4),
(28.2743338823082,28.3823371513587,28.4809354104368,28.5793933287022,28.6796158627795,
28.7778955584748,28.8761422761379,28.9743854982056,29.0760825239843,29.1744670761058,
29.2778203387132,29.3811736013206,29.4797717427275,29.5782295425788,29.6784521061668,
29.7767316825037,29.8749782807199,29.9732213834117,30.0749185503794,30.1733029845339,
30.2766565179082,30.3800100512825,30.4786103665625,30.5006744364989),
 .UNSPECIFIED.);
#702=B_SPLINE_CURVE_WITH_KNOTS('',3,(#65001,#65002,#65003,#65004,#65005,
#65006,#65007,#65008,#65009,#65010,#65011,#65012,#65013,#65014,#65015,#65016,
#65017,#65018,#65019,#65020,#65021,#65022,#65023,#65024,#65025,#65026,#65027,
#65028,#65029,#65030,#65031,#65032,#65033,#65034,#65035,#65036,#65037,#65038,
#65039,#65040,#65041,#65042,#65043,#65044,#65045,#65046,#65047,#65048,#65049,
#65050,#65051,#65052,#65053,#65054,#65055,#65056,#65057,#65058,#65059,#65060,
#65061,#65062,#65063,#65064,#65065,#65066,#65067,#65068,#65069,#65070,#65071,
#65072,#65073,#65074,#65075,#65076,#65077,#65078,#65079,#65080,#65081,#65082,
#65083,#65084,#65085,#65086,#65087,#65088,#65089,#65090,#65091,#65092,#65093,
#65094,#65095,#65096,#65097,#65098,#65099,#65100,#65101,#65102,#65103,#65104,
#65105,#65106,#65107,#65108,#65109,#65110,#65111,#65112,#65113,#65114,#65115,
#65116,#65117,#65118,#65119,#65120,#65121,#65122,#65123,#65124,#65125,#65126,
#65127),.UNSPECIFIED.,.F.,.F.,(4,3,3,3,3,3,3,3,3,3,3,3,3,3,3,3,3,3,3,3,
3,3,3,3,3,3,3,3,3,3,3,3,3,3,3,3,3,3,3,3,3,3,4),(24.2164091062169,24.3149891554594,
24.3869913515112,24.4855869755136,24.5840422190559,24.6842654168581,24.7825423598393,
24.8807863016633,24.9790267283841,25.0807269966564,25.1791087331383,25.2824682673057,
25.3858278014731,25.4844267472597,25.5828853582973,25.6831077199395,25.7813881181849,
25.8796355405022,25.9778794683927,26.0795756641532,26.1779609177654,26.2813125846002,
26.384664251435,26.4832625890263,26.5817205904922,26.6819431043553,26.7802228942346,
26.8784697099906,26.976713033946,27.0784099508087,27.1767946133168,27.2801476573568,
27.3835007013968,27.4808124349029,27.5800026158,27.6770619108145,27.7740624128206,
27.8710350559302,27.9718597624675,28.0689211605358,28.1660361013683,28.2632831488084,
28.2743338820795),.UNSPECIFIED.);
#703=B_SPLINE_CURVE_WITH_KNOTS('',3,(#65133,#65134,#65135,#65136,#65137,
#65138),.UNSPECIFIED.,.F.,.F.,(4,1,1,4),(15.707963267949,16.3962997518162,
17.3951362017781,17.9335273147171),.UNSPECIFIED.);
#704=B_SPLINE_CURVE_WITH_KNOTS('',3,(#65140,#65141,#65142,#65143,#65144),
 .UNSPECIFIED.,.F.,.F.,(4,1,4),(14.3986268518925,15.3974633018543,15.707963267949),
 .UNSPECIFIED.);
#705=B_SPLINE_CURVE_WITH_KNOTS('',3,(#65148,#65149,#65150,#65151,#65152,
#65153,#65154,#65155,#65156,#65157,#65158,#65159,#65160,#65161,#65162,#65163,
#65164,#65165,#65166,#65167,#65168,#65169,#65170,#65171,#65172,#65173,#65174,
#65175,#65176,#65177,#65178,#65179,#65180,#65181,#65182,#65183,#65184,#65185,
#65186,#65187,#65188,#65189,#65190,#65191,#65192,#65193,#65194,#65195,#65196,
#65197,#65198,#65199,#65200,#65201,#65202,#65203,#65204,#65205),
 .UNSPECIFIED.,.F.,.F.,(4,3,3,3,3,3,3,3,3,3,3,3,3,3,3,3,3,3,3,4),(13.8757070305535,
13.9742334885845,14.0726196430263,14.1714713856995,14.2696800147308,14.3678555358063,
14.4660275256487,14.5653790403395,14.6636889428954,14.7635612636537,14.8634335844121,
14.9606976643214,15.0578044061946,15.154822904629,15.2517842090804,15.3487192963901,
15.4457083601634,15.5427241599105,15.6398692512359,15.707963267949),
 .UNSPECIFIED.);
#706=B_SPLINE_CURVE_WITH_KNOTS('',3,(#65206,#65207,#65208,#65209,#65210,
#65211,#65212),.UNSPECIFIED.,.F.,.F.,(4,1,1,1,4),(15.707963267949,15.8622700343739,
16.8611064843358,17.8599429342977,17.9342415705864),.UNSPECIFIED.);
#707=B_SPLINE_CURVE_WITH_KNOTS('',3,(#65218,#65219,#65220,#65221,#65222,
#65223,#65224,#65225,#65226,#65227,#65228,#65229,#65230,#65231,#65232,#65233,
#65234,#65235,#65236,#65237,#65238,#65239,#65240,#65241,#65242,#65243,#65244,
#65245,#65246,#65247,#65248,#65249,#65250,#65251,#65252,#65253,#65254,#65255),
 .UNSPECIFIED.,.F.,.F.,(4,2,2,2,2,2,2,2,2,2,2,2,2,2,2,2,2,2,4),(2.08269229218369E-5,
0.127845741022052,0.200677725447424,0.317389539257015,0.404625699897331,
0.484292562096328,0.651098313987348,0.735080070424923,0.809478158094123,
0.977078046750801,1.04711496328757,1.11953227018629,1.23167820677694,1.31165216412917,
1.44942689358888,1.5844225186206,1.6597570912359,1.79045634738967,1.80127748042845),
 .UNSPECIFIED.);
#708=B_SPLINE_CURVE_WITH_KNOTS('',3,(#65259,#65260,#65261,#65262,#65263,
#65264,#65265,#65266,#65267,#65268,#65269,#65270,#65271,#65272,#65273),
 .UNSPECIFIED.,.F.,.F.,(4,1,1,1,1,1,1,1,1,1,1,1,4),(2.02178176728025,2.43673748880502,
2.92408498656602,3.41143248432702,3.89877998208802,4.38612747984902,4.87347497761003,
5.36082247537103,5.84816997313203,6.33551747089303,6.82286496865404,7.31021246641504,
7.59153924858055),.UNSPECIFIED.);
#709=B_SPLINE_CURVE_WITH_KNOTS('',3,(#65274,#65275,#65276,#65277,#65278,
#65279,#65280,#65281,#65282,#65283,#65284,#65285,#65286,#65287,#65288,#65289),
 .UNSPECIFIED.,.F.,.F.,(4,3,3,3,3,4),(7.59153924858055,7.6845224783778,
7.77753299194073,7.79755996417604,7.88865013802183,7.94826257243732),
 .UNSPECIFIED.);
#710=B_SPLINE_CURVE_WITH_KNOTS('',3,(#65295,#65296,#65297,#65298,#65299,
#65300,#65301,#65302,#65303,#65304,#65305,#65306,#65307),.UNSPECIFIED.,
 .F.,.F.,(4,3,3,3,4),(-10.494778244858,-10.4064615792516,-10.3181205168946,
-10.2342974529811,-10.1382057107015),.UNSPECIFIED.);
#711=B_SPLINE_CURVE_WITH_KNOTS('',3,(#65308,#65309,#65310,#65311,#65312,
#65313,#65314,#65315,#65316,#65317,#65318,#65319,#65320,#65321,#65322,#65323,
#65324,#65325,#65326,#65327,#65328,#65329,#65330,#65331,#65332,#65333,#65334,
#65335,#65336,#65337,#65338,#65339,#65340,#65341,#65342,#65343,#65344,#65345,
#65346,#65347,#65348,#65349,#65350,#65351,#65352,#65353,#65354,#65355,#65356,
#65357,#65358,#65359,#65360,#65361),.UNSPECIFIED.,.F.,.F.,(4,2,2,2,2,2,
2,2,2,2,2,2,2,2,2,2,2,2,2,2,2,2,2,2,2,2,4),(1.80127748042845,1.89084368471754,
1.95813908989248,2.04086238183236,2.16780801322339,2.30159594752158,2.38018362026978,
2.50753564499175,2.58026582803546,2.72352856314932,2.80831445209385,2.89229737147604,
3.05890113029296,3.13853522888799,3.22570967551258,3.30970314422656,3.47395562175451,
3.55354130187497,3.69234485228637,3.77242982395912,3.83814226949863,3.88038829310432,
3.95516208872894,4.02096865651561,4.17915166056594,4.2564735047848,4.33558734702027),
 .UNSPECIFIED.);
#712=B_SPLINE_CURVE_WITH_KNOTS('',3,(#65363,#65364,#65365,#65366,#65367,
#65368,#65369,#65370,#65371,#65372,#65373,#65374,#65375,#65376,#65377,#65378,
#65379,#65380,#65381,#65382,#65383,#65384,#65385,#65386,#65387,#65388,#65389,
#65390,#65391,#65392,#65393,#65394,#65395,#65396,#65397,#65398,#65399,#65400,
#65401,#65402,#65403,#65404,#65405,#65406,#65407,#65408,#65409,#65410,#65411,
#65412,#65413,#65414,#65415,#65416,#65417,#65418,#65419,#65420,#65421,#65422,
#65423,#65424,#65425,#65426,#65427,#65428,#65429,#65430,#65431,#65432,#65433,
#65434,#65435,#65436,#65437,#65438,#65439,#65440,#65441,#65442,#65443,#65444,
#65445,#65446,#65447,#65448,#65449,#65450,#65451,#65452,#65453,#65454,#65455,
#65456,#65457,#65458,#65459,#65460,#65461,#65462,#65463,#65464,#65465,#65466,
#65467,#65468,#65469,#65470,#65471,#65472,#65473,#65474,#65475,#65476,#65477,
#65478,#65479,#65480,#65481,#65482,#65483,#65484,#65485,#65486,#65487,#65488,
#65489,#65490,#65491,#65492,#65493,#65494,#65495,#65496,#65497,#65498,#65499,
#65500,#65501,#65502,#65503,#65504,#65505,#65506,#65507,#65508,#65509,#65510,
#65511,#65512,#65513,#65514,#65515,#65516,#65517,#65518,#65519,#65520,#65521,
#65522,#65523,#65524,#65525,#65526,#65527,#65528,#65529,#65530,#65531,#65532,
#65533,#65534,#65535,#65536,#65537,#65538,#65539,#65540,#65541,#65542,#65543,
#65544,#65545,#65546,#65547,#65548,#65549,#65550,#65551,#65552,#65553,#65554,
#65555,#65556,#65557,#65558,#65559,#65560,#65561,#65562,#65563,#65564,#65565,
#65566,#65567,#65568,#65569,#65570,#65571,#65572,#65573),.UNSPECIFIED.,
 .F.,.F.,(4,3,3,3,3,3,3,3,3,3,3,3,3,3,3,3,3,3,3,3,3,3,3,3,3,3,3,3,3,3,3,
3,3,3,3,3,3,3,3,3,3,3,3,3,3,3,3,3,3,3,3,3,3,3,3,3,3,3,3,3,3,3,3,3,3,3,3,
3,3,3,4),(7.94826257243732,8.03933927732266,8.13040900661477,8.22150087575582,
8.28490746193705,8.37600661966196,8.46708750385086,8.55817107950977,8.64925032934137,
8.7403486849684,8.77225495969805,8.86358446014535,8.95489727790249,9.04621272797726,
9.13752315628156,9.22884970421161,9.25960245745905,9.35004563389331,9.44046838421938,
9.53089683726842,9.62132426183796,9.71178086513476,9.74694995522005,9.83977082466953,
9.93258020493847,10.0253815422507,10.1181658427925,10.2109349487687,10.2342974529811,
10.3226340982603,10.4109484628818,10.4992807310775,10.5876214045936,10.6760195929041,
10.7216449507421,10.8172935625052,10.9152182840046,11.0107916985716,11.1098920735374,
11.2089924485031,11.2974475293379,11.3858999834853,11.4743988429813,11.5629222999095,
11.6515265886469,11.6963399462641,11.7845988436236,11.8727845281299,11.96091671564,
12.0496814939083,12.1377836965724,12.2258943659517,12.3140313137176,12.4032822207347,
12.4915724815489,12.5813037116675,12.6710349417861,12.7563666072233,12.8415825207838,
12.9267064287632,13.0117619568872,13.0967819333776,13.1817864079043,13.2667966276969,
13.3518338433476,13.4369714570383,13.5221663247904,13.6074971372277,13.6457299373081,
13.7757706988632,13.8747245557601),.UNSPECIFIED.);
#713=B_SPLINE_CURVE_WITH_KNOTS('',3,(#65574,#65575,#65576,#65577,#65578,
#65579,#65580,#65581,#65582,#65583,#65584,#65585,#65586,#65587,#65588,#65589),
 .UNSPECIFIED.,.F.,.F.,(4,3,3,3,3,4),(13.8747245559393,13.964019218205,
14.0502847363995,14.1364982676294,14.222679165221,14.2319032050023),
 .UNSPECIFIED.);
#714=B_SPLINE_CURVE_WITH_KNOTS('',3,(#65595,#65596,#65597,#65598,#65599,
#65600),.UNSPECIFIED.,.F.,.F.,(4,2,4),(-0.153225104208862,-0.0777958673852031,
-0.000838790028883987),.UNSPECIFIED.);
#715=B_SPLINE_CURVE_WITH_KNOTS('',3,(#65601,#65602,#65603,#65604,#65605,
#65606,#65607,#65608,#65609,#65610,#65611,#65612,#65613,#65614,#65615,#65616,
#65617,#65618,#65619,#65620,#65621,#65622,#65623,#65624,#65625,#65626,#65627,
#65628,#65629,#65630,#65631,#65632,#65633,#65634,#65635,#65636,#65637,#65638,
#65639,#65640,#65641,#65642,#65643,#65644,#65645,#65646,#65647,#65648,#65649,
#65650,#65651,#65652,#65653,#65654,#65655,#65656,#65657,#65658,#65659,#65660,
#65661,#65662,#65663,#65664,#65665,#65666,#65667,#65668,#65669,#65670,#65671,
#65672,#65673,#65674,#65675,#65676,#65677,#65678,#65679,#65680,#65681,#65682,
#65683,#65684,#65685,#65686,#65687,#65688,#65689,#65690,#65691,#65692,#65693,
#65694,#65695,#65696,#65697,#65698,#65699,#65700,#65701,#65702,#65703,#65704,
#65705,#65706,#65707,#65708,#65709,#65710,#65711,#65712,#65713,#65714,#65715,
#65716,#65717,#65718,#65719,#65720,#65721,#65722,#65723,#65724,#65725,#65726,
#65727,#65728,#65729,#65730,#65731,#65732,#65733,#65734,#65735,#65736,#65737,
#65738,#65739,#65740,#65741,#65742,#65743,#65744,#65745,#65746,#65747,#65748,
#65749,#65750,#65751,#65752,#65753,#65754,#65755,#65756,#65757,#65758,#65759,
#65760,#65761,#65762,#65763,#65764,#65765,#65766,#65767,#65768,#65769,#65770,
#65771,#65772,#65773,#65774,#65775,#65776,#65777,#65778,#65779,#65780,#65781,
#65782,#65783,#65784,#65785,#65786,#65787,#65788,#65789,#65790,#65791,#65792,
#65793,#65794,#65795,#65796,#65797,#65798,#65799,#65800,#65801,#65802,#65803,
#65804,#65805,#65806,#65807,#65808),.UNSPECIFIED.,.F.,.F.,(4,3,3,3,3,3,
3,3,3,3,3,3,3,3,3,3,3,3,3,3,3,3,3,3,3,3,3,3,3,3,3,3,3,3,3,3,3,3,3,3,3,3,
3,3,3,3,3,3,3,3,3,3,3,3,3,3,3,3,3,3,3,3,3,3,3,3,3,3,3,4),(-16.4213910178811,
-16.3286432460334,-16.2359126775523,-16.1431937736906,-16.0824674261131,
-15.9941326347525,-15.9058201280992,-15.81748971347,-15.7291508902718,-15.6407545361228,
-15.5951199283521,-15.4994686331016,-15.401544582474,-15.3059685045778,
-15.2068704675844,-15.1077724305911,-15.0193184286812,-14.9308670580831,
-14.8423692825813,-14.7538469094734,-14.6652436972666,-14.6204249328301,
-14.5321659959703,-14.4439802741915,-14.3558480516816,-14.2670832873849,
-14.1789810556079,-14.0908703594027,-14.0027333871464,-13.9134825246869,
-13.8251922454331,-13.7354610913706,-13.6457299373081,-13.5603980691463,
-13.4751819518284,-13.3900578392207,-13.3050021057494,-13.2199819233987,
-13.134977242644,-13.0499668163815,-12.9649293941461,-12.8797915746879,
-12.7945965012499,-12.7092654850702,-12.6710349417861,-12.5825725222911,
-12.4942230261398,-12.405966583943,-12.3172632542332,-12.2291343186378,
-12.1410336270666,-12.0529433623445,-11.9637925083244,-11.8756388741685,
-11.7859894102163,-11.6963399462641,-11.6077342332092,-11.5191955002859,
-11.4307068279097,-11.342248612659,-11.2537923358304,-11.2089924485031,
-11.1135915257343,-11.0156048819863,-10.9199968256523,-10.8208208881972,
-10.7216449507421,-10.6332463945045,-10.5448975523916,-10.494778244858),
 .UNSPECIFIED.);
#716=B_SPLINE_CURVE_WITH_KNOTS('',3,(#65810,#65811,#65812,#65813,#65814,
#65815,#65816,#65817,#65818,#65819,#65820,#65821,#65822,#65823,#65824,#65825,
#65826,#65827,#65828,#65829,#65830,#65831,#65832,#65833,#65834,#65835,#65836,
#65837,#65838,#65839,#65840,#65841,#65842,#65843,#65844,#65845,#65846,#65847,
#65848,#65849,#65850,#65851,#65852,#65853,#65854,#65855,#65856,#65857,#65858,
#65859,#65860,#65861,#65862,#65863,#65864,#65865,#65866,#65867,#65868,#65869,
#65870,#65871,#65872,#65873,#65874,#65875,#65876,#65877,#65878,#65879,#65880,
#65881,#65882,#65883,#65884,#65885,#65886,#65887,#65888,#65889,#65890,#65891,
#65892,#65893,#65894,#65895,#65896,#65897,#65898,#65899,#65900,#65901,#65902,
#65903,#65904,#65905,#65906,#65907,#65908,#65909,#65910,#65911,#65912,#65913,
#65914,#65915,#65916,#65917,#65918,#65919,#65920,#65921,#65922,#65923,#65924,
#65925,#65926,#65927,#65928,#65929,#65930,#65931,#65932,#65933,#65934,#65935,
#65936,#65937,#65938,#65939,#65940,#65941,#65942,#65943,#65944,#65945,#65946,
#65947,#65948,#65949,#65950,#65951,#65952,#65953,#65954,#65955,#65956,#65957,
#65958,#65959,#65960,#65961,#65962,#65963,#65964,#65965,#65966,#65967,#65968,
#65969,#65970,#65971,#65972,#65973,#65974,#65975,#65976,#65977,#65978,#65979,
#65980,#65981,#65982,#65983,#65984,#65985,#65986,#65987,#65988,#65989,#65990,
#65991,#65992,#65993,#65994,#65995,#65996,#65997,#65998,#65999,#66000,#66001,
#66002,#66003,#66004,#66005,#66006,#66007,#66008,#66009,#66010,#66011,#66012,
#66013,#66014,#66015,#66016,#66017,#66018,#66019,#66020,#66021,#66022,#66023,
#66024,#66025,#66026),.UNSPECIFIED.,.F.,.F.,(4,3,3,3,3,3,3,3,3,3,3,3,3,
3,3,3,3,3,3,3,3,3,3,3,3,3,3,3,3,3,3,3,3,3,3,3,3,3,3,3,3,3,3,3,3,3,3,3,3,
3,3,3,3,3,3,3,3,3,3,3,3,3,3,3,3,3,3,3,3,3,3,3,4),(14.2319032050023,14.3180783398705,
14.4043013520915,14.4905508815598,14.5768909610204,14.6204249328301,14.7090317212767,
14.7975715349282,14.8860612901713,14.9745205887241,15.0629779437081,15.1077724305911,
15.2031708278285,15.3011581029594,15.3967634736636,15.4959417010079,15.5951199283521,
15.6835192874087,15.7718698144088,15.8601984027851,15.9485126799093,16.0368502402501,
16.0824674261131,16.1752378011632,16.2680191188897,16.3608252586661,16.4536335932026,
16.5464539861204,16.5698149238741,16.6602714687669,16.7507017943729,16.8411292346796,
16.9315506889061,17.0219940616611,17.0571624216351,17.1484889520193,17.2398000990734,
17.3311157956058,17.422427582782,17.5137570989986,17.5445099193961,17.6356082056985,
17.7266885987632,17.8177722450881,17.908851891124,17.9999511154388,18.0318574171571,
18.1229465647275,18.2140172401526,18.3050904133561,18.3961591751174,18.4872470013927,
18.5192049149181,18.6103536567512,18.7014849737903,18.792619714476,18.8837504128207,
18.9749001970642,19.0065524126791,19.0976529191154,19.1887352474846,19.2798203891772,
19.3709012703821,19.4620013365704,19.4938999104401,19.5850275018026,19.6761373102866,
19.7672502347794,19.8583589984622,19.9494868590967,19.9812474082011,20.0749895405449,
20.1579098627142),.UNSPECIFIED.);
#717=B_SPLINE_CURVE_WITH_KNOTS('',3,(#66027,#66028,#66029,#66030,#66031,
#66032,#66033,#66034,#66035,#66036,#66037,#66038,#66039,#66040,#66041,#66042),
 .UNSPECIFIED.,.F.,.F.,(4,3,3,3,3,4),(20.1579098629397,20.2491418453206,
20.3403708768365,20.4316208898443,20.4685949059621,20.5146317045532),
 .UNSPECIFIED.);
#718=B_SPLINE_CURVE_WITH_KNOTS('',3,(#66049,#66050,#66051,#66052,#66053,
#66054,#66055,#66056,#66057,#66058,#66059,#66060,#66061,#66062),
 .UNSPECIFIED.,.F.,.F.,(4,2,2,2,2,2,4),(-3.36831712780366,-3.29736812950927,
-3.2281135588852,-3.10483059742013,-3.02255231766649,-2.85213247050082,
-2.84070125419267),.UNSPECIFIED.);
#719=B_SPLINE_CURVE_WITH_KNOTS('',3,(#66069,#66070,#66071,#66072,#66073,
#66074,#66075,#66076,#66077,#66078,#66079,#66080,#66081,#66082),
 .UNSPECIFIED.,.F.,.F.,(4,2,2,2,2,2,4),(-3.36831719559857,-3.29736749922203,
-3.22811229767945,-3.10483036543586,-3.02255213049028,-2.85213226983663,
-2.84070132266613),.UNSPECIFIED.);
#720=B_SPLINE_CURVE_WITH_KNOTS('',3,(#66088,#66089,#66090,#66091,#66092,
#66093,#66094,#66095,#66096,#66097,#66098,#66099,#66100,#66101,#66102,#66103,
#66104,#66105,#66106,#66107,#66108,#66109,#66110,#66111,#66112,#66113,#66114,
#66115,#66116,#66117,#66118,#66119,#66120,#66121,#66122,#66123,#66124,#66125,
#66126,#66127,#66128,#66129,#66130,#66131,#66132,#66133,#66134,#66135,#66136,
#66137,#66138,#66139,#66140,#66141,#66142,#66143,#66144,#66145,#66146,#66147,
#66148,#66149,#66150,#66151,#66152,#66153,#66154,#66155,#66156,#66157,#66158,
#66159,#66160,#66161,#66162,#66163,#66164,#66165,#66166,#66167,#66168,#66169,
#66170,#66171,#66172,#66173,#66174,#66175,#66176,#66177,#66178,#66179,#66180,
#66181,#66182,#66183,#66184,#66185,#66186,#66187,#66188,#66189,#66190,#66191,
#66192,#66193,#66194,#66195,#66196,#66197,#66198,#66199,#66200,#66201,#66202,
#66203,#66204,#66205,#66206,#66207,#66208,#66209,#66210,#66211,#66212,#66213,
#66214,#66215,#66216,#66217,#66218,#66219,#66220,#66221,#66222,#66223,#66224,
#66225,#66226,#66227,#66228,#66229,#66230,#66231,#66232,#66233,#66234,#66235,
#66236,#66237,#66238,#66239,#66240,#66241,#66242,#66243,#66244,#66245,#66246,
#66247,#66248,#66249,#66250,#66251,#66252,#66253,#66254,#66255,#66256,#66257,
#66258,#66259,#66260,#66261,#66262,#66263,#66264,#66265,#66266,#66267,#66268,
#66269,#66270,#66271,#66272,#66273,#66274,#66275,#66276,#66277,#66278,#66279,
#66280,#66281,#66282,#66283,#66284,#66285,#66286,#66287,#66288,#66289,#66290,
#66291,#66292,#66293,#66294,#66295,#66296,#66297,#66298,#66299,#66300,#66301),
 .UNSPECIFIED.,.F.,.F.,(4,3,3,3,3,3,3,3,3,3,3,3,3,3,3,3,3,3,3,3,3,3,3,3,
3,3,3,3,3,3,3,3,3,3,3,3,3,3,3,3,3,3,3,3,3,3,3,3,3,3,3,3,3,3,3,3,3,3,3,3,
3,3,3,3,3,3,3,3,3,3,3,4),(20.5146317059255,20.6057411556705,20.6968512036646,
20.787952699175,20.8790768172452,20.9559424037231,21.0470612884176,21.1381622711603,
21.2292662844587,21.3203661118309,21.4114850745217,21.4432899014841,21.5344090077396,
21.6255102062777,21.7166144247242,21.8077144504978,21.8988336000398,21.9306373992451,
22.0217552919853,22.1128552791001,22.2039583013779,22.2950571431046,22.3861751362555,
22.4179848970061,22.509105908084,22.6002090175663,22.6913151367396,22.7824170521249,
22.8735380592111,22.9053323947671,22.9964483149354,23.0875463288368,23.1786473967051,
23.2697443002416,23.3608603950902,23.3926798925281,23.4838001230218,23.5749024336183,
23.6660077353362,23.7571088247932,23.8482290006467,23.8800273902891,23.9711543961236,
24.0622635601542,24.1533757600712,24.2444837545981,24.3356107871391,24.3673748880501,
24.4584574255276,24.5495218955094,24.6405895201973,24.7316531300112,24.8227364288934,
24.8547223858112,24.9459388473859,25.0371377774975,25.1283392870914,25.2195360775557,
25.3107504070892,25.3420698835721,25.4329781236218,25.5238682415749,25.6147631576547,
25.7056554643935,25.7965709429544,25.8294173813331,25.9210354533695,26.012634445065,
26.1042294234823,26.1958146217395,26.2874065688899,26.3167648790942),
 .UNSPECIFIED.);
#721=B_SPLINE_CURVE_WITH_KNOTS('',3,(#66303,#66304,#66305,#66306,#66307,
#66308,#66309,#66310,#66311,#66312,#66313,#66314,#66315,#66316,#66317,#66318,
#66319,#66320,#66321,#66322,#66323,#66324,#66325,#66326,#66327,#66328,#66329,
#66330,#66331,#66332,#66333,#66334,#66335,#66336,#66337,#66338,#66339,#66340,
#66341,#66342,#66343,#66344,#66345,#66346,#66347,#66348,#66349,#66350,#66351,
#66352,#66353,#66354,#66355,#66356),.UNSPECIFIED.,.F.,.F.,(4,2,2,2,2,2,
2,2,2,2,2,2,2,2,2,2,2,2,2,2,2,2,2,2,2,2,4),(-2.84070132266613,-2.78020515581023,
-2.65435156006841,-2.57658993540392,-2.49698956383074,-2.32946341040136,
-2.24549532116482,-2.17252610320999,-2.05532975785649,-1.97398058008043,
-1.85252492978697,-1.68460878885054,-1.51626217315707,-1.44268575556167,
-1.30223153656894,-1.22322211388899,-1.10079068218151,-1.03028045314551,
-0.859935588437529,-0.777911177383843,-0.65632125055536,-0.575111733431278,
-0.460088756394275,-0.393765504197562,-0.309841478073698,-0.154378575284087,
-0.153225086960603),.UNSPECIFIED.);
#722=B_SPLINE_CURVE_WITH_KNOTS('',3,(#66362,#66363,#66364,#66365,#66366,
#66367,#66368,#66369,#66370,#66371,#66372,#66373,#66374,#66375,#66376,#66377,
#66378,#66379,#66380,#66381,#66382,#66383,#66384,#66385,#66386,#66387,#66388,
#66389,#66390,#66391,#66392,#66393,#66394,#66395,#66396,#66397,#66398,#66399,
#66400,#66401,#66402,#66403,#66404,#66405,#66406,#66407,#66408,#66409,#66410,
#66411,#66412,#66413,#66414,#66415,#66416,#66417,#66418,#66419,#66420,#66421,
#66422,#66423,#66424,#66425,#66426,#66427,#66428,#66429,#66430,#66431,#66432,
#66433,#66434,#66435,#66436,#66437,#66438,#66439,#66440,#66441,#66442,#66443,
#66444,#66445,#66446,#66447,#66448,#66449,#66450,#66451,#66452,#66453,#66454,
#66455,#66456,#66457,#66458,#66459,#66460,#66461,#66462,#66463,#66464,#66465,
#66466,#66467,#66468,#66469,#66470,#66471,#66472,#66473,#66474,#66475,#66476,
#66477,#66478,#66479,#66480,#66481,#66482,#66483,#66484,#66485,#66486,#66487,
#66488,#66489,#66490,#66491,#66492,#66493,#66494,#66495,#66496,#66497,#66498,
#66499,#66500,#66501,#66502,#66503,#66504,#66505,#66506,#66507,#66508,#66509,
#66510,#66511,#66512,#66513,#66514,#66515,#66516,#66517,#66518,#66519,#66520,
#66521,#66522,#66523,#66524,#66525,#66526,#66527,#66528,#66529,#66530,#66531,
#66532,#66533,#66534,#66535,#66536,#66537,#66538,#66539,#66540,#66541,#66542,
#66543,#66544,#66545,#66546,#66547,#66548,#66549,#66550,#66551,#66552,#66553,
#66554,#66555,#66556,#66557,#66558,#66559,#66560,#66561,#66562,#66563,#66564,
#66565,#66566,#66567,#66568,#66569,#66570,#66571,#66572,#66573,#66574,#66575,
#66576,#66577,#66578),.UNSPECIFIED.,.F.,.F.,(4,3,3,3,3,3,3,3,3,3,3,3,3,
3,3,3,3,3,3,3,3,3,3,3,3,3,3,3,3,3,3,3,3,3,3,3,3,3,3,3,3,3,3,3,3,3,3,3,3,
3,3,3,3,3,3,3,3,3,3,3,3,3,3,3,3,3,3,3,3,3,3,3,4),(14.2319029117468,14.3180786703085,
14.4043023140868,14.4905524798541,14.5768932001375,14.6204249328301,14.709029072133,
14.7975662235017,14.8860533112043,14.9745099411476,15.0629646402058,15.1077724305911,
15.2031770525732,15.301162771518,15.3967747615889,15.4959473449705,15.5951199283521,
15.6835147693779,15.7718607477815,15.8601847664223,15.9484944641987,16.0368274563183,
16.0824674261131,16.1752416501605,16.2680268918029,16.3608370085562,16.4536493321215,
16.5464736883574,16.5698149238741,16.6602697202645,16.7506982784102,16.8411239387326,
16.9315436094234,17.02198520695,17.0571624216351,17.1484896189004,17.2398014408522,
17.3311178169076,17.4224302842788,17.513760475784,17.5445099193961,17.6356081111592,
17.7266884093325,17.8177719612098,17.9088515133148,17.9999506452483,18.0318574171571,
18.1229464656923,18.2140170402529,18.3050901109109,18.3961587694273,18.4872464922916,
18.5192049149181,18.6103537750563,18.7014852122315,18.7926200745213,18.8837508949863,
18.9749008010787,19.0065524126791,19.0976528378301,19.1887350837563,19.2798201421328,
19.370900939742,19.4620009226222,19.4938999104401,19.585027544216,19.6761373956887,
19.7672503635792,19.8583591707788,19.9494870747378,19.9812474082011,20.074989510816,
20.1579098627142),.UNSPECIFIED.);
#723=B_SPLINE_CURVE_WITH_KNOTS('',3,(#66579,#66580,#66581,#66582,#66583,
#66584,#66585,#66586,#66587,#66588,#66589,#66590,#66591,#66592,#66593,#66594),
 .UNSPECIFIED.,.F.,.F.,(4,3,3,3,3,4),(20.1579098629397,20.2491418336797,
20.3403708535511,20.4316208550079,20.4685949059621,20.5146317059255),
 .UNSPECIFIED.);
#724=B_SPLINE_CURVE_WITH_KNOTS('',3,(#66596,#66597,#66598,#66599,#66600,
#66601),.UNSPECIFIED.,.F.,.F.,(4,2,4),(-0.153225086960603,-0.0778068263849535,
-0.000838734811037899),.UNSPECIFIED.);
#725=B_SPLINE_CURVE_WITH_KNOTS('',3,(#66602,#66603,#66604,#66605,#66606,
#66607,#66608,#66609,#66610,#66611,#66612,#66613,#66614,#66615,#66616,#66617,
#66618,#66619,#66620,#66621,#66622,#66623,#66624,#66625,#66626,#66627,#66628,
#66629,#66630,#66631,#66632,#66633,#66634,#66635,#66636,#66637,#66638,#66639,
#66640,#66641,#66642,#66643,#66644,#66645,#66646,#66647,#66648,#66649,#66650,
#66651,#66652,#66653,#66654,#66655,#66656,#66657,#66658,#66659,#66660,#66661,
#66662,#66663,#66664,#66665,#66666,#66667,#66668,#66669,#66670,#66671,#66672,
#66673,#66674,#66675,#66676,#66677,#66678,#66679,#66680,#66681,#66682,#66683,
#66684,#66685,#66686,#66687,#66688,#66689,#66690,#66691,#66692,#66693,#66694,
#66695,#66696,#66697,#66698,#66699,#66700,#66701,#66702,#66703,#66704,#66705,
#66706,#66707,#66708,#66709,#66710,#66711,#66712,#66713,#66714,#66715,#66716,
#66717,#66718,#66719,#66720,#66721,#66722,#66723,#66724,#66725,#66726,#66727,
#66728,#66729,#66730,#66731,#66732,#66733,#66734,#66735,#66736,#66737,#66738,
#66739,#66740,#66741,#66742,#66743,#66744,#66745,#66746,#66747,#66748,#66749,
#66750,#66751,#66752,#66753,#66754,#66755,#66756,#66757,#66758,#66759,#66760,
#66761,#66762,#66763,#66764,#66765,#66766,#66767,#66768,#66769,#66770,#66771,
#66772,#66773,#66774,#66775,#66776,#66777,#66778,#66779,#66780,#66781,#66782,
#66783,#66784,#66785,#66786,#66787,#66788,#66789,#66790,#66791,#66792,#66793,
#66794,#66795,#66796,#66797,#66798,#66799,#66800,#66801,#66802,#66803,#66804,
#66805,#66806,#66807,#66808,#66809),.UNSPECIFIED.,.F.,.F.,(4,3,3,3,3,3,
3,3,3,3,3,3,3,3,3,3,3,3,3,3,3,3,3,3,3,3,3,3,3,3,3,3,3,3,3,3,3,3,3,3,3,3,
3,3,3,3,3,3,3,3,3,3,3,3,3,3,3,3,3,3,3,3,3,3,3,3,3,3,3,4),(-16.4213910178811,
-16.3286400772641,-16.2359063591921,-16.1431843748859,-16.0824674261131,
-15.9941362568266,-15.9058273801709,-15.8175005869686,-15.7291653788733,
-15.6407726083022,-15.5951199283521,-15.4994633914501,-15.4015406512354,
-15.3059593709262,-15.2068659007586,-15.1077724305911,-15.0193205338912,
-14.9308712775328,-14.84237561715,-14.7538553588308,-14.6652542472042,-14.6204249328301,
-14.5321659202474,-14.4439801271102,-14.3558478376921,-14.2670831001441,
-14.1789808129682,-14.0908700658319,-14.0027330472036,-13.9134822697297,
-13.8251919559008,-13.7354609466044,-13.6457299373081,-13.5603976716426,
-13.4751811547976,-13.390056640956,-13.3050005048409,-13.2199799188415,
-13.1349748337167,-13.0499640026098,-12.9649261753039,-12.8797879523774,
-12.7945924756304,-12.7092610599517,-12.6710349417861,-12.5825724970548,
-12.4942229702032,-12.4059664919653,-12.3172631737526,-12.2291341894402,
-12.1410334445326,-12.0529431219476,-11.9637923280267,-11.8756386254687,
-11.7859892858664,-11.6963399462641,-11.6077363315675,-11.5191997074042,
-11.430713147944,-11.3422570464542,-11.253802873335,-11.2089924485031,-11.1135865925285,
-11.0156011820819,-10.9199878797788,-10.8208164152605,-10.7216449507421,
-10.6332499745261,-10.5449047398611,-10.49477808198),.UNSPECIFIED.);
#726=B_SPLINE_CURVE_WITH_KNOTS('',3,(#66815,#66816,#66817,#66818,#66819,
#66820,#66821,#66822,#66823,#66824,#66825,#66826,#66827,#66828,#66829,#66830,
#66831,#66832,#66833,#66834,#66835,#66836,#66837,#66838,#66839,#66840,#66841,
#66842,#66843,#66844,#66845,#66846,#66847,#66848,#66849,#66850,#66851,#66852),
 .UNSPECIFIED.,.F.,.F.,(4,2,2,2,2,2,2,2,2,2,2,2,2,2,2,2,2,2,4),(2.08228018305572E-5,
0.134148024868073,0.202716477712664,0.327559837231032,0.405484389532305,
0.485128229324024,0.652510410323932,0.736487383617962,0.809797659300728,
0.977479155573237,1.04684058460045,1.11942531708603,1.23168220985833,1.31165597792338,
1.44944632348465,1.58444765771081,1.65977704604661,1.79047000383681,1.80129261558726),
 .UNSPECIFIED.);
#727=B_SPLINE_CURVE_WITH_KNOTS('',3,(#66856,#66857,#66858,#66859,#66860,
#66861,#66862,#66863,#66864,#66865,#66866,#66867,#66868,#66869,#66870),
 .UNSPECIFIED.,.F.,.F.,(4,1,1,1,1,1,1,1,1,1,1,1,4),(2.0217817672715,2.43673748880501,
2.92408498656602,3.41143248432702,3.89877998208802,4.38612747984903,4.87347497761003,
5.36082247537103,5.84816997313203,6.33551747089303,6.82286496865404,7.31021246641504,
7.59153924858053),.UNSPECIFIED.);
#728=B_SPLINE_CURVE_WITH_KNOTS('',3,(#66871,#66872,#66873,#66874,#66875,
#66876,#66877,#66878,#66879,#66880,#66881,#66882,#66883,#66884,#66885,#66886),
 .UNSPECIFIED.,.F.,.F.,(4,3,3,3,3,4),(7.59153924858053,7.68452254538593,
7.77753312315858,7.79755996417604,7.88865003464089,7.94826257357117),
 .UNSPECIFIED.);
#729=B_SPLINE_CURVE_WITH_KNOTS('',3,(#66892,#66893,#66894,#66895,#66896,
#66897,#66898,#66899,#66900,#66901,#66902,#66903,#66904,#66905,#66906,#66907,
#66908,#66909,#66910,#66911,#66912,#66913,#66914,#66915,#66916,#66917),
 .UNSPECIFIED.,.F.,.F.,(4,2,2,2,2,2,2,2,2,2,2,2,4),(-0.0747573509028117,
-0.0739383148717887,-0.0616383873536828,-0.0559544033060534,-0.0377854288912249,
-0.0350633930401213,-0.0337175069903932,-0.0326484285706749,-0.0316335607138953,
-0.0303960629492908,-0.0285520710439741,-0.0215326227016456,-0.000655565290617223),
 .UNSPECIFIED.);
#730=B_SPLINE_CURVE_WITH_KNOTS('',3,(#66919,#66920,#66921,#66922,#66923,
#66924,#66925,#66926,#66927,#66928,#66929,#66930,#66931,#66932,#66933,#66934,
#66935,#66936,#66937,#66938,#66939,#66940,#66941,#66942,#66943,#66944,#66945,
#66946,#66947,#66948,#66949,#66950,#66951,#66952,#66953,#66954,#66955,#66956,
#66957,#66958,#66959,#66960,#66961,#66962,#66963,#66964,#66965,#66966,#66967,
#66968,#66969,#66970,#66971,#66972,#66973,#66974,#66975,#66976,#66977,#66978,
#66979,#66980,#66981,#66982,#66983,#66984,#66985,#66986,#66987,#66988,#66989,
#66990,#66991,#66992,#66993,#66994,#66995,#66996,#66997,#66998,#66999,#67000,
#67001,#67002,#67003,#67004,#67005,#67006,#67007,#67008,#67009,#67010,#67011,
#67012,#67013,#67014,#67015,#67016,#67017,#67018,#67019,#67020,#67021,#67022,
#67023,#67024,#67025,#67026,#67027,#67028,#67029,#67030,#67031,#67032,#67033,
#67034,#67035,#67036),.UNSPECIFIED.,.F.,.F.,(4,3,3,3,3,3,3,3,3,3,3,3,3,
3,3,3,3,3,3,3,3,3,3,3,3,3,3,3,3,3,3,3,3,3,3,3,3,3,3,4),(170.955339710339,
171.060905920727,171.162663401337,171.264353092419,171.366010725341,171.467671982924,
171.569433774829,171.671256091623,171.77323959999,171.799869393442,171.903390623982,
172.006760853885,172.110012748576,172.2132010018,172.316359435341,172.419521829469,
172.522792194405,172.626119678124,172.729629765827,172.798705843404,172.90100919765,
173.00315849853,173.10519039517,173.207159585109,173.309101433958,173.411051266852,
173.513123449993,173.615258630591,173.71759950971,173.797542293366,173.903815983742,
174.01538632869,174.121306695383,174.227127466107,174.332876381024,174.438581090584,
174.544298932523,174.650021856933,174.755817740451,174.796378743328),
 .UNSPECIFIED.);
#731=B_SPLINE_CURVE_WITH_KNOTS('',3,(#67040,#67041,#67042,#67043,#67044,
#67045,#67046,#67047,#67048,#67049,#67050,#67051,#67052,#67053,#67054,#67055,
#67056,#67057,#67058,#67059,#67060,#67061,#67062,#67063,#67064,#67065,#67066,
#67067,#67068,#67069,#67070,#67071,#67072,#67073,#67074,#67075,#67076,#67077,
#67078,#67079,#67080,#67081,#67082,#67083,#67084,#67085,#67086,#67087,#67088,
#67089,#67090,#67091,#67092,#67093,#67094,#67095,#67096,#67097,#67098,#67099,
#67100,#67101,#67102,#67103,#67104,#67105,#67106,#67107,#67108,#67109,#67110,
#67111,#67112,#67113,#67114,#67115,#67116,#67117,#67118,#67119,#67120,#67121,
#67122,#67123,#67124,#67125,#67126,#67127,#67128,#67129,#67130,#67131,#67132,
#67133,#67134,#67135,#67136,#67137,#67138,#67139,#67140,#67141,#67142,#67143,
#67144,#67145,#67146,#67147,#67148,#67149,#67150,#67151,#67152,#67153,#67154,
#67155,#67156,#67157,#67158,#67159,#67160,#67161,#67162,#67163,#67164,#67165,
#67166,#67167,#67168,#67169,#67170,#67171,#67172,#67173,#67174,#67175,#67176,
#67177,#67178,#67179,#67180,#67181,#67182,#67183,#67184,#67185,#67186,#67187,
#67188,#67189,#67190,#67191,#67192,#67193,#67194,#67195,#67196,#67197,#67198,
#67199,#67200,#67201,#67202,#67203,#67204,#67205,#67206,#67207,#67208),
 .UNSPECIFIED.,.F.,.F.,(4,3,3,3,3,3,3,3,3,3,3,3,3,3,3,3,3,3,3,3,3,3,3,3,
3,3,3,3,3,3,3,3,3,3,3,3,3,3,3,3,3,3,3,3,3,3,3,3,3,3,3,3,3,3,3,3,4),(-172.787594226351,
-172.684274645609,-172.581108473843,-172.478063715916,-172.375084159336,
-172.272135658752,-172.169184111836,-172.066127763492,-171.963014418944,
-171.859724811317,-171.799869393442,-171.696296400939,-171.592873101958,
-171.489566394852,-171.386322278747,-171.283106998388,-171.179886839023,
-171.076557646842,-170.973170650988,-170.869600563122,-170.801032943481,
-170.69777070211,-170.594663824546,-170.491680473781,-170.388763813606,
-170.285879610087,-170.182993673711,-170.080001243854,-169.976952951891,
-169.873720941887,-169.802196493519,-169.698775124036,-169.595507109046,
-169.492360393262,-169.389279078215,-169.286229166357,-169.183176703332,
-169.080017631391,-168.976802370632,-168.873404720303,-168.803360043557,
-168.699944496997,-168.596681938659,-168.493540101833,-168.39046330706,
-168.287417549124,-168.184368865631,-168.081212965654,-167.978000541589,
-167.874605151471,-167.804523593595,-167.699671773339,-167.594987964963,
-167.490464903685,-167.386036670661,-167.281667151101,-167.203857020092),
 .UNSPECIFIED.);
#732=B_SPLINE_CURVE_WITH_KNOTS('',3,(#67209,#67210,#67211,#67212,#67213,
#67214,#67215,#67216),.UNSPECIFIED.,.F.,.F.,(4,2,2,4),(-2.66727759453781,
-2.64513467794962,-2.59594303077105,-2.59308707914317),.UNSPECIFIED.);
#733=B_SPLINE_CURVE_WITH_KNOTS('',3,(#67221,#67222,#67223,#67224,#67225,
#67226,#67227,#67228,#67229,#67230,#67231,#67232,#67233,#67234,#67235,#67236,
#67237,#67238,#67239,#67240,#67241,#67242,#67243,#67244,#67245,#67246,#67247,
#67248,#67249,#67250,#67251,#67252,#67253,#67254,#67255,#67256,#67257,#67258,
#67259,#67260,#67261,#67262,#67263,#67264,#67265,#67266,#67267,#67268,#67269,
#67270,#67271,#67272,#67273,#67274,#67275,#67276,#67277,#67278,#67279,#67280,
#67281,#67282,#67283,#67284,#67285,#67286,#67287,#67288,#67289,#67290,#67291,
#67292,#67293,#67294,#67295,#67296,#67297,#67298,#67299,#67300,#67301,#67302,
#67303,#67304,#67305,#67306,#67307,#67308,#67309,#67310,#67311,#67312,#67313,
#67314,#67315,#67316,#67317,#67318,#67319,#67320,#67321,#67322,#67323,#67324,
#67325,#67326,#67327,#67328,#67329,#67330,#67331,#67332,#67333,#67334,#67335,
#67336,#67337,#67338,#67339,#67340,#67341,#67342,#67343,#67344,#67345,#67346,
#67347,#67348,#67349,#67350,#67351,#67352,#67353,#67354,#67355,#67356,#67357,
#67358,#67359,#67360,#67361,#67362,#67363,#67364,#67365,#67366,#67367,#67368,
#67369,#67370,#67371,#67372,#67373,#67374,#67375,#67376,#67377,#67378,#67379,
#67380,#67381,#67382,#67383,#67384,#67385,#67386,#67387,#67388,#67389,#67390,
#67391,#67392,#67393,#67394,#67395,#67396,#67397,#67398,#67399,#67400,#67401,
#67402,#67403,#67404,#67405,#67406,#67407,#67408,#67409,#67410,#67411,#67412,
#67413,#67414,#67415,#67416,#67417,#67418,#67419,#67420,#67421,#67422,#67423,
#67424,#67425,#67426,#67427,#67428,#67429,#67430,#67431,#67432,#67433,#67434,
#67435,#67436,#67437,#67438,#67439,#67440,#67441,#67442,#67443,#67444,#67445,
#67446),.UNSPECIFIED.,.F.,.F.,(4,2,2,2,2,2,2,2,2,2,2,2,2,2,2,2,2,2,2,2,
2,2,2,2,2,2,2,2,2,2,2,2,2,2,2,2,2,2,2,2,2,2,2,2,2,2,2,2,2,2,2,2,2,2,2,2,
2,2,2,2,2,2,2,2,2,2,2,2,2,2,2,2,2,2,2,2,2,2,2,2,2,2,2,2,2,2,2,2,2,2,2,2,
2,2,2,2,2,2,2,2,2,2,2,2,2,2,2,2,2,2,2,2,4),(-1.40817977626643,-1.40705404837906,
-1.40292854648138,-1.3757426548093,-1.3337320464292,-1.32763512392359,-1.30978754890451,
-1.30709916425526,-1.30573723566938,-1.30466495450943,-1.30341928540201,
-1.30119586266891,-1.29070305773952,-1.26784056942761,-1.21011170611799,
-1.20367843769144,-1.20117007693688,-1.19935221924447,-1.19740892849055,
-1.19480672238284,-1.1889830009617,-1.16514966199108,-1.11614970333744,
-1.09779132445287,-1.09505198420995,-1.09369779480841,-1.09262569366162,
-1.09137327576406,-1.08912117532948,-1.07817666003123,-1.05366046115555,
-0.998557418932194,-0.991850218090042,-0.98929760171817,-0.987467733874629,
-0.98553005735288,-0.982966800167927,-0.977359065828194,-0.92907584220918,
-0.888723738506282,-0.884011345098199,-0.882271365568769,-0.881246080095021,
-0.880154646224944,-0.878645357309653,-0.875062863423288,-0.870037787607825,
-0.856214116460312,-0.83386094240738,-0.787184939428978,-0.779989395426667,
-0.777074388953639,-0.775273873406327,-0.773322052655055,-0.770660422919828,
-0.764492409594996,-0.737950196320098,-0.698622945036696,-0.687289264474059,
-0.673503769726914,-0.671211303564944,-0.669826550081623,-0.668750098233928,
-0.667534982181281,-0.665449708224016,-0.656908941372315,-0.64035066459171,
-0.598278958259621,-0.571099348034574,-0.566971801379125,-0.564478971054942,
-0.562545228654309,-0.560449567398847,-0.557102065583082,-0.54590445943643,
-0.527329550124218,-0.484797482353254,-0.462028184514635,-0.459170491849498,
-0.457791868994825,-0.456715605017749,-0.455474595675706,-0.453286877187307,
-0.443433219831685,-0.394231943383457,-0.359839415981377,-0.355551723858008,
-0.353009728095418,-0.351065351000036,-0.348985053513911,-0.345718999305572,
-0.335297147001225,-0.318505182775914,-0.258883353406481,-0.249294266218978,
-0.247244927429815,-0.24591830870456,-0.244851270525529,-0.243841554781177,
-0.241869173859128,-0.234451256057864,-0.220918078416166,-0.19233797325591,
-0.147271569436308,-0.143024766803768,-0.140506708098782,-0.138580709949515,
-0.136520279126182,-0.133286131263482,-0.122977226377692,-0.106384758650064,
-0.0845186243735332,-0.0747573509028117),.UNSPECIFIED.);
#734=B_SPLINE_CURVE_WITH_KNOTS('',3,(#67447,#67448,#67449,#67450,#67451,
#67452,#67453,#67454,#67455,#67456,#67457,#67458,#67459,#67460,#67461,#67462,
#67463,#67464,#67465,#67466,#67467,#67468,#67469,#67470,#67471,#67472,#67473,
#67474,#67475,#67476,#67477,#67478,#67479,#67480,#67481,#67482,#67483,#67484,
#67485,#67486,#67487,#67488,#67489,#67490,#67491,#67492,#67493,#67494,#67495,
#67496,#67497,#67498,#67499,#67500,#67501,#67502,#67503,#67504,#67505,#67506,
#67507,#67508,#67509,#67510,#67511,#67512,#67513,#67514,#67515,#67516,#67517,
#67518,#67519,#67520,#67521,#67522,#67523,#67524,#67525,#67526,#67527,#67528,
#67529,#67530,#67531,#67532,#67533,#67534,#67535,#67536,#67537,#67538,#67539,
#67540,#67541,#67542,#67543,#67544,#67545,#67546,#67547,#67548,#67549,#67550,
#67551,#67552,#67553,#67554,#67555,#67556,#67557,#67558,#67559,#67560,#67561,
#67562,#67563,#67564,#67565,#67566,#67567,#67568,#67569,#67570,#67571,#67572,
#67573,#67574,#67575,#67576,#67577,#67578,#67579,#67580,#67581,#67582,#67583,
#67584,#67585,#67586,#67587,#67588,#67589,#67590,#67591,#67592,#67593,#67594,
#67595,#67596,#67597,#67598,#67599,#67600,#67601,#67602,#67603,#67604,#67605,
#67606,#67607,#67608,#67609,#67610,#67611,#67612,#67613,#67614,#67615,#67616,
#67617,#67618,#67619,#67620,#67621,#67622,#67623,#67624,#67625,#67626,#67627,
#67628,#67629,#67630,#67631,#67632,#67633,#67634,#67635,#67636,#67637,#67638,
#67639,#67640,#67641,#67642,#67643,#67644,#67645,#67646,#67647,#67648,#67649,
#67650,#67651,#67652,#67653,#67654,#67655,#67656,#67657,#67658,#67659,#67660,
#67661,#67662,#67663,#67664,#67665,#67666,#67667,#67668,#67669,#67670,#67671,
#67672,#67673,#67674,#67675,#67676,#67677,#67678,#67679,#67680,#67681,#67682,
#67683,#67684,#67685,#67686),.UNSPECIFIED.,.F.,.F.,(4,2,2,2,2,2,2,2,2,2,
2,2,2,2,2,2,2,2,2,2,2,2,2,2,2,2,2,2,2,2,2,2,2,2,2,2,2,2,2,2,2,2,2,2,2,2,
2,2,2,2,2,2,2,2,2,2,2,2,2,2,2,2,2,2,2,2,2,2,2,2,2,2,2,2,2,2,2,2,2,2,2,2,
2,2,2,2,2,2,2,2,2,2,2,2,2,2,2,2,2,2,2,2,2,2,2,2,2,2,2,2,2,2,2,2,2,2,2,2,
2,4),(-2.59308707914317,-2.58660339095032,-2.58445919195256,-2.58323177533603,
-2.58215751868089,-2.58077043530716,-2.57786397952892,-2.55018880910383,
-2.51342558454827,-2.49426240188725,-2.48668611853075,-2.48276630063086,
-2.47946214186469,-2.47740892179214,-2.47557482273063,-2.47314289880733,
-2.46930670208162,-2.44885991797817,-2.39982767402896,-2.38317168920143,
-2.37459660300356,-2.37250763718333,-2.37129113892439,-2.37021375841239,
-2.36882821887161,-2.36653549590919,-2.352776798318,-2.34956221923803,-2.30364431015071,
-2.27574252048464,-2.2694060026503,-2.26671390106241,-2.26475530302475,
-2.26295934469996,-2.26007554580225,-2.25307603892048,-2.20166204145705,
-2.17457501360255,-2.16297249090162,-2.1606835625134,-2.15942370522108,
-2.15835287954249,-2.15701016563937,-2.15441100969585,-2.13887685921022,
-2.13224538774638,-2.11843770774554,-2.08555660440661,-2.06900013269377,
-2.05869293340974,-2.05544501071139,-2.05337209491736,-2.0514317309228,
-2.04889087994364,-2.04459622664776,-2.00945889627829,-1.96051823719871,
-1.95080595205933,-1.94863405103307,-1.9473997476301,-1.94632596381445,
-1.94494745533952,-1.94208504331836,-1.9187250304066,-1.90642929072587,
-1.8735610181683,-1.85702171008859,-1.84672167402945,-1.84347406604569,
-1.8414008763816,-1.83945991991007,-1.83691780450014,-1.83261990550126,
-1.79727828371102,-1.7481056860041,-1.73878848869331,-1.73664401139367,
-1.73541553172288,-1.73434063280646,-1.73295243648934,-1.73004063366615,
-1.69799462154211,-1.66509896851337,-1.64627173589911,-1.63878733585992,
-1.6331650344244,-1.63059944363341,-1.62866178266993,-1.62683325088112,
-1.62428463486109,-1.61760105385288,-1.56220871125131,-1.53786714397332,
-1.52696845967853,-1.52471985742216,-1.52346857113848,-1.52239665890621,
-1.52104187455343,-1.51838773260031,-1.5015054258139,-1.48271832796275,
-1.44975300002144,-1.43310009018563,-1.42274853775617,-1.41949490171918,
-1.41742031456669,-1.41547977023576,-1.41294067605154,-1.40865344674532,
-1.36489353865936,-1.3338431236361,-1.31579288364011,-1.31309721063966,
-1.31173353935863,-1.31066089516692,-1.30941595854817,-1.30719660708235,
-1.29677323663359,-1.27415949578997,-1.25967545240964),.UNSPECIFIED.);
#735=B_SPLINE_CURVE_WITH_KNOTS('',3,(#67692,#67693,#67694,#67695),
 .UNSPECIFIED.,.F.,.F.,(4,4),(158.039785833466,158.388969095546),
 .UNSPECIFIED.);
#736=B_SPLINE_CURVE_WITH_KNOTS('',3,(#67696,#67697,#67698,#67699,#67700,
#67701,#67702,#67703,#67704,#67705,#67706,#67707,#67708,#67709,#67710,#67711,
#67712,#67713,#67714,#67715,#67716,#67717,#67718,#67719,#67720,#67721,#67722,
#67723,#67724,#67725,#67726,#67727,#67728,#67729,#67730,#67731,#67732,#67733,
#67734,#67735,#67736,#67737,#67738,#67739,#67740,#67741,#67742,#67743,#67744,
#67745,#67746,#67747,#67748,#67749,#67750,#67751,#67752,#67753,#67754,#67755,
#67756,#67757,#67758,#67759,#67760,#67761,#67762,#67763,#67764,#67765,#67766,
#67767,#67768,#67769,#67770,#67771,#67772,#67773,#67774,#67775,#67776,#67777,
#67778,#67779,#67780,#67781,#67782,#67783,#67784,#67785,#67786,#67787,#67788,
#67789,#67790,#67791,#67792,#67793,#67794,#67795,#67796,#67797,#67798,#67799,
#67800,#67801,#67802,#67803,#67804,#67805,#67806,#67807,#67808,#67809,#67810,
#67811,#67812,#67813,#67814,#67815,#67816,#67817,#67818,#67819,#67820,#67821,
#67822,#67823,#67824,#67825,#67826,#67827,#67828,#67829,#67830,#67831,#67832,
#67833,#67834,#67835,#67836,#67837,#67838,#67839,#67840,#67841,#67842,#67843,
#67844,#67845,#67846,#67847,#67848,#67849,#67850,#67851,#67852,#67853,#67854,
#67855,#67856,#67857,#67858,#67859,#67860,#67861,#67862,#67863,#67864,#67865,
#67866,#67867,#67868,#67869,#67870,#67871,#67872,#67873,#67874,#67875,#67876,
#67877,#67878,#67879,#67880,#67881,#67882,#67883,#67884,#67885,#67886,#67887,
#67888,#67889,#67890,#67891,#67892,#67893,#67894,#67895,#67896,#67897,#67898,
#67899,#67900,#67901,#67902,#67903,#67904,#67905),.UNSPECIFIED.,.F.,.F.,
(4,2,2,2,2,2,2,2,2,2,2,2,2,2,2,2,2,2,2,2,2,2,2,2,2,2,2,2,2,2,2,2,2,2,2,
2,2,2,2,2,2,2,2,2,2,2,2,2,2,2,2,2,2,2,2,2,2,2,2,2,2,2,2,2,2,2,2,2,2,2,2,
2,2,2,2,2,2,2,2,2,2,2,2,2,2,2,2,2,2,2,2,2,2,2,2,2,2,2,2,2,2,2,2,2,4),(-2.66742168608762,
-2.60891631867856,-2.59007764397007,-2.58078446874693,-2.57864197349874,
-2.57741406063882,-2.57633923786897,-2.57495062526262,-2.57203625467893,
-2.54226133830511,-2.49162589315616,-2.48229452219811,-2.47774260774225,
-2.4750043939937,-2.47252013229421,-2.47064406291432,-2.46881762812438,
-2.46627635089932,-2.4596385901056,-2.40382442043769,-2.37976923285203,
-2.36894807799156,-2.36670434245785,-2.36545420467988,-2.36438230657845,
-2.36302629722187,-2.36088073731076,-2.34984288349558,-2.29863084526714,
-2.26992308987829,-2.2634896846549,-2.2607811211191,-2.25881952762152,-2.25702700783975,
-2.25416222296684,-2.24727819180679,-2.19420894295487,-2.16830014997293,
-2.15699277058606,-2.15472035925147,-2.15346399585151,-2.15239272370896,
-2.1510451002617,-2.14842374276434,-2.13238357857934,-2.12707470228156,
-2.11250761379384,-2.07961726854607,-2.06305114959986,-2.05273923724512,
-2.04949046214227,-2.04741714979941,-2.04547651675621,-2.04293545891172,
-2.03864077531949,-2.00353502978294,-1.95465173086845,-1.94486010336139,
-1.94268253678395,-1.94144686883343,-1.9403731914348,-1.93899644170192,
-1.93614300531494,-1.91344691262992,-1.87272244847054,-1.84568047407998,
-1.83944847022109,-1.83677412701535,-1.83481853110581,-1.83301840721638,
-1.83011261847492,-1.82298231667828,-1.77422753641161,-1.73505269101668,
-1.73147803677481,-1.7299690266759,-1.72887686259395,-1.72785087591977,
-1.72610765891376,-1.72137455777659,-1.68179787421688,-1.63388991451972,
-1.62749311103965,-1.62479053543221,-1.62282984380313,-1.62103578005503,
-1.61816336359812,-1.6112342296848,-1.55875523121196,-1.53242869245377,
-1.52101503560159,-1.51873640346793,-1.51747862048654,-1.5164074474784,
-1.51506158505104,-1.51244823859092,-1.49656822458989,-1.49069798720759,
-1.44666701832739,-1.42810815459567,-1.41691845469197,-1.41357286139829,
-1.41147833564995,-1.40954560842506,-1.40817977626643),.UNSPECIFIED.);
#737=B_SPLINE_CURVE_WITH_KNOTS('',3,(#67907,#67908,#67909,#67910,#67911,
#67912,#67913,#67914,#67915,#67916,#67917,#67918,#67919,#67920,#67921,#67922,
#67923,#67924,#67925,#67926,#67927,#67928,#67929,#67930,#67931,#67932,#67933,
#67934,#67935,#67936,#67937,#67938,#67939,#67940,#67941,#67942,#67943,#67944,
#67945,#67946,#67947,#67948,#67949,#67950,#67951,#67952,#67953,#67954,#67955,
#67956,#67957,#67958,#67959,#67960,#67961,#67962,#67963,#67964,#67965,#67966,
#67967,#67968,#67969,#67970,#67971,#67972,#67973,#67974,#67975,#67976,#67977,
#67978,#67979,#67980,#67981,#67982,#67983,#67984,#67985,#67986,#67987,#67988,
#67989,#67990,#67991,#67992,#67993,#67994,#67995,#67996,#67997,#67998,#67999,
#68000,#68001,#68002,#68003,#68004,#68005,#68006,#68007,#68008,#68009,#68010,
#68011,#68012,#68013,#68014,#68015,#68016,#68017,#68018,#68019,#68020,#68021,
#68022,#68023,#68024,#68025,#68026,#68027,#68028,#68029,#68030,#68031,#68032,
#68033,#68034,#68035,#68036,#68037,#68038,#68039,#68040,#68041,#68042,#68043,
#68044,#68045,#68046,#68047,#68048,#68049,#68050,#68051,#68052,#68053,#68054,
#68055,#68056,#68057,#68058,#68059,#68060,#68061,#68062,#68063,#68064,#68065,
#68066,#68067,#68068,#68069,#68070,#68071,#68072,#68073,#68074,#68075,#68076,
#68077,#68078,#68079,#68080,#68081,#68082,#68083,#68084,#68085,#68086,#68087,
#68088,#68089,#68090,#68091,#68092,#68093,#68094,#68095,#68096,#68097,#68098,
#68099,#68100,#68101,#68102,#68103,#68104,#68105,#68106,#68107,#68108,#68109,
#68110,#68111,#68112,#68113,#68114,#68115,#68116,#68117,#68118,#68119,#68120,
#68121,#68122,#68123,#68124),.UNSPECIFIED.,.F.,.F.,(4,2,2,2,2,2,2,2,2,2,
2,2,2,2,2,2,2,2,2,2,2,2,2,2,2,2,2,2,2,2,2,2,2,2,2,2,2,2,2,2,2,2,2,2,2,2,
2,2,2,2,2,2,2,2,2,2,2,2,2,2,2,2,2,2,2,2,2,2,2,2,2,2,2,2,2,2,2,2,2,2,2,2,
2,2,2,2,2,2,2,2,2,2,2,2,2,2,2,2,2,2,2,2,2,2,2,2,2,2,4),(-1.25967545240964,
-1.21603450062663,-1.20965074388613,-1.20715044527458,-1.20533455736151,
-1.20338974317654,-1.20077919166635,-1.19491004781942,-1.17073316723345,
-1.12024909211881,-1.11981771635252,-1.10363128851434,-1.10100429816945,
-1.09965533242265,-1.09858382112367,-1.09732814791181,-1.0950593759243,
-1.08381930989898,-1.05817324909408,-1.00467041016011,-0.997816279860048,
-0.994956195199608,-0.993164369803906,-0.991201732196623,-0.988488404215831,
-0.982027865896532,-0.928091077431277,-0.891881747497268,-0.889027100044917,
-0.88765004663581,-0.886576260003394,-0.88534061670953,-0.883163442615538,
-0.873379711594447,-0.824459281097766,-0.789336857387192,-0.785041540824683,
-0.782500245766603,-0.780559499431617,-0.778486130777015,-0.775237400962393,
-0.764926665557967,-0.74836570266938,-0.715506838201965,-0.701764290024532,
-0.694918605780388,-0.694617606395491,-0.689272618525284,-0.679046785444263,
-0.676953690046489,-0.675613735928834,-0.674542897810459,-0.6732804504582,
-0.670980060592823,-0.659174101423956,-0.609440981833727,-0.577290998430011,
-0.573047500398641,-0.570521388151345,-0.5685832562753,-0.566503913936642,
-0.563227376669613,-0.552670037094953,-0.535559300082063,-0.490855041937219,
-0.467947985146961,-0.465089509731197,-0.463711842265131,-0.462638156455778,
-0.461403283918996,-0.459229028439546,-0.449484199246655,-0.400540681780043,
-0.365414331604263,-0.361119622900382,-0.358578726476474,-0.356638306991323,
-0.354565309237553,-0.351317205877297,-0.341008839774697,-0.324452044065934,
-0.269353861263425,-0.255460787948246,-0.25316186225543,-0.251774615966507,
-0.250697334644219,-0.249482811132885,-0.247442410732315,-0.239363469070486,
-0.224068135375557,-0.194118069974039,-0.189562252439922,-0.153470226585707,
-0.148747145118772,-0.146324136468359,-0.14440527489037,-0.142252619221595,
-0.138644787576576,-0.124692185510215,-0.0975100746812418,-0.074965690734507,
-0.0441240230176781,-0.0412117859648847,-0.039823666732855,-0.0387489813187693,
-0.0375209610406752,-0.0362288375614461,-0.0342508993908115,-0.000628702460286411),
 .UNSPECIFIED.);
#738=B_SPLINE_CURVE_WITH_KNOTS('',3,(#68125,#68126,#68127,#68128,#68129,
#68130,#68131,#68132,#68133,#68134,#68135,#68136,#68137,#68138,#68139,#68140,
#68141,#68142),.UNSPECIFIED.,.F.,.F.,(4,2,2,2,2,2,2,2,4),(-2.66795380407825,
-2.63770974612478,-2.61100504121503,-2.60481461466704,-2.60214740071707,
-2.60019300038953,-2.59839116228356,-2.59547634001882,-2.59347629365865),
 .UNSPECIFIED.);
#739=B_SPLINE_CURVE_WITH_KNOTS('',3,(#68148,#68149,#68150,#68151,#68152,
#68153,#68154,#68155,#68156,#68157,#68158,#68159,#68160),.UNSPECIFIED.,
 .F.,.F.,(4,3,3,3,4),(151.755345441108,151.823140394205,151.951948597244,
152.078650414019,152.105783788367),.UNSPECIFIED.);
#740=B_SPLINE_CURVE_WITH_KNOTS('',3,(#68161,#68162,#68163,#68164,#68165,
#68166,#68167,#68168,#68169,#68170),.UNSPECIFIED.,.F.,.F.,(4,1,1,1,1,1,
1,4),(152.105783788367,152.821976844167,153.820813294129,154.819649744091,
155.818486194052,156.817322644014,157.816159093976,158.039785833466),
 .UNSPECIFIED.);
#741=B_SPLINE_CURVE_WITH_KNOTS('',3,(#68171,#68172,#68173,#68174,#68175,
#68176,#68177,#68178,#68179,#68180,#68181,#68182,#68183,#68184,#68185,#68186,
#68187,#68188,#68189,#68190,#68191,#68192,#68193,#68194,#68195,#68196,#68197,
#68198,#68199,#68200,#68201,#68202,#68203,#68204,#68205,#68206,#68207,#68208,
#68209,#68210,#68211,#68212,#68213,#68214,#68215,#68216,#68217,#68218,#68219,
#68220,#68221,#68222,#68223,#68224,#68225,#68226,#68227,#68228,#68229,#68230,
#68231,#68232,#68233,#68234,#68235,#68236,#68237,#68238,#68239,#68240,#68241,
#68242,#68243,#68244,#68245,#68246,#68247,#68248,#68249,#68250,#68251,#68252,
#68253,#68254,#68255,#68256,#68257,#68258,#68259,#68260,#68261,#68262,#68263,
#68264,#68265,#68266,#68267,#68268,#68269,#68270,#68271,#68272,#68273,#68274,
#68275,#68276,#68277,#68278,#68279,#68280,#68281,#68282,#68283,#68284,#68285,
#68286,#68287,#68288,#68289,#68290,#68291,#68292,#68293,#68294,#68295,#68296,
#68297,#68298,#68299,#68300,#68301,#68302,#68303,#68304,#68305,#68306,#68307,
#68308,#68309,#68310,#68311,#68312,#68313,#68314,#68315,#68316,#68317,#68318,
#68319,#68320,#68321,#68322,#68323,#68324,#68325,#68326,#68327,#68328,#68329,
#68330,#68331,#68332,#68333,#68334,#68335,#68336,#68337,#68338,#68339,#68340,
#68341,#68342,#68343,#68344,#68345,#68346,#68347,#68348,#68349,#68350,#68351,
#68352,#68353,#68354,#68355,#68356,#68357,#68358,#68359,#68360,#68361,#68362,
#68363,#68364,#68365,#68366,#68367,#68368,#68369,#68370,#68371,#68372,#68373,
#68374,#68375,#68376,#68377,#68378,#68379,#68380,#68381,#68382,#68383,#68384,
#68385,#68386,#68387,#68388,#68389,#68390,#68391,#68392,#68393,#68394,#68395,
#68396,#68397,#68398,#68399,#68400),.UNSPECIFIED.,.F.,.F.,(4,2,2,2,2,2,
2,2,2,2,2,2,2,2,2,2,2,2,2,2,2,2,2,2,2,2,2,2,2,2,2,2,2,2,2,2,2,2,2,2,2,2,
2,2,2,2,2,2,2,2,2,2,2,2,2,2,2,2,2,2,2,2,2,2,2,2,2,2,2,2,2,2,2,2,2,2,2,2,
2,2,2,2,2,2,2,2,2,2,2,2,2,2,2,2,2,2,2,2,2,2,2,2,2,2,2,2,2,2,2,2,2,2,2,2,
4),(-2.59347629365865,-2.58829257532513,-2.5411668967311,-2.51687818982104,
-2.50473142931873,-2.49785808943214,-2.49591737153289,-2.49490285462753,
-2.49383144840807,-2.49248355938424,-2.48986143190541,-2.47381247037154,
-2.46857792372863,-2.42101660746502,-2.40445238062561,-2.39414115779919,
-2.39089233110921,-2.38881892057753,-2.38687814957512,-2.3843368443699,
-2.38004159228423,-2.34490982704621,-2.29594431707583,-2.28624551428981,
-2.28407421432403,-2.28283987477601,-2.28176592354043,-2.28038695137753,
-2.27816588351489,-2.26581830620826,-2.26271188533856,-2.2554980111405,
-2.2143647193356,-2.18429814564924,-2.17987187928093,-2.17754187380324,
-2.17562996445238,-2.17341113183488,-2.16960586932928,-2.15480566428064,
-2.14257500429753,-2.10708124210635,-2.08472118800863,-2.07436930278858,
-2.0721546848398,-2.07091085958896,-2.06983819716764,-2.06847323943045,
-2.06577120476464,-2.04752376693149,-2.02951962955377,-1.99678709087343,
-1.97428208502551,-1.96863575959022,-1.96606571148314,-1.96412733601595,
-1.96230008081796,-1.95975637932984,-1.95310462516989,-1.89738998985074,
-1.87326204029726,-1.86242060551688,-1.86017539939669,-1.85892482506506,
-1.85785279594466,-1.85649693031458,-1.85435216700402,-1.84333052050339,
-1.7920312423049,-1.76336881456514,-1.75694036291911,-1.75423240096493,
-1.7522707046935,-1.75047772064283,-1.74761138835131,-1.7407194677468,-1.68772908512975,
-1.66175608240713,-1.65043163279768,-1.64815799909465,-1.64690125659645,
-1.64582982839145,-1.6444822262148,-1.64186158218782,-1.6258376692416,-1.62043556344291,
-1.60593574777678,-1.57304126179432,-1.55028558881354,-1.54460521787163,
-1.54202881306141,-1.54008935023846,-1.53826378903245,-1.53572680233329,
-1.52911838860071,-1.4729707930136,-1.44912251428612,-1.43835641248185,
-1.43611567424345,-1.43486602144414,-1.43379381485167,-1.43243648266648,
-1.42977082786721,-1.41258483359625,-1.36250940842122,-1.34495460388798,
-1.3342008367151,-1.33090191892753,-1.32881733320829,-1.32688051001754,
-1.32432142927179,-1.31873513605441,-1.31131206952259,-1.2927112038443,
-1.25986769515979),.UNSPECIFIED.);
#742=B_SPLINE_CURVE_WITH_KNOTS('',3,(#68406,#68407,#68408,#68409,#68410,
#68411,#68412,#68413,#68414,#68415,#68416,#68417,#68418,#68419),
 .UNSPECIFIED.,.F.,.F.,(4,2,2,2,2,2,4),(-0.0749178273173223,-0.0723413266242414,
-0.0418124322290516,-0.00539432297196826,-0.00193487110848845,-0.000864100279469971,
-0.000629065621366007),.UNSPECIFIED.);
#743=B_SPLINE_CURVE_WITH_KNOTS('',3,(#68420,#68421,#68422,#68423,#68424,
#68425,#68426,#68427,#68428,#68429,#68430,#68431,#68432,#68433,#68434,#68435,
#68436,#68437,#68438,#68439,#68440,#68441,#68442,#68443,#68444,#68445,#68446,
#68447,#68448,#68449,#68450,#68451,#68452,#68453,#68454,#68455,#68456,#68457,
#68458,#68459,#68460,#68461,#68462,#68463,#68464,#68465,#68466,#68467,#68468,
#68469,#68470,#68471,#68472,#68473,#68474,#68475,#68476,#68477,#68478,#68479,
#68480,#68481,#68482,#68483,#68484,#68485,#68486,#68487,#68488,#68489,#68490,
#68491,#68492,#68493,#68494,#68495,#68496,#68497,#68498,#68499,#68500,#68501,
#68502,#68503,#68504,#68505,#68506,#68507,#68508,#68509,#68510,#68511,#68512,
#68513,#68514,#68515,#68516,#68517,#68518,#68519,#68520,#68521,#68522,#68523,
#68524,#68525,#68526,#68527,#68528,#68529,#68530,#68531,#68532,#68533,#68534,
#68535,#68536,#68537,#68538,#68539,#68540,#68541,#68542,#68543,#68544,#68545,
#68546,#68547,#68548,#68549,#68550,#68551,#68552,#68553,#68554,#68555,#68556,
#68557,#68558,#68559,#68560,#68561,#68562,#68563,#68564,#68565,#68566,#68567,
#68568,#68569,#68570,#68571,#68572,#68573,#68574,#68575,#68576,#68577,#68578,
#68579,#68580,#68581,#68582,#68583,#68584,#68585,#68586,#68587,#68588,#68589,
#68590,#68591,#68592,#68593,#68594,#68595,#68596,#68597,#68598,#68599,#68600),
 .UNSPECIFIED.,.F.,.F.,(4,3,3,3,3,3,3,3,3,3,3,3,3,3,3,3,3,3,3,3,3,3,3,3,
3,3,3,3,3,3,3,3,3,3,3,3,3,3,3,3,3,3,3,3,3,3,3,3,3,3,3,3,3,3,3,3,3,3,3,3,
4),(145.822598481187,145.830121694434,145.93351643147,146.036757713572,
146.139877678952,146.242932247149,146.345955455495,146.448981298155,146.552114064922,
146.65530315632,146.758675149691,146.828958144396,146.932352881429,147.035594163529,
147.138714128907,147.2417686971,147.344791905443,147.4478177481,147.550950514863,
147.654139606257,147.757511599624,147.827794594357,147.931189331481,148.034430613672,
148.137550579141,148.240605147425,148.343628355859,148.446654198607,148.54978696546,
148.652976056944,148.756348050398,148.826631044319,148.930025781262,149.033267063272,
149.136387028561,149.239441596667,149.342464804923,149.445490647494,149.548623414173,
149.651812505485,149.755184498771,149.825467494281,149.928862231266,150.032103513316,
150.135223478642,150.238278046784,150.341301255073,150.444327097677,150.547459864385,
150.650648955725,150.754020949036,150.824303944243,150.927703487106,151.031158731356,
151.134277037909,151.237328088427,151.340345921593,151.444095801472,151.547200194451,
151.651272817779,151.755345441108),.UNSPECIFIED.);
#744=B_SPLINE_CURVE_WITH_KNOTS('',3,(#68602,#68603,#68604,#68605,#68606,
#68607,#68608,#68609,#68610,#68611,#68612,#68613,#68614,#68615,#68616,#68617,
#68618,#68619,#68620,#68621,#68622,#68623,#68624,#68625,#68626,#68627,#68628,
#68629,#68630,#68631,#68632,#68633,#68634,#68635,#68636,#68637,#68638,#68639,
#68640,#68641,#68642,#68643,#68644,#68645,#68646,#68647,#68648,#68649,#68650,
#68651,#68652,#68653,#68654,#68655,#68656,#68657,#68658,#68659,#68660,#68661,
#68662,#68663,#68664,#68665,#68666,#68667,#68668,#68669,#68670,#68671,#68672,
#68673,#68674,#68675,#68676,#68677,#68678,#68679,#68680,#68681,#68682,#68683,
#68684,#68685,#68686,#68687,#68688,#68689,#68690,#68691,#68692,#68693,#68694,
#68695,#68696,#68697,#68698,#68699,#68700,#68701,#68702,#68703,#68704,#68705,
#68706,#68707,#68708,#68709,#68710,#68711,#68712,#68713,#68714,#68715,#68716,
#68717,#68718,#68719,#68720,#68721,#68722,#68723,#68724,#68725,#68726,#68727,
#68728,#68729,#68730,#68731,#68732,#68733,#68734,#68735,#68736,#68737,#68738,
#68739,#68740,#68741,#68742,#68743,#68744,#68745,#68746,#68747,#68748,#68749,
#68750,#68751,#68752,#68753,#68754,#68755,#68756,#68757,#68758,#68759,#68760,
#68761,#68762,#68763,#68764,#68765,#68766,#68767,#68768,#68769,#68770,#68771,
#68772,#68773,#68774,#68775,#68776,#68777,#68778,#68779,#68780,#68781,#68782,
#68783,#68784,#68785,#68786,#68787,#68788,#68789,#68790,#68791,#68792,#68793,
#68794,#68795,#68796,#68797,#68798,#68799,#68800,#68801,#68802,#68803,#68804,
#68805,#68806,#68807,#68808,#68809,#68810,#68811,#68812,#68813,#68814,#68815,
#68816,#68817,#68818,#68819,#68820,#68821,#68822,#68823,#68824,#68825,#68826,
#68827),.UNSPECIFIED.,.F.,.F.,(4,2,2,2,2,2,2,2,2,2,2,2,2,2,2,2,2,2,2,2,
2,2,2,2,2,2,2,2,2,2,2,2,2,2,2,2,2,2,2,2,2,2,2,2,2,2,2,2,2,2,2,2,2,2,2,2,
2,2,2,2,2,2,2,2,2,2,2,2,2,2,2,2,2,2,2,2,2,2,2,2,2,2,2,2,2,2,2,2,2,2,2,2,
2,2,2,2,2,2,2,2,2,2,2,2,2,2,2,2,2,2,2,2,4),(-1.25986769515979,-1.2499844263308,
-1.2273577862635,-1.22450577490825,-1.22312919393204,-1.22205539983242,
-1.22081932328019,-1.21864036701087,-1.20883170496701,-1.15992913113595,
-1.12481181987302,-1.12051636491675,-1.11797495911435,-1.11603411154155,
-1.11396061854871,-1.11071166006578,-1.10039991255488,-1.08383704907641,
-1.05097559989016,-1.03714819275762,-1.03049858177144,-1.01502580013971,
-1.01242885687368,-1.01108642443104,-1.01001538880904,-1.00875478599536,
-1.00646309891425,-0.994817037352779,-0.967552171293446,-0.947368838057844,
-0.912862935943923,-0.908576485430226,-0.906037714206087,-0.904097325737947,
-0.902022815774536,-0.89876911199953,-0.888415649495207,-0.871760344990376,
-0.838822650589742,-0.820097325676813,-0.803187318670966,-0.800532350845072,
-0.79917744626026,-0.798105594584209,-0.796854563336167,-0.794606865326288,
-0.783721648218932,-0.759426221407249,-0.703933009258047,-0.69725755512765,
-0.694710329946686,-0.692882274966,-0.690944640687363,-0.688378266025517,
-0.682750918500276,-0.675258439804106,-0.656402509725772,-0.626239603600697,
-0.603910453728246,-0.590918431140894,-0.588663906675867,-0.587274966899738,
-0.586200150638521,-0.584972544910109,-0.582831270663668,-0.57355424355626,
-0.554763343083938,-0.545913352488733,-0.492210670271743,-0.485374614518985,
-0.482517793901791,-0.480726769064398,-0.478764004306589,-0.476048652516343,
-0.469574475530155,-0.440526057182572,-0.394674488142699,-0.379152289898522,
-0.376553533538344,-0.375210828710214,-0.374139928436181,-0.372879895432954,
-0.37059029811673,-0.359258417209125,-0.333150177798527,-0.281816442239883,
-0.273829151212125,-0.270784101753617,-0.268957978537776,-0.267019676727467,
-0.264447801193517,-0.259241715375701,-0.252198209225489,-0.234953887526279,
-0.197957856253062,-0.167653358059792,-0.164740323769206,-0.163352090118205,
-0.16227743845337,-0.161049593689972,-0.159757697637198,-0.15511185568413,
-0.128865267669617,-0.106990977580988,-0.105569210849635,-0.0651104303029907,
-0.0603738338460286,-0.0579480560258702,-0.056029046889496,-0.0538783718243573,
-0.0516516615518185,-0.0483298236007792,-0.000628984974797087),
 .UNSPECIFIED.);
#745=B_SPLINE_CURVE_WITH_KNOTS('',3,(#68828,#68829,#68830,#68831,#68832,
#68833,#68834,#68835,#68836,#68837,#68838,#68839,#68840,#68841,#68842,#68843,
#68844,#68845,#68846,#68847),.UNSPECIFIED.,.F.,.F.,(4,2,2,2,2,2,2,2,2,4),
(-2.6677982910831,-2.62484284417815,-2.62190879437548,-2.62022600193997,
-2.61872103544168,-2.61762940481273,-2.61660206215556,-2.6148524262143,
-2.61007806701873,-2.5936683297307),.UNSPECIFIED.);
#746=B_SPLINE_CURVE_WITH_KNOTS('',3,(#68852,#68853,#68854,#68855,#68856,
#68857,#68858,#68859,#68860,#68861,#68862,#68863,#68864,#68865,#68866,#68867,
#68868,#68869,#68870,#68871,#68872,#68873,#68874,#68875,#68876,#68877,#68878,
#68879,#68880,#68881,#68882,#68883,#68884,#68885,#68886,#68887,#68888,#68889,
#68890,#68891,#68892,#68893,#68894,#68895,#68896,#68897,#68898,#68899,#68900,
#68901,#68902,#68903,#68904,#68905,#68906,#68907,#68908,#68909,#68910,#68911,
#68912,#68913,#68914,#68915,#68916,#68917,#68918,#68919,#68920,#68921,#68922,
#68923,#68924,#68925,#68926,#68927,#68928,#68929,#68930,#68931,#68932,#68933,
#68934,#68935,#68936,#68937,#68938,#68939,#68940,#68941,#68942,#68943,#68944,
#68945,#68946,#68947,#68948,#68949,#68950,#68951,#68952,#68953,#68954,#68955,
#68956,#68957,#68958,#68959,#68960,#68961,#68962,#68963,#68964,#68965,#68966,
#68967,#68968,#68969,#68970,#68971,#68972,#68973,#68974,#68975,#68976,#68977,
#68978,#68979,#68980,#68981,#68982,#68983,#68984,#68985,#68986,#68987,#68988,
#68989,#68990,#68991,#68992,#68993,#68994,#68995,#68996,#68997,#68998,#68999,
#69000,#69001,#69002,#69003,#69004,#69005,#69006,#69007,#69008,#69009,#69010,
#69011,#69012,#69013,#69014,#69015,#69016,#69017,#69018,#69019,#69020,#69021,
#69022,#69023,#69024,#69025,#69026,#69027,#69028,#69029,#69030,#69031,#69032,
#69033,#69034,#69035,#69036,#69037,#69038,#69039,#69040,#69041,#69042,#69043,
#69044,#69045,#69046,#69047,#69048,#69049,#69050,#69051,#69052,#69053,#69054,
#69055,#69056,#69057,#69058,#69059,#69060,#69061,#69062,#69063,#69064,#69065,
#69066,#69067,#69068,#69069,#69070,#69071,#69072,#69073,#69074,#69075,#69076,
#69077,#69078,#69079,#69080,#69081,#69082,#69083,#69084,#69085,#69086,#69087,
#69088,#69089,#69090,#69091,#69092,#69093,#69094,#69095,#69096,#69097,#69098,
#69099,#69100,#69101,#69102,#69103,#69104,#69105,#69106,#69107,#69108,#69109,
#69110,#69111,#69112,#69113,#69114,#69115,#69116,#69117,#69118,#69119,#69120,
#69121,#69122,#69123,#69124,#69125),.UNSPECIFIED.,.F.,.F.,(4,2,2,2,2,2,
2,2,2,2,2,2,2,2,2,2,2,2,2,2,2,2,2,2,2,2,2,2,2,2,2,2,2,2,2,2,2,2,2,2,2,2,
2,2,2,2,2,2,2,2,2,2,2,2,2,2,2,2,2,2,2,2,2,2,2,2,2,2,2,2,2,2,2,2,2,2,2,2,
2,2,2,2,2,2,2,2,2,2,2,2,2,2,2,2,2,2,2,2,2,2,2,2,2,2,2,2,2,2,2,2,2,2,2,2,
2,2,2,2,2,2,2,2,2,2,2,2,2,2,2,2,2,2,2,2,2,2,4),(-1.40862414609624,-1.39318980279119,
-1.38284072661476,-1.37958737276298,-1.37751284603091,-1.37557227418975,
-1.37303302268065,-1.36874525537374,-1.33415944586128,-1.2781862454669,
-1.27391184913531,-1.27224005010757,-1.27122788636052,-1.27012540359843,
-1.26856027607177,-1.2646472311334,-1.24543237740231,-1.189051015541,-1.17220367699145,
-1.16858648625196,-1.1662220751037,-1.1643080269843,-1.16211558550351,-1.15832879058625,
-1.14208004095366,-1.08459839210323,-1.07962518793354,-1.06363760215019,
-1.06101890048426,-1.05967166679635,-1.05860019941163,-1.05734303160051,
-1.05506765324818,-1.04371503635272,-1.01762985177148,-0.964752180156942,
-0.957848408238544,-0.954980018513344,-0.95318658397866,-0.951225072691281,
-0.948518600603874,-0.942099509999168,-0.913520898721511,-0.862318476563556,
-0.851156478542139,-0.849003060786239,-0.847644536526994,-0.846572282368348,
-0.845323607248431,-0.843087178903938,-0.832390627380297,-0.808794013748438,
-0.75222100751256,-0.745655083270969,-0.743124936486027,-0.741301236761814,
-0.73936092215405,-0.736778539925796,-0.731065044743599,-0.708064530032574,
-0.67504301687471,-0.653990204817018,-0.647228276238945,-0.638780487972627,
-0.636628936585396,-0.635386248131689,-0.634313429629788,-0.632946801850073,
-0.630144870928438,-0.596426883720288,-0.54028254859855,-0.533672456392464,
-0.531135432182919,-0.529310043610141,-0.527370948020244,-0.524795337208315,
-0.519117959943133,-0.496384070865972,-0.463534763653935,-0.427913975639064,
-0.425051291782673,-0.423672766840067,-0.422598961154527,-0.421364568781365,
-0.419192637218565,-0.409482528108991,-0.360507265752088,-0.325369848208395,
-0.321074835958497,-0.318533798237304,-0.316593292897703,-0.314520224798732,
-0.311272055836028,-0.300963857377367,-0.28440768653318,-0.233328469855719,
-0.231093888984576,-0.215559530390286,-0.212981629890186,-0.211658069355316,
-0.210638095905596,-0.210630093278843,-0.210622259266652,-0.210614583458265,
-0.210607056158067,-0.210599668548909,-0.210592412317678,-0.210585279938524,
-0.210578264423103,-0.210571359038716,-0.210564557512432,-0.210557854162641,
-0.210551243629364,-0.210544720702707,-0.21053828046371,-0.210531918507408,
-0.210525630626156,-0.21051941260701,-0.210513260713285,-0.210507171285705,
-0.21050114086118,-0.210495166127197,-0.210489243937745,-0.210483371400245,
-0.210477545698568,-0.209214406034747,-0.206826847606485,-0.19326725644468,
-0.157092503551496,-0.113387632942077,-0.109098752214622,-0.10655954168276,
-0.104619394012564,-0.10254570114519,-0.0992944491784891,-0.0889586946482435,
-0.0749178273173223),.UNSPECIFIED.);
#747=B_SPLINE_CURVE_WITH_KNOTS('',3,(#69126,#69127,#69128,#69129,#69130,
#69131,#69132,#69133,#69134,#69135,#69136,#69137,#69138,#69139,#69140,#69141,
#69142,#69143,#69144,#69145,#69146,#69147,#69148,#69149,#69150,#69151,#69152,
#69153,#69154,#69155,#69156,#69157,#69158,#69159,#69160,#69161,#69162,#69163,
#69164,#69165,#69166,#69167,#69168,#69169,#69170,#69171,#69172,#69173,#69174,
#69175,#69176,#69177,#69178,#69179,#69180,#69181,#69182,#69183,#69184,#69185,
#69186,#69187,#69188,#69189,#69190,#69191,#69192,#69193,#69194,#69195,#69196,
#69197,#69198,#69199,#69200,#69201,#69202,#69203,#69204,#69205,#69206,#69207,
#69208,#69209,#69210,#69211,#69212,#69213,#69214,#69215,#69216,#69217,#69218,
#69219,#69220,#69221,#69222,#69223,#69224,#69225,#69226,#69227,#69228,#69229,
#69230,#69231,#69232,#69233,#69234,#69235,#69236,#69237,#69238,#69239,#69240,
#69241,#69242,#69243,#69244,#69245,#69246,#69247,#69248,#69249,#69250,#69251,
#69252,#69253,#69254,#69255,#69256,#69257,#69258,#69259,#69260,#69261,#69262,
#69263,#69264,#69265,#69266,#69267,#69268,#69269,#69270,#69271,#69272,#69273,
#69274,#69275,#69276,#69277,#69278,#69279,#69280,#69281,#69282,#69283,#69284,
#69285,#69286,#69287,#69288,#69289,#69290,#69291,#69292,#69293,#69294,#69295,
#69296,#69297,#69298,#69299,#69300,#69301,#69302,#69303,#69304,#69305,#69306,
#69307,#69308,#69309,#69310,#69311,#69312,#69313,#69314,#69315,#69316,#69317,
#69318,#69319,#69320,#69321,#69322,#69323,#69324,#69325,#69326,#69327,#69328,
#69329,#69330,#69331,#69332,#69333,#69334,#69335,#69336,#69337,#69338,#69339,
#69340,#69341,#69342,#69343,#69344,#69345,#69346,#69347,#69348,#69349,#69350,
#69351,#69352,#69353,#69354,#69355,#69356,#69357),.UNSPECIFIED.,.F.,.F.,
(4,2,2,2,2,2,2,2,2,2,2,2,2,2,2,2,2,2,2,2,2,2,2,2,2,2,2,2,2,2,2,2,2,2,2,
2,2,2,2,2,2,2,2,2,2,2,2,2,2,2,2,2,2,2,2,2,2,2,2,2,2,2,2,2,2,2,2,2,2,2,2,
2,2,2,2,2,2,2,2,2,2,2,2,2,2,2,2,2,2,2,2,2,2,2,2,2,2,2,2,2,2,2,2,2,2,2,2,
2,2,2,2,2,2,2,2,4),(-2.5936683297307,-2.5726207840679,-2.55119822559827,
-2.52286135770751,-2.51638838092519,-2.51426413649379,-2.51218418040178,
-2.51024532309731,-2.50771804735601,-2.50347214253205,-2.47125311799585,
-2.43576565912732,-2.41832802532113,-2.40950864041021,-2.40740843522256,
-2.4061801278211,-2.40510499243148,-2.40371601917802,-2.40080104535941,
-2.3706852886388,-2.31914736690955,-2.31048993812756,-2.30424070509671,
-2.30153110187088,-2.29956889863741,-2.29777592025381,-2.29491061704547,
-2.2880264542602,-2.23491463762945,-2.20901717245987,-2.19771130706315,
-2.19543851015384,-2.19418184086959,-2.19311023869051,-2.19176211668817,
-2.1891395762449,-2.1730887360403,-2.16783995619816,-2.15321513168035,-2.12031456163141,
-2.10374303951701,-2.09342781749038,-2.09017801912045,-2.08810405773785,
-2.08616281978226,-2.0836209733347,-2.0793249637779,-2.04420790571177,-1.99530255525716,
-1.98551591591854,-1.98333821708696,-1.98210228269514,-1.98102825171372,
-1.97965088664476,-1.97679561477164,-1.9538281481496,-1.95168520789728,
-1.91152613950497,-1.89283640251648,-1.88158938989891,-1.878236792081,-1.87614013048961,
-1.8742069566071,-1.87171694656131,-1.8675985967015,-1.84074921139561,-1.79877078660577,
-1.78196749243118,-1.77334179158195,-1.77124909985302,-1.77003193385426,
-1.76895464362035,-1.76757038233075,-1.7652825972158,-1.75163464434942,
-1.74988584604178,-1.70251515946709,-1.67153888852473,-1.66708667104672,
-1.66475093468465,-1.66283834912034,-1.66062326542956,-1.65683551969551,
-1.64224021250126,-1.6299740707683,-1.58956098626714,-1.57070633717263,
-1.56140707116998,-1.55926368223693,-1.55803533939617,-1.55696019326658,
-1.55557123290499,-1.55265638065077,-1.52381683594311,-1.48570476804185,
-1.46817820092768,-1.45743650849027,-1.45413866485049,-1.45205414839308,
-1.4501169686029,-1.44760031308069,-1.44339085464906,-1.41291513139376,
-1.36768694294417,-1.35579379322469,-1.35125847821227,-1.34794990407903,
-1.34648734813586,-1.34540259097681,-1.34421364338769,-1.3422475989548,
-1.33584217266315,-1.33428618716082,-1.31969892252657,-1.26065445785916,
-1.25983890058673),.UNSPECIFIED.);
#748=B_SPLINE_CURVE_WITH_KNOTS('',3,(#69363,#69364,#69365,#69366,#69367,
#69368,#69369,#69370),.UNSPECIFIED.,.F.,.F.,(4,2,2,4),(-0.0748543400333247,
-0.0730685011140681,-0.0491237947608074,-0.000629479192835824),
 .UNSPECIFIED.);
#749=B_SPLINE_CURVE_WITH_KNOTS('',3,(#69371,#69372,#69373,#69374,#69375,
#69376,#69377,#69378,#69379,#69380,#69381,#69382,#69383,#69384,#69385,#69386,
#69387,#69388,#69389,#69390,#69391,#69392,#69393,#69394,#69395,#69396,#69397,
#69398,#69399,#69400,#69401,#69402,#69403,#69404,#69405,#69406,#69407,#69408,
#69409,#69410,#69411,#69412,#69413,#69414,#69415,#69416,#69417,#69418,#69419,
#69420,#69421,#69422,#69423,#69424,#69425,#69426,#69427,#69428,#69429,#69430,
#69431,#69432,#69433,#69434,#69435,#69436,#69437,#69438,#69439,#69440,#69441,
#69442,#69443,#69444,#69445,#69446,#69447,#69448,#69449,#69450,#69451,#69452,
#69453,#69454,#69455,#69456,#69457,#69458,#69459,#69460,#69461,#69462,#69463,
#69464,#69465,#69466,#69467,#69468,#69469,#69470,#69471,#69472,#69473,#69474,
#69475,#69476,#69477,#69478,#69479,#69480,#69481,#69482,#69483,#69484,#69485,
#69486,#69487,#69488,#69489,#69490,#69491,#69492,#69493,#69494,#69495,#69496,
#69497,#69498,#69499,#69500,#69501,#69502,#69503,#69504,#69505,#69506,#69507,
#69508,#69509,#69510,#69511,#69512,#69513,#69514,#69515,#69516,#69517,#69518,
#69519,#69520,#69521,#69522,#69523,#69524,#69525,#69526,#69527,#69528,#69529,
#69530,#69531,#69532,#69533,#69534,#69535,#69536,#69537,#69538,#69539,#69540,
#69541,#69542,#69543,#69544,#69545,#69546,#69547,#69548,#69549,#69550,#69551,
#69552,#69553,#69554,#69555,#69556,#69557,#69558,#69559,#69560,#69561,#69562,
#69563,#69564,#69565,#69566,#69567,#69568,#69569,#69570,#69571,#69572,#69573,
#69574,#69575,#69576,#69577,#69578,#69579,#69580,#69581,#69582,#69583,#69584,
#69585,#69586,#69587,#69588,#69589,#69590,#69591,#69592,#69593,#69594,#69595,
#69596,#69597,#69598,#69599,#69600,#69601,#69602,#69603,#69604,#69605,#69606,
#69607,#69608,#69609,#69610,#69611,#69612,#69613,#69614,#69615,#69616,#69617,
#69618,#69619,#69620,#69621,#69622,#69623,#69624,#69625,#69626,#69627,#69628),
 .UNSPECIFIED.,.F.,.F.,(4,2,2,2,2,2,2,2,2,2,2,2,2,2,2,2,2,2,2,2,2,2,2,2,
2,2,2,2,2,2,2,2,2,2,2,2,2,2,2,2,2,2,2,2,2,2,2,2,2,2,2,2,2,2,2,2,2,2,2,2,
2,2,2,2,2,2,2,2,2,2,2,2,2,2,2,2,2,2,2,2,2,2,2,2,2,2,2,2,2,2,2,2,2,2,2,2,
2,2,2,2,2,2,2,2,2,2,2,2,2,2,2,2,2,2,2,2,2,2,2,2,2,2,2,2,2,2,2,2,4),(-2.66814368829348,
-2.66034873118431,-2.65505152358494,-2.65260779199081,-2.65072566522708,
-2.6488846910573,-2.64705802280244,-2.64451726183137,-2.63932533848064,
-2.62681330898061,-2.57513659029226,-2.55629150625919,-2.54699526628027,
-2.54485209086409,-2.54362379238626,-2.54254863419885,-2.54115959109167,
-2.53824432801602,-2.50854367015596,-2.45808754405171,-2.44859722597837,
-2.44398932066425,-2.44020970600377,-2.43803870623047,-2.43802300969667,
-2.4380067605024,-2.43798993855578,-2.43797252300731,-2.43795449224214,
-2.43793582387495,-2.4379164947004,-2.43789648064213,-2.43787575678477,
-2.4378542973178,-2.43783207551628,-2.43780906301748,-2.43778902406746,
-2.4377656706735,-2.43773846067708,-2.43770676597262,-2.43766986014221,
-2.43762690482853,-2.4375726852995,-2.43563170291138,-2.43308934965835,
-2.42879059675919,-2.39366442341326,-2.34469891665934,-2.33499836395926,
-2.33282690447066,-2.33159251024439,-2.33051853457682,-2.32913956130739,
-2.32627516729251,-2.29031752177012,-2.2575466302749,-2.23498252385049,
-2.22932813927916,-2.22675657538432,-2.22481793266635,-2.22299106930673,
-2.22044894667414,-2.21380749423047,-2.15799208910578,-2.13392861942916,
-2.12310446786992,-2.12086027325997,-2.1196099025175,-2.11853782608796,
-2.11718161605693,-2.1150357747995,-2.10399726717983,-2.05277424947031,
-2.02406100664172,-2.0176264316783,-2.01491739871002,-2.01295547388808,
-2.01116265737428,-2.00829741164116,-2.00141234454558,-1.94832934653784,
-1.92241930829777,-1.91111079398823,-1.90883803777882,-1.90758146809275,
-1.90650999765976,-1.90516210101186,-1.90254017435152,-1.8864959682302,
-1.88120554232293,-1.86661833145533,-1.8337220866743,-1.81715303187371,
-1.80683926115751,-1.80358987508024,-1.80151616601908,-1.79957515665534,
-1.79703359858572,-1.79273805190484,-1.75762153288418,-1.70871089440112,
-1.69893858239314,-1.6967620416682,-1.69552645190864,-1.69445252034459,
-1.69307502126333,-1.69021857225249,-1.66741781584811,-1.61179980388429,
-1.59578596449105,-1.59201598172407,-1.58982721629583,-1.58791275959955,
-1.58554317036637,-1.58190933911534,-1.56481024540013,-1.55674001414502,
-1.52192473962697,-1.49787209418288,-1.48705111597682,-1.48480720636253,
-1.48355694212671,-1.48248492478154,-1.48112874813835,-1.47846810954277,
-1.46141221384331,-1.44279783998196,-1.40983725064088,-1.40862414609624),
 .UNSPECIFIED.);
#750=B_SPLINE_CURVE_WITH_KNOTS('',3,(#69630,#69631,#69632,#69633,#69634,
#69635,#69636,#69637,#69638,#69639,#69640,#69641,#69642,#69643,#69644,#69645,
#69646,#69647,#69648,#69649,#69650,#69651,#69652,#69653,#69654,#69655,#69656,
#69657,#69658,#69659,#69660,#69661,#69662,#69663,#69664,#69665,#69666,#69667,
#69668,#69669,#69670,#69671,#69672,#69673,#69674,#69675,#69676,#69677,#69678,
#69679,#69680,#69681,#69682,#69683,#69684,#69685,#69686,#69687,#69688,#69689,
#69690,#69691,#69692,#69693,#69694,#69695,#69696,#69697,#69698,#69699,#69700,
#69701,#69702,#69703,#69704,#69705,#69706,#69707,#69708,#69709,#69710,#69711,
#69712,#69713,#69714,#69715,#69716,#69717,#69718,#69719,#69720,#69721,#69722,
#69723,#69724,#69725,#69726,#69727,#69728,#69729,#69730,#69731,#69732,#69733,
#69734,#69735,#69736,#69737,#69738,#69739,#69740,#69741,#69742,#69743,#69744,
#69745,#69746,#69747,#69748,#69749,#69750,#69751,#69752,#69753,#69754,#69755,
#69756,#69757,#69758,#69759,#69760,#69761,#69762,#69763,#69764,#69765,#69766,
#69767,#69768,#69769,#69770,#69771,#69772,#69773,#69774,#69775,#69776,#69777,
#69778,#69779,#69780,#69781,#69782,#69783,#69784,#69785,#69786,#69787,#69788,
#69789,#69790,#69791,#69792,#69793,#69794,#69795,#69796,#69797,#69798,#69799,
#69800,#69801,#69802,#69803,#69804,#69805,#69806,#69807,#69808,#69809,#69810,
#69811,#69812,#69813,#69814,#69815,#69816,#69817,#69818,#69819,#69820,#69821,
#69822,#69823,#69824,#69825,#69826,#69827,#69828,#69829,#69830,#69831,#69832,
#69833,#69834,#69835,#69836,#69837,#69838,#69839,#69840,#69841),
 .UNSPECIFIED.,.F.,.F.,(4,2,2,2,2,2,2,2,2,2,2,2,2,2,2,2,2,2,2,2,2,2,2,2,
2,2,2,2,2,2,2,2,2,2,2,2,2,2,2,2,2,2,2,2,2,2,2,2,2,2,2,2,2,2,2,2,2,2,2,2,
2,2,2,2,2,2,2,2,2,2,2,2,2,2,2,2,2,2,2,2,2,2,2,2,2,2,2,2,2,2,2,2,2,2,2,2,
2,2,2,2,2,2,2,2,2,4),(-1.25983890058673,-1.24634406344438,-1.24258219161815,
-1.24037324998251,-1.23846050074872,-1.23611765858758,-1.23163051026512,
-1.19926717360426,-1.15908299348593,-1.1541501744994,-1.13819946766059,
-1.13558278234653,-1.13423599916244,-1.13316458106479,-1.13190711265831,
-1.1296302780235,-1.1182515945149,-1.09206315122662,-1.03933492965326,-1.03242027292118,
-1.02955012835499,-1.02775640087641,-1.02579521475537,-1.02309037344317,
-1.01668073355414,-0.988180701441149,-0.937248744330339,-0.925763770623649,
-0.923591050901342,-0.922226669260455,-0.921153966790587,-0.919909539851915,
-0.917692476034015,-0.907304808266461,-0.884817221689897,-0.826488685982098,
-0.820131081486876,-0.817635177981923,-0.815820450706279,-0.813874971674538,
-0.811260203321051,-0.8053673892928,-0.78100871753366,-0.730336180278094,
-0.714124144264271,-0.711496163020898,-0.710147000641374,-0.709075492226207,
-0.707820004520276,-0.705552050381173,-0.694325812729196,-0.668733325368552,
-0.61515331894606,-0.608305517771778,-0.605446487862613,-0.603654862354507,
-0.601692072007581,-0.598977849116755,-0.592511919936247,-0.538387101565756,
-0.502385066625971,-0.499523482558151,-0.498145071609489,-0.497071159822568,
-0.495836425627053,-0.493663367892962,-0.483939608367895,-0.434968805203786,
-0.399816974208812,-0.395528974833991,-0.39298980903015,-0.391049420450672,
-0.388975203055071,-0.385722570313168,-0.375377700659135,-0.358741168315753,
-0.325819822418563,-0.307757445673727,-0.290182369777355,-0.287503244684659,
-0.28614321277118,-0.285071011863426,-0.283823823813925,-0.281593590316445,
-0.270992728538176,-0.247741175267763,-0.192010060381105,-0.18452885394621,
-0.181563540173496,-0.179752471417974,-0.177922125735423,-0.175416890437485,
-0.170092083543928,-0.163020954964638,-0.145679755924338,-0.097270332702688,
-0.0924434285828069,-0.0779766547156677,-0.075650015844025,-0.0742546067190068,
-0.0731762444961421,-0.0719663774955741,-0.0699052135922942,-0.0616645216555707,
-0.0459685411644556,-0.000629550022902194),.UNSPECIFIED.);
#751=B_SPLINE_CURVE_WITH_KNOTS('',3,(#69842,#69843,#69844,#69845,#69846,
#69847,#69848,#69849,#69850,#69851,#69852,#69853,#69854,#69855,#69856,#69857,
#69858,#69859,#69860,#69861,#69862,#69863),.UNSPECIFIED.,.F.,.F.,(4,2,2,
2,2,2,2,2,2,2,4),(-2.667696362868,-2.64236919542473,-2.63924210061828,-2.63709594523076,
-2.63529507404303,-2.63338105697752,-2.63101180962497,-2.62737812380157,
-2.61027214598184,-2.59808114560931,-2.59327317464725),.UNSPECIFIED.);
#752=B_SPLINE_CURVE_WITH_KNOTS('',3,(#69868,#69869,#69870,#69871,#69872,
#69873,#69874,#69875,#69876,#69877,#69878,#69879,#69880,#69881,#69882,#69883,
#69884,#69885,#69886,#69887,#69888,#69889,#69890,#69891,#69892,#69893,#69894,
#69895,#69896,#69897,#69898,#69899,#69900,#69901,#69902,#69903,#69904,#69905,
#69906,#69907,#69908,#69909,#69910,#69911,#69912,#69913,#69914,#69915,#69916,
#69917,#69918,#69919,#69920,#69921,#69922,#69923,#69924,#69925,#69926,#69927,
#69928,#69929,#69930,#69931,#69932,#69933,#69934,#69935,#69936,#69937,#69938,
#69939,#69940,#69941,#69942,#69943,#69944,#69945,#69946,#69947,#69948,#69949,
#69950,#69951,#69952,#69953,#69954,#69955,#69956,#69957,#69958,#69959,#69960,
#69961,#69962,#69963,#69964,#69965,#69966,#69967,#69968,#69969,#69970,#69971,
#69972,#69973,#69974,#69975,#69976,#69977,#69978,#69979,#69980,#69981,#69982,
#69983,#69984,#69985,#69986,#69987,#69988,#69989,#69990,#69991,#69992,#69993,
#69994,#69995,#69996,#69997,#69998,#69999,#70000,#70001,#70002,#70003,#70004,
#70005,#70006,#70007,#70008,#70009,#70010,#70011,#70012,#70013,#70014,#70015,
#70016,#70017,#70018,#70019,#70020,#70021,#70022,#70023,#70024,#70025,#70026,
#70027,#70028,#70029,#70030,#70031,#70032,#70033,#70034,#70035,#70036,#70037,
#70038,#70039,#70040,#70041,#70042,#70043,#70044,#70045,#70046,#70047,#70048,
#70049,#70050,#70051,#70052,#70053,#70054,#70055,#70056,#70057,#70058,#70059,
#70060,#70061,#70062,#70063,#70064,#70065,#70066,#70067,#70068,#70069,#70070,
#70071,#70072,#70073,#70074,#70075,#70076,#70077,#70078,#70079,#70080,#70081,
#70082,#70083,#70084,#70085,#70086,#70087,#70088,#70089,#70090,#70091,#70092,
#70093,#70094,#70095,#70096,#70097,#70098,#70099,#70100,#70101,#70102,#70103,
#70104,#70105,#70106,#70107,#70108,#70109),.UNSPECIFIED.,.F.,.F.,(4,2,2,
2,2,2,2,2,2,2,2,2,2,2,2,2,2,2,2,2,2,2,2,2,2,2,2,2,2,2,2,2,2,2,2,2,2,2,2,
2,2,2,2,2,2,2,2,2,2,2,2,2,2,2,2,2,2,2,2,2,2,2,2,2,2,2,2,2,2,2,2,2,2,2,2,
2,2,2,2,2,2,2,2,2,2,2,2,2,2,2,2,2,2,2,2,2,2,2,2,2,2,2,2,2,2,2,2,2,2,2,2,
2,2,2,2,2,2,2,2,2,4),(-1.40834652030694,-1.40119964678896,-1.3750453295523,
-1.36367482587345,-1.36139854842979,-1.36014122842095,-1.35906984371272,
-1.35772297797095,-1.35510576847566,-1.33914378880401,-1.33419979165065,
-1.32855380466372,-1.28159454650626,-1.28014905551357,-1.26110947023717,
-1.25734830242951,-1.25493954883956,-1.25302179779228,-1.25085960514823,
-1.24720980334545,-1.2327575183561,-1.18237043657965,-1.1527028321594,-1.1497883459888,
-1.14839958362139,-1.14732459775158,-1.14609645511031,-1.14395344114746,
-1.13465649989949,-1.11580505635895,-1.07535189164056,-1.06307322427455,
-1.04849344934274,-1.04470748206018,-1.04249303256104,-1.04058074806373,
-1.03824506925409,-1.03379200257817,-1.002756085599,-0.954779146164212,
-0.940189593244896,-0.93785721640681,-0.936459975086064,-0.935381181248489,
-0.934171927756229,-0.932114237676863,-0.923919063393083,-0.90835353979627,
-0.866772127234862,-0.854686082958407,-0.836943624112443,-0.833267940453417,
-0.830885427656707,-0.828969951331454,-0.826790253764856,-0.823061439572297,
-0.807603545846204,-0.755931244369677,-0.728679182947644,-0.725775379934821,
-0.724388660243346,-0.723313849021782,-0.722084330554783,-0.719935218297145,
-0.710554369962836,-0.661283712197524,-0.626052679490348,-0.621755690793678,
-0.619213822412307,-0.617272877714507,-0.615199529265458,-0.611951315626917,
-0.60164630011947,-0.585098401745746,-0.552249102173091,-0.539739318930592,
-0.516621656941801,-0.513764052151514,-0.512386448205456,-0.511312644072672,
-0.510077445504139,-0.507902165131855,-0.49814530336416,-0.449204353142808,
-0.414077528364177,-0.409781556887335,-0.407240121406575,-0.405299410053123,
-0.403226216624753,-0.399978049116185,-0.389671522433624,-0.373119621693654,
-0.34026903733369,-0.327235070420115,-0.318518706322198,-0.304213318370959,
-0.301892997747478,-0.300499430127896,-0.299421295226148,-0.298210346503724,
-0.296144370484358,-0.287845384120449,-0.271983674965682,-0.22595801836517,
-0.201643903831069,-0.197626207315011,-0.195166461523407,-0.193295990106968,
-0.191268163552431,-0.188078056392624,-0.184324499429698,-0.177192650513944,
-0.159636482061495,-0.109560650108114,-0.0924412901657382,-0.0897787049546927,
-0.0884222410408426,-0.087350360247461,-0.0861006799385381,-0.0838588658302869,
-0.0748543400333247),.UNSPECIFIED.);
#753=B_SPLINE_CURVE_WITH_KNOTS('',3,(#70110,#70111,#70112,#70113,#70114,
#70115,#70116,#70117,#70118,#70119,#70120,#70121,#70122,#70123,#70124,#70125,
#70126,#70127,#70128,#70129,#70130,#70131,#70132,#70133,#70134,#70135,#70136,
#70137,#70138,#70139,#70140,#70141,#70142,#70143,#70144,#70145,#70146,#70147,
#70148,#70149,#70150,#70151,#70152,#70153,#70154,#70155,#70156,#70157,#70158,
#70159,#70160,#70161,#70162,#70163,#70164,#70165,#70166,#70167,#70168,#70169,
#70170,#70171,#70172,#70173,#70174,#70175,#70176,#70177,#70178,#70179,#70180,
#70181,#70182,#70183,#70184,#70185,#70186,#70187,#70188,#70189,#70190,#70191,
#70192,#70193,#70194,#70195,#70196,#70197,#70198,#70199,#70200,#70201,#70202,
#70203,#70204,#70205,#70206,#70207,#70208,#70209,#70210,#70211,#70212,#70213,
#70214,#70215,#70216,#70217,#70218,#70219,#70220,#70221,#70222,#70223,#70224,
#70225,#70226,#70227,#70228,#70229,#70230,#70231,#70232,#70233,#70234,#70235,
#70236,#70237,#70238,#70239,#70240,#70241,#70242,#70243,#70244,#70245,#70246,
#70247,#70248,#70249,#70250,#70251,#70252,#70253,#70254,#70255,#70256,#70257,
#70258,#70259,#70260,#70261,#70262,#70263,#70264,#70265,#70266,#70267,#70268,
#70269,#70270,#70271,#70272,#70273,#70274,#70275,#70276,#70277,#70278,#70279,
#70280,#70281,#70282,#70283,#70284,#70285,#70286,#70287,#70288,#70289,#70290,
#70291,#70292,#70293,#70294,#70295,#70296,#70297,#70298,#70299,#70300,#70301,
#70302,#70303,#70304,#70305,#70306,#70307,#70308,#70309,#70310,#70311,#70312,
#70313,#70314,#70315,#70316,#70317,#70318,#70319,#70320,#70321,#70322,#70323,
#70324,#70325,#70326,#70327,#70328,#70329,#70330,#70331,#70332,#70333,#70334,
#70335,#70336,#70337,#70338,#70339),.UNSPECIFIED.,.F.,.F.,(4,2,2,2,2,2,
2,2,2,2,2,2,2,2,2,2,2,2,2,2,2,2,2,2,2,2,2,2,2,2,2,2,2,2,2,2,2,2,2,2,2,2,
2,2,2,2,2,2,2,2,2,2,2,2,2,2,2,2,2,2,2,2,2,2,2,2,2,2,2,2,2,2,2,2,2,2,2,2,
2,2,2,2,2,2,2,2,2,2,2,2,2,2,2,2,2,2,2,2,2,2,2,2,2,2,2,2,2,2,2,2,2,2,2,2,
4),(-2.59327317464725,-2.5704590027846,-2.54404918097376,-2.53261552028791,
-2.53033608522694,-2.5290782841031,-2.52800725378591,-2.52666180509699,
-2.52405019688048,-2.50827802161836,-2.50219760153401,-2.48282618273537,
-2.45493277432578,-2.43856538231164,-2.43177383929103,-2.42660779292877,
-2.42413937703768,-2.4222998924718,-2.42047511511372,-2.41793999218273,
-2.41134096218204,-2.35511961642112,-2.33133628620871,-2.32058892226935,
-2.31834972848019,-2.31710060479993,-2.31602864689801,-2.31467136584933,
-2.31252153835837,-2.30141357383613,-2.25015852191306,-2.22155602401871,
-2.21513527000744,-2.2124289049315,-2.21046776747491,-2.20867488257282,
-2.20580781280618,-2.19890947715483,-2.14603385775022,-2.11999207485746,
-2.10865099916055,-2.10637670979702,-2.10511996465956,-2.10404875247291,
-2.10270169977916,-2.10008294074918,-2.08408638148977,-2.07858665334349,
-2.06415914998794,-2.03127147490742,-2.0147079811946,-2.00439730764157,
-2.00114870346013,-1.99907544681252,-1.99713482819271,-1.99459373455749,
-1.99029886703047,-1.95517383607453,-1.90622460815131,-1.89651182976436,
-1.89433968318877,-1.89310521584231,-1.89203138021895,-1.89065285328871,
-1.88843307926109,-1.87610725052837,-1.8729791507541,-1.87277770786138,
-1.86591077771597,-1.8521781256169,-1.81929555402153,-1.80273984895054,
-1.79243249631211,-1.78918412564446,-1.78711082267907,-1.78517002347376,
-1.78262849535985,-1.77833244964047,-1.74313778478156,-1.69396685742474,
-1.68450731601472,-1.68235275394786,-1.68112210340309,-1.68004759568449,
-1.67866295841088,-1.67576945747559,-1.64973504199282,-1.61156794503932,
-1.58253999009771,-1.57814437560976,-1.57582080172747,-1.57390919438664,
-1.5716850692273,-1.5678568102575,-1.55279545393319,-1.50062697925078,-1.48178138712014,
-1.47248554193453,-1.47034264219521,-1.46911453147393,-1.46803955704983,
-1.46665077698046,-1.4637361564445,-1.43368995263626,-1.38234822370932,
-1.369008011865,-1.36545296099196,-1.36331180205574,-1.36139051569147,-1.35894717976743,
-1.3550726159874,-1.33399840580333,-1.2761823698615,-1.26122152598105,-1.2597871053314),
 .UNSPECIFIED.);
#754=B_SPLINE_CURVE_WITH_KNOTS('',3,(#70345,#70346,#70347,#70348),
 .UNSPECIFIED.,.F.,.F.,(4,4),(120.339865638913,120.689851223516),
 .UNSPECIFIED.);
#755=B_SPLINE_CURVE_WITH_KNOTS('',3,(#70349,#70350,#70351,#70352,#70353,
#70354,#70355,#70356,#70357,#70358,#70359,#70360,#70361,#70362,#70363,#70364,
#70365,#70366,#70367,#70368,#70369,#70370,#70371,#70372,#70373,#70374,#70375,
#70376,#70377,#70378,#70379,#70380,#70381,#70382,#70383,#70384,#70385,#70386,
#70387,#70388,#70389,#70390,#70391,#70392,#70393,#70394,#70395,#70396,#70397,
#70398,#70399,#70400,#70401,#70402,#70403,#70404,#70405,#70406,#70407,#70408,
#70409,#70410,#70411,#70412,#70413,#70414,#70415,#70416,#70417,#70418,#70419,
#70420,#70421,#70422,#70423,#70424,#70425,#70426,#70427,#70428,#70429,#70430,
#70431,#70432,#70433,#70434,#70435,#70436,#70437,#70438,#70439,#70440,#70441,
#70442,#70443,#70444,#70445,#70446,#70447,#70448,#70449,#70450,#70451,#70452,
#70453,#70454,#70455,#70456,#70457,#70458,#70459,#70460,#70461,#70462,#70463,
#70464,#70465,#70466,#70467,#70468,#70469,#70470,#70471,#70472,#70473,#70474,
#70475,#70476,#70477,#70478,#70479,#70480,#70481,#70482,#70483,#70484,#70485,
#70486,#70487,#70488,#70489,#70490,#70491,#70492,#70493,#70494,#70495,#70496,
#70497,#70498,#70499,#70500,#70501,#70502,#70503,#70504,#70505,#70506,#70507,
#70508,#70509,#70510,#70511,#70512,#70513,#70514,#70515,#70516,#70517,#70518,
#70519,#70520,#70521,#70522,#70523,#70524,#70525,#70526,#70527,#70528,#70529,
#70530,#70531,#70532,#70533,#70534,#70535,#70536,#70537,#70538,#70539,#70540,
#70541,#70542,#70543,#70544,#70545,#70546,#70547,#70548,#70549,#70550,#70551,
#70552,#70553,#70554,#70555,#70556,#70557,#70558,#70559,#70560,#70561,#70562,
#70563,#70564,#70565,#70566,#70567,#70568,#70569,#70570,#70571,#70572,#70573,
#70574,#70575,#70576),.UNSPECIFIED.,.F.,.F.,(4,2,2,2,2,2,2,2,2,2,2,2,2,
2,2,2,2,2,2,2,2,2,2,2,2,2,2,2,2,2,2,2,2,2,2,2,2,2,2,2,2,2,2,2,2,2,2,2,2,
2,2,2,2,2,2,2,2,2,2,2,2,2,2,2,2,2,2,2,2,2,2,2,2,2,2,2,2,2,2,2,2,2,2,2,2,
2,2,2,2,2,2,2,2,2,2,2,2,2,2,2,2,2,2,2,2,2,2,2,2,2,2,2,2,4),(-2.66748066396766,
-2.64325165294474,-2.63611998857546,-2.63432914679269,-2.6331142274289,
-2.63210518692895,-2.63103064790152,-2.62964466350476,-2.62674376603921,
-2.59982441801465,-2.58614200050883,-2.57462196577174,-2.54604820313479,
-2.53214899282668,-2.52854547413825,-2.52639366245585,-2.52447447035581,
-2.52204958324415,-2.51731825731717,-2.47994237194092,-2.42958389839601,
-2.42522387950895,-2.42204644301473,-2.42060887408388,-2.4195236539985,
-2.4183371979469,-2.41638144970986,-2.41006037803734,-2.4080000595306,-2.35602879302201,
-2.32315616991477,-2.31773705582591,-2.31520955914026,-2.3132777088833,
-2.31143746612195,-2.30831990111571,-2.29985602604933,-2.29781059032818,
-2.23583608353085,-2.21970622265552,-2.21131263343446,-2.20923883645165,
-2.20802607386156,-2.20694821608152,-2.20555744504906,-2.20324687255974,
-2.18912145936736,-2.18398898501836,-2.14011387655121,-2.10956182064669,
-2.10512208970602,-2.10278932770777,-2.10087736000318,-2.09866094449101,
-2.094865914625,-2.08018098825123,-2.07341156456318,-2.02549659616954,-2.0081840522412,
-1.99938767863716,-1.99728211867183,-1.9960623108214,-1.99498591849885,
-1.99360696590135,-1.99133649089239,-1.97803188926882,-1.9742970159181,
-1.92390847972603,-1.90628290727486,-1.89549845985183,-1.89219648694784,
-1.89011143904926,-1.88817519919052,-1.88566179821301,-1.88146225363339,
-1.85137878627351,-1.79974424985816,-1.78774269885316,-1.78543170571901,
-1.78416692499859,-1.78309618670941,-1.7817589750698,-1.77967491397366,
-1.76959036346571,-1.76409043029117,-1.7566627632639,-1.74315564492008,
-1.71027397103749,-1.69372031343915,-1.68341376853591,-1.68016540386274,
-1.67809204497705,-1.67615115145131,-1.67360943925168,-1.66931294658394,
-1.63409593080558,-1.58485106489426,-1.57547341884819,-1.57332463114969,
-1.57209522158556,-1.5710204609527,-1.56963373723613,-1.56738702422891,
-1.55455413319405,-1.55238811132641,-1.50510774622675,-1.47658362094603,
-1.47017166108594,-1.46746647789825,-1.46550527825293,-1.46371170374019,
-1.46084215261057,-1.45393070740558,-1.40834652030694),.UNSPECIFIED.);
#756=B_SPLINE_CURVE_WITH_KNOTS('',3,(#70578,#70579,#70580,#70581,#70582,
#70583,#70584,#70585,#70586,#70587,#70588,#70589,#70590,#70591,#70592,#70593,
#70594,#70595,#70596,#70597,#70598,#70599,#70600,#70601,#70602,#70603,#70604,
#70605,#70606,#70607,#70608,#70609,#70610,#70611,#70612,#70613,#70614,#70615,
#70616,#70617,#70618,#70619,#70620,#70621,#70622,#70623,#70624,#70625,#70626,
#70627,#70628,#70629,#70630,#70631,#70632,#70633,#70634,#70635,#70636,#70637,
#70638,#70639,#70640,#70641,#70642,#70643,#70644,#70645,#70646,#70647,#70648,
#70649,#70650,#70651,#70652,#70653,#70654,#70655,#70656,#70657,#70658,#70659,
#70660,#70661,#70662,#70663,#70664,#70665,#70666,#70667,#70668,#70669,#70670,
#70671,#70672,#70673,#70674,#70675,#70676,#70677,#70678,#70679,#70680,#70681,
#70682,#70683,#70684,#70685,#70686,#70687,#70688,#70689,#70690,#70691,#70692,
#70693,#70694,#70695,#70696,#70697,#70698,#70699,#70700,#70701,#70702,#70703,
#70704,#70705,#70706,#70707,#70708,#70709,#70710,#70711,#70712,#70713,#70714,
#70715,#70716,#70717,#70718,#70719,#70720,#70721,#70722,#70723,#70724,#70725,
#70726,#70727,#70728,#70729,#70730,#70731,#70732,#70733,#70734,#70735,#70736,
#70737,#70738,#70739,#70740,#70741,#70742,#70743,#70744,#70745,#70746,#70747,
#70748,#70749,#70750,#70751,#70752,#70753,#70754,#70755,#70756,#70757,#70758,
#70759,#70760,#70761,#70762,#70763,#70764,#70765,#70766,#70767,#70768,#70769,
#70770,#70771,#70772,#70773,#70774,#70775,#70776,#70777,#70778,#70779,#70780,
#70781,#70782,#70783,#70784,#70785,#70786,#70787,#70788,#70789,#70790,#70791,
#70792,#70793,#70794,#70795,#70796,#70797,#70798,#70799),.UNSPECIFIED.,
 .F.,.F.,(4,2,2,2,2,2,2,2,2,2,2,2,2,2,2,2,2,2,2,2,2,2,2,2,2,2,2,2,2,2,2,
2,2,2,2,2,2,2,2,2,2,2,2,2,2,2,2,2,2,2,2,2,2,2,2,2,2,2,2,2,2,2,2,2,2,2,2,
2,2,2,2,2,2,2,2,2,2,2,2,2,2,2,2,2,2,2,2,2,2,2,2,2,2,2,2,2,2,2,2,2,2,2,2,
2,2,2,2,2,2,2,4),(-1.2597871053314,-1.25887347369017,-1.25747165391834,
-1.25639225300539,-1.25518557366362,-1.25313941938559,-1.24508186513212,
-1.22990236286778,-1.19000532650871,-1.15896082754083,-1.15473920053375,
-1.15221921376362,-1.15028176133158,-1.14819920279464,-1.14490923784977,
-1.13423538145055,-1.11686367757923,-1.06815910703513,-1.06164421519791,
-1.04902104344771,-1.0467852565193,-1.0454018029575,-1.04432735582621,-1.04309581997592,
-1.04093743820442,-1.03142541094137,-0.982270896994583,-0.94707459333318,
-0.942778177758734,-0.940236518512811,-0.938295658716597,-0.936222328456378,
-0.93297399196045,-0.922667311552972,-0.906115527507918,-0.873263638508922,
-0.860347034121186,-0.83764215987386,-0.834788517686226,-0.833411718799653,
-0.832338022503596,-0.831102361020054,-0.828924860828711,-0.819134785946288,
-0.7702237455661,-0.735106029926622,-0.730811050487319,-0.728269945308957,
-0.726329338426539,-0.724256113342667,-0.721007597131434,-0.710697442888723,
-0.694137318817379,-0.661280543360498,-0.647507728098617,-0.640736120221123,
-0.638932715519826,-0.625194664212764,-0.622903217053436,-0.621518164924736,
-0.620441147562204,-0.619225301156506,-0.617137147897312,-0.608561829424292,
-0.591900724848428,-0.549983861062186,-0.522882171738444,-0.518758559277137,
-0.516267555254865,-0.514334899235427,-0.512240088120757,-0.508893246797823,
-0.497691736551139,-0.479107693233423,-0.436053004741267,-0.413736718190669,
-0.410895310730124,-0.409521024357598,-0.408447687297467,-0.407210628650563,
-0.405026318471844,-0.395132864872299,-0.346315929464636,-0.311232105982675,
-0.306938077712082,-0.304397417376839,-0.302457082306048,-0.300384081761896,
-0.297135779882849,-0.286825146569242,-0.270263150252942,-0.237926861129942,
-0.201815817541599,-0.198960598642569,-0.197583673275514,-0.196557139456272,
-0.195363769522401,-0.193380885957696,-0.190941232363002,-0.18598313874413,
-0.172433471217775,-0.149619114975562,-0.103071362503241,-0.0958751270226328,
-0.092958673276615,-0.0911568740503026,-0.0892033454969263,-0.0865388014388443,
-0.0803612544710696,-0.0537575033662972,-0.000629602941351068),
 .UNSPECIFIED.);
#757=B_SPLINE_CURVE_WITH_KNOTS('',3,(#70800,#70801,#70802,#70803,#70804,
#70805,#70806,#70807,#70808,#70809,#70810,#70811,#70812,#70813,#70814,#70815,
#70816,#70817,#70818,#70819,#70820,#70821,#70822,#70823),.UNSPECIFIED.,
 .F.,.F.,(4,2,2,2,2,2,2,2,2,2,2,4),(-2.667759750698,-2.65970368163532,-2.65534688392438,
-2.65393402192932,-2.65286686819766,-2.65183675354335,-2.65065694971661,
-2.64873191207764,-2.64266693400501,-2.64138504326144,-2.63358536386622,
-2.59350983441696),.UNSPECIFIED.);
#758=B_SPLINE_CURVE_WITH_KNOTS('',3,(#70829,#70830,#70831,#70832,#70833,
#70834,#70835,#70836,#70837,#70838,#70839,#70840,#70841),.UNSPECIFIED.,
 .F.,.F.,(4,3,3,3,4),(114.057240399931,114.163813791282,114.27025049183,
114.376547404602,114.406671945289),.UNSPECIFIED.);
#759=B_SPLINE_CURVE_WITH_KNOTS('',3,(#70842,#70843,#70844,#70845,#70846,
#70847,#70848,#70849,#70850,#70851),.UNSPECIFIED.,.F.,.F.,(4,1,1,1,1,1,
1,4),(114.406674973252,114.866191745616,115.865028195577,116.863864645539,
117.862701095501,118.861537545463,119.860373995425,120.339865638913),
 .UNSPECIFIED.);
#760=B_SPLINE_CURVE_WITH_KNOTS('',3,(#70852,#70853,#70854,#70855,#70856,
#70857,#70858,#70859,#70860,#70861,#70862,#70863,#70864,#70865,#70866,#70867,
#70868,#70869,#70870,#70871,#70872,#70873,#70874,#70875,#70876,#70877,#70878,
#70879,#70880,#70881,#70882,#70883,#70884,#70885,#70886,#70887,#70888,#70889,
#70890,#70891,#70892,#70893,#70894,#70895,#70896,#70897,#70898,#70899,#70900,
#70901,#70902,#70903,#70904,#70905,#70906,#70907,#70908,#70909,#70910,#70911,
#70912,#70913,#70914,#70915,#70916,#70917,#70918,#70919,#70920,#70921,#70922,
#70923,#70924,#70925,#70926,#70927,#70928,#70929,#70930,#70931,#70932,#70933,
#70934,#70935,#70936,#70937,#70938,#70939,#70940,#70941,#70942,#70943,#70944,
#70945,#70946,#70947,#70948,#70949,#70950,#70951,#70952,#70953,#70954,#70955,
#70956,#70957,#70958,#70959,#70960,#70961,#70962,#70963,#70964,#70965,#70966,
#70967,#70968,#70969,#70970,#70971,#70972,#70973,#70974,#70975,#70976,#70977,
#70978,#70979,#70980,#70981,#70982,#70983,#70984,#70985,#70986,#70987,#70988,
#70989,#70990,#70991,#70992,#70993,#70994,#70995,#70996,#70997,#70998,#70999,
#71000,#71001,#71002,#71003,#71004,#71005,#71006,#71007,#71008,#71009,#71010,
#71011,#71012,#71013,#71014,#71015,#71016,#71017,#71018,#71019,#71020,#71021,
#71022,#71023,#71024,#71025,#71026,#71027,#71028,#71029,#71030,#71031,#71032,
#71033,#71034,#71035,#71036,#71037,#71038,#71039,#71040,#71041,#71042,#71043,
#71044,#71045,#71046,#71047,#71048,#71049,#71050,#71051,#71052,#71053,#71054,
#71055,#71056,#71057,#71058,#71059,#71060,#71061,#71062,#71063,#71064,#71065,
#71066,#71067,#71068,#71069,#71070,#71071,#71072,#71073,#71074,#71075,#71076,
#71077,#71078,#71079,#71080,#71081,#71082,#71083,#71084,#71085,#71086,#71087,
#71088,#71089,#71090,#71091,#71092,#71093,#71094,#71095,#71096,#71097,#71098,
#71099,#71100,#71101,#71102,#71103,#71104,#71105,#71106,#71107,#71108,#71109,
#71110,#71111,#71112,#71113,#71114,#71115),.UNSPECIFIED.,.F.,.F.,(4,2,2,
2,2,2,2,2,2,2,2,2,2,2,2,2,2,2,2,2,2,2,2,2,2,2,2,2,2,2,2,2,2,2,2,2,2,2,2,
2,2,2,2,2,2,2,2,2,2,2,2,2,2,2,2,2,2,2,2,2,2,2,2,2,2,2,2,2,2,2,2,2,2,2,2,
2,2,2,2,2,2,2,2,2,2,2,2,2,2,2,2,2,2,2,2,2,2,2,2,2,2,2,2,2,2,2,2,2,2,2,2,
2,2,2,2,2,2,2,2,2,2,2,2,2,2,2,2,2,2,2,2,4),(-2.59350983441696,-2.58039355821006,
-2.56264877629364,-2.55181134345083,-2.54850310221189,-2.54641638655259,
-2.54448017492711,-2.54196904314671,-2.53777818827189,-2.508277658003,-2.46717253757524,
-2.45174120878521,-2.44632784540861,-2.44372939350055,-2.44162299355241,
-2.44041042587091,-2.44040731116854,-2.44040417763524,-2.44040102491068,
-2.440397852994,-2.44039466191649,-2.44039145130121,-2.44038822114729,-2.44038497129897,
-2.44038170150704,-2.44037841173811,-2.44037510156982,-2.44037177123605,
-2.44036843317822,-2.44036508059764,-2.44036170686419,-2.44035830040255,
-2.4393314385167,-2.43795394913262,-2.43509669186788,-2.39901740817715,
-2.36628980770353,-2.34379016539112,-2.33814477880076,-2.33557502850762,
-2.33363682488902,-2.3318096928843,-2.3292661005672,-2.3226142583808,-2.26691048442739,
-2.24278034575134,-2.23193867646507,-2.22969358600825,-2.22844309908252,
-2.22737115902849,-2.22601542419282,-2.22387090179953,-2.21285121490067,
-2.16159321935567,-2.13290046513907,-2.12646864493506,-2.12376024625422,
-2.12179859010036,-2.12000588793617,-2.11714053969733,-2.11025374837044,
-2.0572080144364,-2.03127863070266,-2.01996567469318,-2.01769283270307,
-2.01643632406596,-2.01536497154924,-2.01401730709105,-2.01139607875927,
-1.99536032524404,-1.99002589608921,-1.97547612193418,-1.94258372428966,
-1.92601689493743,-1.9157044252239,-1.91245540419634,-1.91038191733261,
-1.908441108381,-1.90589980181412,-1.90160465573686,-1.86648816611598,-1.81757147313822,
-1.80781339684992,-1.80563798745994,-1.80440272547343,-1.80332887745643,
-1.80195122229711,-1.79909354371259,-1.7631415572081,-1.73036511925745,
-1.7077923314465,-1.70213677580606,-1.69956499870042,-1.69762632517493,
-1.69579952824608,-1.69325765124335,-1.6866177528121,-1.63078270198163,
-1.59793943797146,-1.59439319603278,-1.59288897697062,-1.59179757900628,
-1.59077020803701,-1.58901999167604,-1.58424099456079,-1.54706883524457,
-1.49680343343329,-1.4904016602027,-1.48769817383609,-1.48573725673049,
-1.48394328737112,-1.4810716798851,-1.47414791125047,-1.42158311608298,
-1.39531119760009,-1.38391089336196,-1.38163289024548,-1.38037518312162,
-1.37930381140584,-1.37795739799209,-1.37534234651273,-1.35942301201897,
-1.35492117671423,-1.33435975724735,-1.2860094575818,-1.27886102805064,
-1.275952021756,-1.27415116971881,-1.2721957871066,-1.26952353577656,-1.2633045979713,
-1.25983685653957),.UNSPECIFIED.);
#761=B_SPLINE_CURVE_WITH_KNOTS('',3,(#71121,#71122,#71123,#71124,#71125,
#71126,#71127,#71128,#71129,#71130,#71131,#71132,#71133,#71134,#71135,#71136,
#71137,#71138,#71139,#71140),.UNSPECIFIED.,.F.,.F.,(4,2,2,2,2,2,2,2,2,4),
(-0.0747504723290347,-0.06102294006139,-0.0562870052721474,-0.0545435820400614,
-0.0535177062400768,-0.052425793662566,-0.0509174408111615,-0.0492296223280002,
-0.0462824121917821,-0.00062912049210774),.UNSPECIFIED.);
#762=B_SPLINE_CURVE_WITH_KNOTS('',3,(#71141,#71142,#71143,#71144,#71145,
#71146,#71147,#71148,#71149,#71150,#71151,#71152,#71153,#71154,#71155,#71156,
#71157,#71158,#71159,#71160,#71161,#71162,#71163,#71164,#71165,#71166,#71167,
#71168,#71169,#71170,#71171,#71172,#71173,#71174,#71175,#71176,#71177,#71178,
#71179,#71180,#71181,#71182,#71183,#71184,#71185,#71186,#71187,#71188,#71189,
#71190,#71191,#71192,#71193,#71194,#71195,#71196,#71197,#71198,#71199,#71200,
#71201,#71202,#71203,#71204,#71205,#71206,#71207,#71208,#71209,#71210,#71211,
#71212,#71213,#71214,#71215,#71216,#71217,#71218,#71219,#71220,#71221,#71222,
#71223,#71224,#71225,#71226,#71227,#71228,#71229,#71230,#71231,#71232,#71233,
#71234,#71235,#71236,#71237,#71238,#71239,#71240,#71241,#71242,#71243,#71244,
#71245,#71246,#71247,#71248,#71249,#71250,#71251,#71252,#71253,#71254,#71255,
#71256,#71257,#71258,#71259,#71260,#71261,#71262,#71263,#71264,#71265,#71266,
#71267,#71268,#71269,#71270,#71271,#71272,#71273,#71274,#71275,#71276,#71277,
#71278,#71279,#71280,#71281,#71282,#71283,#71284,#71285,#71286,#71287,#71288,
#71289,#71290,#71291,#71292,#71293,#71294,#71295,#71296,#71297,#71298,#71299,
#71300,#71301,#71302,#71303,#71304,#71305,#71306,#71307,#71308,#71309,#71310,
#71311,#71312,#71313,#71314,#71315,#71316,#71317,#71318,#71319,#71320,#71321),
 .UNSPECIFIED.,.F.,.F.,(4,3,3,3,3,3,3,3,3,3,3,3,3,3,3,3,3,3,3,3,3,3,3,3,
3,3,3,3,3,3,3,3,3,3,3,3,3,3,3,3,3,3,3,3,3,3,3,3,3,3,3,3,3,3,3,3,3,3,3,3,
4),(108.12348663811,108.225421296431,108.327291076164,108.429131491865,
108.530978014042,108.632930880402,108.734945943836,108.837130903885,108.873173045844,
108.976567782892,109.079809065007,109.182929030399,109.285983598608,109.389006806966,
109.492032649639,109.595165416417,109.698354507827,109.801726501209,109.872009495806,
109.975404232854,110.078645514969,110.181765480362,110.284820048571,110.387843256929,
110.490869099601,110.594001866379,110.69719095779,110.800562951171,110.870845945768,
110.974240682816,111.077481964931,111.180601930323,111.283656498532,111.38667970689,
111.489705549562,111.592838316341,111.69602740775,111.799399401132,111.86968239573,
111.973077132778,112.076318414893,112.179438380285,112.282492948494,112.385516156852,
112.488541999524,112.591674766302,112.694863857712,112.798235851094,112.868518845692,
112.97191358274,113.075154864856,113.178274830248,113.281329398457,113.384352606815,
113.487378449487,113.590511216266,113.693700307675,113.797072301057,113.867355295654,
113.974272639397,114.057240399931),.UNSPECIFIED.);
#763=B_SPLINE_CURVE_WITH_KNOTS('',3,(#71323,#71324,#71325,#71326,#71327,
#71328,#71329,#71330,#71331,#71332,#71333,#71334,#71335,#71336,#71337,#71338,
#71339,#71340,#71341,#71342,#71343,#71344,#71345,#71346,#71347,#71348,#71349,
#71350,#71351,#71352,#71353,#71354,#71355,#71356,#71357,#71358,#71359,#71360,
#71361,#71362,#71363,#71364,#71365,#71366,#71367,#71368,#71369,#71370,#71371,
#71372,#71373,#71374,#71375,#71376,#71377,#71378,#71379,#71380,#71381,#71382,
#71383,#71384,#71385,#71386,#71387,#71388,#71389,#71390,#71391,#71392,#71393,
#71394,#71395,#71396,#71397,#71398,#71399,#71400,#71401,#71402,#71403,#71404,
#71405,#71406,#71407,#71408,#71409,#71410,#71411,#71412,#71413,#71414,#71415,
#71416,#71417,#71418,#71419,#71420,#71421,#71422,#71423,#71424,#71425,#71426,
#71427,#71428,#71429,#71430,#71431,#71432,#71433,#71434,#71435,#71436,#71437,
#71438,#71439,#71440,#71441,#71442,#71443,#71444,#71445,#71446,#71447,#71448,
#71449,#71450,#71451,#71452,#71453,#71454,#71455,#71456,#71457,#71458,#71459,
#71460,#71461,#71462,#71463,#71464,#71465,#71466,#71467,#71468,#71469,#71470,
#71471,#71472,#71473,#71474,#71475,#71476,#71477,#71478,#71479,#71480,#71481,
#71482,#71483,#71484,#71485,#71486,#71487,#71488,#71489,#71490,#71491,#71492,
#71493,#71494,#71495,#71496,#71497,#71498,#71499,#71500,#71501,#71502,#71503,
#71504,#71505,#71506,#71507,#71508,#71509,#71510,#71511,#71512,#71513,#71514,
#71515,#71516,#71517,#71518,#71519,#71520,#71521,#71522,#71523,#71524,#71525,
#71526,#71527,#71528,#71529,#71530,#71531,#71532,#71533,#71534,#71535,#71536,
#71537,#71538),.UNSPECIFIED.,.F.,.F.,(4,2,2,2,2,2,2,2,2,2,2,2,2,2,2,2,2,
2,2,2,2,2,2,2,2,2,2,2,2,2,2,2,2,2,2,2,2,2,2,2,2,2,2,2,2,2,2,2,2,2,2,2,2,
2,2,2,2,2,2,2,2,2,2,2,2,2,2,2,2,2,2,2,2,2,2,2,2,2,2,2,2,2,2,2,2,2,2,2,2,
2,2,2,2,2,2,2,2,2,2,2,2,2,2,2,2,2,2,4),(-1.25983685653957,-1.2363744642156,
-1.1958522808464,-1.17286244743288,-1.17000730397881,-1.1686301350547,-1.16755631675952,
-1.16632070299258,-1.16414373713736,-1.15436352877039,-1.10543890910008,
-1.07031498195434,-1.06601956755178,-1.06347821694089,-1.06153742948484,
-1.05946401813863,-1.05621522396254,-1.04590430459282,-1.02934306292726,
-0.996483599797937,-0.982742350350651,-0.975892406261312,-0.975578869095316,
-0.970007428554194,-0.959995609972315,-0.95791662584862,-0.95658099402074,
-0.955510371164392,-0.954244384698694,-0.951927683705647,-0.93981815029731,
-0.887088451149664,-0.876442966387558,-0.857376854613134,-0.853613472599162,
-0.851204245472093,-0.849286724526475,-0.84712543589334,-0.84347871972519,
-0.82905929736825,-0.778655873958179,-0.748982408997737,-0.746068394828556,
-0.744679858434579,-0.743605047970853,-0.74237710627218,-0.740234444215214,
-0.730939049319063,-0.712090773430482,-0.671644321247857,-0.659367695302661,
-0.644790071409047,-0.641004701799636,-0.638790609095994,-0.636878637071265,
-0.634543345405316,-0.630091033724474,-0.599061232992771,-0.55110113604688,
-0.536504623440271,-0.534172221810807,-0.532775089796961,-0.531696456253336,
-0.530487467068014,-0.528430413770078,-0.520240202580606,-0.504687456620258,
-0.463145707466814,-0.434210277073354,-0.430031719140513,-0.427524515873234,
-0.425589300708636,-0.423501647145032,-0.420187609892399,-0.409292201123117,
-0.391415722944751,-0.340792529831821,-0.324645112217682,-0.322019930743042,
-0.320671450254275,-0.319600087051743,-0.318344310563733,-0.316074671633414,
-0.304816503315135,-0.27909797100561,-0.225709947894199,-0.218851080843394,
-0.216045375303452,-0.21408523103112,-0.212146031668788,-0.210185549506391,
-0.205109051866494,-0.163990473157819,-0.115019701111411,-0.110791357719309,
-0.109127238460932,-0.108116689967441,-0.107013221161621,-0.105442050010592,
-0.10148989773849,-0.0819023791992277,-0.0267279003317656,-0.0187639987473031,
-0.00802108770802645,-0.00466632887790808,-0.0025813007720164,-0.00128118372687951,
-0.000628942024347663),.UNSPECIFIED.);
#764=B_SPLINE_CURVE_WITH_KNOTS('',3,(#71539,#71540,#71541,#71542,#71543,
#71544,#71545,#71546,#71547,#71548,#71549,#71550,#71551),.UNSPECIFIED.,
 .F.,.F.,(4,3,3,3,4),(-104.372003947921,-104.263735348717,-104.155311094171,
-104.046631225627,-104.022525439493),.UNSPECIFIED.);
#765=B_SPLINE_CURVE_WITH_KNOTS('',3,(#71556,#71557,#71558,#71559,#71560,
#71561,#71562,#71563,#71564,#71565,#71566,#71567,#71568,#71569,#71570,#71571,
#71572,#71573,#71574,#71575,#71576,#71577,#71578,#71579,#71580,#71581,#71582,
#71583,#71584,#71585,#71586,#71587,#71588,#71589,#71590,#71591,#71592,#71593,
#71594,#71595,#71596,#71597,#71598,#71599,#71600,#71601,#71602,#71603,#71604,
#71605,#71606,#71607,#71608,#71609,#71610,#71611,#71612,#71613,#71614,#71615,
#71616,#71617,#71618,#71619,#71620,#71621,#71622,#71623,#71624,#71625,#71626,
#71627,#71628,#71629,#71630,#71631,#71632,#71633,#71634,#71635,#71636,#71637,
#71638,#71639,#71640,#71641,#71642,#71643,#71644,#71645,#71646,#71647,#71648,
#71649,#71650,#71651,#71652,#71653,#71654,#71655,#71656,#71657,#71658,#71659,
#71660,#71661,#71662,#71663,#71664,#71665,#71666,#71667,#71668,#71669,#71670,
#71671,#71672,#71673,#71674,#71675,#71676,#71677,#71678,#71679,#71680,#71681,
#71682,#71683,#71684,#71685,#71686,#71687,#71688,#71689,#71690,#71691,#71692,
#71693,#71694,#71695,#71696,#71697,#71698,#71699,#71700,#71701,#71702,#71703,
#71704,#71705,#71706,#71707,#71708,#71709,#71710,#71711,#71712,#71713,#71714,
#71715,#71716,#71717,#71718,#71719,#71720,#71721,#71722,#71723,#71724,#71725,
#71726,#71727,#71728,#71729,#71730,#71731,#71732,#71733,#71734,#71735,#71736,
#71737,#71738,#71739,#71740,#71741,#71742,#71743,#71744,#71745,#71746,#71747,
#71748,#71749,#71750,#71751,#71752,#71753,#71754,#71755,#71756,#71757,#71758,
#71759,#71760,#71761,#71762,#71763,#71764,#71765,#71766,#71767,#71768,#71769,
#71770,#71771,#71772,#71773,#71774,#71775),.UNSPECIFIED.,.F.,.F.,(4,2,2,
2,2,2,2,2,2,2,2,2,2,2,2,2,2,2,2,2,2,2,2,2,2,2,2,2,2,2,2,2,2,2,2,2,2,2,2,
2,2,2,2,2,2,2,2,2,2,2,2,2,2,2,2,2,2,2,2,2,2,2,2,2,2,2,2,2,2,2,2,2,2,2,2,
2,2,2,2,2,2,2,2,2,2,2,2,2,2,2,2,2,2,2,2,2,2,2,2,2,2,2,2,2,2,2,2,2,2,4),
(-1.40835488213934,-1.37307257504326,-1.3339620916423,-1.33297753375494,
-1.32826981672132,-1.32653033786744,-1.32550501098063,-1.32441218079595,
-1.3229001105707,-1.31930847814899,-1.28016936056107,-1.23134352087163,
-1.22421237079347,-1.22130613403507,-1.21950569928475,-1.21754974510166,
-1.21487486720901,-1.20864139691479,-1.18159511324464,-1.14086737517617,
-1.11820862392735,-1.11535573440555,-1.11397894781042,-1.11290509602158,
-1.11166906909407,-1.10949047827219,-1.09968808257067,-1.05077792159248,
-1.01565733517771,-1.01136168157912,-1.00882016567859,-1.00687923830419,
-1.00480566420508,-1.0015565873001,-0.991244536980126,-0.97468125662034,
-0.941818686606974,-0.928011069381496,-0.921314234906394,-0.905865126248385,
-0.903497163203982,-0.902089567451067,-0.90100940943892,-0.899805967893813,
-0.897774199595886,-0.889884364618558,-0.875168237518788,-0.846104164476846,
-0.803698149152738,-0.799404687404572,-0.796863863883766,-0.794923117079057,
-0.792849398195703,-0.78959938910586,-0.77927842973857,-0.762695175853825,
-0.72981688302325,-0.714515615030122,-0.709793792620108,-0.693941565195866,
-0.691328752708666,-0.689982895750886,-0.688911651900714,-0.687653734986515,
-0.685374423961639,-0.673948890377299,-0.647572514827088,-0.595122290095803,
-0.588188793898627,-0.585315750368055,-0.583521643686318,-0.581561191357775,
-0.578859462281914,-0.572467091064481,-0.526046239066656,-0.484947967846882,
-0.480263104017284,-0.478527321164545,-0.477502870249328,-0.476409866291896,
-0.47489574639119,-0.471290890966269,-0.432950716683481,-0.38331732109614,
-0.376221647411313,-0.373321726606491,-0.371522734313794,-0.369566391628544,
-0.366887452921059,-0.360806545645847,-0.352445678521271,-0.301551117062902,
-0.270313242225972,-0.26740127492247,-0.266013098083552,-0.264938282463211,
-0.263710017758472,-0.261566049314298,-0.252414971273518,-0.20366644528238,
-0.167704290585459,-0.162982356767182,-0.160559558506669,-0.158640677246885,
-0.15648780368554,-0.154258048649232,-0.146612097675678,-0.121083045893507,
-0.100337618335071,-0.0747504723290347),.UNSPECIFIED.);
#766=B_SPLINE_CURVE_WITH_KNOTS('',3,(#71777,#71778,#71779,#71780,#71781,
#71782,#71783,#71784,#71785,#71786,#71787,#71788,#71789,#71790,#71791,#71792,
#71793,#71794,#71795,#71796,#71797,#71798,#71799,#71800,#71801,#71802,#71803,
#71804,#71805,#71806,#71807,#71808,#71809,#71810,#71811,#71812,#71813,#71814,
#71815,#71816,#71817,#71818,#71819,#71820,#71821,#71822,#71823,#71824,#71825,
#71826,#71827,#71828,#71829,#71830,#71831,#71832,#71833,#71834,#71835,#71836,
#71837,#71838,#71839,#71840,#71841,#71842,#71843,#71844,#71845,#71846,#71847,
#71848,#71849,#71850,#71851,#71852,#71853,#71854,#71855,#71856,#71857,#71858,
#71859,#71860,#71861,#71862,#71863,#71864,#71865,#71866,#71867,#71868,#71869,
#71870,#71871,#71872,#71873,#71874,#71875,#71876,#71877,#71878,#71879,#71880,
#71881,#71882,#71883,#71884,#71885,#71886,#71887,#71888,#71889,#71890,#71891,
#71892,#71893,#71894,#71895,#71896,#71897,#71898,#71899,#71900,#71901,#71902,
#71903,#71904,#71905,#71906,#71907,#71908,#71909,#71910,#71911,#71912,#71913,
#71914,#71915,#71916,#71917,#71918,#71919,#71920,#71921,#71922,#71923,#71924,
#71925,#71926,#71927,#71928,#71929,#71930,#71931,#71932,#71933,#71934,#71935,
#71936,#71937,#71938,#71939,#71940,#71941,#71942,#71943,#71944,#71945,#71946,
#71947,#71948,#71949,#71950,#71951,#71952,#71953,#71954,#71955,#71956,#71957),
 .UNSPECIFIED.,.F.,.F.,(4,3,3,3,3,3,3,3,3,3,3,3,3,3,3,3,3,3,3,3,3,3,3,3,
3,3,3,3,3,3,3,3,3,3,3,3,3,3,3,3,3,3,3,3,3,3,3,3,3,3,3,3,3,3,3,3,3,3,3,3,
4),(-104.022525439493,-103.9135142963,-103.878990796035,-103.775596058987,
-103.672354776872,-103.569234811479,-103.46618024327,-103.363157034913,
-103.26013119224,-103.156998425462,-103.053809334052,-102.95043734067,-102.880154346073,
-102.776759609025,-102.67351832691,-102.570398361518,-102.467343793309,
-102.364320584951,-102.261294742278,-102.1581619755,-102.054972884091,-101.951600890709,
-101.881317896111,-101.777923159063,-101.674681876948,-101.571561911556,
-101.468507343347,-101.365484134989,-101.262458292316,-101.159325525538,
-101.056136434128,-100.952764440747,-100.882481446149,-100.779086709101,
-100.675845426986,-100.572725461594,-100.469670893385,-100.366647685027,
-100.263621842355,-100.160489075577,-100.057299984167,-99.9539279907856,
-99.8836449961874,-99.7802502591395,-99.6770089770246,-99.5738890116324,
-99.4708344434235,-99.3678112350658,-99.2647853923933,-99.1616526256152,
-99.0584635342055,-98.9550915408238,-98.8848085462256,-98.7829332776308,
-98.6811932844012,-98.579552537636,-98.4779751499172,-98.3763829554482,
-98.2747883682234,-98.1730805291731,-98.0888188327757),.UNSPECIFIED.);
#767=B_SPLINE_CURVE_WITH_KNOTS('',3,(#71958,#71959,#71960,#71961,#71962),
 .UNSPECIFIED.,.F.,.F.,(4,1,4),(-98.0888186411165,-97.8859720962637,-97.7379483049134),
 .UNSPECIFIED.);
#768=B_SPLINE_CURVE_WITH_KNOTS('',3,(#71968,#71969,#71970,#71971,#71972,
#71973,#71974,#71975,#71976,#71977,#71978,#71979,#71980,#71981,#71982,#71983,
#71984,#71985,#71986,#71987,#71988,#71989),.UNSPECIFIED.,.F.,.F.,(4,2,2,
2,2,2,2,2,2,2,4),(-0.0750517038529886,-0.0634020312911012,-0.0604357711843507,
-0.0436144622418274,-0.0399995473077869,-0.0376361122359522,-0.0357225144891595,
-0.0339209951592301,-0.0317709072211862,-0.0286342749703805,-0.000628476579351984),
 .UNSPECIFIED.);
#769=B_SPLINE_CURVE_WITH_KNOTS('',3,(#71990,#71991,#71992,#71993,#71994,
#71995,#71996,#71997,#71998,#71999,#72000,#72001,#72002,#72003,#72004,#72005,
#72006,#72007,#72008,#72009,#72010,#72011,#72012,#72013,#72014,#72015,#72016,
#72017,#72018,#72019,#72020,#72021,#72022,#72023,#72024,#72025,#72026,#72027,
#72028,#72029,#72030,#72031,#72032,#72033,#72034,#72035,#72036,#72037,#72038,
#72039,#72040,#72041,#72042,#72043,#72044,#72045,#72046,#72047,#72048,#72049,
#72050,#72051,#72052,#72053,#72054,#72055,#72056,#72057,#72058,#72059,#72060,
#72061,#72062,#72063,#72064,#72065,#72066,#72067,#72068,#72069,#72070,#72071,
#72072,#72073,#72074,#72075,#72076,#72077,#72078,#72079,#72080,#72081,#72082,
#72083,#72084,#72085,#72086,#72087,#72088,#72089,#72090,#72091,#72092,#72093,
#72094,#72095,#72096,#72097,#72098,#72099,#72100,#72101,#72102,#72103,#72104,
#72105,#72106,#72107,#72108,#72109,#72110,#72111,#72112,#72113,#72114,#72115,
#72116,#72117,#72118,#72119,#72120,#72121,#72122,#72123,#72124,#72125,#72126,
#72127,#72128,#72129,#72130,#72131,#72132,#72133,#72134,#72135,#72136,#72137,
#72138,#72139,#72140,#72141,#72142,#72143,#72144,#72145,#72146,#72147,#72148,
#72149,#72150,#72151,#72152,#72153,#72154,#72155,#72156,#72157,#72158,#72159,
#72160,#72161,#72162,#72163,#72164,#72165,#72166,#72167,#72168,#72169,#72170,
#72171,#72172,#72173,#72174,#72175,#72176,#72177,#72178,#72179,#72180,#72181,
#72182,#72183,#72184,#72185,#72186,#72187,#72188,#72189,#72190,#72191,#72192,
#72193,#72194,#72195,#72196,#72197,#72198,#72199,#72200,#72201,#72202,#72203,
#72204,#72205,#72206,#72207,#72208,#72209,#72210,#72211,#72212,#72213),
 .UNSPECIFIED.,.F.,.F.,(4,2,2,2,2,2,2,2,2,2,2,2,2,2,2,2,2,2,2,2,2,2,2,2,
2,2,2,2,2,2,2,2,2,2,2,2,2,2,2,2,2,2,2,2,2,2,2,2,2,2,2,2,2,2,2,2,2,2,2,2,
2,2,2,2,2,2,2,2,2,2,2,2,2,2,2,2,2,2,2,2,2,2,2,2,2,2,2,2,2,2,2,2,2,2,2,2,
2,2,2,2,2,2,2,2,2,2,2,2,2,2,2,4),(-2.66756143460973,-2.63526158114188,-2.61196230848377,
-2.60134680143366,-2.59911541518788,-2.59786784425495,-2.59679548087336,
-2.59543544972892,-2.59275695546045,-2.57521180506395,-2.56873788357839,
-2.52873913767827,-2.50908323364963,-2.50137439649208,-2.49567141392468,
-2.4930937964052,-2.49114560662755,-2.48933460017414,-2.48637121157221,
-2.47890392946452,-2.43049268194267,-2.39142719262711,-2.38785262315977,
-2.38634352320541,-2.38525126065573,-2.38422520908087,-2.38248181364631,
-2.37774784605682,-2.33778536583976,-2.29024389770352,-2.28384709393534,
-2.28114439637311,-2.27918357379278,-2.27738936151038,-2.27451664630728,
-2.26758649178128,-2.21511242539049,-2.18877416132953,-2.17735697994162,
-2.17507796411341,-2.17382001241067,-2.17274862275564,-2.17140242886039,
-2.16878851328827,-2.15290786883536,-2.14823494534728,-2.1076598964018,
-2.07837184499827,-2.07186899357031,-2.0691483656054,-2.0671842174186,-2.06539359761044,
-2.06254101658788,-2.05573352895158,-2.00168838114947,-1.97643617187404,
-1.96529679649396,-1.96303373522922,-1.96177921650124,-1.96070747757425,
-1.95935666877263,-1.95672147233761,-1.94033577505885,-1.93130037954646,
-1.89233437778975,-1.86585523809554,-1.85969238780467,-1.85702970978129,
-1.85507586639276,-1.85327259845599,-1.85035112192351,-1.8431294203899,
-1.79878562848196,-1.78472886360406,-1.76327485952442,-1.75318358713273,
-1.75098562471165,-1.74974532232207,-1.74867201891863,-1.74730146858214,
-1.74510858042782,-1.73333797761026,-1.72962678752198,-1.72236562682105,
-1.67901010237693,-1.66042269618648,-1.64921988866115,-1.64587222689119,
-1.64377681315624,-1.64184354124563,-1.63935166085027,-1.63522644810675,
-1.60809059376719,-1.56616640321535,-1.54954738484282,-1.54098479943008,
-1.53889724862778,-1.53768130974134,-1.53660391771465,-1.53521799319194,
-1.53292428769805,-1.51915035535241,-1.50784475531045,-1.46844818339477,
-1.4418753908946,-1.43570088024064,-1.43303617244619,-1.43108197182575,
-1.42927916916287,-1.42636022261411,-1.41915355869009,-1.40835488213934),
 .UNSPECIFIED.);
#770=B_SPLINE_CURVE_WITH_KNOTS('',3,(#72215,#72216,#72217,#72218,#72219,
#72220,#72221,#72222,#72223,#72224),.UNSPECIFIED.,.F.,.F.,(4,1,1,1,1,1,
1,4),(-97.7379483049134,-96.8871356463018,-95.88829919634,-94.8894627463781,
-93.8906262964162,-92.8917898464543,-91.8929533964925,-91.8056333339369),
 .UNSPECIFIED.);
#771=B_SPLINE_CURVE_WITH_KNOTS('',3,(#72225,#72226,#72227,#72228,#72229,
#72230,#72231,#72232),.UNSPECIFIED.,.F.,.F.,(4,2,2,4),(-2.66774030490623,
-2.61554842952445,-2.59714695246637,-2.59330484294858),.UNSPECIFIED.);
#772=B_SPLINE_CURVE_WITH_KNOTS('',3,(#72237,#72238,#72239,#72240,#72241,
#72242,#72243,#72244,#72245,#72246,#72247,#72248,#72249,#72250,#72251,#72252,
#72253,#72254,#72255,#72256,#72257,#72258,#72259,#72260,#72261,#72262,#72263,
#72264,#72265,#72266,#72267,#72268,#72269,#72270,#72271,#72272,#72273,#72274,
#72275,#72276,#72277,#72278,#72279,#72280,#72281,#72282,#72283,#72284,#72285,
#72286,#72287,#72288,#72289,#72290,#72291,#72292,#72293,#72294,#72295,#72296,
#72297,#72298,#72299,#72300,#72301,#72302,#72303,#72304,#72305,#72306,#72307,
#72308,#72309,#72310,#72311,#72312,#72313,#72314,#72315,#72316,#72317,#72318,
#72319,#72320,#72321,#72322,#72323,#72324,#72325,#72326,#72327,#72328,#72329,
#72330,#72331,#72332,#72333,#72334,#72335,#72336,#72337,#72338,#72339,#72340,
#72341,#72342,#72343,#72344,#72345,#72346,#72347,#72348,#72349,#72350,#72351,
#72352,#72353,#72354,#72355,#72356,#72357,#72358,#72359,#72360,#72361,#72362,
#72363,#72364,#72365,#72366,#72367,#72368,#72369,#72370,#72371,#72372,#72373,
#72374,#72375,#72376,#72377,#72378,#72379,#72380,#72381,#72382,#72383,#72384,
#72385,#72386,#72387,#72388,#72389,#72390,#72391,#72392,#72393,#72394,#72395,
#72396,#72397,#72398,#72399,#72400,#72401,#72402,#72403,#72404,#72405,#72406,
#72407,#72408,#72409,#72410,#72411,#72412,#72413,#72414,#72415,#72416,#72417,
#72418,#72419,#72420,#72421,#72422,#72423,#72424,#72425,#72426,#72427,#72428,
#72429,#72430,#72431,#72432,#72433,#72434,#72435,#72436,#72437,#72438,#72439,
#72440,#72441,#72442,#72443,#72444,#72445,#72446,#72447,#72448,#72449,#72450,
#72451,#72452),.UNSPECIFIED.,.F.,.F.,(4,2,2,2,2,2,2,2,2,2,2,2,2,2,2,2,2,
2,2,2,2,2,2,2,2,2,2,2,2,2,2,2,2,2,2,2,2,2,2,2,2,2,2,2,2,2,2,2,2,2,2,2,2,
2,2,2,2,2,2,2,2,2,2,2,2,2,2,2,2,2,2,2,2,2,2,2,2,2,2,2,2,2,2,2,2,2,2,2,2,
2,2,2,2,2,2,2,2,2,2,2,2,2,2,2,2,2,2,4),(-1.40856908540218,-1.37753522697878,
-1.33437646265475,-1.31573881175565,-1.31200609447521,-1.3096061864511,
-1.30768941851849,-1.30552186708829,-1.30184727203203,-1.2870843685882,
-1.25915934386313,-1.20936241991539,-1.20515946999307,-1.20349949633772,
-1.20248970435662,-1.20138546249729,-1.19981047693733,-1.19583457286336,
-1.17602191091469,-1.14710912276,-1.10479019933331,-1.10049508706726,-1.09795384795708,
-1.09601310691878,-1.09393970760558,-1.0906908538647,-1.08037908431328,
-1.06381584829322,-1.03095508345967,-1.01703053161134,-1.01060083943746,
-0.995017829819212,-0.992416282823265,-0.991072895883222,-0.990001854157967,
-0.988742123099013,-0.986454275545898,-0.974875690663942,-0.947884200897821,
-0.896303812276763,-0.889312873156469,-0.886430427292855,-0.88463466695291,
-0.882675776730312,-0.879982340662421,-0.873638322814003,-0.845680030525046,
-0.799188271842068,-0.783069666423301,-0.78044234287599,-0.779093421705149,
-0.778022054296434,-0.776766673285566,-0.77449876366209,-0.763269746460913,
-0.737664174487258,-0.684114700678137,-0.677265839950885,-0.674406855721565,
-0.672615400618229,-0.670652911279771,-0.667939314949484,-0.661475881210283,
-0.607416520889947,-0.571354708571906,-0.568495766685227,-0.567117978027443,
-0.566044245810071,-0.564809373611564,-0.562635250243668,-0.552893181014568,
-0.503945162920013,-0.468810091673628,-0.464518828287601,-0.461978880853651,
-0.460038558400026,-0.457965055434286,-0.454714888497141,-0.444389237321866,
-0.427794453298269,-0.371095860345277,-0.358711505310279,-0.356488685664063,
-0.355109269256772,-0.35403539081567,-0.352801615436594,-0.350632439144015,
-0.340961945140005,-0.291953827328591,-0.256811972815142,-0.252513674847289,
-0.249971703843863,-0.248031067492687,-0.24624041893856,-0.243302997727772,
-0.235328228390283,-0.223523979421678,-0.190998868263142,-0.150078454373832,
-0.145387647649334,-0.143651117531566,-0.142626623837441,-0.141533912861887,
-0.140020751969381,-0.136420736347178,-0.0985299881454376,-0.0757357797478958,
-0.0750517038529886),.UNSPECIFIED.);
#773=B_SPLINE_CURVE_WITH_KNOTS('',3,(#72453,#72454,#72455,#72456,#72457,
#72458,#72459,#72460,#72461,#72462,#72463,#72464,#72465,#72466,#72467,#72468,
#72469,#72470,#72471,#72472,#72473,#72474,#72475,#72476,#72477,#72478,#72479,
#72480,#72481,#72482,#72483,#72484,#72485,#72486,#72487,#72488,#72489,#72490,
#72491,#72492,#72493,#72494,#72495,#72496,#72497,#72498,#72499,#72500,#72501,
#72502,#72503,#72504,#72505,#72506,#72507,#72508,#72509,#72510,#72511,#72512,
#72513,#72514,#72515,#72516,#72517,#72518,#72519,#72520,#72521,#72522,#72523,
#72524,#72525,#72526,#72527,#72528,#72529,#72530,#72531,#72532,#72533,#72534,
#72535,#72536,#72537,#72538,#72539,#72540,#72541,#72542,#72543,#72544,#72545,
#72546,#72547,#72548,#72549,#72550,#72551,#72552,#72553,#72554,#72555,#72556,
#72557,#72558,#72559,#72560,#72561,#72562,#72563,#72564,#72565,#72566,#72567,
#72568,#72569,#72570,#72571,#72572,#72573,#72574,#72575,#72576,#72577,#72578,
#72579,#72580,#72581,#72582,#72583,#72584,#72585,#72586,#72587,#72588,#72589,
#72590,#72591,#72592,#72593,#72594,#72595,#72596,#72597,#72598,#72599,#72600,
#72601,#72602,#72603,#72604,#72605,#72606,#72607,#72608,#72609,#72610,#72611,
#72612,#72613,#72614,#72615,#72616,#72617,#72618,#72619,#72620,#72621,#72622,
#72623,#72624,#72625,#72626,#72627,#72628,#72629,#72630,#72631,#72632,#72633,
#72634,#72635,#72636,#72637,#72638,#72639,#72640,#72641,#72642,#72643,#72644,
#72645,#72646,#72647,#72648,#72649,#72650,#72651,#72652,#72653,#72654,#72655,
#72656,#72657,#72658,#72659,#72660,#72661,#72662,#72663,#72664,#72665,#72666,
#72667,#72668,#72669,#72670,#72671,#72672,#72673,#72674,#72675,#72676,#72677,
#72678,#72679,#72680,#72681,#72682,#72683,#72684,#72685,#72686,#72687,#72688,
#72689,#72690,#72691,#72692,#72693,#72694,#72695,#72696,#72697,#72698,#72699,
#72700,#72701,#72702,#72703,#72704,#72705,#72706,#72707,#72708,#72709,#72710,
#72711,#72712,#72713,#72714,#72715,#72716,#72717,#72718,#72719,#72720,#72721,
#72722,#72723,#72724,#72725,#72726,#72727,#72728,#72729,#72730,#72731,#72732,
#72733,#72734,#72735,#72736,#72737,#72738,#72739,#72740,#72741,#72742),
 .UNSPECIFIED.,.F.,.F.,(4,2,2,2,2,2,2,2,2,2,2,2,2,2,2,2,2,2,2,2,2,2,2,2,
2,2,2,2,2,2,2,2,2,2,2,2,2,2,2,2,2,2,2,2,2,2,2,2,2,2,2,2,2,2,2,2,2,2,2,2,
2,2,2,2,2,2,2,2,2,2,2,2,2,2,2,2,2,2,2,2,2,2,2,2,2,2,2,2,2,2,2,2,2,2,2,2,
2,2,2,2,2,2,2,2,2,2,2,2,2,2,2,2,2,2,2,2,2,2,2,2,2,2,2,2,2,2,2,2,2,2,2,2,
2,2,2,2,2,2,2,2,2,2,2,2,4),(-2.59330484294858,-2.58602528648615,-2.58268708564519,
-2.58059427506186,-2.57866114609222,-2.57616628761683,-2.57202929296363,
-2.54438681825075,-2.50209974648873,-2.48614458575997,-2.48061017196621,
-2.47797051539189,-2.47585511611322,-2.47463186447299,-2.47462831875154,
-2.47462475941621,-2.47462118639474,-2.47461759969858,-2.47461399899299,
-2.47461010811779,-2.47460614934466,-2.47460212124373,-2.47459802244419,
-2.47459385135599,-2.47458960644169,-2.47458528604957,-2.47458088858814,
-2.47457641235878,-2.47457185554549,-2.47456721633684,-2.47456249317495,
-2.47455768398931,-2.47455278693299,-2.47454780001297,-2.47454272104155,
-2.47453754790565,-2.4745322783669,-2.47345441286973,-2.47206186854742,
-2.46974466039954,-2.4554939036522,-2.45395997197966,-2.40802155766746,
-2.37916109038657,-2.37270998665603,-2.36999869161699,-2.3680368288707,
-2.36624523708514,-2.36338448544629,-2.35652334896222,-2.30318068000754,
-2.277470815958,-2.2662150159399,-2.26394582030786,-2.26269026979525,-2.26161909125403,
-2.26027082644707,-2.25764601760577,-2.24150091212544,-2.24101583413295,
-2.1912284482388,-2.16646318981933,-2.16051888163591,-2.15789537647367,
-2.15594889602381,-2.15413717743174,-2.15165157738876,-2.14535272088737,
-2.08663824047158,-2.06442962816323,-2.05412172347329,-2.05191024628017,
-2.05066726634226,-2.04959475679824,-2.04822924812027,-2.04605211190154,
-2.03448401034164,-2.03055853187892,-2.02328262038887,-2.00971921905664,
-1.97684352417414,-1.96029246488461,-1.94998765821279,-1.9467399055131,
-1.94466695264969,-1.94272645003395,-1.94018526537915,-1.93588969949699,
-1.90068511608129,-1.85146887356543,-1.84207165134789,-1.83992175857942,
-1.83869225630838,-1.8376177652025,-1.83623185099467,-1.83333112984071,
-1.80641914775787,-1.78860930819631,-1.74316008080986,-1.73677802729641,
-1.73407817692694,-1.73211818365603,-1.73032387676618,-1.72744914555655,
-1.72050450426299,-1.66826227906386,-1.64177462558227,-1.63032094645971,
-1.6280402111505,-1.62678205006324,-1.62571092940103,-1.62436564187795,
-1.62225506102581,-1.61176546417713,-1.60669564299256,-1.60640905281637,
-1.6050069692956,-1.59754472576318,-1.58574645830924,-1.5528830398556,-1.53634929533727,
-1.52605201131508,-1.52280489426815,-1.52073192976694,-1.51879112296061,
-1.5162491166074,-1.51195121246868,-1.47659221344915,-1.42743063198728,
-1.41811521441628,-1.41597103124672,-1.41474270437563,-1.4136678793923,
-1.41227973920362,-1.40936803809381,-1.37753527998185,-1.33437651320211,
-1.31573886100134,-1.31200614340079,-1.30960623516013,-1.30768946704697,
-1.30552191540457,-1.30184731996868,-1.28708441470362,-1.25997088998495),
 .UNSPECIFIED.);
#774=B_SPLINE_CURVE_WITH_KNOTS('',3,(#72748,#72749,#72750,#72751,#72752),
 .UNSPECIFIED.,.F.,.F.,(4,1,4),(82.6397395021165,82.9034253468356,82.9907454093913),
 .UNSPECIFIED.);
#775=B_SPLINE_CURVE_WITH_KNOTS('',3,(#72753,#72754,#72755,#72756,#72757,
#72758,#72759,#72760,#72761,#72762,#72763,#72764,#72765,#72766,#72767,#72768,
#72769,#72770,#72771,#72772,#72773,#72774,#72775,#72776,#72777,#72778,#72779,
#72780,#72781,#72782,#72783,#72784,#72785,#72786,#72787,#72788,#72789,#72790,
#72791,#72792,#72793,#72794,#72795,#72796,#72797,#72798,#72799,#72800,#72801,
#72802,#72803,#72804,#72805,#72806,#72807,#72808,#72809,#72810,#72811,#72812,
#72813,#72814,#72815,#72816,#72817,#72818,#72819,#72820,#72821,#72822,#72823,
#72824,#72825,#72826,#72827,#72828,#72829,#72830,#72831,#72832,#72833,#72834,
#72835,#72836,#72837,#72838,#72839,#72840,#72841,#72842,#72843,#72844,#72845,
#72846,#72847,#72848,#72849,#72850,#72851,#72852,#72853,#72854,#72855,#72856,
#72857,#72858,#72859,#72860,#72861,#72862,#72863,#72864,#72865,#72866,#72867,
#72868,#72869,#72870,#72871,#72872,#72873,#72874,#72875,#72876,#72877,#72878,
#72879,#72880,#72881,#72882,#72883,#72884,#72885,#72886,#72887,#72888,#72889,
#72890,#72891,#72892,#72893,#72894,#72895,#72896,#72897,#72898,#72899,#72900,
#72901,#72902,#72903,#72904,#72905,#72906,#72907,#72908,#72909,#72910,#72911,
#72912,#72913,#72914,#72915,#72916,#72917,#72918,#72919,#72920,#72921,#72922,
#72923,#72924,#72925,#72926,#72927,#72928,#72929,#72930,#72931,#72932,#72933,
#72934,#72935,#72936,#72937,#72938,#72939,#72940,#72941,#72942,#72943,#72944,
#72945,#72946,#72947,#72948,#72949,#72950,#72951,#72952,#72953,#72954,#72955,
#72956,#72957,#72958,#72959,#72960,#72961,#72962,#72963,#72964,#72965,#72966,
#72967,#72968,#72969,#72970,#72971,#72972,#72973,#72974,#72975,#72976,#72977,
#72978,#72979,#72980,#72981,#72982,#72983,#72984,#72985,#72986,#72987,#72988,
#72989,#72990,#72991,#72992,#72993,#72994,#72995,#72996,#72997,#72998,#72999,
#73000,#73001,#73002,#73003,#73004,#73005,#73006,#73007,#73008,#73009,#73010),
 .UNSPECIFIED.,.F.,.F.,(4,2,2,2,2,2,2,2,2,2,2,2,2,2,2,2,2,2,2,2,2,2,2,2,
2,2,2,2,2,2,2,2,2,2,2,2,2,2,2,2,2,2,2,2,2,2,2,2,2,2,2,2,2,2,2,2,2,2,2,2,
2,2,2,2,2,2,2,2,2,2,2,2,2,2,2,2,2,2,2,2,2,2,2,2,2,2,2,2,2,2,2,2,2,2,2,2,
2,2,2,2,2,2,2,2,2,2,2,2,2,2,2,2,2,2,2,2,2,2,2,2,2,2,2,2,2,2,2,2,4),(-2.66768858982521,
-2.61548896877153,-2.59709218284674,-2.58597251558751,-2.58263451317238,
-2.58054173678217,-2.57860857796354,-2.5761135948932,-2.57197620698229,
-2.54431964197868,-2.50203657869528,-2.48608860941616,-2.48055584025264,
-2.47791674022811,-2.47580170224508,-2.47457852674913,-2.47457497998066,
-2.47457141961672,-2.47456784565589,-2.47456425770073,-2.47456065578851,
-2.47455676068287,-2.47455279767257,-2.47454876538423,-2.4745446621522,
-2.47454048653611,-2.47453623699223,-2.47453191195419,-2.47452750977546,
-2.47452302865531,-2.47451846685654,-2.47349995987621,-2.47213831295872,
-2.4693606005064,-2.44976951333447,-2.40678477004586,-2.37604589982498,
-2.37160172333146,-2.36926829660271,-2.36735663298897,-2.36514152603537,
-2.36135107466242,-2.34671264791226,-2.33445992859165,-2.2940883402603,
-2.27526162494784,-2.26597271472751,-2.26383073347549,-2.26260303948821,
-2.26152835828382,-2.26013986258116,-2.25722550529324,-2.22720436744997,
-2.22134525855173,-2.18858927941237,-2.16604120359468,-2.16038964584546,
-2.15781898892924,-2.15588087587657,-2.15405439840896,-2.15151263101193,
-2.14487102325656,-2.08908347801888,-2.06501753820829,-2.05419381562661,
-2.05195004850705,-2.05069996338546,-2.04962816109695,-2.04827233538406,
-2.04612717251834,-2.03509364883462,-1.98380446409605,-1.95516390243856,
-1.94873875176907,-1.94603172128124,-1.94407053306687,-1.94227789866082,
-1.93941187568713,-1.93251940555216,-1.87956931497458,-1.85358275109322,
-1.84225593726981,-1.83998254241669,-1.83872602773826,-1.83765485189969,
-1.83630764114471,-1.83368797587197,-1.8176741187007,-1.81224529340355,
-1.79776915784436,-1.76488248766917,-1.74831911116621,-1.73800862446994,
-1.73476013975599,-1.73268697391084,-1.73074645051109,-1.72820549631391,
-1.72391089752837,-1.68879247073889,-1.63986091691466,-1.63013049875607,
-1.62795721093769,-1.62672252855143,-1.6256487838211,-1.62427073719501,
-1.62205244279046,-1.60975260750496,-1.60659787281006,-1.60639522129257,
-1.60500788913289,-1.59754454953592,-1.58574638597926,-1.55288297089003,
-1.5363492285818,-1.52605194581472,-1.52280482910815,-1.52073186481134,
-1.51879105818772,-1.51624905206128,-1.51195114827854,-1.47659214975019,
-1.427430573787,-1.41811515732466,-1.41597097437513,-1.41474264762363,-1.4136678227414,
-1.41227968268057,-1.40936798182881,-1.40856908540218),.UNSPECIFIED.);
#776=B_SPLINE_CURVE_WITH_KNOTS('',3,(#73012,#73013,#73014,#73015,#73016,
#73017,#73018,#73019,#73020,#73021,#73022,#73023,#73024,#73025,#73026,#73027,
#73028,#73029,#73030,#73031,#73032,#73033,#73034,#73035,#73036,#73037,#73038,
#73039,#73040,#73041,#73042,#73043,#73044,#73045,#73046,#73047,#73048,#73049,
#73050,#73051,#73052,#73053,#73054,#73055,#73056,#73057,#73058,#73059,#73060,
#73061,#73062,#73063,#73064,#73065,#73066,#73067,#73068,#73069,#73070,#73071,
#73072,#73073,#73074,#73075,#73076,#73077,#73078,#73079,#73080,#73081,#73082,
#73083,#73084,#73085,#73086,#73087,#73088,#73089,#73090,#73091,#73092,#73093,
#73094,#73095,#73096,#73097,#73098,#73099,#73100,#73101,#73102,#73103,#73104,
#73105,#73106,#73107,#73108,#73109,#73110,#73111,#73112,#73113,#73114,#73115,
#73116,#73117,#73118,#73119,#73120,#73121,#73122,#73123,#73124,#73125,#73126,
#73127,#73128,#73129,#73130,#73131,#73132,#73133,#73134,#73135,#73136,#73137,
#73138,#73139,#73140,#73141,#73142,#73143,#73144,#73145,#73146,#73147,#73148,
#73149,#73150,#73151,#73152,#73153,#73154,#73155,#73156,#73157,#73158,#73159,
#73160,#73161,#73162,#73163,#73164,#73165,#73166,#73167,#73168,#73169,#73170,
#73171,#73172,#73173,#73174,#73175,#73176,#73177,#73178,#73179,#73180,#73181,
#73182,#73183,#73184,#73185,#73186,#73187,#73188,#73189,#73190,#73191,#73192,
#73193,#73194,#73195,#73196,#73197,#73198,#73199,#73200,#73201,#73202,#73203,
#73204,#73205,#73206,#73207,#73208,#73209,#73210,#73211,#73212,#73213,#73214,
#73215,#73216,#73217,#73218,#73219,#73220,#73221,#73222,#73223,#73224,#73225,
#73226,#73227),.UNSPECIFIED.,.F.,.F.,(4,2,2,2,2,2,2,2,2,2,2,2,2,2,2,2,2,
2,2,2,2,2,2,2,2,2,2,2,2,2,2,2,2,2,2,2,2,2,2,2,2,2,2,2,2,2,2,2,2,2,2,2,2,
2,2,2,2,2,2,2,2,2,2,2,2,2,2,2,2,2,2,2,2,2,2,2,2,2,2,2,2,2,2,2,2,2,2,2,2,
2,2,2,2,2,2,2,2,2,2,2,2,2,2,2,2,2,2,4),(-1.25997088998495,-1.25915938594851,
-1.20936246129004,-1.20515951081736,-1.20349953697922,-1.20248974489613,
-1.20138550293452,-1.19981051724376,-1.19583461291313,-1.17602195020207,
-1.14710915924182,-1.10479023230581,-1.10049511966369,-1.09795388032023,
-1.09601313909686,-1.09393973957955,-1.09069088550478,-1.08037911476509,
-1.0638158766874,-1.03095510860562,-1.01703048962702,-1.01060094149894,
-0.995017859170259,-0.992416308889875,-0.991072921165533,-0.990001879297503,
-0.988742148630458,-0.986454303225226,-0.974875759619038,-0.947884438765955,
-0.896303807819882,-0.889312882965154,-0.886430439299655,-0.884634679239556,
-0.882675788452561,-0.879982350025813,-0.873638319236514,-0.845679922156646,
-0.799187143952254,-0.783069530515761,-0.780442292428072,-0.779093389562779,
-0.778022023285564,-0.776766628080356,-0.774498653501712,-0.763268518759134,
-0.737658607207535,-0.684115422820024,-0.677266049977641,-0.674406981219692,
-0.672615510694201,-0.67065303473273,-0.667939512583055,-0.661476520998392,
-0.607432539657972,-0.57135384080706,-0.568495481477209,-0.567117807054397,
-0.566044085688787,-0.564809137742537,-0.562634670186238,-0.552887583070529,
-0.503943804097238,-0.468812369254383,-0.464519859198177,-0.461979550208044,
-0.460039168375182,-0.457965812272562,-0.454716314930514,-0.444396501120506,
-0.427814631244484,-0.371116881744046,-0.358713447202724,-0.356489604077167,
-0.355109878850799,-0.354035970281442,-0.352802397213448,-0.350634140673739,
-0.340976935671784,-0.291957487243451,-0.256812038695503,-0.252513704361133,
-0.249971722796989,-0.248031084683539,-0.246240436043974,-0.243303027853584,
-0.235328349705132,-0.223524277204574,-0.190998983152449,-0.15007844644583,
-0.145387645993221,-0.143651116808162,-0.14262662328381,-0.141533912165226,
-0.140020750544341,-0.136420730740827,-0.0985295544978921,-0.075735779521925,
-0.0634020308221991,-0.0604357883634491,-0.0436144641611536,-0.0399995481703897,
-0.0376361127493614,-0.0357225149470006,-0.0339209956216892,-0.0317709078565799,
-0.0286342760631504,-0.000628476376618018),.UNSPECIFIED.);
#777=B_SPLINE_CURVE_WITH_KNOTS('',3,(#73228,#73229,#73230,#73231,#73232,
#73233,#73234,#73235,#73236,#73237,#73238,#73239,#73240,#73241,#73242,#73243,
#73244,#73245),.UNSPECIFIED.,.F.,.F.,(4,2,2,2,2,2,2,2,4),(-2.66749886584903,
-2.62118884059196,-2.60358532551492,-2.5998480387605,-2.59831158971457,
-2.59721449148509,-2.5961956497179,-2.59448907267751,-2.59335004581682),
 .UNSPECIFIED.);
#778=B_SPLINE_CURVE_WITH_KNOTS('',3,(#73251,#73252,#73253,#73254,#73255,
#73256,#73257,#73258,#73259,#73260,#73261,#73262,#73263),.UNSPECIFIED.,
 .F.,.F.,(4,3,3,3,4),(76.3573194796184,76.4589088025925,76.5605127982575,
76.6622238139045,76.707559910557),.UNSPECIFIED.);
#779=B_SPLINE_CURVE_WITH_KNOTS('',3,(#73264,#73265,#73266,#73267,#73268,
#73269,#73270,#73271,#73272,#73273),.UNSPECIFIED.,.F.,.F.,(4,1,1,1,1,1,
1,4),(76.7075601022117,76.9104066470643,77.9092430970262,78.9080795469881,
79.90691599695,80.9057524469119,81.9045888968737,82.6397395021165),
 .UNSPECIFIED.);
#780=B_SPLINE_CURVE_WITH_KNOTS('',3,(#73274,#73275,#73276,#73277,#73278,
#73279,#73280,#73281,#73282,#73283,#73284,#73285,#73286,#73287,#73288,#73289,
#73290,#73291,#73292,#73293,#73294,#73295,#73296,#73297,#73298,#73299,#73300,
#73301,#73302,#73303,#73304,#73305,#73306,#73307,#73308,#73309,#73310,#73311,
#73312,#73313,#73314,#73315,#73316,#73317,#73318,#73319,#73320,#73321,#73322,
#73323,#73324,#73325,#73326,#73327,#73328,#73329,#73330,#73331,#73332,#73333,
#73334,#73335,#73336,#73337,#73338,#73339,#73340,#73341,#73342,#73343,#73344,
#73345,#73346,#73347,#73348,#73349,#73350,#73351,#73352,#73353,#73354,#73355,
#73356,#73357,#73358,#73359,#73360,#73361,#73362,#73363,#73364,#73365,#73366,
#73367,#73368,#73369,#73370,#73371,#73372,#73373,#73374,#73375,#73376,#73377,
#73378,#73379,#73380,#73381,#73382,#73383,#73384,#73385,#73386,#73387,#73388,
#73389,#73390,#73391,#73392,#73393,#73394,#73395,#73396,#73397,#73398,#73399,
#73400,#73401,#73402,#73403,#73404,#73405,#73406,#73407,#73408,#73409,#73410,
#73411,#73412,#73413,#73414,#73415,#73416,#73417,#73418,#73419,#73420,#73421,
#73422,#73423,#73424,#73425,#73426,#73427,#73428,#73429,#73430,#73431,#73432,
#73433,#73434,#73435,#73436,#73437,#73438,#73439,#73440,#73441,#73442,#73443,
#73444,#73445,#73446,#73447,#73448,#73449,#73450,#73451,#73452,#73453,#73454,
#73455,#73456,#73457,#73458,#73459,#73460,#73461,#73462,#73463,#73464,#73465,
#73466,#73467,#73468,#73469,#73470,#73471,#73472,#73473,#73474,#73475,#73476,
#73477,#73478,#73479,#73480,#73481,#73482,#73483,#73484,#73485,#73486,#73487,
#73488,#73489,#73490,#73491,#73492,#73493,#73494,#73495,#73496,#73497,#73498,
#73499,#73500,#73501,#73502,#73503,#73504,#73505,#73506,#73507,#73508,#73509),
 .UNSPECIFIED.,.F.,.F.,(4,2,2,2,2,2,2,2,2,2,2,2,2,2,2,2,2,2,2,2,2,2,2,2,
2,2,2,2,2,2,2,2,2,2,2,2,2,2,2,2,2,2,2,2,2,2,2,2,2,2,2,2,2,2,2,2,2,2,2,2,
2,2,2,2,2,2,2,2,2,2,2,2,2,2,2,2,2,2,2,2,2,2,2,2,2,2,2,2,2,2,2,2,2,2,2,2,
2,2,2,2,2,2,2,2,2,2,2,2,2,2,2,2,2,2,2,2,2,4),(-2.59335004581682,-2.58999661647289,
-2.54298822566556,-2.52282531450821,-2.50695145909145,-2.50030351558134,
-2.49524072965445,-2.49278360397924,-2.49085430630762,-2.48900664979301,
-2.48585214961438,-2.47714077652947,-2.47621720966657,-2.42660199449724,
-2.40064010349671,-2.38931836114964,-2.38704484075098,-2.38578810308318,
-2.38471664392004,-2.38336895814841,-2.38074802022203,-2.36471991080766,
-2.35646656727578,-2.31512128777579,-2.29646839836423,-2.2852377555109,
-2.28188729080691,-2.27979135151281,-2.27785842862949,-2.27536816262005,
-2.27124813843114,-2.24430743096339,-2.20161635166961,-2.18540412607491,
-2.17698169006088,-2.17490542676618,-2.17369204246962,-2.17261418945241,
-2.17122414614609,-2.16891628770687,-2.15484859550471,-2.14363434223291,
-2.10759082339872,-2.07836174403861,-2.07186583929587,-2.06914637507462,
-2.06718244016351,-2.0653915856908,-2.06253770342873,-2.05572235948569,
-2.00176933962491,-1.97645424138811,-1.96529851669718,-1.9630344988653,
-1.96177977212936,-1.96070805213172,-1.95935751814658,-1.95672360049277,
-1.94037023846529,-1.93130268342654,-1.89233486680948,-1.86585535645503,
-1.85969246019393,-1.85702977428294,-1.85507592961925,-1.85327266367671,
-1.85035119746512,-1.84312955644879,-1.79876310021537,-1.78472961336681,
-1.76327504185664,-1.75318360347803,-1.75098563009592,-1.74974532528916,
-1.74867202217588,-1.74730147530282,-1.74510859862459,-1.73333817430004,
-1.72962679302802,-1.72236561755901,-1.67901009945593,-1.66042269314622,
-1.64921988552873,-1.64587222371128,-1.64377680994162,-1.64184353799485,
-1.63935165754725,-1.63522644470455,-1.60809058835119,-1.56616639778275,
-1.54954738105999,-1.54098479617681,-1.53889724539177,-1.53768130649548,
-1.53660391444603,-1.53521798987499,-1.53292428426228,-1.51915035003429,
-1.50784475920294,-1.46844818184545,-1.4418753879567,-1.43570087708518,
-1.43303616922358,-1.43108196856404,-1.42927916587146,-1.4263602192889,
-1.41915355534996,-1.37307257018466,-1.33396208825774,-1.33297752449863,
-1.32826981195437,-1.32653033376173,-1.32550500699202,-1.32441217670042,
-1.32290010594739,-1.31930847052064,-1.28016891975437,-1.25968440179264),
 .UNSPECIFIED.);
#781=B_SPLINE_CURVE_WITH_KNOTS('',3,(#73515,#73516,#73517,#73518,#73519,
#73520,#73521,#73522,#73523,#73524,#73525,#73526,#73527,#73528,#73529,#73530,
#73531,#73532),.UNSPECIFIED.,.F.,.F.,(4,2,2,2,2,2,2,2,4),(-0.0749304253432432,
-0.0455284962237961,-0.0267278979708963,-0.0187639971196157,-0.00802108746917657,
-0.00466632884064646,-0.00258130080575418,-0.00128118374794539,-0.000628942230927431),
 .UNSPECIFIED.);
#782=B_SPLINE_CURVE_WITH_KNOTS('',3,(#73533,#73534,#73535,#73536,#73537,
#73538,#73539,#73540,#73541,#73542,#73543,#73544,#73545,#73546,#73547,#73548,
#73549,#73550,#73551,#73552,#73553,#73554,#73555,#73556,#73557,#73558,#73559,
#73560,#73561,#73562,#73563,#73564,#73565,#73566,#73567,#73568,#73569,#73570,
#73571,#73572,#73573,#73574,#73575,#73576,#73577,#73578,#73579,#73580,#73581,
#73582,#73583,#73584,#73585,#73586,#73587,#73588,#73589,#73590,#73591,#73592,
#73593,#73594,#73595,#73596,#73597,#73598,#73599,#73600,#73601,#73602,#73603,
#73604,#73605,#73606,#73607,#73608,#73609,#73610,#73611,#73612,#73613,#73614,
#73615,#73616,#73617,#73618,#73619,#73620,#73621,#73622,#73623,#73624,#73625,
#73626,#73627,#73628,#73629,#73630,#73631,#73632,#73633,#73634,#73635,#73636,
#73637,#73638,#73639,#73640,#73641,#73642,#73643,#73644,#73645,#73646,#73647,
#73648,#73649,#73650,#73651,#73652,#73653,#73654,#73655,#73656,#73657,#73658,
#73659,#73660,#73661,#73662,#73663,#73664,#73665,#73666,#73667,#73668,#73669,
#73670,#73671,#73672,#73673,#73674,#73675,#73676,#73677,#73678,#73679,#73680,
#73681,#73682,#73683,#73684,#73685,#73686,#73687,#73688,#73689,#73690,#73691,
#73692,#73693,#73694,#73695,#73696,#73697,#73698,#73699,#73700,#73701,#73702,
#73703,#73704,#73705,#73706,#73707,#73708,#73709,#73710,#73711,#73712,#73713),
 .UNSPECIFIED.,.F.,.F.,(4,3,3,3,3,3,3,3,3,3,3,3,3,3,3,3,3,3,3,3,3,3,3,3,
3,3,3,3,3,3,3,3,3,3,3,3,3,3,3,3,3,3,3,3,3,3,3,3,3,3,3,3,3,3,3,3,3,3,3,3,
4),(70.4243747954073,70.5325790413758,70.6410991164239,70.7497863837817,
70.8587740112793,70.9173879472931,71.0207826843411,71.1240239664562,71.2271439318486,
71.3301985000576,71.4332217084154,71.5362475510879,71.639380317866,71.7425694092759,
71.8459414026576,71.916224397255,72.0196191343029,72.1228604164179,72.2259803818102,
72.3290349500191,72.4320581583768,72.5350840010492,72.6382167678273,72.7414058592371,
72.8447778526187,72.9150608472168,73.0184555842647,73.1216968663797,73.224816831772,
73.3278713999809,73.4308946083386,73.5339204510111,73.6370532177892,73.740242309199,
73.8436143025806,73.9138972971787,74.0172920342267,74.1205333163417,74.223653281734,
74.326707849943,74.4297310583007,74.5327569009732,74.6358896677513,74.7390787591612,
74.8424507525428,74.9127337471406,75.0161284841886,75.1193697663036,75.2224897316959,
75.3255442999048,75.4285675082626,75.531593350935,75.6347261177131,75.7379152091229,
75.8412872025045,75.9115701971025,76.0134810050385,76.1152211478776,76.2168630906285,
76.3184433457388,76.3573194796184),.UNSPECIFIED.);
#783=B_SPLINE_CURVE_WITH_KNOTS('',3,(#73715,#73716,#73717,#73718,#73719,
#73720,#73721,#73722,#73723,#73724,#73725,#73726,#73727,#73728,#73729,#73730,
#73731,#73732,#73733,#73734,#73735,#73736,#73737,#73738,#73739,#73740,#73741,
#73742,#73743,#73744,#73745,#73746,#73747,#73748,#73749,#73750,#73751,#73752,
#73753,#73754,#73755,#73756,#73757,#73758,#73759,#73760,#73761,#73762,#73763,
#73764,#73765,#73766,#73767,#73768,#73769,#73770,#73771,#73772,#73773,#73774,
#73775,#73776,#73777,#73778,#73779,#73780,#73781,#73782,#73783,#73784,#73785,
#73786,#73787,#73788,#73789,#73790,#73791,#73792,#73793,#73794,#73795,#73796,
#73797,#73798,#73799,#73800,#73801,#73802,#73803,#73804,#73805,#73806,#73807,
#73808,#73809,#73810,#73811,#73812,#73813,#73814,#73815,#73816,#73817,#73818,
#73819,#73820,#73821,#73822,#73823,#73824,#73825,#73826,#73827,#73828,#73829,
#73830,#73831,#73832,#73833,#73834,#73835,#73836,#73837,#73838,#73839,#73840,
#73841,#73842,#73843,#73844,#73845,#73846,#73847,#73848,#73849,#73850,#73851,
#73852,#73853,#73854,#73855,#73856,#73857,#73858,#73859,#73860,#73861,#73862,
#73863,#73864,#73865,#73866,#73867,#73868,#73869,#73870,#73871,#73872,#73873,
#73874,#73875,#73876,#73877,#73878,#73879,#73880,#73881,#73882,#73883,#73884,
#73885,#73886,#73887,#73888,#73889,#73890,#73891,#73892,#73893,#73894,#73895,
#73896,#73897,#73898,#73899,#73900,#73901,#73902,#73903,#73904,#73905,#73906,
#73907,#73908,#73909,#73910,#73911,#73912,#73913,#73914,#73915,#73916,#73917,
#73918,#73919,#73920,#73921,#73922,#73923,#73924,#73925,#73926,#73927,#73928,
#73929,#73930),.UNSPECIFIED.,.F.,.F.,(4,2,2,2,2,2,2,2,2,2,2,2,2,2,2,2,2,
2,2,2,2,2,2,2,2,2,2,2,2,2,2,2,2,2,2,2,2,2,2,2,2,2,2,2,2,2,2,2,2,2,2,2,2,
2,2,2,2,2,2,2,2,2,2,2,2,2,2,2,2,2,2,2,2,2,2,2,2,2,2,2,2,2,2,2,2,2,2,2,2,
2,2,2,2,2,2,2,2,2,2,2,2,2,2,2,2,2,2,4),(-1.25968440179264,-1.23134354359258,
-1.22421237516867,-1.22130613530729,-1.21950569996339,-1.21754974618457,
-1.21487487073439,-1.20864141476093,-1.18159524773247,-1.14086775040501,
-1.11820863565655,-1.11535573719631,-1.11397894883129,-1.11290509685899,
-1.11166907107165,-1.10949048549418,-1.09968816714513,-1.05077794022017,
-1.0156573334309,-1.01136167951513,-1.00882016350117,-1.00687923608233,
-1.00480566197672,-1.00155658514622,-0.991244535768014,-0.974681257565122,
-0.941818689315611,-0.928011237409794,-0.921314019760237,-0.905865110191607,
-0.903497154921353,-0.902089561422103,-0.901009403711653,-0.899805960922281,
-0.897774187092332,-0.889884288291235,-0.875167986218626,-0.846104074711493,
-0.803698149660333,-0.799404686669405,-0.796863862765149,-0.794923115869781,
-0.792849397085583,-0.789599388560396,-0.779278434431453,-0.762695192216084,
-0.729816909009761,-0.71451639446695,-0.709793784952005,-0.69394156356986,
-0.6913287511807,-0.689982894230297,-0.688911650363044,-0.687653733401105,
-0.685374422218113,-0.673948886331171,-0.647572501794949,-0.59512229006198,
-0.588188792919766,-0.585315749203526,-0.583521642465524,-0.581561190123421,
-0.578859461115646,-0.572467090465569,-0.526046462190321,-0.484947958096599,
-0.480263100775048,-0.478527318893239,-0.477502868156652,-0.476409864053683,
-0.474895743400699,-0.471290883635746,-0.432950265486838,-0.383317351113001,
-0.376221655519629,-0.373321731023507,-0.371522738030721,-0.36956639584249,
-0.366887460089059,-0.360806569983863,-0.352445732563901,-0.301551240269501,
-0.27031324179841,-0.267401274645498,-0.266013097821487,-0.264938282186225,
-0.263710017433473,-0.261566048832606,-0.252414968969124,-0.203666437397408,
-0.167704290380167,-0.162982356583487,-0.160559558302476,-0.158640677010409,
-0.156487803395795,-0.154258048298956,-0.146612096948347,-0.121083045479512,
-0.100337617846573,-0.0610229399657464,-0.0562870051492831,-0.0545435818946793,
-0.0535177060778159,-0.0524257934789496,-0.0509174405909417,-0.0492296220639371,
-0.0462824118400645,-0.00062912028025528),.UNSPECIFIED.);
#784=B_SPLINE_CURVE_WITH_KNOTS('',3,(#73931,#73932,#73933,#73934,#73935,
#73936,#73937,#73938,#73939,#73940,#73941,#73942,#73943),.UNSPECIFIED.,
 .F.,.F.,(4,3,3,3,4),(-66.6728921052185,-66.5709585796832,-66.4690950147654,
-66.3672509448922,-66.3228588019918),.UNSPECIFIED.);
#785=B_SPLINE_CURVE_WITH_KNOTS('',3,(#73948,#73949,#73950,#73951,#73952,
#73953,#73954,#73955,#73956,#73957,#73958,#73959,#73960,#73961,#73962,#73963,
#73964,#73965,#73966,#73967,#73968,#73969,#73970,#73971,#73972,#73973,#73974,
#73975,#73976,#73977,#73978,#73979,#73980,#73981,#73982,#73983,#73984,#73985,
#73986,#73987,#73988,#73989,#73990,#73991,#73992,#73993,#73994,#73995,#73996,
#73997,#73998,#73999,#74000,#74001,#74002,#74003,#74004,#74005,#74006,#74007,
#74008,#74009,#74010,#74011,#74012,#74013,#74014,#74015,#74016,#74017,#74018,
#74019,#74020,#74021,#74022,#74023,#74024,#74025,#74026,#74027,#74028,#74029,
#74030,#74031,#74032,#74033,#74034,#74035,#74036,#74037,#74038,#74039,#74040,
#74041,#74042,#74043,#74044,#74045,#74046,#74047,#74048,#74049,#74050,#74051,
#74052,#74053,#74054,#74055,#74056,#74057,#74058,#74059,#74060,#74061,#74062,
#74063,#74064,#74065,#74066,#74067,#74068,#74069,#74070,#74071,#74072,#74073,
#74074,#74075,#74076,#74077,#74078,#74079,#74080,#74081,#74082,#74083,#74084,
#74085,#74086,#74087,#74088,#74089,#74090,#74091,#74092,#74093,#74094,#74095,
#74096,#74097,#74098,#74099,#74100,#74101,#74102,#74103,#74104,#74105,#74106,
#74107,#74108,#74109,#74110,#74111,#74112,#74113,#74114,#74115,#74116,#74117,
#74118,#74119,#74120,#74121,#74122,#74123,#74124,#74125,#74126,#74127,#74128,
#74129,#74130,#74131,#74132,#74133,#74134,#74135,#74136,#74137,#74138,#74139,
#74140,#74141,#74142,#74143,#74144,#74145,#74146,#74147,#74148,#74149,#74150,
#74151,#74152,#74153,#74154,#74155,#74156,#74157,#74158,#74159,#74160,#74161,
#74162,#74163,#74164,#74165,#74166,#74167,#74168,#74169,#74170,#74171,#74172,
#74173,#74174,#74175,#74176,#74177,#74178,#74179,#74180,#74181,#74182,#74183),
 .UNSPECIFIED.,.F.,.F.,(4,2,2,2,2,2,2,2,2,2,2,2,2,2,2,2,2,2,2,2,2,2,2,2,
2,2,2,2,2,2,2,2,2,2,2,2,2,2,2,2,2,2,2,2,2,2,2,2,2,2,2,2,2,2,2,2,2,2,2,2,
2,2,2,2,2,2,2,2,2,2,2,2,2,2,2,2,2,2,2,2,2,2,2,2,2,2,2,2,2,2,2,2,2,2,2,2,
2,2,2,2,2,2,2,2,2,2,2,2,2,2,2,2,2,2,2,2,2,4),(-1.40858075324139,-1.3954320310824,
-1.38403044609259,-1.38175218761962,-1.38049433958623,-1.37942284788281,
-1.37807628373716,-1.37546093967725,-1.35953982828857,-1.3550374675103,
-1.33447375915959,-1.28611804330527,-1.2789688130659,-1.27605948095026,
-1.27425842721691,-1.27230282560658,-1.26963027500151,-1.2634106407658,
-1.236477491613,-1.19595077061155,-1.17295835890062,-1.17010289559586,-1.16872557241452,
-1.16765163385077,-1.16641588170656,-1.16423867208337,-1.1544573691123,
-1.10552726911894,-1.07039940615101,-1.06610351061807,-1.06356187536306,
-1.06162087053721,-1.05954722697486,-1.05629806895955,-1.045985994997,-1.02942289900999,
-0.996559755773456,-0.982817040336085,-0.975966154357702,-0.975652096740871,
-0.970071493947574,-0.960066604665169,-0.957987944541318,-0.956652334414198,
-0.955581600488022,-0.95431533213327,-0.951997722631066,-0.939874527391814,
-0.887010946290296,-0.858184668381248,-0.85401554228252,-0.851511002737233,
-0.849576079450493,-0.847486992237177,-0.844166926328647,-0.833217602457786,
-0.815218071557374,-0.764880679873219,-0.748636138557531,-0.746006908141442,
-0.744657497923189,-0.743585998854998,-0.742330760681044,-0.740063861275224,
-0.728855049170755,-0.703329670730521,-0.649654556879947,-0.64281484722695,
-0.639957196981804,-0.638165854861379,-0.636202906072923,-0.63348760102407,
-0.627014974625186,-0.572643457020699,-0.565705913317623,-0.536988933091167,
-0.534076816790993,-0.53268857431109,-0.53161371034783,-0.530385393173036,
-0.528241339642794,-0.518928532966178,-0.469757761828656,-0.434365043220982,
-0.430066107429614,-0.427523821151675,-0.425582979749055,-0.423510150961256,
-0.42026360554307,-0.409971071037893,-0.393450040703956,-0.360625201356664,
-0.350841379626458,-0.32499280592247,-0.322101634848752,-0.320717556899922,
-0.319643221873447,-0.318412484745028,-0.316257085837481,-0.306783343152919,
-0.257606400046225,-0.222412842168993,-0.217734027536337,-0.215348525553729,
-0.213485530932822,-0.211693643003537,-0.208571161773771,-0.199305098970657,
-0.18498357052622,-0.124681947776451,-0.11228550953053,-0.110062031709171,
-0.108682412250948,-0.1076085081102,-0.106374852361822,-0.104206241556676,
-0.0945440565291435,-0.0749304253432432),.UNSPECIFIED.);
#786=B_SPLINE_CURVE_WITH_KNOTS('',3,(#74185,#74186,#74187,#74188,#74189,
#74190,#74191,#74192,#74193,#74194,#74195,#74196,#74197,#74198,#74199,#74200,
#74201,#74202,#74203,#74204,#74205,#74206,#74207,#74208,#74209,#74210,#74211,
#74212,#74213,#74214,#74215,#74216,#74217,#74218,#74219,#74220,#74221,#74222,
#74223,#74224,#74225,#74226,#74227,#74228,#74229,#74230,#74231,#74232,#74233,
#74234,#74235,#74236,#74237,#74238,#74239,#74240,#74241,#74242,#74243,#74244,
#74245,#74246,#74247,#74248,#74249,#74250,#74251,#74252,#74253,#74254,#74255,
#74256,#74257,#74258,#74259,#74260,#74261,#74262,#74263,#74264,#74265,#74266,
#74267,#74268,#74269,#74270,#74271,#74272,#74273,#74274,#74275,#74276,#74277,
#74278,#74279,#74280,#74281,#74282,#74283,#74284,#74285,#74286,#74287,#74288,
#74289,#74290,#74291,#74292,#74293,#74294,#74295,#74296,#74297,#74298,#74299,
#74300,#74301,#74302,#74303,#74304,#74305,#74306,#74307,#74308,#74309,#74310,
#74311,#74312,#74313,#74314,#74315,#74316,#74317,#74318,#74319,#74320,#74321,
#74322,#74323,#74324,#74325,#74326,#74327,#74328,#74329,#74330,#74331,#74332,
#74333,#74334,#74335,#74336,#74337,#74338,#74339,#74340,#74341,#74342,#74343,
#74344,#74345,#74346,#74347,#74348,#74349,#74350,#74351,#74352,#74353,#74354,
#74355,#74356,#74357,#74358,#74359,#74360,#74361,#74362),.UNSPECIFIED.,
 .F.,.F.,(4,3,3,3,3,3,3,3,3,3,3,3,3,3,3,3,3,3,3,3,3,3,3,3,3,3,3,3,3,3,3,
3,3,3,3,3,3,3,3,3,3,3,3,3,3,3,3,3,3,3,3,3,3,3,3,3,3,3,3,4),(-66.3228588019918,
-66.2209269508808,-66.1189508703786,-66.0167874549306,-65.9232056974837,
-65.8198109604357,-65.7165696783206,-65.6134497129283,-65.5103951447194,
-65.4073719363618,-65.3043460936894,-65.2012133269113,-65.0980242355016,
-64.99465224212,-64.9243692475218,-64.820974510474,-64.7177332283591,-64.6146132629669,
-64.5115586947579,-64.4085354864001,-64.3055096437278,-64.2023768769497,
-64.09918778554,-63.9958157921584,-63.92553279756,-63.8221380605121,-63.7188967783972,
-63.6157768130049,-63.512722244796,-63.4096990364381,-63.3066731937657,
-63.2035404269877,-63.1003513355779,-62.9969793421963,-62.9266963475981,
-62.8233016105501,-62.7200603284351,-62.6169403630427,-62.5138857948337,
-62.4108625864758,-62.3078367438028,-62.2047039770247,-62.101514885615,
-61.9981428922333,-61.9278598976362,-61.8244651605883,-61.721223878473,
-61.6181039130809,-61.515049344872,-61.4120261365142,-61.3090002938415,
-61.2058675270636,-61.1026784356539,-60.9993064422722,-60.9290234476744,
-60.8220651862381,-60.7139755891883,-60.6074364851713,-60.4985716416051,
-60.3897067980389),.UNSPECIFIED.);
#787=B_SPLINE_CURVE_WITH_KNOTS('',3,(#74363,#74364,#74365,#74366),
 .UNSPECIFIED.,.F.,.F.,(4,4),(-60.3897037700897,-60.0402340406592),
 .UNSPECIFIED.);
#788=B_SPLINE_CURVE_WITH_KNOTS('',3,(#74372,#74373,#74374,#74375,#74376,
#74377),.UNSPECIFIED.,.F.,.F.,(4,2,4),(-0.0750411156564984,-0.0537578376115912,
-0.000629603145374127),.UNSPECIFIED.);
#789=B_SPLINE_CURVE_WITH_KNOTS('',3,(#74378,#74379,#74380,#74381,#74382,
#74383,#74384,#74385,#74386,#74387,#74388,#74389,#74390,#74391,#74392,#74393,
#74394,#74395,#74396,#74397,#74398,#74399,#74400,#74401,#74402,#74403,#74404,
#74405,#74406,#74407,#74408,#74409,#74410,#74411,#74412,#74413,#74414,#74415,
#74416,#74417,#74418,#74419,#74420,#74421,#74422,#74423,#74424,#74425,#74426,
#74427,#74428,#74429,#74430,#74431,#74432,#74433,#74434,#74435,#74436,#74437,
#74438,#74439,#74440,#74441,#74442,#74443,#74444,#74445,#74446,#74447,#74448,
#74449,#74450,#74451,#74452,#74453,#74454,#74455,#74456,#74457,#74458,#74459,
#74460,#74461,#74462,#74463,#74464,#74465,#74466,#74467,#74468,#74469,#74470,
#74471,#74472,#74473,#74474,#74475,#74476,#74477,#74478,#74479,#74480,#74481,
#74482,#74483,#74484,#74485,#74486,#74487,#74488,#74489,#74490,#74491,#74492,
#74493,#74494,#74495,#74496,#74497,#74498,#74499,#74500,#74501,#74502,#74503,
#74504,#74505,#74506,#74507,#74508,#74509,#74510,#74511,#74512,#74513,#74514,
#74515,#74516,#74517,#74518,#74519,#74520,#74521,#74522,#74523,#74524,#74525,
#74526,#74527,#74528,#74529,#74530,#74531,#74532,#74533,#74534,#74535,#74536,
#74537,#74538,#74539,#74540,#74541,#74542,#74543,#74544,#74545,#74546,#74547,
#74548,#74549,#74550,#74551,#74552,#74553,#74554,#74555,#74556,#74557,#74558,
#74559,#74560,#74561,#74562,#74563,#74564,#74565,#74566,#74567,#74568,#74569,
#74570,#74571,#74572,#74573,#74574,#74575,#74576,#74577,#74578,#74579,#74580,
#74581,#74582,#74583,#74584,#74585,#74586,#74587,#74588,#74589,#74590,#74591,
#74592,#74593,#74594,#74595,#74596,#74597,#74598,#74599,#74600,#74601,#74602,
#74603,#74604,#74605,#74606,#74607,#74608,#74609,#74610,#74611,#74612,#74613,
#74614,#74615,#74616,#74617,#74618,#74619,#74620,#74621,#74622,#74623,#74624,
#74625,#74626,#74627),.UNSPECIFIED.,.F.,.F.,(4,2,2,2,2,2,2,2,2,2,2,2,2,
2,2,2,2,2,2,2,2,2,2,2,2,2,2,2,2,2,2,2,2,2,2,2,2,2,2,2,2,2,2,2,2,2,2,2,2,
2,2,2,2,2,2,2,2,2,2,2,2,2,2,2,2,2,2,2,2,2,2,2,2,2,2,2,2,2,2,2,2,2,2,2,2,
2,2,2,2,2,2,2,2,2,2,2,2,2,2,2,2,2,2,2,2,2,2,2,2,2,2,2,2,2,2,2,2,2,2,2,2,
2,2,2,4),(-2.66802149891279,-2.65996458342106,-2.65560732822634,-2.65419431785302,
-2.65312705204955,-2.65209682921456,-2.65091690148876,-2.64899166169616,
-2.64292604677928,-2.64164402158647,-2.63384352312468,-2.58064371327289,
-2.56289863577731,-2.55206075228039,-2.54875223902499,-2.54666532087034,
-2.54472890007616,-2.54221746690857,-2.53802604302116,-2.50852862303808,
-2.46741476353145,-2.45198071083895,-2.446566520425,-2.44396770674802,-2.4418610274011,
-2.44064831929846,-2.44064520469193,-2.44064207103828,-2.44063891828999,
-2.44063574642833,-2.4406325552362,-2.4406293446271,-2.44062611448397,-2.44062286459684,
-2.44061959475947,-2.44061630481875,-2.44061299472082,-2.44060966428502,
-2.44060632625828,-2.44060297370119,-2.44059959991487,-2.440596193339,-2.4395692317791,
-2.43819161733589,-2.43533418909548,-2.3992426131968,-2.36651413632511,
-2.34401631510754,-2.33837088445508,-2.33580095458918,-2.33386255053541,
-2.33203518178347,-2.32949118310903,-2.3228378179571,-2.26713559001317,
-2.24299761845435,-2.23215335381526,-2.2299079283935,-2.22865728322776,
-2.22758522498347,-2.22622936305462,-2.22408468155608,-2.21306506631437,
-2.16179724453626,-2.13310351536653,-2.12667124165372,-2.12396258478076,
-2.12200071722641,-2.12020780508928,-2.11734208474587,-2.11045420999899,
-2.0574066039162,-2.03147148976289,-2.02015654662414,-2.01788340882972,
-2.01662675056411,-2.01555527890836,-2.01420747533148,-2.01158600802693,
-1.99554933897305,-1.99020921886958,-1.97566181123813,-1.94276577714998,
-1.92619714808673,-1.91588354880024,-1.91263416695763,-1.91056044864088,
-1.90861942221413,-1.90607782968398,-1.90178219760266,-1.86666137899937,
-1.81773799092039,-1.80798026585771,-1.80580471181151,-1.80456933329518,
-1.80349536195426,-1.80211751978968,-1.79925935418478,-1.76331272716668,
-1.73052944568667,-1.70794918515225,-1.70229232727367,-1.69972013924318,
-1.6977812296767,-1.6959542644931,-1.69341224028618,-1.68677247458836,-1.63092250795175,
-1.59808291707098,-1.59453631026601,-1.59303192828603,-1.59194040903838,
-1.59091292144257,-1.58916250110634,-1.58438291672268,-1.5472057861471,
-1.49693562938493,-1.49053314054903,-1.48782935163067,-1.4858682149485,
-1.48407404461922,-1.48120211525056,-1.47427756954005,-1.42170690742326,
-1.40858075324139),.UNSPECIFIED.);
#790=B_SPLINE_CURVE_WITH_KNOTS('',3,(#74629,#74630,#74631,#74632,#74633,
#74634,#74635,#74636,#74637,#74638),.UNSPECIFIED.,.F.,.F.,(4,1,1,1,1,1,
1,4),(-60.0402340406592,-59.9301869977125,-58.9313505477506,-57.9325140977887,
-56.9336776478269,-55.934841197865,-54.9360047479031,-54.1065275198801),
 .UNSPECIFIED.);
#791=B_SPLINE_CURVE_WITH_KNOTS('',3,(#74639,#74640,#74641,#74642,#74643,
#74644,#74645,#74646,#74647,#74648,#74649,#74650,#74651,#74652,#74653,#74654,
#74655,#74656,#74657,#74658,#74659,#74660),.UNSPECIFIED.,.F.,.F.,(4,2,2,
2,2,2,2,2,2,2,4),(-2.66747056838221,-2.64324040236149,-2.63610839841556,
-2.63431747142202,-2.63310249420984,-2.63209340562307,-2.6310188153633,
-2.62963276479483,-2.62673172851018,-2.59981102814518,-2.59336897902399),
 .UNSPECIFIED.);
#792=B_SPLINE_CURVE_WITH_KNOTS('',3,(#74665,#74666,#74667,#74668,#74669,
#74670,#74671,#74672,#74673,#74674,#74675,#74676,#74677,#74678,#74679,#74680,
#74681,#74682,#74683,#74684,#74685,#74686,#74687,#74688,#74689,#74690,#74691,
#74692,#74693,#74694,#74695,#74696,#74697,#74698,#74699,#74700,#74701,#74702,
#74703,#74704,#74705,#74706,#74707,#74708,#74709,#74710,#74711,#74712,#74713,
#74714,#74715,#74716,#74717,#74718,#74719,#74720,#74721,#74722,#74723,#74724,
#74725,#74726,#74727,#74728,#74729,#74730,#74731,#74732,#74733,#74734,#74735,
#74736,#74737,#74738,#74739,#74740,#74741,#74742,#74743,#74744,#74745,#74746,
#74747,#74748,#74749,#74750,#74751,#74752,#74753,#74754,#74755,#74756,#74757,
#74758,#74759,#74760,#74761,#74762,#74763,#74764,#74765,#74766,#74767,#74768,
#74769,#74770,#74771,#74772,#74773,#74774,#74775,#74776,#74777,#74778,#74779,
#74780,#74781,#74782,#74783,#74784,#74785,#74786,#74787,#74788,#74789,#74790,
#74791,#74792,#74793,#74794,#74795,#74796,#74797,#74798,#74799,#74800,#74801,
#74802,#74803,#74804,#74805,#74806,#74807,#74808,#74809,#74810,#74811,#74812,
#74813,#74814,#74815,#74816,#74817,#74818,#74819,#74820,#74821,#74822,#74823,
#74824,#74825,#74826,#74827,#74828,#74829,#74830,#74831,#74832,#74833,#74834,
#74835,#74836,#74837,#74838,#74839,#74840,#74841,#74842,#74843,#74844,#74845,
#74846,#74847,#74848,#74849,#74850,#74851,#74852,#74853,#74854,#74855,#74856,
#74857,#74858,#74859,#74860,#74861,#74862,#74863,#74864,#74865,#74866,#74867,
#74868,#74869,#74870,#74871,#74872,#74873,#74874,#74875,#74876,#74877,#74878,
#74879,#74880,#74881,#74882,#74883,#74884,#74885,#74886,#74887,#74888,#74889,
#74890,#74891,#74892,#74893,#74894,#74895,#74896,#74897,#74898,#74899,#74900,
#74901,#74902,#74903,#74904),.UNSPECIFIED.,.F.,.F.,(4,2,2,2,2,2,2,2,2,2,
2,2,2,2,2,2,2,2,2,2,2,2,2,2,2,2,2,2,2,2,2,2,2,2,2,2,2,2,2,2,2,2,2,2,2,2,
2,2,2,2,2,2,2,2,2,2,2,2,2,2,2,2,2,2,2,2,2,2,2,2,2,2,2,2,2,2,2,2,2,2,2,2,
2,2,2,2,2,2,2,2,2,2,2,2,2,2,2,2,2,2,2,2,2,2,2,2,2,2,2,2,2,2,2,2,2,2,2,2,
2,4),(-1.40843520122759,-1.38234929436498,-1.36900905915055,-1.3654540019979,
-1.36331283927105,-1.36139154949988,-1.35894820923574,-1.35507363855925,
-1.33399939059767,-1.27618325037938,-1.261222380279,-1.25887432383507,-1.2574725015804,
-1.25639309875386,-1.2551864172719,-1.25314025936278,-1.24508269079824,
-1.22990316159912,-1.19000605476775,-1.15896149866968,-1.15473986411574,
-1.15221987285824,-1.15028241698707,-1.14819985476394,-1.14490988401863,
-1.13423600901413,-1.11686427510417,-1.06815962875071,-1.0616448088961,
-1.04902152617613,-1.04678573062594,-1.04540227320803,-1.04432782403015,
-1.04309628690015,-1.04093790540806,-1.03142591956689,-0.982271267862854,
-0.947074884913862,-0.942778461482244,-0.940236797658543,-0.938295934407803,
-0.936222600497801,-0.932974258368066,-0.922667560803234,-0.906115749914522,
-0.87326380443128,-0.860347435873508,-0.837642264741501,-0.834788611155627,
-0.833411808582419,-0.832338110264254,-0.831102447418038,-0.828924947134709,
-0.819134910169642,-0.770223736401356,-0.735105941467411,-0.730810954169608,
-0.728269844415247,-0.72632923408081,-0.724256005350361,-0.721007483512324,
-0.71069731215435,-0.69413716132622,-0.661280329478122,-0.647507728962088,
-0.640735546171248,-0.638905965280025,-0.625192231067182,-0.622901959248708,
-0.621517252313713,-0.620440276297059,-0.619224220890304,-0.617135131191565,
-0.608547985552004,-0.591852209341912,-0.549940166263519,-0.522879829308167,
-0.518757257096096,-0.516266556573872,-0.514333942997878,-0.512238984866759,
-0.508891489621154,-0.497683856649682,-0.479085549244681,-0.436433318725784,
-0.41374922225421,-0.410899941218018,-0.409524105866194,-0.40845062388991,
-0.407214602033347,-0.40503501200496,-0.395211333805982,-0.346336012184542,
-0.311232573450771,-0.306938283389392,-0.304397547223245,-0.302457199773498,
-0.300384230154729,-0.297136068926355,-0.286826659398029,-0.270267368247141,
-0.237928974445208,-0.201815752245152,-0.198960572232045,-0.197583654521324,
-0.196557124730904,-0.195363751317161,-0.19338085248251,-0.190941175898945,
-0.185983016961778,-0.172433086751189,-0.149616938249916,-0.103071425770781,
-0.0958751453617127,-0.0929586840934602,-0.0911568835027484,-0.0892033560504339,
-0.0865388181216794,-0.0803613062889754,-0.0750411156564984),
 .UNSPECIFIED.);
#793=B_SPLINE_CURVE_WITH_KNOTS('',3,(#74905,#74906,#74907,#74908,#74909,
#74910,#74911,#74912,#74913,#74914,#74915,#74916,#74917,#74918,#74919,#74920,
#74921,#74922,#74923,#74924,#74925,#74926,#74927,#74928,#74929,#74930,#74931,
#74932,#74933,#74934,#74935,#74936,#74937,#74938,#74939,#74940,#74941,#74942,
#74943,#74944,#74945,#74946,#74947,#74948,#74949,#74950,#74951,#74952,#74953,
#74954,#74955,#74956,#74957,#74958,#74959,#74960,#74961,#74962,#74963,#74964,
#74965,#74966,#74967,#74968,#74969,#74970,#74971,#74972,#74973,#74974,#74975,
#74976,#74977,#74978,#74979,#74980,#74981,#74982,#74983,#74984,#74985,#74986,
#74987,#74988,#74989,#74990,#74991,#74992,#74993,#74994,#74995,#74996,#74997,
#74998,#74999,#75000,#75001,#75002,#75003,#75004,#75005,#75006,#75007,#75008,
#75009,#75010,#75011,#75012,#75013,#75014,#75015,#75016,#75017,#75018,#75019,
#75020,#75021,#75022,#75023,#75024,#75025,#75026,#75027,#75028,#75029,#75030,
#75031,#75032,#75033,#75034,#75035,#75036,#75037,#75038,#75039,#75040,#75041,
#75042,#75043,#75044,#75045,#75046,#75047,#75048,#75049,#75050,#75051,#75052,
#75053,#75054,#75055,#75056,#75057,#75058,#75059,#75060,#75061,#75062,#75063,
#75064,#75065,#75066,#75067,#75068,#75069,#75070,#75071,#75072,#75073,#75074,
#75075,#75076,#75077,#75078,#75079,#75080,#75081,#75082,#75083,#75084,#75085,
#75086,#75087,#75088,#75089,#75090,#75091,#75092,#75093,#75094,#75095,#75096,
#75097,#75098,#75099,#75100,#75101,#75102,#75103,#75104,#75105,#75106,#75107,
#75108,#75109,#75110,#75111,#75112,#75113,#75114,#75115,#75116,#75117,#75118,
#75119,#75120,#75121,#75122,#75123,#75124,#75125,#75126,#75127,#75128,#75129,
#75130,#75131,#75132,#75133,#75134),.UNSPECIFIED.,.F.,.F.,(4,2,2,2,2,2,
2,2,2,2,2,2,2,2,2,2,2,2,2,2,2,2,2,2,2,2,2,2,2,2,2,2,2,2,2,2,2,2,2,2,2,2,
2,2,2,2,2,2,2,2,2,2,2,2,2,2,2,2,2,2,2,2,2,2,2,2,2,2,2,2,2,2,2,2,2,2,2,2,
2,2,2,2,2,2,2,2,2,2,2,2,2,2,2,2,2,2,2,2,2,2,2,2,2,2,2,2,2,2,2,2,2,2,2,2,
4),(-2.59336897902399,-2.58612775773752,-2.57460692284161,-2.54603037275735,
-2.53213217693245,-2.52852862917153,-2.52637674652784,-2.52445745754336,
-2.5220324026772,-2.5173006069789,-2.47986237414341,-2.42951076665685,-2.42303686747642,
-2.42114543005634,-2.42013445334268,-2.419061171705,-2.41768947020732,-2.41549247588205,
-2.40365533751416,-2.34625797232683,-2.32969428769209,-2.31938348363044,
-2.31613483212643,-2.31406154378695,-2.31212089445579,-2.30957975909593,
-2.3052848176617,-2.27015873082236,-2.22120715913026,-2.21149608652536,
-2.20932403380151,-2.20808957524292,-2.20701571868636,-2.20563712748466,
-2.20277431791584,-2.1671499722037,-2.13426642530221,-2.1177090732739,-2.10740103365598,
-2.10415262657573,-2.10207934365023,-2.10013859360948,-2.09759717375137,
-2.09330140936512,-2.05812248547131,-2.0090030328744,-1.99948550962677,
-1.99732688032396,-1.99609534933601,-1.99502100607967,-1.99363780696882,
-1.99140265782503,-1.97878987261475,-1.97427160519009,-1.92390177362098,
-1.90628135760737,-1.89549917621213,-1.89219745169104,-1.89011245776445,
-1.88817619708699,-1.88566266851789,-1.88146268977052,-1.85136029210321,
-1.79974352603178,-1.78774374617407,-1.785432846755,-1.78416808589976,-1.78309734572312,
-1.78176010813924,-1.77967596377317,-1.76959020978519,-1.76409154505887,
-1.75666401725485,-1.74315683683923,-1.71027514660382,-1.69372148045322,
-1.68341493028853,-1.68016656398209,-1.67809320405943,-1.67615230956651,
-1.67361059610496,-1.66931410131359,-1.63409706808228,-1.58485217209879,
-1.57547452778713,-1.5733257394765,-1.5720963294015,-1.57102156821656,-1.56963484364631,
-1.56738812898032,-1.55455522106751,-1.55238921011321,-1.50510882210855,
-1.47658468319908,-1.47017272022229,-1.46746753569891,-1.46550633507785,
-1.46371275966823,-1.46084320709142,-1.45393175833352,-1.40120067523501,
-1.37504634358037,-1.36367583392588,-1.36139955533112,-1.36014223469209,
-1.35907084944986,-1.35772398303932,-1.35510677225267,-1.33914478487925,
-1.3342007853959,-1.32855480469969,-1.28159544034006,-1.28015025094885,
-1.26111046282178,-1.25973256582632),.UNSPECIFIED.);
#794=B_SPLINE_CURVE_WITH_KNOTS('',3,(#75140,#75141,#75142,#75143,#75144,
#75145,#75146,#75147,#75148,#75149,#75150,#75151,#75152,#75153,#75154,#75155),
 .UNSPECIFIED.,.F.,.F.,(4,2,2,2,2,2,2,4),(-0.0747818727151328,-0.0742459240434196,
-0.0731681029222417,-0.0719558860471734,-0.0698841331767219,-0.0615139050350039,
-0.0454480673956834,-0.000629549970892275),.UNSPECIFIED.);
#795=B_SPLINE_CURVE_WITH_KNOTS('',3,(#75156,#75157,#75158,#75159,#75160,
#75161,#75162,#75163,#75164,#75165,#75166,#75167,#75168,#75169,#75170,#75171,
#75172,#75173,#75174,#75175,#75176,#75177,#75178,#75179,#75180,#75181,#75182,
#75183,#75184,#75185,#75186,#75187,#75188,#75189,#75190,#75191,#75192,#75193,
#75194,#75195,#75196,#75197,#75198,#75199,#75200,#75201,#75202,#75203,#75204,
#75205,#75206,#75207,#75208,#75209,#75210,#75211,#75212,#75213,#75214,#75215,
#75216,#75217,#75218,#75219,#75220,#75221,#75222,#75223,#75224,#75225,#75226,
#75227,#75228,#75229,#75230,#75231,#75232,#75233,#75234,#75235,#75236,#75237,
#75238,#75239,#75240,#75241,#75242,#75243,#75244,#75245,#75246,#75247,#75248,
#75249,#75250,#75251,#75252,#75253,#75254,#75255,#75256,#75257,#75258,#75259,
#75260,#75261,#75262,#75263,#75264,#75265,#75266,#75267,#75268,#75269,#75270,
#75271,#75272,#75273,#75274,#75275,#75276,#75277,#75278,#75279,#75280,#75281,
#75282,#75283,#75284,#75285,#75286,#75287,#75288,#75289,#75290,#75291,#75292,
#75293,#75294,#75295,#75296,#75297,#75298,#75299,#75300,#75301,#75302,#75303,
#75304,#75305,#75306,#75307,#75308,#75309,#75310,#75311,#75312,#75313,#75314,
#75315,#75316,#75317,#75318,#75319,#75320,#75321,#75322,#75323,#75324,#75325,
#75326,#75327,#75328,#75329,#75330,#75331,#75332,#75333,#75334,#75335,#75336,
#75337,#75338,#75339,#75340,#75341,#75342,#75343,#75344,#75345,#75346,#75347,
#75348,#75349,#75350,#75351,#75352,#75353,#75354,#75355,#75356,#75357,#75358,
#75359,#75360,#75361,#75362,#75363,#75364,#75365,#75366,#75367,#75368,#75369,
#75370,#75371,#75372,#75373,#75374,#75375,#75376,#75377,#75378,#75379),
 .UNSPECIFIED.,.F.,.F.,(4,2,2,2,2,2,2,2,2,2,2,2,2,2,2,2,2,2,2,2,2,2,2,2,
2,2,2,2,2,2,2,2,2,2,2,2,2,2,2,2,2,2,2,2,2,2,2,2,2,2,2,2,2,2,2,2,2,2,2,2,
2,2,2,2,2,2,2,2,2,2,2,2,2,2,2,2,2,2,2,2,2,2,2,2,2,2,2,2,2,2,2,2,2,2,2,2,
2,2,2,2,2,2,2,2,2,2,2,2,2,2,2,4),(-2.66773930540004,-2.64241116651683,-2.63928395192308,
-2.63713771430998,-2.63533677411038,-2.63342268369052,-2.63105334550721,
-2.62741952032345,-2.61031288541215,-2.59812141782425,-2.56892054787406,
-2.53462366403773,-2.53107188279988,-2.52956695134289,-2.52847565367427,
-2.52744886994475,-2.52570071393307,-2.52093343051611,-2.48338424598238,
-2.45585429059528,-2.43890003757105,-2.4319395124763,-2.42667070342962,
-2.42418246266504,-2.42234810064803,-2.42053096910391,-2.41802500843694,
-2.41160546890512,-2.35378688144598,-2.33102452161715,-2.32055935487983,
-2.31833768920478,-2.31709239399665,-2.31602001809181,-2.31465743126096,
-2.31249017417579,-2.30109422186171,-2.25006719077044,-2.22154459090812,
-2.21513337203888,-2.21242861569957,-2.21046776707741,-2.20867454222068,
-2.20580561291208,-2.19889598835342,-2.14617228536373,-2.12002416897991,
-2.1086561187757,-2.10638028414092,-2.10512320225078,-2.10405201652662,
-2.10270539594568,-2.1000886481999,-2.08412916043406,-2.07850644238329,
-2.06415895635759,-2.03127212101885,-2.01470967563004,-2.00439947158316,
-2.00115091795063,-1.99907767016636,-1.99713704340873,-1.9945959154069,
-1.99030093665389,-1.95516790019283,-1.90619370162443,-1.89651019123151,
-1.89434005987186,-1.89310603453091,-1.89203213189743,-1.89065292780709,
-1.88843091391134,-1.87606365563223,-1.87297920045015,-1.87277976154329,
-1.86591263585554,-1.85218003620042,-1.81929740647948,-1.80274167262832,
-1.79243430196009,-1.78918592555969,-1.78711261892362,-1.78517181627456,
-1.78263028364007,-1.77833423025561,-1.74313950070793,-1.69396848415567,
-1.68450892814661,-1.68235436241328,-1.68112370972071,-1.68004920009232,
-1.6786645603133,-1.67577105398807,-1.64973656568661,-1.61156942222171,
-1.58254141965607,-1.57814579748564,-1.57582221950715,-1.57391060877851,
-1.57168647965745,-1.56785821382003,-1.55279682990344,-1.50062826088653,
-1.48178263607802,-1.4724867746221,-1.47034387109809,-1.46911575820303,
-1.46804078187306,-1.46665199933797,-1.46373737361904,-1.43369111484034,
-1.40843520122759),.UNSPECIFIED.);
#796=B_SPLINE_CURVE_WITH_KNOTS('',3,(#75381,#75382,#75383,#75384,#75385,
#75386,#75387,#75388,#75389,#75390,#75391,#75392,#75393,#75394,#75395,#75396,
#75397,#75398,#75399,#75400,#75401,#75402,#75403,#75404,#75405,#75406,#75407,
#75408,#75409,#75410,#75411,#75412,#75413,#75414,#75415,#75416,#75417,#75418,
#75419,#75420,#75421,#75422,#75423,#75424,#75425,#75426,#75427,#75428,#75429,
#75430,#75431,#75432,#75433,#75434,#75435,#75436,#75437,#75438,#75439,#75440,
#75441,#75442,#75443,#75444,#75445,#75446,#75447,#75448,#75449,#75450,#75451,
#75452,#75453,#75454,#75455,#75456,#75457,#75458,#75459,#75460,#75461,#75462,
#75463,#75464,#75465,#75466,#75467,#75468,#75469,#75470,#75471,#75472,#75473,
#75474,#75475,#75476,#75477,#75478,#75479,#75480,#75481,#75482,#75483,#75484,
#75485,#75486,#75487,#75488,#75489,#75490,#75491,#75492,#75493,#75494,#75495,
#75496,#75497,#75498,#75499,#75500,#75501,#75502,#75503,#75504,#75505,#75506,
#75507,#75508,#75509,#75510,#75511,#75512,#75513,#75514,#75515,#75516,#75517,
#75518,#75519,#75520,#75521,#75522,#75523,#75524,#75525,#75526,#75527,#75528,
#75529,#75530,#75531,#75532,#75533,#75534,#75535,#75536,#75537,#75538,#75539,
#75540,#75541,#75542,#75543,#75544,#75545,#75546,#75547,#75548,#75549,#75550,
#75551,#75552,#75553,#75554,#75555,#75556,#75557,#75558,#75559,#75560,#75561,
#75562,#75563,#75564,#75565,#75566,#75567,#75568,#75569,#75570,#75571,#75572,
#75573,#75574,#75575,#75576,#75577,#75578,#75579,#75580,#75581,#75582,#75583,
#75584,#75585,#75586,#75587,#75588,#75589,#75590,#75591,#75592,#75593,#75594,
#75595,#75596,#75597,#75598),.UNSPECIFIED.,.F.,.F.,(4,2,2,2,2,2,2,2,2,2,
2,2,2,2,2,2,2,2,2,2,2,2,2,2,2,2,2,2,2,2,2,2,2,2,2,2,2,2,2,2,2,2,2,2,2,2,
2,2,2,2,2,2,2,2,2,2,2,2,2,2,2,2,2,2,2,2,2,2,2,2,2,2,2,2,2,2,2,2,2,2,2,2,
2,2,2,2,2,2,2,2,2,2,2,2,2,2,2,2,2,2,2,2,2,2,2,2,2,2,4),(-1.25973256582632,
-1.25734927536444,-1.25494051512531,-1.25302276260143,-1.25086057234657,
-1.24721078439067,-1.23275868433367,-1.18237142310263,-1.15270373796546,
-1.14978925033321,-1.14840048727113,-1.14732550086462,-1.14609735761107,
-1.14395434257905,-1.13465739666924,-1.11580594357347,-1.07535275874928,
-1.0630740852536,-1.04849430481256,-1.04470833580197,-1.04249388523533,
-1.04058159978212,-1.03824591976207,-1.03379285064424,-1.00275690956424,
-0.954779868459052,-0.940190390243041,-0.937858015806157,-0.936460774833188,
-0.935381980597219,-0.934172725913621,-0.932115032158586,-0.923919821841095,
-0.908354200208845,-0.866772480596383,-0.854678395852469,-0.836943442398868,
-0.833268238942155,-0.830885873611517,-0.828970408497621,-0.826790607377273,
-0.823061326865718,-0.807597276748613,-0.755884060562644,-0.728679220408929,
-0.725775768173161,-0.724389116142881,-0.723314311240784,-0.722084748327888,
-0.719935436921174,-0.710551821461474,-0.661283547357181,-0.626053184033462,
-0.62175620112068,-0.61921433348283,-0.617273387810849,-0.615200036826116,
-0.611951816094066,-0.601646751784312,-0.585098750021702,-0.552249351195666,
-0.539730922023649,-0.51662183427344,-0.51376440127891,-0.512386830460004,
-0.511313028808089,-0.510077806743987,-0.507902421998602,-0.498144051760086,
-0.44920433462688,-0.414077902096759,-0.409781931034492,-0.407240494728494,
-0.405299782127785,-0.403226586768878,-0.399978414986767,-0.389671864211867,
-0.373119914740638,-0.340269276295497,-0.327232030559009,-0.318524919112912,
-0.30421425517336,-0.301893582119799,-0.300499910548861,-0.2994217613812,
-0.298210870599363,-0.296145157880832,-0.287849400271933,-0.271996907622163,
-0.225995378602473,-0.20164681590449,-0.197627685049602,-0.195167512852649,
-0.193296806704232,-0.191269131835227,-0.188079691277217,-0.18432709544764,
-0.177197803230122,-0.159650714105301,-0.109620595682326,-0.0924449856537553,
-0.0897803292526254,-0.0884234221347708,-0.0873515073188859,-0.0861021507250372,
-0.0838618226893698,-0.0730958619668398,-0.0492411657667594,-0.000629479043906068),
 .UNSPECIFIED.);
#797=B_SPLINE_CURVE_WITH_KNOTS('',3,(#75599,#75600,#75601,#75602,#75603,
#75604,#75605,#75606,#75607,#75608,#75609,#75610,#75611,#75612,#75613,#75614,
#75615,#75616,#75617,#75618,#75619,#75620),.UNSPECIFIED.,.F.,.F.,(4,2,2,
2,2,2,2,2,2,2,4),(-2.66782448542482,-2.66003056299692,-2.65473405888332,
-2.65229065144145,-2.65040877439129,-2.64856804455869,-2.6467416187617,
-2.644201195173,-2.63900996170188,-2.62649959238965,-2.59341035609829),
 .UNSPECIFIED.);
#798=B_SPLINE_CURVE_WITH_KNOTS('',3,(#75625,#75626,#75627,#75628,#75629,
#75630,#75631,#75632,#75633,#75634,#75635,#75636,#75637,#75638,#75639,#75640,
#75641,#75642,#75643,#75644,#75645,#75646,#75647,#75648,#75649,#75650,#75651,
#75652,#75653,#75654,#75655,#75656,#75657,#75658,#75659,#75660,#75661,#75662,
#75663,#75664,#75665,#75666,#75667,#75668,#75669,#75670,#75671,#75672,#75673,
#75674,#75675,#75676,#75677,#75678,#75679,#75680,#75681,#75682,#75683,#75684,
#75685,#75686,#75687,#75688,#75689,#75690,#75691,#75692,#75693,#75694,#75695,
#75696,#75697,#75698,#75699,#75700,#75701,#75702,#75703,#75704,#75705,#75706,
#75707,#75708,#75709,#75710,#75711,#75712,#75713,#75714,#75715,#75716,#75717,
#75718,#75719,#75720,#75721,#75722,#75723,#75724,#75725,#75726,#75727,#75728,
#75729,#75730,#75731,#75732,#75733,#75734,#75735,#75736,#75737,#75738,#75739,
#75740,#75741,#75742,#75743,#75744,#75745,#75746,#75747,#75748,#75749,#75750,
#75751,#75752,#75753,#75754,#75755,#75756,#75757,#75758,#75759,#75760,#75761,
#75762,#75763,#75764,#75765,#75766,#75767,#75768,#75769,#75770,#75771,#75772,
#75773,#75774,#75775,#75776,#75777,#75778,#75779,#75780,#75781,#75782,#75783,
#75784,#75785,#75786,#75787,#75788,#75789,#75790,#75791,#75792,#75793,#75794,
#75795,#75796,#75797,#75798,#75799,#75800,#75801,#75802,#75803,#75804,#75805,
#75806,#75807,#75808,#75809,#75810,#75811,#75812,#75813,#75814,#75815,#75816,
#75817,#75818,#75819,#75820,#75821,#75822,#75823,#75824,#75825,#75826,#75827,
#75828,#75829,#75830,#75831,#75832,#75833,#75834,#75835,#75836,#75837,#75838,
#75839,#75840,#75841,#75842,#75843,#75844,#75845,#75846,#75847,#75848,#75849,
#75850),.UNSPECIFIED.,.F.,.F.,(4,2,2,2,2,2,2,2,2,2,2,2,2,2,2,2,2,2,2,2,
2,2,2,2,2,2,2,2,2,2,2,2,2,2,2,2,2,2,2,2,2,2,2,2,2,2,2,2,2,2,2,2,2,2,2,2,
2,2,2,2,2,2,2,2,2,2,2,2,2,2,2,2,2,2,2,2,2,2,2,2,2,2,2,2,2,2,2,2,2,2,2,2,
2,2,2,2,2,2,2,2,2,2,2,2,2,2,2,2,2,2,2,2,4),(-1.40853711338947,-1.36768270255549,
-1.35578956926343,-1.35125426050673,-1.3479456909352,-1.34648313700913,
-1.34539838134693,-1.34420943539953,-1.34224339368389,-1.33583797627915,
-1.33428199270909,-1.31969474787633,-1.26065036180123,-1.24633998830998,
-1.2425781217769,-1.24036918321174,-1.23845643661397,-1.2361135976534,-1.23162645537363,
-1.19926315773716,-1.15907925242498,-1.15414634840198,-1.13819555014462,
-1.13557886251389,-1.13423207991095,-1.13316066320953,-1.13190319752587,
-1.12962637058364,-1.11824778254315,-1.09205969086143,-1.03933108993612,
-1.03241647585102,-1.02954634069093,-1.02775261667785,-1.02579143240917,
-1.02308659010719,-1.01667693114487,-0.988176704974518,-0.937243776280263,
-0.925759998176468,-0.923587350311914,-0.922222991473029,-0.921150292215095,
-0.919905852199562,-0.917688723844539,-0.907300008974863,-0.884808705648799,
-0.8264863374873,-0.820127956641291,-0.817631925077921,-0.815817166197529,
-0.813871711075465,-0.811257075627084,-0.805364991996072,-0.781011902670562,
-0.730339777255363,-0.714121237846193,-0.711492998487255,-0.71014378163785,
-0.709072270871095,-0.707816827755718,-0.705549074063951,-0.694326253900503,
-0.668747008170932,-0.615147894274237,-0.608301667084345,-0.60544289883552,
-0.603651322368631,-0.601688493056375,-0.598974045732415,-0.592506768400468,
-0.538333992281918,-0.502384842989942,-0.499521337710469,-0.498142551109291,
-0.497068604359849,-0.495834120598664,-0.493662197067835,-0.483954892154799,
-0.434970205919605,-0.399813904055265,-0.39552587454896,-0.392986701772883,
-0.391046314133845,-0.388972103828962,-0.385719494932899,-0.375374808873267,
-0.358738674649535,-0.325817684217832,-0.30777021760443,-0.290180233967672,
-0.287500587862765,-0.286140445965236,-0.285068237708011,-0.283821132051401,
-0.281591270946103,-0.270996363690899,-0.247766310106086,-0.192021882931062,
-0.184529990832604,-0.181562890210456,-0.179751487614206,-0.177920924583202,
-0.175416652164948,-0.17009691241572,-0.163034149925774,-0.145722466034039,
-0.0976541025404786,-0.0933269148221475,-0.0921194914598723,-0.0779498329751376,
-0.0756372155382893,-0.0747818727151328),.UNSPECIFIED.);
#799=B_SPLINE_CURVE_WITH_KNOTS('',3,(#75851,#75852,#75853,#75854,#75855,
#75856,#75857,#75858,#75859,#75860,#75861,#75862,#75863,#75864,#75865,#75866,
#75867,#75868,#75869,#75870,#75871,#75872,#75873,#75874,#75875,#75876,#75877,
#75878,#75879,#75880,#75881,#75882,#75883,#75884,#75885,#75886,#75887,#75888,
#75889,#75890,#75891,#75892,#75893,#75894,#75895,#75896,#75897,#75898,#75899,
#75900,#75901,#75902,#75903,#75904,#75905,#75906,#75907,#75908,#75909,#75910,
#75911,#75912,#75913,#75914,#75915,#75916,#75917,#75918,#75919,#75920,#75921,
#75922,#75923,#75924,#75925,#75926,#75927,#75928,#75929,#75930,#75931,#75932,
#75933,#75934,#75935,#75936,#75937,#75938,#75939,#75940,#75941,#75942,#75943,
#75944,#75945,#75946,#75947,#75948,#75949,#75950,#75951,#75952,#75953,#75954,
#75955,#75956,#75957,#75958,#75959,#75960,#75961,#75962,#75963,#75964,#75965,
#75966,#75967,#75968,#75969,#75970,#75971,#75972,#75973,#75974,#75975,#75976,
#75977,#75978,#75979,#75980,#75981,#75982,#75983,#75984,#75985,#75986,#75987,
#75988,#75989,#75990,#75991,#75992,#75993,#75994,#75995,#75996,#75997,#75998,
#75999,#76000,#76001,#76002,#76003,#76004,#76005,#76006,#76007,#76008,#76009,
#76010,#76011,#76012,#76013,#76014,#76015,#76016,#76017,#76018,#76019,#76020,
#76021,#76022,#76023,#76024,#76025,#76026,#76027,#76028,#76029,#76030,#76031,
#76032,#76033,#76034,#76035,#76036,#76037,#76038,#76039,#76040,#76041,#76042,
#76043,#76044,#76045,#76046,#76047,#76048,#76049,#76050,#76051,#76052,#76053,
#76054,#76055,#76056,#76057,#76058,#76059,#76060,#76061,#76062,#76063,#76064,
#76065,#76066,#76067,#76068,#76069,#76070,#76071,#76072,#76073,#76074,#76075,
#76076,#76077,#76078,#76079,#76080,#76081,#76082,#76083,#76084,#76085,#76086,
#76087,#76088,#76089,#76090,#76091,#76092,#76093,#76094,#76095,#76096,#76097,
#76098,#76099,#76100,#76101,#76102,#76103,#76104,#76105,#76106,#76107,#76108,
#76109,#76110,#76111,#76112,#76113,#76114,#76115,#76116,#76117,#76118,#76119,
#76120),.UNSPECIFIED.,.F.,.F.,(4,2,2,2,2,2,2,2,2,2,2,2,2,2,2,2,2,2,2,2,
2,2,2,2,2,2,2,2,2,2,2,2,2,2,2,2,2,2,2,2,2,2,2,2,2,2,2,2,2,2,2,2,2,2,2,2,
2,2,2,2,2,2,2,2,2,2,2,2,2,2,2,2,2,2,2,2,2,2,2,2,2,2,2,2,2,2,2,2,2,2,2,2,
2,2,2,2,2,2,2,2,2,2,2,2,2,2,2,2,2,2,2,2,2,2,2,2,2,2,2,2,2,2,2,2,2,2,2,2,
2,2,2,2,2,2,4),(-2.59341035609829,-2.57482973281229,-2.55598714875694,-2.54669214216968,
-2.54454925113748,-2.54332111565175,-2.54224610013818,-2.54085724135978,
-2.53794236515546,-2.50824565034493,-2.45779622037755,-2.44830716136627,
-2.44369986741691,-2.43992075424202,-2.43775004254392,-2.43773434805528,
-2.43771810100957,-2.43770128128463,-2.43768386804235,-2.4376658396592,
-2.43764717373721,-2.43762784707113,-2.43760783566919,-2.43758711458412,
-2.43756565797438,-2.43754343913426,-2.43752042968978,-2.43750039340549,
-2.43747704310926,-2.43744983674674,-2.43741814627615,-2.43738124537686,
-2.4373382957925,-2.43728408358569,-2.43534335946234,-2.43280134459612,
-2.42850316409415,-2.39338170488472,-2.34442283443053,-2.33472342946418,
-2.33255224903429,-2.33131801687544,-2.33024418441593,-2.32886539790547,
-2.32600140177476,-2.29004808887267,-2.25728170633324,-2.23472083343327,
-2.22906723249113,-2.22649601649929,-2.22455763260498,-2.22273101060838,
-2.22018921976626,-2.21354860988395,-2.15774103602243,-2.13368050345915,
-2.12285772072217,-2.12061382038051,-2.11936361505868,-2.11829168136597,
-2.11693565306005,-2.1147901015043,-2.10375313026405,-2.05253679571314,
-2.02382742289741,-2.01739370999166,-2.0146850384666,-2.01272337486551,
-2.01093079668361,-2.00806593103643,-2.00118177306371,-1.94810593027268,
-1.92219927649779,-1.91089225080458,-1.90861979607212,-1.90736339337595,
-1.90629206552154,-1.90494434847348,-1.90232277186784,-1.8862807194765,
-1.88099085656435,-1.86640570341081,-1.83351383751184,-1.81694698925262,
-1.80663459172248,-1.80338563809073,-1.8013122049657,-1.79937145384903,
-1.79683023388239,-1.79253525853405,-1.75742339526241,-1.70851920848977,
-1.6987482631656,-1.6965720165787,-1.69533659221617,-1.69426280339793,-1.69288548608946,
-1.69002940945599,-1.66723137756675,-1.61162104754378,-1.5956093759142,
-1.59183989743885,-1.58965142381957,-1.58773722178025,-1.58536794699408,
-1.58173459654937,-1.56463773712466,-1.55656865460642,-1.52175804244607,
-1.4977085530994,-1.48688900275794,-1.48464539097727,-1.48339529293298,
-1.4823234182358,-1.48096742224301,-1.47830713863393,-1.46125353870752,
-1.44264161588998,-1.4096854119617,-1.39304017869419,-1.38269247931452,
-1.37943955830635,-1.37736530758679,-1.37542499394027,-1.37288608028755,
-1.36859888349708,-1.33401767631518,-1.27805192423931,-1.2737780967122,
-1.27210652013368,-1.27109449105814,-1.26999215497845,-1.26842723567567,
-1.26451471126435,-1.25986135129038),.UNSPECIFIED.);
#800=B_SPLINE_CURVE_WITH_KNOTS('',3,(#76126,#76127,#76128,#76129,#76130,
#76131,#76132,#76133,#76134,#76135,#76136,#76137,#76138,#76139,#76140,#76141,
#76142,#76143),.UNSPECIFIED.,.F.,.F.,(4,2,2,2,2,2,2,2,4),(-0.0751187349318719,
-0.0651106329348145,-0.0603739125176121,-0.0579481082617559,-0.0560290964025899,
-0.0538784373609023,-0.0516517499321186,-0.048329966890634,-0.00062898517661497),
 .UNSPECIFIED.);
#801=B_SPLINE_CURVE_WITH_KNOTS('',3,(#76144,#76145,#76146,#76147,#76148,
#76149,#76150,#76151,#76152,#76153,#76154,#76155,#76156,#76157,#76158,#76159,
#76160,#76161,#76162,#76163,#76164,#76165,#76166,#76167,#76168,#76169,#76170,
#76171,#76172,#76173,#76174,#76175,#76176,#76177,#76178,#76179,#76180,#76181,
#76182,#76183,#76184,#76185,#76186,#76187,#76188,#76189,#76190,#76191,#76192,
#76193,#76194,#76195,#76196,#76197,#76198,#76199,#76200,#76201,#76202,#76203,
#76204,#76205,#76206,#76207,#76208,#76209,#76210,#76211,#76212,#76213,#76214,
#76215,#76216,#76217,#76218,#76219,#76220,#76221,#76222,#76223,#76224,#76225,
#76226,#76227,#76228,#76229,#76230,#76231,#76232,#76233,#76234,#76235,#76236,
#76237,#76238,#76239,#76240,#76241,#76242,#76243,#76244,#76245,#76246,#76247,
#76248,#76249,#76250,#76251,#76252,#76253,#76254,#76255,#76256,#76257,#76258,
#76259,#76260,#76261,#76262,#76263,#76264,#76265,#76266,#76267,#76268,#76269,
#76270,#76271,#76272,#76273,#76274,#76275,#76276,#76277,#76278,#76279,#76280,
#76281,#76282,#76283,#76284,#76285,#76286,#76287,#76288,#76289,#76290,#76291,
#76292,#76293,#76294,#76295,#76296,#76297,#76298,#76299,#76300,#76301,#76302,
#76303,#76304,#76305,#76306,#76307,#76308,#76309,#76310,#76311,#76312,#76313,
#76314,#76315,#76316,#76317,#76318,#76319,#76320,#76321,#76322,#76323,#76324,
#76325,#76326,#76327,#76328,#76329,#76330,#76331,#76332,#76333,#76334,#76335,
#76336,#76337,#76338,#76339,#76340,#76341,#76342,#76343,#76344,#76345,#76346,
#76347,#76348,#76349,#76350,#76351,#76352,#76353,#76354,#76355,#76356,#76357,
#76358,#76359,#76360,#76361,#76362,#76363,#76364,#76365,#76366,#76367,#76368,
#76369),.UNSPECIFIED.,.F.,.F.,(4,2,2,2,2,2,2,2,2,2,2,2,2,2,2,2,2,2,2,2,
2,2,2,2,2,2,2,2,2,2,2,2,2,2,2,2,2,2,2,2,2,2,2,2,2,2,2,2,2,2,2,2,2,2,2,2,
2,2,2,2,2,2,2,2,2,2,2,2,2,2,2,2,2,2,2,2,2,2,2,2,2,2,2,2,2,2,2,2,2,2,2,2,
2,2,2,2,2,2,2,2,2,2,2,2,2,2,2,2,2,2,2,2,4),(-2.66780309434801,-2.62484505800817,
-2.6219108313024,-2.62022793742123,-2.61872288020446,-2.61763118378487,
-2.61660377922286,-2.61485403788078,-2.61007939121883,-2.57261984535515,
-2.55119597702224,-2.52285730101152,-2.51638402150457,-2.51425965737376,
-2.512179581606,-2.51024060531169,-2.50771316384361,-2.50346695702633,-2.47124361159917,
-2.43574887781677,-2.41831569260106,-2.40949761061823,-2.40739741601031,
-2.40616906546414,-2.40509386011329,-2.40370475397877,-2.4007893512284,
-2.3710053731005,-2.32035366152312,-2.30620902996869,-2.30265828682094,
-2.3004738999177,-2.29855864866291,-2.29618207295407,-2.29252624039311,
-2.27509632343502,-2.22285291979168,-2.20601392043731,-2.19737612072976,
-2.19528248952006,-2.19406512069525,-2.19298788184882,-2.19160398401279,
-2.18931741368778,-2.17569419079213,-2.17392046746541,-2.166804715018,-2.12338057659755,
-2.10479361976828,-2.09359066569597,-2.09024276176984,-2.08814715216989,
-2.08621366946873,-2.08372147533988,-2.07959565232913,-2.05244999275112,
-2.01051591878271,-1.99390430985192,-1.98534395402353,-1.98325643172913,
-1.98204042008085,-1.9809629033154,-1.97957674056477,-1.97728247970232,
-1.96350060092353,-1.95214312780525,-1.91150136399021,-1.89282467746958,
-1.88158325256089,-1.87823124900663,-1.87613472058105,-1.8742015077424,
-1.87171122179838,-1.86759192826074,-1.84070506459315,-1.79874615663962,
-1.78195714237243,-1.7733362968348,-1.77124398859113,-1.77002690865292,
-1.76894960247881,-1.76756520202095,-1.76527694171419,-1.7516191663709,
-1.7498803364374,-1.70251038386924,-1.67153423136465,-1.66708202205485,
-1.6647462893385,-1.66283370643507,-1.66061862546172,-1.65683088348565,
-1.64223557993222,-1.62996945749286,-1.58955643563185,-1.57070181848982,
-1.5614025671802,-1.55925918133821,-1.55803084022124,-1.55695569556991,
-1.55556673707924,-1.5526518886144,-1.52381225837565,-1.48570039543634,
-1.46817383401427,-1.45743214822732,-1.45413430823221,-1.45204979445138,
-1.45011261740564,-1.4475959658139,-1.44338651476126,-1.41291090387463,
-1.40853711338947),.UNSPECIFIED.);
#802=B_SPLINE_CURVE_WITH_KNOTS('',3,(#76371,#76372,#76373,#76374,#76375,
#76376,#76377,#76378,#76379,#76380,#76381,#76382,#76383,#76384,#76385,#76386,
#76387,#76388,#76389,#76390,#76391,#76392,#76393,#76394,#76395,#76396,#76397,
#76398,#76399,#76400,#76401,#76402,#76403,#76404,#76405,#76406,#76407,#76408,
#76409,#76410,#76411,#76412,#76413,#76414,#76415,#76416,#76417,#76418,#76419,
#76420,#76421,#76422,#76423,#76424,#76425,#76426,#76427,#76428,#76429,#76430,
#76431,#76432,#76433,#76434,#76435,#76436,#76437,#76438,#76439,#76440,#76441,
#76442,#76443,#76444,#76445,#76446,#76447,#76448,#76449,#76450,#76451,#76452,
#76453,#76454,#76455,#76456,#76457,#76458,#76459,#76460,#76461,#76462,#76463,
#76464,#76465,#76466,#76467,#76468,#76469,#76470,#76471,#76472,#76473,#76474,
#76475,#76476,#76477,#76478,#76479,#76480,#76481,#76482,#76483,#76484,#76485,
#76486,#76487,#76488,#76489,#76490,#76491,#76492,#76493,#76494,#76495,#76496,
#76497,#76498,#76499,#76500,#76501,#76502,#76503,#76504,#76505,#76506,#76507,
#76508,#76509,#76510,#76511,#76512,#76513,#76514,#76515,#76516,#76517,#76518,
#76519,#76520,#76521,#76522,#76523,#76524,#76525,#76526,#76527,#76528,#76529,
#76530,#76531,#76532,#76533,#76534,#76535,#76536,#76537,#76538,#76539,#76540,
#76541,#76542,#76543,#76544,#76545,#76546,#76547,#76548,#76549,#76550,#76551,
#76552,#76553,#76554,#76555,#76556,#76557,#76558,#76559,#76560,#76561,#76562,
#76563,#76564,#76565,#76566,#76567,#76568,#76569,#76570,#76571,#76572,#76573,
#76574,#76575,#76576,#76577,#76578,#76579,#76580,#76581,#76582,#76583,#76584,
#76585,#76586,#76587,#76588,#76589,#76590,#76591,#76592,#76593,#76594,#76595,
#76596,#76597,#76598,#76599,#76600,#76601,#76602,#76603,#76604,#76605,#76606,
#76607,#76608,#76609,#76610,#76611,#76612,#76613,#76614,#76615,#76616,#76617,
#76618),.UNSPECIFIED.,.F.,.F.,(4,2,2,2,2,2,2,2,2,2,2,2,2,2,2,2,2,2,2,2,
2,2,2,2,2,2,2,2,2,2,2,2,2,2,2,2,2,2,2,2,2,2,2,2,2,2,2,2,2,2,2,2,2,2,2,2,
2,2,2,2,2,2,2,2,2,2,2,2,2,2,2,2,2,2,2,2,2,2,2,2,2,2,2,2,2,2,2,2,2,2,2,2,
2,2,2,2,2,2,2,2,2,2,2,2,2,2,2,2,2,2,2,2,2,2,2,2,2,2,2,2,2,2,2,4),(-1.25986135129038,
-1.24530241304872,-1.18892854063003,-1.17208345698105,-1.1684667484003,
-1.16610265211268,-1.16418885867655,-1.16199670869744,-1.15821041669407,
-1.14196381604285,-1.08448970814712,-1.0795172366509,-1.06353182564182,
-1.06091347502439,-1.05956642115189,-1.05849509636142,-1.05723809537606,
-1.05496301773918,-1.0436118759728,-1.01753002264744,-0.964659587630602,
-0.957756719319972,-0.954888708775274,-0.95309551240865,-0.951134262484446,
-0.948428152624589,-0.942009928704008,-0.913435225488642,-0.862239864547941,
-0.851079020293154,-0.848925868779101,-0.847567519096587,-0.846495407124745,
-0.845246902631221,-0.843010792420016,-0.832315998632985,-0.80872374665589,
-0.752156378070943,-0.745591532409124,-0.743061755128935,-0.741238306696934,
-0.739298245534177,-0.736716176795954,-0.731003276960136,-0.708004592533687,
-0.674986690410184,-0.653922324950132,-0.639428764806459,-0.637099290227801,
-0.635703054238043,-0.634624587936592,-0.633415201032819,-0.631356176608807,
-0.623141284813286,-0.607518365865643,-0.565765413269225,-0.537118824493238,
-0.532954837851641,-0.530451971739961,-0.528517507706292,-0.526428089253623,
-0.523105719214729,-0.512132575251355,-0.494077374872629,-0.443985019031152,
-0.427602851320191,-0.424968414734493,-0.423617988860906,-0.422546549653114,
-0.421292383098954,-0.419029949548998,-0.407894034232583,-0.382647589360761,
-0.328577165374617,-0.321772203085985,-0.318920524702571,-0.317130429035644,
-0.315166827285759,-0.312446895803623,-0.305945402103554,-0.27666548529029,
-0.229654393283906,-0.21545674752028,-0.2129408363912,-0.211630983235744,
-0.210618633622361,-0.210611043586414,-0.210603596973413,-0.21059628534332,
-0.210589100829224,-0.210582036068197,-0.210575084198925,-0.210568238859746,
-0.210561494134435,-0.210554844443709,-0.210548284498576,-0.210541809366055,
-0.210535414439193,-0.210529095285272,-0.210522847770718,-0.210516667985328,
-0.210510552242024,-0.210504496979383,-0.210498498772053,-0.210492554419833,
-0.210486660957257,-0.210480815489451,-0.209218763863868,-0.206836299392488,
-0.193388069173711,-0.157802414423416,-0.113366775909924,-0.109089434563902,
-0.106553571364546,-0.104613969153839,-0.102538903441034,-0.0992814031391307,
-0.0888910015985643,-0.0721524541642749,-0.0417417147298587,-0.00539305727599119,
-0.00193455410719084,-0.000863977557054734,-0.000629065414789221),
 .UNSPECIFIED.);
#803=B_SPLINE_CURVE_WITH_KNOTS('',3,(#76619,#76620,#76621,#76622,#76623,
#76624,#76625,#76626,#76627,#76628,#76629,#76630,#76631,#76632,#76633,#76634),
 .UNSPECIFIED.,.F.,.F.,(4,3,3,3,3,4),(-28.973780262141,-28.9662570488944,
-28.8628842312467,-28.7596459043877,-28.6565264336552,-28.6232428442244),
 .UNSPECIFIED.);
#804=B_SPLINE_CURVE_WITH_KNOTS('',3,(#76639,#76640,#76641,#76642,#76643,
#76644,#76645,#76646,#76647,#76648,#76649,#76650,#76651,#76652,#76653,#76654,
#76655,#76656,#76657,#76658,#76659,#76660,#76661,#76662,#76663,#76664,#76665,
#76666,#76667,#76668,#76669,#76670,#76671,#76672,#76673,#76674,#76675,#76676,
#76677,#76678,#76679,#76680,#76681,#76682,#76683,#76684,#76685,#76686,#76687,
#76688,#76689,#76690,#76691,#76692,#76693,#76694,#76695,#76696,#76697,#76698,
#76699,#76700,#76701,#76702,#76703,#76704,#76705,#76706,#76707,#76708,#76709,
#76710,#76711,#76712,#76713,#76714,#76715,#76716,#76717,#76718,#76719,#76720,
#76721,#76722,#76723,#76724,#76725,#76726,#76727,#76728,#76729,#76730,#76731,
#76732,#76733,#76734,#76735,#76736,#76737,#76738,#76739,#76740,#76741,#76742,
#76743,#76744,#76745,#76746,#76747,#76748,#76749,#76750,#76751,#76752,#76753,
#76754,#76755,#76756,#76757,#76758,#76759,#76760,#76761,#76762,#76763,#76764,
#76765,#76766,#76767,#76768,#76769,#76770,#76771,#76772,#76773,#76774,#76775,
#76776,#76777,#76778,#76779,#76780,#76781,#76782,#76783,#76784,#76785,#76786,
#76787,#76788,#76789,#76790,#76791,#76792,#76793,#76794,#76795,#76796,#76797,
#76798,#76799,#76800,#76801,#76802,#76803,#76804,#76805,#76806,#76807,#76808,
#76809,#76810,#76811,#76812,#76813,#76814,#76815,#76816,#76817,#76818,#76819,
#76820,#76821,#76822,#76823,#76824,#76825,#76826,#76827,#76828,#76829,#76830,
#76831,#76832,#76833,#76834,#76835,#76836,#76837,#76838,#76839,#76840,#76841,
#76842,#76843,#76844,#76845,#76846,#76847,#76848,#76849,#76850,#76851,#76852,
#76853,#76854,#76855,#76856,#76857,#76858,#76859,#76860,#76861,#76862,#76863,
#76864,#76865,#76866,#76867,#76868),.UNSPECIFIED.,.F.,.F.,(4,2,2,2,2,2,
2,2,2,2,2,2,2,2,2,2,2,2,2,2,2,2,2,2,2,2,2,2,2,2,2,2,2,2,2,2,2,2,2,2,2,2,
2,2,2,2,2,2,2,2,2,2,2,2,2,2,2,2,2,2,2,2,2,2,2,2,2,2,2,2,2,2,2,2,2,2,2,2,
2,2,2,2,2,2,2,2,2,2,2,2,2,2,2,2,2,2,2,2,2,2,2,2,2,2,2,2,2,2,2,2,2,2,2,2,
4),(-1.40851932798763,-1.36251967303565,-1.34496387376542,-1.33420949748336,
-1.33091039297545,-1.32882568929973,-1.32688875653648,-1.32432953104823,
-1.31874292200313,-1.31131943588228,-1.29271751926307,-1.24998826934857,
-1.22736039816029,-1.22450822663683,-1.22313156801119,-1.22205771318169,
-1.22082156654236,-1.21864248629277,-1.20883325900351,-1.1599279269835,
-1.12480863003436,-1.12051293205289,-1.11797138246468,-1.11603042508517,
-1.11395681478208,-1.11070767248791,-1.1003953416141,-1.08383154118467,
-1.05096823261267,-1.03714008214105,-1.03049000477807,-1.01501639385347,
-1.01241930562685,-1.01107679765891,-1.01000570146705,-1.00874502699915,
-1.00645320871981,-0.994806460469776,-0.967539938546587,-0.947355528278572,
-0.912847748863482,-0.90856105700415,-0.906022142483153,-0.904081644289435,
-0.90200701681872,-0.898753128330105,-0.888399074567619,-0.871742815617945,
-0.838803247362783,-0.820076463512285,-0.803165902003435,-0.800510799090681,
-0.799155821086824,-0.798083909006519,-0.796832804582979,-0.794584968412347,
-0.783698952920323,-0.759401470361552,-0.703906144516429,-0.697230212082474,
-0.694682827186489,-0.692854664646051,-0.690916922843327,-0.688350416764518,
-0.682722825640793,-0.675230048959998,-0.656373513318399,-0.626172116799537,
-0.603803549513684,-0.590878592279148,-0.588627399430395,-0.587239420040068,
-0.586164651678936,-0.58493632280847,-0.582791965444088,-0.573473453360424,
-0.524286329905296,-0.488922121577425,-0.484624198957251,-0.482082301351664,
-0.480141635517877,-0.478068876837535,-0.474822196268678,-0.464527172285693,
-0.448000188859423,-0.417117631706392,-0.397781521153882,-0.379330553425616,
-0.37658873622334,-0.375234258339661,-0.374162591387321,-0.372911599748906,
-0.370663532494245,-0.360092078763205,-0.336830824961793,-0.28752854758086,
-0.275018187417155,-0.271389981246374,-0.269232925473199,-0.267506777687011,
-0.265182988966667,-0.261107434718789,-0.240159355657591,-0.199117570020485,
-0.167650338839419,-0.164739213826966,-0.163351351009537,-0.162276738228571,
-0.161048660238643,-0.159756431943822,-0.155106585482959,-0.128864138723284,
-0.106990698897584,-0.105541851048307,-0.0751187349318719),
 .UNSPECIFIED.);
#805=B_SPLINE_CURVE_WITH_KNOTS('',3,(#76870,#76871,#76872,#76873,#76874,
#76875,#76876,#76877,#76878,#76879,#76880,#76881,#76882,#76883,#76884,#76885,
#76886,#76887,#76888,#76889,#76890,#76891,#76892,#76893,#76894,#76895,#76896,
#76897,#76898,#76899,#76900,#76901,#76902,#76903,#76904,#76905,#76906,#76907,
#76908,#76909,#76910,#76911,#76912,#76913,#76914,#76915,#76916,#76917,#76918,
#76919,#76920,#76921,#76922,#76923,#76924,#76925,#76926,#76927,#76928,#76929,
#76930,#76931,#76932,#76933,#76934,#76935,#76936,#76937,#76938,#76939,#76940,
#76941,#76942,#76943,#76944,#76945,#76946,#76947,#76948,#76949,#76950,#76951,
#76952,#76953,#76954,#76955,#76956,#76957,#76958,#76959,#76960,#76961,#76962,
#76963,#76964,#76965,#76966,#76967,#76968,#76969,#76970,#76971,#76972,#76973,
#76974,#76975,#76976,#76977,#76978,#76979,#76980,#76981,#76982,#76983,#76984,
#76985,#76986,#76987,#76988,#76989,#76990,#76991,#76992,#76993,#76994,#76995,
#76996,#76997,#76998,#76999,#77000,#77001,#77002,#77003,#77004,#77005,#77006,
#77007,#77008,#77009,#77010,#77011,#77012,#77013,#77014,#77015,#77016,#77017,
#77018,#77019,#77020,#77021,#77022,#77023,#77024,#77025,#77026,#77027,#77028,
#77029,#77030,#77031,#77032,#77033,#77034,#77035,#77036,#77037,#77038,#77039,
#77040,#77041,#77042,#77043,#77044,#77045,#77046,#77047,#77048,#77049,#77050),
 .UNSPECIFIED.,.F.,.F.,(4,3,3,3,3,3,3,3,3,3,3,3,3,3,3,3,3,3,3,3,3,3,3,3,
3,3,3,3,3,3,3,3,3,3,3,3,3,3,3,3,3,3,3,3,3,3,3,3,3,3,3,3,3,3,3,3,3,3,3,3,
4),(-28.6232428442244,-28.520202111683,-28.4171817669707,-28.3141478226609,
-28.2110002317942,-28.1077864632061,-28.0043998658756,-27.9674205989325,
-27.864025861899,-27.7607845797986,-27.6576646144211,-27.5546100462272,
-27.4515868378845,-27.3485609952271,-27.2454282284641,-27.1422391370695,
-27.0388671437029,-26.9685841489706,-26.8651894118466,-26.7619481296554,
-26.658828164187,-26.555773595902,-26.4527503874685,-26.3497245447204,-26.2465917778677,
-26.1434026863838,-26.0400306929296,-25.9697476990087,-25.8663529620658,
-25.7631116800555,-25.659991714767,-25.5569371466611,-25.4539139384057,
-25.3508880958346,-25.2477553291558,-25.1445662378443,-25.0411942445581,
-24.9709112490469,-24.8675165120622,-24.7642752300117,-24.6611552646857,
-24.558100696544,-24.4550774882544,-24.3520516456508,-24.2489188789423,
-24.1457297876027,-24.0423577942913,-23.972074799085,-23.8686800615155,
-23.7654387788772,-23.6623188129617,-23.5592642442299,-23.4562410353503,
-23.3532151921577,-23.2500824248659,-23.1468933329451,-23.0435213390625,
-22.9732383491231,-22.8444301460781,-22.7177283292995,-22.6905949549614),
 .UNSPECIFIED.);
#806=B_SPLINE_CURVE_WITH_KNOTS('',3,(#77051,#77052,#77053,#77054),
 .UNSPECIFIED.,.F.,.F.,(4,4),(-22.6905949549614,-22.3411473213039),
 .UNSPECIFIED.);
#807=B_SPLINE_CURVE_WITH_KNOTS('',3,(#77060,#77061,#77062,#77063,#77064,
#77065,#77066,#77067,#77068,#77069,#77070,#77071,#77072,#77073,#77074,#77075,
#77076,#77077),.UNSPECIFIED.,.F.,.F.,(4,2,2,2,2,2,2,2,4),(-0.0747374607281607,
-0.0441237834881369,-0.0412117014333899,-0.039823612314504,-0.0387489300670153,
-0.0375208908713778,-0.0362287404382341,-0.034250737200593,-0.000628702685456983),
 .UNSPECIFIED.);
#808=B_SPLINE_CURVE_WITH_KNOTS('',3,(#77078,#77079,#77080,#77081,#77082,
#77083,#77084,#77085,#77086,#77087,#77088,#77089,#77090,#77091,#77092,#77093,
#77094,#77095,#77096,#77097,#77098,#77099,#77100,#77101,#77102,#77103,#77104,
#77105,#77106,#77107,#77108,#77109,#77110,#77111,#77112,#77113,#77114,#77115,
#77116,#77117,#77118,#77119,#77120,#77121,#77122,#77123,#77124,#77125,#77126,
#77127,#77128,#77129,#77130,#77131,#77132,#77133,#77134,#77135,#77136,#77137,
#77138,#77139,#77140,#77141,#77142,#77143,#77144,#77145,#77146,#77147,#77148,
#77149,#77150,#77151,#77152,#77153,#77154,#77155,#77156,#77157,#77158,#77159,
#77160,#77161,#77162,#77163,#77164,#77165,#77166,#77167,#77168,#77169,#77170,
#77171,#77172,#77173,#77174,#77175,#77176,#77177,#77178,#77179,#77180,#77181,
#77182,#77183,#77184,#77185,#77186,#77187,#77188,#77189,#77190,#77191,#77192,
#77193,#77194,#77195,#77196,#77197,#77198,#77199,#77200,#77201,#77202,#77203,
#77204,#77205,#77206,#77207,#77208,#77209,#77210,#77211,#77212,#77213,#77214,
#77215,#77216,#77217,#77218,#77219,#77220,#77221,#77222,#77223,#77224,#77225,
#77226,#77227,#77228,#77229,#77230,#77231,#77232,#77233,#77234,#77235,#77236,
#77237,#77238,#77239,#77240,#77241,#77242,#77243,#77244,#77245,#77246,#77247,
#77248,#77249,#77250,#77251,#77252,#77253,#77254,#77255,#77256,#77257,#77258,
#77259,#77260,#77261,#77262,#77263,#77264,#77265,#77266,#77267,#77268,#77269,
#77270,#77271,#77272,#77273,#77274,#77275,#77276,#77277,#77278,#77279,#77280,
#77281,#77282,#77283,#77284,#77285,#77286,#77287,#77288,#77289,#77290,#77291,
#77292,#77293,#77294,#77295),.UNSPECIFIED.,.F.,.F.,(4,2,2,2,2,2,2,2,2,2,
2,2,2,2,2,2,2,2,2,2,2,2,2,2,2,2,2,2,2,2,2,2,2,2,2,2,2,2,2,2,2,2,2,2,2,2,
2,2,2,2,2,2,2,2,2,2,2,2,2,2,2,2,2,2,2,2,2,2,2,2,2,2,2,2,2,2,2,2,2,2,2,2,
2,2,2,2,2,2,2,2,2,2,2,2,2,2,2,2,2,2,2,2,2,2,2,2,2,2,4),(-2.66809505953643,
-2.63761331797238,-2.61110679367198,-2.60494080474704,-2.60227773168817,
-2.60032396047389,-2.59852101349307,-2.59560062553725,-2.58838442381747,
-2.54313761767022,-2.52325627693072,-2.50675385428201,-2.49825766913804,
-2.49621111536066,-2.49497891808633,-2.49390458241747,-2.49252216605694,
-2.48964027606611,-2.45494094605814,-2.41403106020496,-2.3955778961565,
-2.39164569804701,-2.38942139223529,-2.38770157987476,-2.38545882655125,
-2.38154963844257,-2.36550449479325,-2.3555748840692,-2.30780578460153,
-2.29374492971221,-2.28865990585603,-2.28504323286418,-2.28352703141438,
-2.28243359063611,-2.28140957725044,-2.27967633134623,-2.27500874914261,
-2.23339056871752,-2.18625557675148,-2.1806587311454,-2.17809785516819,
-2.17616092327188,-2.17433098820525,-2.17177704313981,-2.16505870553325,
-2.11003460213544,-2.0854500870359,-2.07448670070358,-2.07223421363577,
-2.0709820761646,-2.06991023822469,-2.06855657487153,-2.06581977354791,
-2.04754250227878,-2.02956943461586,-1.99683442078875,-1.97432717202141,
-1.96868039576043,-1.96611017807903,-1.96417168923076,-1.96234433782488,
-1.95980051954979,-1.95314856270812,-1.89742903710516,-1.87330086627225,
-1.86245912606583,-1.86021381154727,-1.85896317051981,-1.85789108033303,
-1.85653513247731,-1.8543902297512,-1.84336766854611,-1.79206530561104,
-1.76340168823991,-1.75697292436754,-1.75426481789332,-1.75230301221034,
-1.75050992491119,-1.7476434204999,-1.74075104945696,-1.68775845932275,
-1.66178343541008,-1.65045820460074,-1.64818443419826,-1.64692761884622,
-1.64585613017212,-1.64450845403046,-1.64188767231965,-1.62586303094119,
-1.62045980395024,-1.60595976788558,-1.57306342699952,-1.5503064766965,
-1.54462578573184,-1.54204923540293,-1.54010966288761,-1.53828399832293,
-1.53574686781244,-1.529138078458,-1.47298732082922,-1.4491376820485,-1.4383709681625,
-1.43613010296641,-1.43488037942495,-1.43380811217426,-1.4324507032515,
-1.42978489789984,-1.41259793855704,-1.40851932798763),.UNSPECIFIED.);
#809=B_SPLINE_CURVE_WITH_KNOTS('',3,(#77297,#77298,#77299,#77300,#77301,
#77302,#77303,#77304,#77305,#77306),.UNSPECIFIED.,.F.,.F.,(4,1,1,1,1,1,
1,4),(-22.3411473213039,-21.9744018991612,-20.9755654491994,-19.9767289992375,
-18.9778925492756,-17.9790560993137,-16.9802196493519,-16.4074096477818),
 .UNSPECIFIED.);
#810=B_SPLINE_CURVE_WITH_KNOTS('',3,(#77307,#77308,#77309,#77310,#77311,
#77312),.UNSPECIFIED.,.F.,.F.,(4,2,4),(-2.66742168182414,-2.60891631380292,
-2.59315594400309),.UNSPECIFIED.);
#811=B_SPLINE_CURVE_WITH_KNOTS('',3,(#77317,#77318,#77319,#77320,#77321,
#77322,#77323,#77324,#77325,#77326,#77327,#77328,#77329,#77330,#77331,#77332,
#77333,#77334,#77335,#77336,#77337,#77338,#77339,#77340,#77341,#77342,#77343,
#77344,#77345,#77346,#77347,#77348,#77349,#77350,#77351,#77352,#77353,#77354,
#77355,#77356,#77357,#77358,#77359,#77360,#77361,#77362,#77363,#77364,#77365,
#77366,#77367,#77368,#77369,#77370,#77371,#77372,#77373,#77374,#77375,#77376,
#77377,#77378,#77379,#77380,#77381,#77382,#77383,#77384,#77385,#77386,#77387,
#77388,#77389,#77390,#77391,#77392,#77393,#77394,#77395,#77396,#77397,#77398,
#77399,#77400,#77401,#77402,#77403,#77404,#77405,#77406,#77407,#77408,#77409,
#77410,#77411,#77412,#77413,#77414,#77415,#77416,#77417,#77418,#77419,#77420,
#77421,#77422,#77423,#77424,#77425,#77426,#77427,#77428,#77429,#77430,#77431,
#77432,#77433,#77434,#77435,#77436,#77437,#77438,#77439,#77440,#77441,#77442,
#77443,#77444,#77445,#77446,#77447,#77448,#77449,#77450,#77451,#77452,#77453,
#77454,#77455,#77456,#77457,#77458,#77459,#77460,#77461,#77462,#77463,#77464,
#77465,#77466,#77467,#77468,#77469,#77470,#77471,#77472,#77473,#77474,#77475,
#77476,#77477,#77478,#77479,#77480,#77481,#77482,#77483,#77484,#77485,#77486,
#77487,#77488,#77489,#77490,#77491,#77492,#77493,#77494,#77495,#77496,#77497,
#77498,#77499,#77500,#77501,#77502,#77503,#77504,#77505,#77506,#77507,#77508,
#77509,#77510,#77511,#77512,#77513,#77514,#77515,#77516,#77517,#77518,#77519,
#77520,#77521,#77522,#77523,#77524,#77525,#77526,#77527,#77528,#77529,#77530,
#77531,#77532,#77533,#77534,#77535,#77536,#77537,#77538,#77539,#77540),
 .UNSPECIFIED.,.F.,.F.,(4,2,2,2,2,2,2,2,2,2,2,2,2,2,2,2,2,2,2,2,2,2,2,2,
2,2,2,2,2,2,2,2,2,2,2,2,2,2,2,2,2,2,2,2,2,2,2,2,2,2,2,2,2,2,2,2,2,2,2,2,
2,2,2,2,2,2,2,2,2,2,2,2,2,2,2,2,2,2,2,2,2,2,2,2,2,2,2,2,2,2,2,2,2,2,2,2,
2,2,2,2,2,2,2,2,2,2,2,2,2,2,2,4),(-1.40821110954925,-1.36481848480488,-1.33376867328224,
-1.31571878383699,-1.3130231632549,-1.31165951849834,-1.31058689517225,
-1.30934198277219,-1.30712267449558,-1.29669950717846,-1.27408620769441,
-1.21596233875948,-1.20957870649379,-1.20707845656185,-1.20526260397841,
-1.20331782760757,-1.20070732681518,-1.19483829682318,-1.17066188426138,
-1.12017878610895,-1.11974730187484,-1.10356130443534,-1.10093436984525,
-1.09958543134425,-1.09851394096311,-1.09725829142831,-1.094989560096,-1.08374965241037,
-1.05810385593581,-1.00460239693588,-0.997748372498273,-0.99488833896926,
-0.993096547627768,-0.991133948949955,-0.988420677784727,-0.981960289021308,
-0.928025358577391,-0.891815848873303,-0.888961284076015,-0.887584262790791,
-0.886510497564794,-0.885274874791088,-0.883097727008738,-0.873313951073665,
-0.824394671026784,-0.789272994150639,-0.784977762009422,-0.782436516651152,
-0.780495808128905,-0.778422479733483,-0.775173812713509,-0.764863274195816,
-0.748302625280135,-0.715444393115923,-0.701701467686459,-0.694857451113974,
-0.694560814745629,-0.689297374813233,-0.678994931801532,-0.67689672763898,
-0.67555521898923,-0.674484310308509,-0.67322314550023,-0.670928611783269,
-0.659228920618754,-0.610479424775481,-0.577268525378623,-0.573005111433949,
-0.570473225836644,-0.568534188769422,-0.566457314082085,-0.563191904701132,
-0.552732891845996,-0.535841971849385,-0.498075526237576,-0.467987735292297,
-0.46507417533318,-0.463685786240215,-0.462611058561022,-0.461383177084474,
-0.459240536492632,-0.44994394434002,-0.431091130978925,-0.387350906491365,
-0.364762305076266,-0.36081450918857,-0.35834922620885,-0.356425700266068,
-0.354297426069673,-0.350799315329481,-0.338078592183232,-0.315779294387565,
-0.265694685127626,-0.255118673220226,-0.253002573467255,-0.251655635915973,
-0.250584471026185,-0.249327735780924,-0.247099073363263,-0.236376527994363,
-0.212617559794168,-0.186546611322787,-0.153396864493389,-0.149134572932028,
-0.146603014355765,-0.144664031112807,-0.142587022380962,-0.13932099922551,
-0.128856559433987,-0.098549695579791,-0.0750525798539899,-0.0747374607281607),
 .UNSPECIFIED.);
#812=B_SPLINE_CURVE_WITH_KNOTS('',3,(#77541,#77542,#77543,#77544,#77545,
#77546,#77547,#77548,#77549,#77550,#77551,#77552,#77553,#77554,#77555,#77556,
#77557,#77558,#77559,#77560,#77561,#77562,#77563,#77564,#77565,#77566,#77567,
#77568,#77569,#77570,#77571,#77572,#77573,#77574,#77575,#77576,#77577,#77578,
#77579,#77580,#77581,#77582,#77583,#77584,#77585,#77586,#77587,#77588,#77589,
#77590,#77591,#77592,#77593,#77594,#77595,#77596,#77597,#77598,#77599,#77600,
#77601,#77602,#77603,#77604,#77605,#77606,#77607,#77608,#77609,#77610,#77611,
#77612,#77613,#77614,#77615,#77616,#77617,#77618,#77619,#77620,#77621,#77622,
#77623,#77624,#77625,#77626,#77627,#77628,#77629,#77630,#77631,#77632,#77633,
#77634,#77635,#77636,#77637,#77638,#77639,#77640,#77641,#77642,#77643,#77644,
#77645,#77646,#77647,#77648,#77649,#77650,#77651,#77652,#77653,#77654,#77655,
#77656,#77657,#77658,#77659,#77660,#77661,#77662,#77663,#77664,#77665,#77666,
#77667,#77668,#77669,#77670,#77671,#77672,#77673,#77674,#77675,#77676,#77677,
#77678,#77679,#77680,#77681,#77682,#77683,#77684,#77685,#77686,#77687,#77688,
#77689,#77690,#77691,#77692,#77693,#77694,#77695,#77696,#77697,#77698,#77699,
#77700,#77701,#77702,#77703,#77704,#77705,#77706,#77707,#77708,#77709,#77710,
#77711,#77712,#77713,#77714,#77715,#77716,#77717,#77718,#77719,#77720,#77721,
#77722,#77723,#77724,#77725,#77726,#77727,#77728,#77729,#77730,#77731,#77732,
#77733,#77734,#77735,#77736,#77737,#77738,#77739,#77740,#77741,#77742,#77743,
#77744,#77745,#77746,#77747,#77748,#77749,#77750,#77751,#77752,#77753,#77754,
#77755,#77756,#77757,#77758,#77759,#77760,#77761,#77762,#77763,#77764,#77765,
#77766,#77767,#77768,#77769,#77770,#77771,#77772,#77773,#77774),
 .UNSPECIFIED.,.F.,.F.,(4,2,2,2,2,2,2,2,2,2,2,2,2,2,2,2,2,2,2,2,2,2,2,2,
2,2,2,2,2,2,2,2,2,2,2,2,2,2,2,2,2,2,2,2,2,2,2,2,2,2,2,2,2,2,2,2,2,2,2,2,
2,2,2,2,2,2,2,2,2,2,2,2,2,2,2,2,2,2,2,2,2,2,2,2,2,2,2,2,2,2,2,2,2,2,2,2,
2,2,2,2,2,2,2,2,2,2,2,2,2,2,2,2,2,2,2,2,4),(-2.59315594400309,-2.59007763676982,
-2.58078446061555,-2.57864196520466,-2.57741405225984,-2.57633922941941,
-2.5749506167247,-2.57203624597322,-2.54226102741123,-2.49162485054994,
-2.48229405620474,-2.47774234381657,-2.47500421303992,-2.47252001085952,
-2.47064395111727,-2.46881749761626,-2.46627614977761,-2.45963793926299,
-2.40382814330879,-2.37977008790781,-2.36894815909931,-2.36670437657868,
-2.36545422852822,-2.36438233142897,-2.36302633592252,-2.36088082150167,
-2.34984370284795,-2.29863021710051,-2.26992299265595,-2.26348965060112,
-2.26078109769207,-2.25881950609727,-2.25702698407049,-2.25416218694483,
-2.24727808144986,-2.19420980221626,-2.16830033475109,-2.15699278329242,
-2.15472036203695,-2.1534639964676,-2.15239272448482,-2.15104510379787,
-2.14842375920586,-2.13238380037999,-2.12707356947599,-2.11250757331232,
-2.07961724050441,-2.06305113666004,-2.05273923107956,-2.0494904567036,
-2.04741714448578,-2.04547651132128,-2.04293545297379,-2.03864076775904,
-2.00353490506159,-1.9546512443564,-1.94486004465277,-1.94268250720782,
-1.94144684564022,-1.94037316729637,-1.93899640786898,-1.93614292224175,
-1.91344482323367,-1.87272167211962,-1.84568035402812,-1.83944843091071,
-1.83677410159091,-1.83481850808743,-1.83301838099935,-1.83011257507762,
-1.82298217100003,-1.77422999705428,-1.73505270581902,-1.73147804015649,
-1.72996902809197,-1.7288768636613,-1.72785087752937,-1.726107663268,-1.72137458018872,
-1.68179593316283,-1.63388990738188,-1.62749310795193,-1.62479053302431,
-1.62282984151228,-1.6210357776119,-1.61816336034547,-1.61123422155785,
-1.55875529170381,-1.53242870486769,-1.52101503587405,-1.51873640302925,
-1.51747861988341,-1.51640744685222,-1.51506158455075,-1.51244823884046,
-1.4965682580066,-1.49069794729026,-1.44666701985389,-1.42810815465924,
-1.41691845401453,-1.41357286054019,-1.41147833468581,-1.40954560736701,
-1.40705404720522,-1.40292854512582,-1.37574265136433,-1.33373204563628,
-1.32763512663023,-1.30978754833016,-1.30709916347252,-1.30573723480036,
-1.30466495358076,-1.30341928440853,-1.30119586157112,-1.29070305630196,
-1.26784056700131,-1.25960928830829),.UNSPECIFIED.);
#813=B_SPLINE_CURVE_WITH_KNOTS('',3,(#77780,#77781,#77782,#77783,#77784,
#77785,#77786,#77787,#77788,#77789,#77790,#77791,#77792,#77793,#77794,#77795,
#77796,#77797,#77798,#77799,#77800,#77801,#77802,#77803,#77804,#77805,#77806,
#77807,#77808,#77809,#77810,#77811,#77812,#77813,#77814,#77815,#77816,#77817,
#77818,#77819,#77820,#77821,#77822,#77823,#77824,#77825,#77826,#77827,#77828,
#77829,#77830,#77831,#77832,#77833,#77834,#77835,#77836,#77837,#77838,#77839,
#77840,#77841,#77842,#77843,#77844,#77845,#77846,#77847,#77848,#77849,#77850,
#77851,#77852,#77853,#77854,#77855,#77856,#77857,#77858,#77859,#77860,#77861,
#77862,#77863,#77864,#77865,#77866,#77867,#77868,#77869,#77870,#77871,#77872,
#77873,#77874,#77875,#77876,#77877,#77878,#77879,#77880,#77881,#77882,#77883,
#77884,#77885),.UNSPECIFIED.,.F.,.F.,(4,3,3,3,3,3,3,3,3,3,3,3,3,3,3,3,3,
3,3,3,3,3,3,3,3,3,3,3,3,3,3,3,3,3,3,4),(-3.49054210138362,-3.38888729762208,
-3.28714621677665,-3.18536357729934,-3.08340265109612,-2.99650934988562,
-2.89298815672403,-2.7896179644128,-2.68636610744677,-2.58317789200706,
-2.48001949625459,-2.37685713986045,-2.27358681231221,-2.17025936584281,
-2.06674931475237,-1.99767289992375,-1.8953694703404,-1.79322009387015,
-1.69118812153633,-1.58921885584019,-1.48727693124249,-1.38532702267508,
-1.28325476444039,-1.1811195089167,-1.07877855598727,-0.998836449961877,
-0.892562814926303,-0.780992463060515,-0.675072152100643,-0.569251436963408,
-0.463502577326272,-0.357797922575414,-0.252080134297595,-0.146357262849723,
-0.0405614307760777,0.),.UNSPECIFIED.);
#814=B_SPLINE_CURVE_WITH_KNOTS('',3,(#77888,#77889,#77890,#77891,#77892,
#77893,#77894,#77895,#77896,#77897,#77898,#77899,#77900,#77901,#77902,#77903,
#77904,#77905,#77906,#77907,#77908,#77909,#77910,#77911,#77912,#77913,#77914,
#77915,#77916,#77917,#77918,#77919,#77920,#77921,#77922,#77923,#77924,#77925,
#77926,#77927,#77928,#77929,#77930,#77931,#77932,#77933,#77934,#77935,#77936,
#77937,#77938,#77939,#77940,#77941,#77942,#77943,#77944,#77945,#77946,#77947,
#77948,#77949,#77950,#77951,#77952,#77953,#77954,#77955,#77956,#77957,#77958,
#77959,#77960,#77961,#77962,#77963,#77964,#77965,#77966,#77967,#77968,#77969,
#77970,#77971,#77972,#77973,#77974,#77975,#77976,#77977,#77978,#77979,#77980,
#77981,#77982,#77983,#77984,#77985,#77986,#77987,#77988,#77989,#77990,#77991,
#77992,#77993,#77994,#77995,#77996,#77997,#77998,#77999,#78000,#78001,#78002,
#78003,#78004,#78005,#78006,#78007,#78008,#78009,#78010,#78011,#78012,#78013,
#78014,#78015,#78016,#78017,#78018,#78019,#78020,#78021,#78022,#78023,#78024,
#78025,#78026,#78027,#78028,#78029,#78030,#78031,#78032,#78033,#78034,#78035,
#78036,#78037,#78038,#78039,#78040,#78041,#78042,#78043,#78044,#78045,#78046,
#78047),.UNSPECIFIED.,.F.,.F.,(4,3,3,3,3,3,3,3,3,3,3,3,3,3,3,3,3,3,3,3,
3,3,3,3,3,3,3,3,3,3,3,3,3,3,3,3,3,3,3,3,3,3,3,3,3,3,3,3,3,3,3,3,3,4),(2.00878451684803,
2.11210413325302,2.21527034106229,2.31831513543173,2.42129472868222,2.52424326611283,
2.62719484999974,2.73025123525842,2.83336461674476,2.93665426095923,2.99650934988563,
3.10008234864184,3.20350565405814,3.30681236784359,3.41005649077515,3.51327177809592,
3.61649194455096,3.7198211439703,3.82320814715696,3.92677824242681,3.9953457998475,
4.09860802522565,4.20171488656681,4.30469822083938,4.40761486436263,4.51049905109401,
4.61338497056926,4.71637738346395,4.8194256584024,4.92265765146998,4.99418224980938,
5.09760362616702,5.20087164810089,5.30401837089659,5.40709969299369,5.51014961192936,
5.61320208205146,5.71636116106699,5.81957642889864,5.92297408622041,5.99301869977126,
6.09643424801845,6.19969680809051,6.30283864671348,6.40591544332069,6.50896120312499,
6.61200988851889,6.71516579043367,6.81837821646031,6.92177360855688,6.99185514973314,
7.09672277111834,7.20139609880503,7.24304101724442),.UNSPECIFIED.);
#815=B_SPLINE_CURVE_WITH_KNOTS('',3,(#78053,#78054,#78055,#78056,#78057,
#78058,#78059,#78060,#78061,#78062,#78063,#78064,#78065,#78066,#78067,#78068,
#78069,#78070,#78071,#78072,#78073,#78074,#78075,#78076,#78077,#78078),
 .UNSPECIFIED.,.F.,.F.,(4,2,2,2,2,2,2,2,2,2,2,2,4),(-0.0747573429482938,
-0.0739377920332611,-0.0616381071463188,-0.0559582138108234,-0.0377856129565647,
-0.0350634467537814,-0.0337175298967136,-0.0326484433152754,-0.0316335720184391,
-0.0303960812896949,-0.0285521141284222,-0.0215327022529327,-0.000655553105070654),
 .UNSPECIFIED.);
#816=B_SPLINE_CURVE_WITH_KNOTS('',3,(#78080,#78081,#78082,#78083,#78084,
#78085,#78086,#78087,#78088,#78089,#78090,#78091,#78092,#78093,#78094,#78095,
#78096,#78097,#78098,#78099,#78100,#78101,#78102,#78103,#78104,#78105,#78106,
#78107,#78108,#78109,#78110,#78111,#78112,#78113,#78114,#78115,#78116,#78117,
#78118,#78119,#78120,#78121,#78122,#78123,#78124,#78125,#78126,#78127,#78128,
#78129,#78130,#78131,#78132,#78133,#78134,#78135,#78136,#78137,#78138,#78139,
#78140,#78141,#78142,#78143,#78144,#78145,#78146,#78147,#78148,#78149,#78150,
#78151,#78152,#78153,#78154,#78155,#78156,#78157,#78158,#78159,#78160,#78161,
#78162,#78163,#78164,#78165,#78166,#78167,#78168,#78169,#78170,#78171,#78172,
#78173,#78174,#78175,#78176,#78177,#78178,#78179,#78180,#78181,#78182,#78183,
#78184,#78185,#78186,#78187,#78188,#78189,#78190,#78191,#78192,#78193,#78194,
#78195,#78196,#78197),.UNSPECIFIED.,.F.,.F.,(4,3,3,3,3,3,3,3,3,3,3,3,3,
3,3,3,3,3,3,3,3,3,3,3,3,3,3,3,3,3,3,3,3,3,3,3,3,3,3,4),(170.955339710339,
171.060905920727,171.162663398586,171.264353088208,171.366010720948,171.467671979619,
171.569433774451,171.671256095252,171.773239609138,171.799869393442,171.903390335715,
172.006760275705,172.110011879462,172.21319984129,172.31635798341,172.419520086533,
172.522790163139,172.626117359596,172.72962716495,172.798705843404,172.901009778732,
173.003159662647,173.105192143119,173.207161917372,173.309104350476,173.411054767032,
173.513127529371,173.615263287867,173.717604736276,173.797542293366,173.903815556868,
174.015385955175,174.121305891971,174.227126233922,174.332874722438,174.438579009226,
174.544296437251,174.650018953138,174.755814439837,174.796378743328),
 .UNSPECIFIED.);
#817=B_SPLINE_CURVE_WITH_KNOTS('',3,(#78201,#78202,#78203,#78204,#78205,
#78206,#78207,#78208,#78209,#78210,#78211,#78212,#78213,#78214,#78215,#78216,
#78217,#78218,#78219,#78220,#78221,#78222,#78223,#78224,#78225,#78226,#78227,
#78228,#78229,#78230,#78231,#78232,#78233,#78234,#78235,#78236,#78237,#78238,
#78239,#78240,#78241,#78242,#78243,#78244,#78245,#78246,#78247,#78248,#78249,
#78250,#78251,#78252,#78253,#78254,#78255,#78256,#78257,#78258,#78259,#78260,
#78261,#78262,#78263,#78264,#78265,#78266,#78267,#78268,#78269,#78270,#78271,
#78272,#78273,#78274,#78275,#78276,#78277,#78278,#78279,#78280,#78281,#78282,
#78283,#78284,#78285,#78286,#78287,#78288,#78289,#78290,#78291,#78292,#78293,
#78294,#78295,#78296,#78297,#78298,#78299,#78300,#78301,#78302,#78303,#78304,
#78305,#78306,#78307,#78308,#78309,#78310,#78311,#78312,#78313,#78314,#78315,
#78316,#78317,#78318,#78319,#78320,#78321,#78322,#78323,#78324,#78325,#78326,
#78327,#78328,#78329,#78330,#78331,#78332,#78333,#78334,#78335,#78336,#78337,
#78338,#78339,#78340,#78341,#78342,#78343,#78344,#78345,#78346,#78347,#78348,
#78349,#78350,#78351,#78352,#78353,#78354,#78355,#78356,#78357,#78358,#78359,
#78360,#78361,#78362,#78363,#78364,#78365,#78366,#78367,#78368,#78369),
 .UNSPECIFIED.,.F.,.F.,(4,3,3,3,3,3,3,3,3,3,3,3,3,3,3,3,3,3,3,3,3,3,3,3,
3,3,3,3,3,3,3,3,3,3,3,3,3,3,3,3,3,3,3,3,3,3,3,3,3,3,3,3,3,3,3,3,4),(-172.787594226732,
-172.684274540723,-172.581108262565,-172.478063397069,-172.375083732247,
-172.272135122901,-172.169183466856,-172.06612700955,-171.963013555969,
-171.859723840347,-171.799869393442,-171.69629638248,-171.592873064501,
-171.489566337677,-171.386322201422,-171.28310690051,-171.179886720216,
-171.076557506667,-170.973170489168,-170.869600379445,-170.801032943481,
-170.697770749322,-170.594663919649,-170.491680617572,-170.388764006554,
-170.285879852593,-170.18299396611,-170.080001586328,-169.976953344622,
-169.873721384615,-169.802196493519,-169.69877510374,-169.595507068251,
-169.492360331767,-169.389278995906,-169.286229063151,-169.183176579175,
-169.080017486348,-168.976802204708,-168.873404533735,-168.803360043557,
-168.699944492016,-168.596681928558,-168.493540086429,-168.390463286242,
-168.28741752279,-168.184368833685,-168.081212927987,-167.978000498131,
-167.874605102172,-167.804523593595,-167.699671782949,-167.594987984343,
-167.490464933024,-167.386036710057,-167.281667200642,-167.203857020092),
 .UNSPECIFIED.);
#818=B_SPLINE_CURVE_WITH_KNOTS('',3,(#78370,#78371,#78372,#78373,#78374,
#78375,#78376,#78377),.UNSPECIFIED.,.F.,.F.,(4,2,2,4),(-2.66731441856907,
-2.64527597576796,-2.59640945473285,-2.59312200712756),.UNSPECIFIED.);
#819=B_SPLINE_CURVE_WITH_KNOTS('',3,(#78382,#78383,#78384,#78385,#78386,
#78387,#78388,#78389,#78390,#78391,#78392,#78393,#78394,#78395,#78396,#78397,
#78398,#78399,#78400,#78401,#78402,#78403,#78404,#78405,#78406,#78407,#78408,
#78409,#78410,#78411,#78412,#78413,#78414,#78415,#78416,#78417,#78418,#78419,
#78420,#78421,#78422,#78423,#78424,#78425,#78426,#78427,#78428,#78429,#78430,
#78431,#78432,#78433,#78434,#78435,#78436,#78437,#78438,#78439,#78440,#78441,
#78442,#78443,#78444,#78445,#78446,#78447,#78448,#78449,#78450,#78451,#78452,
#78453,#78454,#78455,#78456,#78457,#78458,#78459,#78460,#78461,#78462,#78463,
#78464,#78465,#78466,#78467,#78468,#78469,#78470,#78471,#78472,#78473,#78474,
#78475,#78476,#78477,#78478,#78479,#78480,#78481,#78482,#78483,#78484,#78485,
#78486,#78487,#78488,#78489,#78490,#78491,#78492,#78493,#78494,#78495,#78496,
#78497,#78498,#78499,#78500,#78501,#78502,#78503,#78504,#78505,#78506,#78507,
#78508,#78509,#78510,#78511,#78512,#78513,#78514,#78515,#78516,#78517,#78518,
#78519,#78520,#78521,#78522,#78523,#78524,#78525,#78526,#78527,#78528,#78529,
#78530,#78531,#78532,#78533,#78534,#78535,#78536,#78537,#78538,#78539,#78540,
#78541,#78542,#78543,#78544,#78545,#78546,#78547,#78548,#78549,#78550,#78551,
#78552,#78553,#78554,#78555,#78556,#78557,#78558,#78559,#78560,#78561,#78562,
#78563,#78564,#78565,#78566,#78567,#78568,#78569,#78570,#78571,#78572,#78573,
#78574,#78575,#78576,#78577,#78578,#78579,#78580,#78581,#78582,#78583,#78584,
#78585,#78586,#78587,#78588,#78589,#78590,#78591,#78592,#78593,#78594,#78595,
#78596,#78597,#78598,#78599,#78600,#78601,#78602,#78603,#78604,#78605,#78606,
#78607),.UNSPECIFIED.,.F.,.F.,(4,2,2,2,2,2,2,2,2,2,2,2,2,2,2,2,2,2,2,2,
2,2,2,2,2,2,2,2,2,2,2,2,2,2,2,2,2,2,2,2,2,2,2,2,2,2,2,2,2,2,2,2,2,2,2,2,
2,2,2,2,2,2,2,2,2,2,2,2,2,2,2,2,2,2,2,2,2,2,2,2,2,2,2,2,2,2,2,2,2,2,2,2,
2,2,2,2,2,2,2,2,2,2,2,2,2,2,2,2,2,2,2,2,4),(-1.40817978975408,-1.40705404757926,
-1.40292854426818,-1.37574263641332,-1.33373204839412,-1.32763515288138,
-1.30978755251285,-1.3070991662496,-1.30573723699631,-1.30466495537313,
-1.30341928575946,-1.30119586221527,-1.29070305463655,-1.2678405586377,
-1.21011174383134,-1.20367847380292,-1.20117011249373,-1.19935225441946,
-1.1974089632733,-1.19480675666405,-1.18898303420208,-1.16514969212771,
-1.11614974786207,-1.09779133728369,-1.09505199613252,-1.09369780661655,
-1.09262570590498,-1.09137328937515,-1.08912119207965,-1.0781767065768,
-1.05366061664344,-0.998557329887152,-0.991850144205298,-0.989297530946018,
-0.987467664534772,-0.985529988805104,-0.982966731454034,-0.977358991914342,
-0.929074949970343,-0.888723643118344,-0.884011288715337,-0.882271315198972,
-0.881246030966405,-0.880154595229384,-0.878645300073168,-0.875062776341669,
-0.870037648176115,-0.856213770806916,-0.833863019819696,-0.787184849699778,
-0.779989349485372,-0.777074348187559,-0.775273831938472,-0.773322007349834,
-0.770660366843926,-0.764492303368742,-0.737949711517808,-0.698620807892402,
-0.687287567855293,-0.673503613153939,-0.671211219321855,-0.669826486150342,
-0.668750035540309,-0.667534904461336,-0.665449567461102,-0.656908029632808,
-0.640347504304022,-0.59827806430656,-0.5710994647725,-0.566971944369264,
-0.564479121525566,-0.56254537992993,-0.560449714544518,-0.557102195271231,
-0.545904429027561,-0.527329152626984,-0.48480646601045,-0.462028585515264,
-0.459170679768378,-0.457792016141116,-0.456715751535966,-0.455474777491361,
-0.453287201529222,-0.443435529530059,-0.394233009637958,-0.359839125135791,
-0.355551417093985,-0.353009420771898,-0.351065048478533,-0.348984761265523,
-0.345718734049554,-0.335297061988363,-0.318505477259715,-0.25888309088138,
-0.249294095406842,-0.247244764404746,-0.245918148672959,-0.244851109626237,
-0.243841387935879,-0.241868990979533,-0.234450971840351,-0.220917549058247,
-0.192337554262401,-0.147271547762224,-0.143024722909869,-0.140506650841021,
-0.13858064226403,-0.136520200019756,-0.133286033524251,-0.122977060350292,
-0.106384465120274,-0.0845184420639834,-0.0747573429482938),
 .UNSPECIFIED.);
#820=B_SPLINE_CURVE_WITH_KNOTS('',3,(#78608,#78609,#78610,#78611,#78612,
#78613,#78614,#78615,#78616,#78617,#78618,#78619,#78620,#78621,#78622,#78623,
#78624,#78625,#78626,#78627,#78628,#78629,#78630,#78631,#78632,#78633,#78634,
#78635,#78636,#78637,#78638,#78639,#78640,#78641,#78642,#78643,#78644,#78645,
#78646,#78647,#78648,#78649,#78650,#78651,#78652,#78653,#78654,#78655,#78656,
#78657,#78658,#78659,#78660,#78661,#78662,#78663,#78664,#78665,#78666,#78667,
#78668,#78669,#78670,#78671,#78672,#78673,#78674,#78675,#78676,#78677,#78678,
#78679,#78680,#78681,#78682,#78683,#78684,#78685,#78686,#78687,#78688,#78689,
#78690,#78691,#78692,#78693,#78694,#78695,#78696,#78697,#78698,#78699,#78700,
#78701,#78702,#78703,#78704,#78705,#78706,#78707,#78708,#78709,#78710,#78711,
#78712,#78713,#78714,#78715,#78716,#78717,#78718,#78719,#78720,#78721,#78722,
#78723,#78724,#78725,#78726,#78727,#78728,#78729,#78730,#78731,#78732,#78733,
#78734,#78735,#78736,#78737,#78738,#78739,#78740,#78741,#78742,#78743,#78744,
#78745,#78746,#78747,#78748,#78749,#78750,#78751,#78752,#78753,#78754,#78755,
#78756,#78757,#78758,#78759,#78760,#78761,#78762,#78763,#78764,#78765,#78766,
#78767,#78768,#78769,#78770,#78771,#78772,#78773,#78774,#78775,#78776,#78777,
#78778,#78779,#78780,#78781,#78782,#78783,#78784,#78785,#78786,#78787,#78788,
#78789,#78790,#78791,#78792,#78793,#78794,#78795,#78796,#78797,#78798,#78799,
#78800,#78801,#78802,#78803,#78804,#78805,#78806,#78807,#78808,#78809,#78810,
#78811,#78812,#78813,#78814,#78815,#78816,#78817,#78818,#78819,#78820,#78821,
#78822,#78823,#78824,#78825,#78826,#78827,#78828,#78829,#78830,#78831,#78832,
#78833,#78834,#78835,#78836,#78837,#78838,#78839,#78840,#78841),
 .UNSPECIFIED.,.F.,.F.,(4,2,2,2,2,2,2,2,2,2,2,2,2,2,2,2,2,2,2,2,2,2,2,2,
2,2,2,2,2,2,2,2,2,2,2,2,2,2,2,2,2,2,2,2,2,2,2,2,2,2,2,2,2,2,2,2,2,2,2,2,
2,2,2,2,2,2,2,2,2,2,2,2,2,2,2,2,2,2,2,2,2,2,2,2,2,2,2,2,2,2,2,2,2,2,2,2,
2,2,2,2,2,2,2,2,2,2,2,2,2,2,2,2,2,2,2,2,4),(-2.59312200712756,-2.58668664222653,
-2.58451546766303,-2.58328207928504,-2.58220871169981,-2.58083073879879,
-2.57797110541151,-2.54189129239521,-2.50916640239598,-2.49279452047219,
-2.48600086106938,-2.48237496634032,-2.47927467296956,-2.47726818405217,
-2.47532693467477,-2.47278524300085,-2.46848983762896,-2.43346398051266,
-2.38445171182475,-2.37475716805989,-2.37258545116,-2.37135064051444,-2.3702764347687,
-2.36889710847375,-2.36667496243012,-2.35430821956314,-2.30479958419138,
-2.27590736793385,-2.26945213717435,-2.26673989329341,-2.26477762736604,
-2.26298586221718,-2.26012525570338,-2.2532666535172,-2.19985319559646,
-2.17417358948347,-2.16292484364099,-2.16065595593984,-2.15940043029352,
-2.15832922288703,-2.15698085418778,-2.15435556021802,-2.13819906501921,
-2.09170618377056,-2.06374275210145,-2.05739900543972,-2.05470588691118,
-2.05274730735861,-2.05095189213046,-2.04807012337105,-2.04108147920287,
-1.98950767075604,-1.96254154867394,-1.95096912120203,-1.94868193553589,
-1.94742248507266,-1.94635153844779,-1.94500812553222,-1.94240635973622,
-1.92681824445236,-1.92033667215102,-1.90643681031755,-1.87355463531687,
-1.85699769932198,-1.84668979822785,-1.84344136769288,-1.84136805127564,
-1.83942725599496,-1.83688575556629,-1.8325898016913,-1.79739244058602,
-1.74815277494505,-1.73876782088624,-1.73661853308056,-1.73538902213904,
-1.73431434234439,-1.73292790728223,-1.73002499827752,-1.69795902725883,
-1.66507249079384,-1.64624588722739,-1.63876175178362,-1.63313965414123,
-1.63057416151338,-1.62863657680158,-1.62680811852904,-1.62425960748694,
-1.61757631709381,-1.56218589452321,-1.53784546862036,-1.52694726338165,
-1.52469875308918,-1.52344751702551,-1.52237564722492,-1.52102091575383,
-1.51836687517718,-1.5014851364578,-1.48269888091522,-1.44973485971465,
-1.4330826113428,-1.42273146978707,-1.41947796277252,-1.41740345786126,
-1.41546299044009,-1.41292399686323,-1.40863693737991,-1.3648787607464,
-1.33382957462007,-1.31578004819068,-1.3130844819512,-1.31172086469994,
-1.31064826301276,-1.30940337573073,-1.30718411226304,-1.29676115595744,
-1.27414831556036,-1.2596648285931),.UNSPECIFIED.);
#821=B_SPLINE_CURVE_WITH_KNOTS('',3,(#78847,#78848,#78849,#78850),
 .UNSPECIFIED.,.F.,.F.,(4,4),(158.039785789814,158.388969095546),
 .UNSPECIFIED.);
#822=B_SPLINE_CURVE_WITH_KNOTS('',3,(#78851,#78852,#78853,#78854,#78855,
#78856,#78857,#78858,#78859,#78860,#78861,#78862,#78863,#78864,#78865,#78866,
#78867,#78868,#78869,#78870,#78871,#78872,#78873,#78874,#78875,#78876,#78877,
#78878,#78879,#78880,#78881,#78882,#78883,#78884,#78885,#78886,#78887,#78888,
#78889,#78890,#78891,#78892,#78893,#78894,#78895,#78896,#78897,#78898,#78899,
#78900,#78901,#78902,#78903,#78904,#78905,#78906,#78907,#78908,#78909,#78910,
#78911,#78912,#78913,#78914,#78915,#78916,#78917,#78918,#78919,#78920,#78921,
#78922,#78923,#78924,#78925,#78926,#78927,#78928,#78929,#78930,#78931,#78932,
#78933,#78934,#78935,#78936,#78937,#78938,#78939,#78940,#78941,#78942,#78943,
#78944,#78945,#78946,#78947,#78948,#78949,#78950,#78951,#78952,#78953,#78954,
#78955,#78956,#78957,#78958,#78959,#78960,#78961,#78962,#78963,#78964,#78965,
#78966,#78967,#78968,#78969,#78970,#78971,#78972,#78973,#78974,#78975,#78976,
#78977,#78978,#78979,#78980,#78981,#78982,#78983,#78984,#78985,#78986,#78987,
#78988,#78989,#78990,#78991,#78992,#78993,#78994,#78995,#78996,#78997,#78998,
#78999,#79000,#79001,#79002,#79003,#79004,#79005,#79006,#79007,#79008,#79009,
#79010,#79011,#79012,#79013,#79014,#79015,#79016,#79017,#79018,#79019,#79020,
#79021,#79022,#79023,#79024,#79025,#79026,#79027,#79028,#79029,#79030,#79031,
#79032,#79033,#79034,#79035,#79036,#79037,#79038,#79039,#79040,#79041,#79042,
#79043,#79044,#79045,#79046,#79047,#79048,#79049,#79050,#79051,#79052,#79053,
#79054,#79055,#79056,#79057,#79058,#79059,#79060),.UNSPECIFIED.,.F.,.F.,
(4,2,2,2,2,2,2,2,2,2,2,2,2,2,2,2,2,2,2,2,2,2,2,2,2,2,2,2,2,2,2,2,2,2,2,
2,2,2,2,2,2,2,2,2,2,2,2,2,2,2,2,2,2,2,2,2,2,2,2,2,2,2,2,2,2,2,2,2,2,2,2,
2,2,2,2,2,2,2,2,2,2,2,2,2,2,2,2,2,2,2,2,2,2,2,2,2,2,2,2,2,2,2,2,2,4),(-2.66742162310756,
-2.60891625458958,-2.59007756301913,-2.5807843811516,-2.57864188477314,
-2.57741397132789,-2.57633914807995,-2.57495053489239,-2.57203616322235,
-2.54225915154028,-2.491618626458,-2.48229125892587,-2.47774074752514,-2.47500310992017,
-2.47251926151665,-2.47064325906592,-2.46881669433059,-2.46627492665722,
-2.45963404079168,-2.40385030414874,-2.37977515805284,-2.36894861844136,
-2.36670455611624,-2.36545434690764,-2.36438245579056,-2.36302654277748,
-2.36088129925783,-2.34984855699457,-2.29862620291396,-2.26992235611622,
-2.26348941602719,-2.2607809307943,-2.2588193513631,-2.25702681510704,-2.25416194012492,
-2.24727736198246,-2.19421525541888,-2.16830149607979,-2.1569928499235,
-2.15472036560436,-2.15346398626832,-2.1523927153326,-2.15104511224504,
-2.1484238498383,-2.13238520146658,-2.12706656171519,-2.11250730991782,
-2.07961705504466,-2.06305104502602,-2.0527391816087,-2.04949041180652,
-2.04741710040982,-2.04547646653824,-2.04293540513378,-2.038640709969,-2.00353412150858,
-1.95464821348685,-1.94485967236405,-1.94268231602897,-1.94144669416129,
-1.9403730099634,-1.93899619029812,-1.93614239862554,-1.91343183992003,
-1.87271682037077,-1.84567960098941,-1.83944818222358,-1.83677393968413,
-1.83481836125248,-1.83301821422818,-1.83011230107754,-1.82298125839401,
-1.77424539366048,-1.73505279865914,-1.73147806163526,-1.72996903731451,
-1.7288768707321,-1.72785088802919,-1.72610769100588,-1.72137472109072,
-1.68178295833899,-1.63388986388747,-1.62749309178188,-1.62479052149567,
-1.62282983083475,-1.62103576597798,-1.61816334339362,-1.61123417222076,
-1.55875570359449,-1.53242879584004,-1.52101504596968,-1.51873640844595,
-1.51747862424396,-1.51640745109487,-1.51506158968022,-1.51244824903978,
-1.49656849145573,-1.49069768702886,-1.44666703851389,-1.4281081634151,
-1.41691845775053,-1.41357286304999,-1.4114783364764,-1.40954560852309,
-1.40817978975408),.UNSPECIFIED.);
#823=B_SPLINE_CURVE_WITH_KNOTS('',3,(#79062,#79063,#79064,#79065,#79066,
#79067,#79068,#79069,#79070,#79071,#79072,#79073,#79074,#79075,#79076,#79077,
#79078,#79079,#79080,#79081,#79082,#79083,#79084,#79085,#79086,#79087,#79088,
#79089,#79090,#79091,#79092,#79093,#79094,#79095,#79096,#79097,#79098,#79099,
#79100,#79101,#79102,#79103,#79104,#79105,#79106,#79107,#79108,#79109,#79110,
#79111,#79112,#79113,#79114,#79115,#79116,#79117,#79118,#79119,#79120,#79121,
#79122,#79123,#79124,#79125,#79126,#79127,#79128,#79129,#79130,#79131,#79132,
#79133,#79134,#79135,#79136,#79137,#79138,#79139,#79140,#79141,#79142,#79143,
#79144,#79145,#79146,#79147,#79148,#79149,#79150,#79151,#79152,#79153,#79154,
#79155,#79156,#79157,#79158,#79159,#79160,#79161,#79162,#79163,#79164,#79165,
#79166,#79167,#79168,#79169,#79170,#79171,#79172,#79173,#79174,#79175,#79176,
#79177,#79178,#79179,#79180,#79181,#79182,#79183,#79184,#79185,#79186,#79187,
#79188,#79189,#79190,#79191,#79192,#79193,#79194,#79195,#79196,#79197,#79198,
#79199,#79200,#79201,#79202,#79203,#79204,#79205,#79206,#79207,#79208,#79209,
#79210,#79211,#79212,#79213,#79214,#79215,#79216,#79217,#79218,#79219,#79220,
#79221,#79222,#79223,#79224,#79225,#79226,#79227,#79228,#79229,#79230,#79231,
#79232,#79233,#79234,#79235,#79236,#79237,#79238,#79239,#79240,#79241,#79242,
#79243,#79244,#79245,#79246,#79247,#79248,#79249,#79250,#79251,#79252,#79253,
#79254,#79255,#79256,#79257,#79258,#79259,#79260,#79261,#79262,#79263,#79264,
#79265,#79266,#79267,#79268,#79269,#79270,#79271,#79272,#79273,#79274,#79275,
#79276,#79277,#79278,#79279,#79280,#79281),.UNSPECIFIED.,.F.,.F.,(4,2,2,
2,2,2,2,2,2,2,2,2,2,2,2,2,2,2,2,2,2,2,2,2,2,2,2,2,2,2,2,2,2,2,2,2,2,2,2,
2,2,2,2,2,2,2,2,2,2,2,2,2,2,2,2,2,2,2,2,2,2,2,2,2,2,2,2,2,2,2,2,2,2,2,2,
2,2,2,2,2,2,2,2,2,2,2,2,2,2,2,2,2,2,2,2,2,2,2,2,2,2,2,2,2,2,2,2,2,2,4),
(-1.2596648285931,-1.2160256105695,-1.2096421076692,-1.20714190826177,-1.20532609232373,
-1.20338135515468,-1.20077090690376,-1.19490199470179,-1.17072606542606,
-1.12024397579635,-1.11981226220589,-1.10362682585641,-1.1009999536592,
-1.09965104438236,-1.09857957574208,-1.09732394998322,-1.09505525728509,
-1.08381545338579,-1.05816969650078,-1.00467000549561,-0.997816063283325,
-0.994956078215463,-0.993164321344302,-0.991201763735631,-0.9884885554406,
-0.982028345407357,-0.928096146003009,-0.891885568568339,-0.889031116345708,
-0.887654133636997,-0.886580391096139,-0.885344786076734,-0.883167649594423,
-0.873383593198826,-0.824465702367648,-0.789344862391968,-0.785049718549043,
-0.782508524928635,-0.78056785562871,-0.778494568855833,-0.775245966469818,
-0.764935628182494,-0.748375296264231,-0.715517712106479,-0.701773749074622,
-0.694932998493534,-0.69464545217534,-0.689556244560843,-0.679089800365006,
-0.676980766915887,-0.675635951791255,-0.6745648624677,-0.673306342658668,
-0.671023941274004,-0.659541239303526,-0.632935074326423,-0.58081796313325,
-0.573862309108464,-0.570985764847464,-0.569191131977569,-0.567231433180628,
-0.564533168175351,-0.558160381320284,-0.529962513252371,-0.48202816084319,
-0.479449715698858,-0.467293909964139,-0.465083541170018,-0.463707902381071,
-0.462634409181775,-0.461398188828441,-0.459217800486224,-0.44938304164365,
-0.400515271221216,-0.365413816321955,-0.361119437563833,-0.358578636710422,
-0.356638232829069,-0.354565196109159,-0.351316915525819,-0.341007007627579,
-0.324446804163342,-0.269351910025381,-0.255460701928919,-0.253161866437407,
-0.251774646689025,-0.250697368696635,-0.249482829523745,-0.247442360045852,
-0.239362587541947,-0.224064932594649,-0.19411672439862,-0.189603855941387,
-0.15347084623078,-0.148747386689599,-0.146324297302805,-0.144405427518325,
-0.142252821210166,-0.138645212087007,-0.124695234879609,-0.0975109104562382,
-0.0749657652856314,-0.0441240231168734,-0.041211786302814,-0.0398236671605482,
-0.0387489818054857,-0.0375209615861949,-0.0362288381666934,-0.0342509000805209,
-0.000628703125059541),.UNSPECIFIED.);
#824=B_SPLINE_CURVE_WITH_KNOTS('',3,(#79282,#79283,#79284,#79285,#79286,
#79287,#79288,#79289,#79290,#79291,#79292,#79293,#79294,#79295,#79296,#79297,
#79298,#79299),.UNSPECIFIED.,.F.,.F.,(4,2,2,2,2,2,2,2,4),(-2.66818930628053,
-2.63771571888677,-2.61120086164018,-2.60503375764702,-2.60237044757543,
-2.60041659460138,-2.59861363688443,-2.59569337617825,-2.59370492657453),
 .UNSPECIFIED.);
#825=B_SPLINE_CURVE_WITH_KNOTS('',3,(#79305,#79306,#79307,#79308,#79309,
#79310,#79311,#79312,#79313,#79314,#79315,#79316,#79317),.UNSPECIFIED.,
 .F.,.F.,(4,3,3,3,4),(151.755345396751,151.823140394205,151.951948597258,
152.078650414045,152.105783788367),.UNSPECIFIED.);
#826=B_SPLINE_CURVE_WITH_KNOTS('',3,(#79318,#79319,#79320,#79321,#79322,
#79323,#79324,#79325,#79326,#79327),.UNSPECIFIED.,.F.,.F.,(4,1,1,1,1,1,
1,4),(152.105783788367,152.821976844167,153.820813294129,154.819649744091,
155.818486194052,156.817322644014,157.816159093976,158.039785789814),
 .UNSPECIFIED.);
#827=B_SPLINE_CURVE_WITH_KNOTS('',3,(#79328,#79329,#79330,#79331,#79332,
#79333,#79334,#79335,#79336,#79337,#79338,#79339,#79340,#79341,#79342,#79343,
#79344,#79345,#79346,#79347,#79348,#79349,#79350,#79351,#79352,#79353,#79354,
#79355,#79356,#79357,#79358,#79359,#79360,#79361,#79362,#79363,#79364,#79365,
#79366,#79367,#79368,#79369,#79370,#79371,#79372,#79373,#79374,#79375,#79376,
#79377,#79378,#79379,#79380,#79381,#79382,#79383,#79384,#79385,#79386,#79387,
#79388,#79389,#79390,#79391,#79392,#79393,#79394,#79395,#79396,#79397,#79398,
#79399,#79400,#79401,#79402,#79403,#79404,#79405,#79406,#79407,#79408,#79409,
#79410,#79411,#79412,#79413,#79414,#79415,#79416,#79417,#79418,#79419,#79420,
#79421,#79422,#79423,#79424,#79425,#79426,#79427,#79428,#79429,#79430,#79431,
#79432,#79433,#79434,#79435,#79436,#79437,#79438,#79439,#79440,#79441,#79442,
#79443,#79444,#79445,#79446,#79447,#79448,#79449,#79450,#79451,#79452,#79453,
#79454,#79455,#79456,#79457,#79458,#79459,#79460,#79461,#79462,#79463,#79464,
#79465,#79466,#79467,#79468,#79469,#79470,#79471,#79472,#79473,#79474,#79475,
#79476,#79477,#79478,#79479,#79480,#79481,#79482,#79483,#79484,#79485,#79486,
#79487,#79488,#79489,#79490,#79491,#79492,#79493,#79494,#79495,#79496,#79497,
#79498,#79499,#79500,#79501,#79502,#79503,#79504,#79505,#79506,#79507,#79508,
#79509,#79510,#79511,#79512,#79513,#79514,#79515,#79516,#79517,#79518,#79519,
#79520,#79521,#79522,#79523,#79524,#79525,#79526,#79527,#79528,#79529,#79530,
#79531,#79532,#79533,#79534,#79535,#79536,#79537,#79538,#79539,#79540,#79541,
#79542,#79543,#79544,#79545,#79546,#79547,#79548,#79549,#79550,#79551,#79552,
#79553,#79554,#79555),.UNSPECIFIED.,.F.,.F.,(4,2,2,2,2,2,2,2,2,2,2,2,2,
2,2,2,2,2,2,2,2,2,2,2,2,2,2,2,2,2,2,2,2,2,2,2,2,2,2,2,2,2,2,2,2,2,2,2,2,
2,2,2,2,2,2,2,2,2,2,2,2,2,2,2,2,2,2,2,2,2,2,2,2,2,2,2,2,2,2,2,2,2,2,2,2,
2,2,2,2,2,2,2,2,2,2,2,2,2,2,2,2,2,2,2,2,2,2,2,2,2,2,2,2,4),(-2.59370492657453,
-2.58847820404563,-2.54309870392059,-2.52300656285645,-2.50674703366011,
-2.49833489705349,-2.49628759775399,-2.49505880127077,-2.49398388929921,
-2.4925960638836,-2.49034578019742,-2.47744469912304,-2.47491956480728,
-2.4706232200629,-2.43000257545183,-2.39666005130046,-2.39214965110867,
-2.38980199149159,-2.38788898195058,-2.38568383373875,-2.38193830658902,
-2.36780631242021,-2.35546526585911,-2.30760509909679,-2.29374245395045,
-2.28870603116317,-2.28511616897621,-2.28360448725736,-2.28251180258687,
-2.28148650553305,-2.27974684899653,-2.27503731979819,-2.23463373138629,
-2.18635069491183,-2.18074307863355,-2.17818014888768,-2.17624284221069,
-2.17441342314041,-2.17186160147031,-2.16515753442451,-2.10997738320941,
-2.0854945172373,-2.07455798185226,-2.07230703406436,-2.07105520034447,
-2.06998328344636,-2.06862908631448,-2.06588979216297,-2.04753865035993,
-2.02964535200168,-1.99690771674675,-1.97439756890853,-1.96875029208805,
-1.96617991876962,-1.96424134195001,-1.96241392924407,-1.95987006037063,
-1.95321817931557,-1.89749282082125,-1.87336596542637,-1.86252439907145,
-1.86027902910937,-1.85902834440211,-1.85795620888598,-1.85660019358752,
-1.85445516523925,-1.84343155678569,-1.79212673046656,-1.76346276898746,
-1.7570338390636,-1.7543256372076,-1.75236375319437,-1.75057058794909,-1.74770394510717,
-1.74081116961503,-1.6878179276519,-1.66184074592123,-1.65051477013927,
-1.64824088959472,-1.64698401865768,-1.64591248581013,-1.64456475820447,
-1.64194388845335,-1.62591893105205,-1.62051388797226,-1.60601441996286,
-1.57311672598438,-1.55035885106369,-1.54467792700712,-1.54210127023863,
-1.54016161730759,-1.53833587683694,-1.53579864049959,-1.52918957349922,
-1.4730365142259,-1.4491858646681,-1.43841869818796,-1.43617773964232,-1.43492796416028,
-1.43385565241863,-1.4324981872711,-1.42983227179874,-1.41264461335246,
-1.36256425545815,-1.34500772461246,-1.33425290066633,-1.33095365909261,
-1.3288688688674,-1.3269318557328,-1.32437252411668,-1.31878568366601,-1.31136189021472,
-1.29275920440411,-1.2599124547823),.UNSPECIFIED.);
#828=B_SPLINE_CURVE_WITH_KNOTS('',3,(#79561,#79562,#79563,#79564,#79565,
#79566,#79567,#79568,#79569,#79570,#79571,#79572,#79573,#79574),
 .UNSPECIFIED.,.F.,.F.,(4,2,2,2,2,2,4),(-0.0749176319822858,-0.0721945338621709,
-0.0417574974960581,-0.00539334313703774,-0.00193462587292075,-0.000864005353919265,
-0.000629064028114969),.UNSPECIFIED.);
#829=B_SPLINE_CURVE_WITH_KNOTS('',3,(#79575,#79576,#79577,#79578,#79579,
#79580,#79581,#79582,#79583,#79584,#79585,#79586,#79587,#79588,#79589,#79590,
#79591,#79592,#79593,#79594,#79595,#79596,#79597,#79598,#79599,#79600,#79601,
#79602,#79603,#79604,#79605,#79606,#79607,#79608,#79609,#79610,#79611,#79612,
#79613,#79614,#79615,#79616,#79617,#79618,#79619,#79620,#79621,#79622,#79623,
#79624,#79625,#79626,#79627,#79628,#79629,#79630,#79631,#79632,#79633,#79634,
#79635,#79636,#79637,#79638,#79639,#79640,#79641,#79642,#79643,#79644,#79645,
#79646,#79647,#79648,#79649,#79650,#79651,#79652,#79653,#79654,#79655,#79656,
#79657,#79658,#79659,#79660,#79661,#79662,#79663,#79664,#79665,#79666,#79667,
#79668,#79669,#79670,#79671,#79672,#79673,#79674,#79675,#79676,#79677,#79678,
#79679,#79680,#79681,#79682,#79683,#79684,#79685,#79686,#79687,#79688,#79689,
#79690,#79691,#79692,#79693,#79694,#79695,#79696,#79697,#79698,#79699,#79700,
#79701,#79702,#79703,#79704,#79705,#79706,#79707,#79708,#79709,#79710,#79711,
#79712,#79713,#79714,#79715,#79716,#79717,#79718,#79719,#79720,#79721,#79722,
#79723,#79724,#79725,#79726,#79727,#79728,#79729,#79730,#79731,#79732,#79733,
#79734,#79735,#79736,#79737,#79738,#79739,#79740,#79741,#79742,#79743,#79744,
#79745,#79746,#79747,#79748,#79749,#79750,#79751,#79752,#79753,#79754,#79755),
 .UNSPECIFIED.,.F.,.F.,(4,3,3,3,3,3,3,3,3,3,3,3,3,3,3,3,3,3,3,3,3,3,3,3,
3,3,3,3,3,3,3,3,3,3,3,3,3,3,3,3,3,3,3,3,3,3,3,3,3,3,3,3,3,3,3,3,3,3,3,3,
4),(145.822598481187,145.830121694434,145.93351643147,146.036757713572,
146.139877678953,146.24293224715,146.345955455495,146.448981298156,146.552114064923,
146.655303156321,146.758675149692,146.828958144396,146.932352881429,147.03559416353,
147.138714128907,147.241768697101,147.344791905443,147.4478177481,147.550950514863,
147.654139606258,147.757511599624,147.827794594357,147.931189331481,148.034430613671,
148.137550579139,148.240605147424,148.343628355857,148.446654198605,148.549786965457,
148.652976056941,148.756348050395,148.826631044319,148.930025781262,149.033267063273,
149.136387028562,149.239441596669,149.342464804925,149.445490647496,149.548623414176,
149.651812505488,149.755184498775,149.825467494281,149.928862231266,150.032103513317,
150.135223478643,150.238278046785,150.341301255075,150.444327097679,150.547459864388,
150.650648955728,150.754020949039,150.824303944243,150.927703487107,151.031158725813,
151.134277032367,151.237328082884,151.340345916045,151.444095786221,151.547200179175,
151.651272787963,151.755345396751),.UNSPECIFIED.);
#830=B_SPLINE_CURVE_WITH_KNOTS('',3,(#79757,#79758,#79759,#79760,#79761,
#79762,#79763,#79764,#79765,#79766,#79767,#79768,#79769,#79770,#79771,#79772,
#79773,#79774,#79775,#79776,#79777,#79778,#79779,#79780,#79781,#79782,#79783,
#79784,#79785,#79786,#79787,#79788,#79789,#79790,#79791,#79792,#79793,#79794,
#79795,#79796,#79797,#79798,#79799,#79800,#79801,#79802,#79803,#79804,#79805,
#79806,#79807,#79808,#79809,#79810,#79811,#79812,#79813,#79814,#79815,#79816,
#79817,#79818,#79819,#79820,#79821,#79822,#79823,#79824,#79825,#79826,#79827,
#79828,#79829,#79830,#79831,#79832,#79833,#79834,#79835,#79836,#79837,#79838,
#79839,#79840,#79841,#79842,#79843,#79844,#79845,#79846,#79847,#79848,#79849,
#79850,#79851,#79852,#79853,#79854,#79855,#79856,#79857,#79858,#79859,#79860,
#79861,#79862,#79863,#79864,#79865,#79866,#79867,#79868,#79869,#79870,#79871,
#79872,#79873,#79874,#79875,#79876,#79877,#79878,#79879,#79880,#79881,#79882,
#79883,#79884,#79885,#79886,#79887,#79888,#79889,#79890,#79891,#79892,#79893,
#79894,#79895,#79896,#79897,#79898,#79899,#79900,#79901,#79902,#79903,#79904,
#79905,#79906,#79907,#79908,#79909,#79910,#79911,#79912,#79913,#79914,#79915,
#79916,#79917,#79918,#79919,#79920,#79921,#79922,#79923,#79924,#79925,#79926,
#79927,#79928,#79929,#79930,#79931,#79932,#79933,#79934,#79935,#79936,#79937,
#79938,#79939,#79940,#79941,#79942,#79943,#79944,#79945,#79946,#79947,#79948,
#79949,#79950,#79951,#79952,#79953,#79954,#79955,#79956,#79957,#79958,#79959,
#79960,#79961,#79962,#79963,#79964,#79965,#79966,#79967,#79968,#79969,#79970,
#79971,#79972,#79973,#79974,#79975,#79976,#79977,#79978,#79979,#79980),
 .UNSPECIFIED.,.F.,.F.,(4,2,2,2,2,2,2,2,2,2,2,2,2,2,2,2,2,2,2,2,2,2,2,2,
2,2,2,2,2,2,2,2,2,2,2,2,2,2,2,2,2,2,2,2,2,2,2,2,2,2,2,2,2,2,2,2,2,2,2,2,
2,2,2,2,2,2,2,2,2,2,2,2,2,2,2,2,2,2,2,2,2,2,2,2,2,2,2,2,2,2,2,2,2,2,2,2,
2,2,2,2,2,2,2,2,2,2,2,2,2,2,2,4),(-1.2599124547823,-1.25002807386397,-1.22739935917188,
-1.2245470716002,-1.22317035629757,-1.22209645694531,-1.22086025870375,
-1.21868108665142,-1.20887143217979,-1.1599640872171,-1.12484333499143,
-1.12054745872809,-1.1180058036613,-1.1160647657301,-1.11399106937169,-1.11074179224174,
-1.10042903347153,-1.08386454585292,-1.05099987303016,-1.03717122403354,
-1.03052069631196,-1.0150465323747,-1.01244934016723,-1.01110677730609,
-1.01003563671185,-1.00877490927762,-1.00648299290409,-0.994835707568061,
-0.967567834981807,-0.947382712475257,-0.912873645829924,-0.90858677832834,
-0.906047759094729,-0.904107180475675,-0.902032466638724,-0.898778441893425,
-0.888423947808562,-0.871766974134913,-0.838826018849427,-0.820097685720636,
-0.803187199701922,-0.800532015826634,-0.799176987846143,-0.798105031739481,
-0.79685387076215,-0.794605920055246,-0.783719099969251,-0.759419292369503,
-0.703923646265877,-0.697247242300925,-0.694699721534836,-0.69287147513404,
-0.690933656972484,-0.688367071008456,-0.682739390828016,-0.675246546493855,
-0.656390119530333,-0.626116411631464,-0.603702869700675,-0.59088098658125,
-0.588635025015686,-0.587248588310373,-0.586173941024472,-0.584944548023931,
-0.582795509189763,-0.57341270182101,-0.524152073686013,-0.488926964416472,
-0.484630607594345,-0.482089109817155,-0.480148446279506,-0.478075396397384,
-0.47482764680899,-0.464524072357827,-0.447978458492938,-0.41710515898568,
-0.397464619463284,-0.37931813610327,-0.37661976383513,-0.375255693963338,
-0.374183237474751,-0.372939096883373,-0.370722545647898,-0.360688865171072,
-0.312016982578369,-0.2769834080816,-0.272689986555764,-0.270149477532661,
-0.268209138396986,-0.266136017507042,-0.262887284792429,-0.25276849119224,
-0.23654606782421,-0.198322585414324,-0.167652355293061,-0.164739955608835,
-0.16335184523917,-0.162277206557913,-0.161049284407586,-0.159757278089317,
-0.155110106861215,-0.128864893942761,-0.106990886563457,-0.105560230878355,
-0.0651104974991618,-0.0603738601647401,-0.0579480736937648,-0.0560290637456423,
-0.0538783940964652,-0.0516516915055142,-0.0483298719236029,-0.00062898557017253),
 .UNSPECIFIED.);
#831=B_SPLINE_CURVE_WITH_KNOTS('',3,(#79981,#79982,#79983,#79984,#79985,
#79986,#79987,#79988,#79989,#79990,#79991,#79992,#79993,#79994,#79995,#79996,
#79997,#79998,#79999,#80000),.UNSPECIFIED.,.F.,.F.,(4,2,2,2,2,2,2,2,2,4),
(-2.66773620090402,-2.62477875133751,-2.6218447624627,-2.62016197467351,
-2.61865699930487,-2.61756533538186,-2.61653793993882,-2.6147881679525,
-2.61001317239784,-2.59360340364756),.UNSPECIFIED.);
#832=B_SPLINE_CURVE_WITH_KNOTS('',3,(#80005,#80006,#80007,#80008,#80009,
#80010,#80011,#80012,#80013,#80014,#80015,#80016,#80017,#80018,#80019,#80020,
#80021,#80022,#80023,#80024,#80025,#80026,#80027,#80028,#80029,#80030,#80031,
#80032,#80033,#80034,#80035,#80036,#80037,#80038,#80039,#80040,#80041,#80042,
#80043,#80044,#80045,#80046,#80047,#80048,#80049,#80050,#80051,#80052,#80053,
#80054,#80055,#80056,#80057,#80058,#80059,#80060,#80061,#80062,#80063,#80064,
#80065,#80066,#80067,#80068,#80069,#80070,#80071,#80072,#80073,#80074,#80075,
#80076,#80077,#80078,#80079,#80080,#80081,#80082,#80083,#80084,#80085,#80086,
#80087,#80088,#80089,#80090,#80091,#80092,#80093,#80094,#80095,#80096,#80097,
#80098,#80099,#80100,#80101,#80102,#80103,#80104,#80105,#80106,#80107,#80108,
#80109,#80110,#80111,#80112,#80113,#80114,#80115,#80116,#80117,#80118,#80119,
#80120,#80121,#80122,#80123,#80124,#80125,#80126,#80127,#80128,#80129,#80130,
#80131,#80132,#80133,#80134,#80135,#80136,#80137,#80138,#80139,#80140,#80141,
#80142,#80143,#80144,#80145,#80146,#80147,#80148,#80149,#80150,#80151,#80152,
#80153,#80154,#80155,#80156,#80157,#80158,#80159,#80160,#80161,#80162,#80163,
#80164,#80165,#80166,#80167,#80168,#80169,#80170,#80171,#80172,#80173,#80174,
#80175,#80176,#80177,#80178,#80179,#80180,#80181,#80182,#80183,#80184,#80185,
#80186,#80187,#80188,#80189,#80190,#80191,#80192,#80193,#80194,#80195,#80196,
#80197,#80198,#80199,#80200,#80201,#80202,#80203,#80204,#80205,#80206,#80207,
#80208,#80209,#80210,#80211,#80212,#80213,#80214,#80215,#80216,#80217,#80218,
#80219,#80220,#80221,#80222,#80223,#80224,#80225,#80226,#80227,#80228,#80229,
#80230,#80231,#80232,#80233,#80234,#80235,#80236,#80237,#80238,#80239,#80240,
#80241,#80242,#80243,#80244,#80245,#80246,#80247,#80248,#80249,#80250,#80251,
#80252,#80253,#80254,#80255,#80256,#80257,#80258,#80259,#80260,#80261,#80262,
#80263,#80264,#80265,#80266,#80267,#80268,#80269,#80270,#80271,#80272,#80273,
#80274,#80275,#80276,#80277,#80278,#80279,#80280),.UNSPECIFIED.,.F.,.F.,
(4,2,2,2,2,2,2,2,2,2,2,2,2,2,2,2,2,2,2,2,2,2,2,2,2,2,2,2,2,2,2,2,2,2,2,
2,2,2,2,2,2,2,2,2,2,2,2,2,2,2,2,2,2,2,2,2,2,2,2,2,2,2,2,2,2,2,2,2,2,2,2,
2,2,2,2,2,2,2,2,2,2,2,2,2,2,2,2,2,2,2,2,2,2,2,2,2,2,2,2,2,2,2,2,2,2,2,2,
2,2,2,2,2,2,2,2,2,2,2,2,2,2,2,2,2,2,2,2,2,2,2,2,2,2,2,2,2,2,4),(-1.40850074877309,
-1.39306820108003,-1.3827203300755,-1.37946735532854,-1.37739307038897,
-1.37545272476306,-1.37291376930828,-1.36862650202268,-1.33404472929969,
-1.2780780617487,-1.27380416440126,-1.27213256037046,-1.27112051463128,
-1.27001816035819,-1.26845321514756,-1.26454062554833,-1.24532800378349,
-1.18895312087029,-1.17210784928932,-1.16849108707793,-1.16612695367344,
-1.16421312881994,-1.16202094134709,-1.15823458076248,-1.14198762558551,
-1.08451185183594,-1.07953977447776,-1.06355442055558,-1.06093604447996,
-1.05958897221224,-1.05851763000277,-1.05726060533859,-1.05498547659474,
-1.04363391000168,-1.01755068902743,-0.964680736697037,-0.957777654122178,
-0.954909579772716,-0.953116350836811,-0.951155071172475,-0.948448931051755,
-0.942030686282602,-0.91345622310966,-0.862261700840353,-0.851098435335316,
-0.848945111478426,-0.847586697714472,-0.846514564852924,-0.845266070101644,
-0.843030061950331,-0.83233735008917,-0.808752957034694,-0.75217190320003,
-0.74560833398379,-0.743078737091019,-0.741255317044758,-0.739315192052921,
-0.736732877379483,-0.731018769371518,-0.708011392560211,-0.67498765768642,
-0.653828795219877,-0.639433447422016,-0.637109964437036,-0.635715473518186,
-0.634637223207563,-0.633426814054773,-0.631363245007312,-0.623093503649382,
-0.607315068087108,-0.565213967485415,-0.537106673358644,-0.532956862476877,
-0.530458132935264,-0.528524275512585,-0.526432936315915,-0.523101960962362,
-0.512049399581106,-0.493811250405697,-0.444967537422689,-0.427675161974073,
-0.425006237327776,-0.42364841644425,-0.422576429706423,-0.42132773562145,
-0.419090452187719,-0.408374313349663,-0.384702628642232,-0.328266125886046,
-0.321688290186996,-0.319156563088247,-0.317332702453529,-0.315393120830567,
-0.312813260737509,-0.307111715066948,-0.284195963295902,-0.233340123968605,
-0.231253244450221,-0.215570925639742,-0.212986407779205,-0.211661411573052,
-0.210640645945836,-0.21063259767656,-0.210624720817426,-0.210617004697119,
-0.210609439587844,-0.210602016435957,-0.210594726820411,-0.210587562955973,
-0.210580517691847,-0.210573584297352,-0.210566756412456,-0.210560028131177,
-0.210553393949895,-0.210546848679633,-0.210540387430724,-0.210534005674419,
-0.210527698994381,-0.210521463257463,-0.210515294582247,-0.210509189323113,
-0.21050314392979,-0.210497155008098,-0.210491219479333,-0.210485334399849,
-0.210479496741158,-0.20921701718876,-0.206832550359035,-0.19334069960194,
-0.157525544287272,-0.113371397423326,-0.109091499988174,-0.106554894876312,
-0.104615171834106,-0.102540411049315,-0.0992842990850559,-0.0889060651941913,
-0.0749176319822858),.UNSPECIFIED.);
#833=B_SPLINE_CURVE_WITH_KNOTS('',3,(#80281,#80282,#80283,#80284,#80285,
#80286,#80287,#80288,#80289,#80290,#80291,#80292,#80293,#80294,#80295,#80296,
#80297,#80298,#80299,#80300,#80301,#80302,#80303,#80304,#80305,#80306,#80307,
#80308,#80309,#80310,#80311,#80312,#80313,#80314,#80315,#80316,#80317,#80318,
#80319,#80320,#80321,#80322,#80323,#80324,#80325,#80326,#80327,#80328,#80329,
#80330,#80331,#80332,#80333,#80334,#80335,#80336,#80337,#80338,#80339,#80340,
#80341,#80342,#80343,#80344,#80345,#80346,#80347,#80348,#80349,#80350,#80351,
#80352,#80353,#80354,#80355,#80356,#80357,#80358,#80359,#80360,#80361,#80362,
#80363,#80364,#80365,#80366,#80367,#80368,#80369,#80370,#80371,#80372,#80373,
#80374,#80375,#80376,#80377,#80378,#80379,#80380,#80381,#80382,#80383,#80384,
#80385,#80386,#80387,#80388,#80389,#80390,#80391,#80392,#80393,#80394,#80395,
#80396,#80397,#80398,#80399,#80400,#80401,#80402,#80403,#80404,#80405,#80406,
#80407,#80408,#80409,#80410,#80411,#80412,#80413,#80414,#80415,#80416,#80417,
#80418,#80419,#80420,#80421,#80422,#80423,#80424,#80425,#80426,#80427,#80428,
#80429,#80430,#80431,#80432,#80433,#80434,#80435,#80436,#80437,#80438,#80439,
#80440,#80441,#80442,#80443,#80444,#80445,#80446,#80447,#80448,#80449,#80450,
#80451,#80452,#80453,#80454,#80455,#80456,#80457,#80458,#80459,#80460,#80461,
#80462,#80463,#80464,#80465,#80466,#80467,#80468,#80469,#80470,#80471,#80472,
#80473,#80474,#80475,#80476,#80477,#80478,#80479,#80480,#80481,#80482,#80483,
#80484,#80485,#80486,#80487,#80488,#80489,#80490,#80491,#80492,#80493,#80494,
#80495,#80496,#80497,#80498,#80499,#80500,#80501,#80502,#80503,#80504,#80505,
#80506,#80507,#80508,#80509,#80510),.UNSPECIFIED.,.F.,.F.,(4,2,2,2,2,2,
2,2,2,2,2,2,2,2,2,2,2,2,2,2,2,2,2,2,2,2,2,2,2,2,2,2,2,2,2,2,2,2,2,2,2,2,
2,2,2,2,2,2,2,2,2,2,2,2,2,2,2,2,2,2,2,2,2,2,2,2,2,2,2,2,2,2,2,2,2,2,2,2,
2,2,2,2,2,2,2,2,2,2,2,2,2,2,2,2,2,2,2,2,2,2,2,2,2,2,2,2,2,2,2,2,2,2,2,2,
4),(-2.59360340364756,-2.57256138631712,-2.5511722392252,-2.52301550873145,
-2.51638365243548,-2.51424433113592,-2.51215404354415,-2.51021879696438,
-2.5077149507316,-2.50354943372637,-2.47488951927506,-2.44415061377801,
-2.42040053984527,-2.40967571461453,-2.40744772913276,-2.40619083706372,
-2.40511921430145,-2.40377128206805,-2.40114974517762,-2.38511582430331,
-2.37974749555331,-2.33011817380235,-2.3073303447698,-2.30312526162724,
-2.30079622950563,-2.29888405526289,-2.29666371272857,-2.29285290562998,
-2.27799414844433,-2.26577003553844,-2.2101296064671,-2.19775202491306,
-2.19542091390671,-2.1941515954388,-2.19308083930896,-2.19174840654282,
-2.18968045830186,-2.17983290835504,-2.12787407010181,-2.0986295662347,
-2.09213164788723,-2.08941174157444,-2.08744763161007,-2.08565671622647,
-2.08280295027271,-2.07598897796227,-2.02201046904536,-1.99670885595042,
-1.98555634046624,-1.98329240682838,-1.98203764946754,-1.98096585615763,
-1.97961516960757,-1.97698077634107,-1.96061862186094,-1.95275972718494,
-1.9113643904438,-1.89271030025426,-1.8814787043257,-1.87812784636064,-1.87603163679148,
-1.87409844819305,-1.87160781687123,-1.8674871386554,-1.84053896816075,
-1.79860981765746,-1.78184881779291,-1.77323763734782,-1.77114615782812,
-1.76992929814559,-1.768852010821,-1.76746740761802,-1.76517834314845,-1.75150239063663,
-1.74978272647663,-1.70241634583266,-1.67144183938627,-1.66698984977577,
-1.6646542310998,-1.66274174095907,-1.66052676672508,-1.65673920557658,
-1.64214457813894,-1.62987905485822,-1.58946800527114,-1.57061431348597,
-1.56131551653981,-1.55917223486231,-1.55794395335048,-1.55686886081234,
-1.55547996957127,-1.55256526197488,-1.52372679175007,-1.48561706592977,
-1.4680913190089,-1.45735013842797,-1.45405245658675,-1.45196804348015,
-1.45003096048238,-1.44751443176755,-1.44330518777702,-1.41283118821453,
-1.36760503613842,-1.35571247943924,-1.35117739054435,-1.34786898136193,
-1.34640649833679,-1.34532179526139,-1.3441329069539,-1.34216696055788,
-1.33576185377284,-1.33420594521446,-1.31961940691524,-1.26057787761394,
-1.25976235679197),.UNSPECIFIED.);
#834=B_SPLINE_CURVE_WITH_KNOTS('',3,(#80516,#80517,#80518,#80519,#80520,
#80521,#80522,#80523),.UNSPECIFIED.,.F.,.F.,(4,2,2,4),(-0.0748537112472781,
-0.0742481380771646,-0.0252918457270349,-0.000629465073284334),
 .UNSPECIFIED.);
#835=B_SPLINE_CURVE_WITH_KNOTS('',3,(#80524,#80525,#80526,#80527,#80528,
#80529,#80530,#80531,#80532,#80533,#80534,#80535,#80536,#80537,#80538,#80539,
#80540,#80541,#80542,#80543,#80544,#80545,#80546,#80547,#80548,#80549,#80550,
#80551,#80552,#80553,#80554,#80555,#80556,#80557,#80558,#80559,#80560,#80561,
#80562,#80563,#80564,#80565,#80566,#80567,#80568,#80569,#80570,#80571,#80572,
#80573,#80574,#80575,#80576,#80577,#80578,#80579,#80580,#80581,#80582,#80583,
#80584,#80585,#80586,#80587,#80588,#80589,#80590,#80591,#80592,#80593,#80594,
#80595,#80596,#80597,#80598,#80599,#80600,#80601,#80602,#80603,#80604,#80605,
#80606,#80607,#80608,#80609,#80610,#80611,#80612,#80613,#80614,#80615,#80616,
#80617,#80618,#80619,#80620,#80621,#80622,#80623,#80624,#80625,#80626,#80627,
#80628,#80629,#80630,#80631,#80632,#80633,#80634,#80635,#80636,#80637,#80638,
#80639,#80640,#80641,#80642,#80643,#80644,#80645,#80646,#80647,#80648,#80649,
#80650,#80651,#80652,#80653,#80654,#80655,#80656,#80657,#80658,#80659,#80660,
#80661,#80662,#80663,#80664,#80665,#80666,#80667,#80668,#80669,#80670,#80671,
#80672,#80673,#80674,#80675,#80676,#80677,#80678,#80679,#80680,#80681,#80682,
#80683,#80684,#80685,#80686,#80687,#80688,#80689,#80690,#80691,#80692,#80693,
#80694,#80695,#80696,#80697,#80698,#80699,#80700,#80701,#80702,#80703,#80704,
#80705,#80706,#80707,#80708,#80709,#80710,#80711,#80712,#80713,#80714,#80715,
#80716,#80717,#80718,#80719,#80720,#80721,#80722,#80723,#80724,#80725,#80726,
#80727,#80728,#80729,#80730,#80731,#80732,#80733,#80734,#80735,#80736,#80737,
#80738,#80739,#80740,#80741,#80742,#80743,#80744,#80745,#80746,#80747,#80748,
#80749,#80750,#80751,#80752,#80753,#80754,#80755,#80756,#80757,#80758,#80759,
#80760,#80761,#80762,#80763,#80764,#80765,#80766,#80767,#80768,#80769,#80770,
#80771,#80772,#80773,#80774,#80775,#80776,#80777,#80778,#80779,#80780,#80781),
 .UNSPECIFIED.,.F.,.F.,(4,2,2,2,2,2,2,2,2,2,2,2,2,2,2,2,2,2,2,2,2,2,2,2,
2,2,2,2,2,2,2,2,2,2,2,2,2,2,2,2,2,2,2,2,2,2,2,2,2,2,2,2,2,2,2,2,2,2,2,2,
2,2,2,2,2,2,2,2,2,2,2,2,2,2,2,2,2,2,2,2,2,2,2,2,2,2,2,2,2,2,2,2,2,2,2,2,
2,2,2,2,2,2,2,2,2,2,2,2,2,2,2,2,2,2,2,2,2,2,2,2,2,2,2,2,2,2,2,2,4),(-2.66787357995012,
-2.66007952305088,-2.6547829299014,-2.65233947880885,-2.65045756852206,
-2.64861680673795,-2.64679034936771,-2.64424988281189,-2.63905856459427,
-2.62654797522341,-2.57487722209167,-2.55603430300991,-2.54673913222438,
-2.54459620358012,-2.5433680465749,-2.54229301224663,-2.54090412918185,
-2.53798920207424,-2.50829197952501,-2.45784167081142,-2.44835244368186,
-2.44374506839699,-2.4399658886159,-2.43779513881799,-2.43777944411622,
-2.43776319681168,-2.43774637681734,-2.43772896331178,-2.43771093465628,
-2.43769226847276,-2.43767294154989,-2.43765292981784,-2.43763220836344,
-2.43761075138144,-2.43758853216956,-2.43756552233064,-2.43754548574042,
-2.43752213510058,-2.43749492833802,-2.43746323740148,-2.43742633595271,
-2.43738338573796,-2.43732917339247,-2.43538841738136,-2.43284636145566,
-2.42854811310968,-2.3934263502408,-2.34446749666977,-2.33476696161901,
-2.33259567850242,-2.33136141126727,-2.33028756323901,-2.32890877629817,
-2.3260448467984,-2.29008787484562,-2.2573219623038,-2.23476228845003,-2.22910880690954,
-2.22653758761028,-2.22459917777942,-2.22277251411468,-2.22023063764096,
-2.21358963927326,-2.15778389595365,-2.13372116995794,-2.12289772429747,
-2.12065375760462,-2.11940352527556,-2.11833157456533,-2.11697553259889,
-2.11482997417052,-2.10379328073334,-2.0525752023922,-2.02386569585539,
-2.0174319174313,-2.01472320811927,-2.0127615134479,-2.01096890432522,-2.00810398368554,
-2.00121966482396,-1.94814357879202,-1.92223606838301,-1.91092874707077,
-1.90865624862904,-1.90739982387573,-1.90632847849168,-1.9049807410111,
-1.90235912942254,-1.88631694266447,-1.8810260332003,-1.86644143482478,
-1.83354904035393,-1.81698193268487,-1.80666937147902,-1.80342036504989,
-1.80134689793032,-1.79940611478273,-1.79686485256737,-1.79256980511797,
-1.75745725127151,-1.70855188049012,-1.69878122353251,-1.69660497181993,
-1.69536953386231,-1.69429572638613,-1.69291837619435,-1.69006220057868,
-1.66726170284572,-1.61165236203527,-1.59564067734481,-1.59187115493372,
-1.58968264924329,-1.58776841522675,-1.58539909578318,-1.58176566734115,
-1.5646682505217,-1.55659954196284,-1.52178855986863,-1.49773837571906,
-1.48691856672895,-1.48467491309625,-1.48342479338141,-1.48235290111825,
-1.4809968841986,-1.47833656340552,-1.46128286132611,-1.44267045856224,
-1.40971371125424,-1.40850074877309),.UNSPECIFIED.);
#836=B_SPLINE_CURVE_WITH_KNOTS('',3,(#80783,#80784,#80785,#80786,#80787,
#80788,#80789,#80790,#80791,#80792,#80793,#80794,#80795,#80796,#80797,#80798,
#80799,#80800,#80801,#80802,#80803,#80804,#80805,#80806,#80807,#80808,#80809,
#80810,#80811,#80812,#80813,#80814,#80815,#80816,#80817,#80818,#80819,#80820,
#80821,#80822,#80823,#80824,#80825,#80826,#80827,#80828,#80829,#80830,#80831,
#80832,#80833,#80834,#80835,#80836,#80837,#80838,#80839,#80840,#80841,#80842,
#80843,#80844,#80845,#80846,#80847,#80848,#80849,#80850,#80851,#80852,#80853,
#80854,#80855,#80856,#80857,#80858,#80859,#80860,#80861,#80862,#80863,#80864,
#80865,#80866,#80867,#80868,#80869,#80870,#80871,#80872,#80873,#80874,#80875,
#80876,#80877,#80878,#80879,#80880,#80881,#80882,#80883,#80884,#80885,#80886,
#80887,#80888,#80889,#80890,#80891,#80892,#80893,#80894,#80895,#80896,#80897,
#80898,#80899,#80900,#80901,#80902,#80903,#80904,#80905,#80906,#80907,#80908,
#80909,#80910,#80911,#80912,#80913,#80914,#80915,#80916,#80917,#80918,#80919,
#80920,#80921,#80922,#80923,#80924,#80925,#80926,#80927,#80928,#80929,#80930,
#80931,#80932,#80933,#80934,#80935,#80936,#80937,#80938,#80939,#80940,#80941,
#80942,#80943,#80944,#80945,#80946,#80947,#80948,#80949,#80950,#80951,#80952,
#80953,#80954,#80955,#80956,#80957,#80958,#80959,#80960,#80961,#80962,#80963,
#80964,#80965,#80966,#80967,#80968,#80969,#80970,#80971,#80972,#80973,#80974,
#80975,#80976,#80977,#80978,#80979,#80980,#80981,#80982,#80983,#80984,#80985,
#80986,#80987,#80988,#80989,#80990,#80991,#80992),.UNSPECIFIED.,.F.,.F.,
(4,2,2,2,2,2,2,2,2,2,2,2,2,2,2,2,2,2,2,2,2,2,2,2,2,2,2,2,2,2,2,2,2,2,2,
2,2,2,2,2,2,2,2,2,2,2,2,2,2,2,2,2,2,2,2,2,2,2,2,2,2,2,2,2,2,2,2,2,2,2,2,
2,2,2,2,2,2,2,2,2,2,2,2,2,2,2,2,2,2,2,2,2,2,2,2,2,2,2,2,2,2,2,2,2,4),(-1.25976235679197,
-1.24626820017445,-1.24250651621246,-1.24029768477833,-1.23838503090232,
-1.236042305457,-1.23155538041799,-1.19919364072031,-1.15901211212556,-1.15407926751949,
-1.13812902112765,-1.13551244877831,-1.13416572897147,-1.13309436405029,
-1.13183696125577,-1.12956025357522,-1.11818237288597,-1.09199616666393,
-1.03926923928351,-1.0323550250493,-1.02948503966214,-1.02769140453988,
-1.02573031367983,-1.02302559328425,-1.01661619053952,-0.988116890300663,
-0.937184400075926,-0.925703478976986,-0.923531070722116,-0.922166818820405,
-0.921094174941895,-0.919849766402907,-0.917632613690453,-0.907242331803809,
-0.88474480639707,-0.826437139346686,-0.820077536526286,-0.817581369715969,
-0.815766632341883,-0.813821312867422,-0.811207056028172,-0.805316664753698,
-0.780975561266437,-0.730307518474436,-0.714076158412379,-0.711447501238598,
-0.710098232471539,-0.709026765673658,-0.707771472672896,-0.705504239768999,
-0.694289042834435,-0.668738500796957,-0.615102074242418,-0.608259444881277,
-0.605401353355504,-0.603609960979995,-0.601647139746122,-0.598932347283126,
-0.592462547390376,-0.538190467564313,-0.502341470790713,-0.49948276983982,
-0.498104964751824,-0.497031157507482,-0.495796128800669,-0.493621562090834,
-0.483874740392211,-0.434926281688211,-0.399782672617695,-0.395494935780452,
-0.392955909870843,-0.391015619219038,-0.3889414977907,-0.385688997314133,
-0.375344394068019,-0.358708143016554,-0.325787971312303,-0.307705323540847,
-0.290152337107941,-0.28747409124646,-0.286114285592324,-0.285042149979008,
-0.283794908271799,-0.281564257964448,-0.270955442677452,-0.247674379497308,
-0.191965057539896,-0.184499505664943,-0.181536909186454,-0.179726412110841,
-0.177896471607758,-0.175389977398866,-0.170058138140225,-0.16297530619806,
-0.145592391782818,-0.0967472308571914,-0.0782163418531925,-0.0754719491544447,
-0.0741169405276754,-0.0730452173091221,-0.0717945786023242,-0.0695481925536985,
-0.0586810442108745,-0.0344507151062333,-0.000629544781513296),
 .UNSPECIFIED.);
#837=B_SPLINE_CURVE_WITH_KNOTS('',3,(#80993,#80994,#80995,#80996,#80997,
#80998,#80999,#81000,#81001,#81002,#81003,#81004,#81005,#81006,#81007,#81008,
#81009,#81010,#81011,#81012,#81013,#81014),.UNSPECIFIED.,.F.,.F.,(4,2,2,
2,2,2,2,2,2,2,4),(-2.6677880043013,-2.64246090365341,-2.63933381754846,
-2.63718766808863,-2.63538680183029,-2.63347278998466,-2.63110354900661,
-2.62746987279902,-2.6103639371884,-2.59817297007628,-2.59336440692509),
 .UNSPECIFIED.);
#838=B_SPLINE_CURVE_WITH_KNOTS('',3,(#81019,#81020,#81021,#81022,#81023,
#81024,#81025,#81026,#81027,#81028,#81029,#81030,#81031,#81032,#81033,#81034,
#81035,#81036,#81037,#81038,#81039,#81040,#81041,#81042,#81043,#81044,#81045,
#81046,#81047,#81048,#81049,#81050,#81051,#81052,#81053,#81054,#81055,#81056,
#81057,#81058,#81059,#81060,#81061,#81062,#81063,#81064,#81065,#81066,#81067,
#81068,#81069,#81070,#81071,#81072,#81073,#81074,#81075,#81076,#81077,#81078,
#81079,#81080,#81081,#81082,#81083,#81084,#81085,#81086,#81087,#81088,#81089,
#81090,#81091,#81092,#81093,#81094,#81095,#81096,#81097,#81098,#81099,#81100,
#81101,#81102,#81103,#81104,#81105,#81106,#81107,#81108,#81109,#81110,#81111,
#81112,#81113,#81114,#81115,#81116,#81117,#81118,#81119,#81120,#81121,#81122,
#81123,#81124,#81125,#81126,#81127,#81128,#81129,#81130,#81131,#81132,#81133,
#81134,#81135,#81136,#81137,#81138,#81139,#81140,#81141,#81142,#81143,#81144,
#81145,#81146,#81147,#81148,#81149,#81150,#81151,#81152,#81153,#81154,#81155,
#81156,#81157,#81158,#81159,#81160,#81161,#81162,#81163,#81164,#81165,#81166,
#81167,#81168,#81169,#81170,#81171,#81172,#81173,#81174,#81175,#81176,#81177,
#81178,#81179,#81180,#81181,#81182,#81183,#81184,#81185,#81186,#81187,#81188,
#81189,#81190,#81191,#81192,#81193,#81194,#81195,#81196,#81197,#81198,#81199,
#81200,#81201,#81202,#81203,#81204,#81205,#81206,#81207,#81208,#81209,#81210,
#81211,#81212,#81213,#81214,#81215,#81216,#81217,#81218,#81219,#81220,#81221,
#81222,#81223,#81224,#81225,#81226,#81227,#81228,#81229,#81230,#81231,#81232,
#81233,#81234,#81235,#81236,#81237,#81238,#81239,#81240,#81241,#81242,#81243,
#81244,#81245,#81246,#81247,#81248,#81249,#81250,#81251,#81252),
 .UNSPECIFIED.,.F.,.F.,(4,2,2,2,2,2,2,2,2,2,2,2,2,2,2,2,2,2,2,2,2,2,2,2,
2,2,2,2,2,2,2,2,2,2,2,2,2,2,2,2,2,2,2,2,2,2,2,2,2,2,2,2,2,2,2,2,2,2,2,2,
2,2,2,2,2,2,2,2,2,2,2,2,2,2,2,2,2,2,2,2,2,2,2,2,2,2,2,2,2,2,2,2,2,2,2,2,
2,2,2,2,2,2,2,2,2,2,2,2,2,2,2,2,2,2,2,2,4),(-1.40847046428017,-1.40132352298175,
-1.37516890792839,-1.36379827702942,-1.36152197446538,-1.36026464062407,
-1.35919324415307,-1.35784636364615,-1.35522912551683,-1.33926697255163,
-1.33432292216282,-1.32867694362814,-1.28171652932453,-1.28027334419647,
-1.26123206893809,-1.25747072348756,-1.25506190165986,-1.25314412556238,
-1.25098193577219,-1.24733221406709,-1.23288124413848,-1.18249242530521,
-1.15282398962037,-1.14990947138451,-1.14852069375532,-1.14744569607883,
-1.14621753994888,-1.1440745024417,-1.13477745886532,-1.11592580700965,
-1.07547219843435,-1.06319339613209,-1.04861347491532,-1.04482746730749,
-1.04261299377957,-1.04070068826315,-1.03836498344053,-1.03391186611421,
-1.00287554051865,-0.954897464000928,-0.940308394020928,-0.937976019532825,
-0.936578771059989,-0.93549996646566,-0.934290695070962,-0.93223296160082,
-0.924037446645905,-0.908471043793413,-0.86688692951543,-0.837982836940759,
-0.833811356119599,-0.831306001341352,-0.829370801191866,-0.827281764944157,
-0.823962531284684,-0.813022789874797,-0.795045951150402,-0.744623147091577,
-0.728417163136248,-0.725789283072615,-0.72444008630442,-0.723368505314425,
-0.722112880174972,-0.71984454505754,-0.708613735516601,-0.683004782707691,
-0.629442188046572,-0.6225921673684,-0.619732647821296,-0.617940842434842,
-0.615977957395679,-0.613263791885522,-0.606798897371197,-0.552722670112585,
-0.516660413468051,-0.51380066915979,-0.512422560592397,-0.511348610414594,
-0.510113522915429,-0.507939104981787,-0.498197107877221,-0.449237654418865,
-0.414102807337012,-0.40980635345955,-0.40726464369366,-0.405323729275715,
-0.403250325111179,-0.400001840352817,-0.389694415829426,-0.373141176416832,
-0.340287500554374,-0.32728540853776,-0.304664045697818,-0.301812381731855,
-0.300435946598413,-0.299362255983898,-0.298126286934198,-0.295947492322959,
-0.286139094692546,-0.237241731478906,-0.202131567716715,-0.197834504820012,
-0.195292756248984,-0.193351997280235,-0.191344263213684,-0.188242470263319,
-0.18461585140243,-0.177819650839178,-0.161438226066528,-0.128729471565566,
-0.092700370640288,-0.0898402863548513,-0.088462274498264,-0.0873885219422777,
-0.0861537996592544,-0.0839803541722877,-0.0748537112472781),
 .UNSPECIFIED.);
#839=B_SPLINE_CURVE_WITH_KNOTS('',3,(#81253,#81254,#81255,#81256,#81257,
#81258,#81259,#81260,#81261,#81262,#81263,#81264,#81265,#81266,#81267,#81268,
#81269,#81270,#81271,#81272,#81273,#81274,#81275,#81276,#81277,#81278,#81279,
#81280,#81281,#81282,#81283,#81284,#81285,#81286,#81287,#81288,#81289,#81290,
#81291,#81292,#81293,#81294,#81295,#81296,#81297,#81298,#81299,#81300,#81301,
#81302,#81303,#81304,#81305,#81306,#81307,#81308,#81309,#81310,#81311,#81312,
#81313,#81314,#81315,#81316,#81317,#81318,#81319,#81320,#81321,#81322,#81323,
#81324,#81325,#81326,#81327,#81328,#81329,#81330,#81331,#81332,#81333,#81334,
#81335,#81336,#81337,#81338,#81339,#81340,#81341,#81342,#81343,#81344,#81345,
#81346,#81347,#81348,#81349,#81350,#81351,#81352,#81353,#81354,#81355,#81356,
#81357,#81358,#81359,#81360,#81361,#81362,#81363,#81364,#81365,#81366,#81367,
#81368,#81369,#81370,#81371,#81372,#81373,#81374,#81375,#81376,#81377,#81378,
#81379,#81380,#81381,#81382,#81383,#81384,#81385,#81386,#81387,#81388,#81389,
#81390,#81391,#81392,#81393,#81394,#81395,#81396,#81397,#81398,#81399,#81400,
#81401,#81402,#81403,#81404,#81405,#81406,#81407,#81408,#81409,#81410,#81411,
#81412,#81413,#81414,#81415,#81416,#81417,#81418,#81419,#81420,#81421,#81422,
#81423,#81424,#81425,#81426,#81427,#81428,#81429,#81430,#81431,#81432,#81433,
#81434,#81435,#81436,#81437,#81438,#81439,#81440,#81441,#81442,#81443,#81444,
#81445,#81446,#81447,#81448,#81449,#81450,#81451,#81452,#81453,#81454,#81455,
#81456,#81457,#81458,#81459,#81460,#81461,#81462,#81463,#81464,#81465,#81466,
#81467,#81468,#81469,#81470,#81471,#81472,#81473,#81474,#81475,#81476,#81477,
#81478,#81479,#81480,#81481,#81482,#81483,#81484,#81485,#81486,#81487,#81488,
#81489,#81490,#81491,#81492,#81493,#81494,#81495,#81496,#81497,#81498,#81499,
#81500,#81501,#81502,#81503,#81504,#81505,#81506,#81507,#81508,#81509,#81510,
#81511,#81512,#81513,#81514,#81515,#81516,#81517,#81518,#81519,#81520,#81521,
#81522,#81523,#81524),.UNSPECIFIED.,.F.,.F.,(4,2,2,2,2,2,2,2,2,2,2,2,2,
2,2,2,2,2,2,2,2,2,2,2,2,2,2,2,2,2,2,2,2,2,2,2,2,2,2,2,2,2,2,2,2,2,2,2,2,
2,2,2,2,2,2,2,2,2,2,2,2,2,2,2,2,2,2,2,2,2,2,2,2,2,2,2,2,2,2,2,2,2,2,2,2,
2,2,2,2,2,2,2,2,2,2,2,2,2,2,2,2,2,2,2,2,2,2,2,2,2,2,2,2,2,2,2,2,2,2,2,2,
2,2,2,2,2,2,2,2,2,2,2,2,2,2,4),(-2.59336440692509,-2.55352828350367,-2.53505701142379,
-2.53122442869316,-2.52967258864427,-2.52857286897742,-2.52755811021205,
-2.52587166995057,-2.52150532217003,-2.47379324060003,-2.44450201015887,
-2.43448885743048,-2.42970049862564,-2.42580682697683,-2.42360320076253,
-2.42359053035804,-2.42357742258592,-2.4235638611813,-2.4235498292744,-2.42353530638362,
-2.42352027587282,-2.42350472032353,-2.42348861994496,-2.42347195416413,
-2.42345470152217,-2.42343683970557,-2.42341834549094,-2.42339919465093,
-2.42337936200965,-2.42335882136724,-2.42333754541899,-2.4233155057623,
-2.42329267219068,-2.4232733641008,-2.42325080766968,-2.42322445319372,
-2.42319365740929,-2.42315766767554,-2.42311560362571,-2.42306770789945,
-2.42112699268115,-2.41858504650969,-2.41428711006614,-2.37917263951499,
-2.33023652674197,-2.32051020260422,-2.31833716733843,-2.31710252607242,
-2.31602875148292,-2.31465058069139,-2.31178973116941,-2.27575005051651,
-2.22155102093976,-2.21514494306319,-2.2124410403361,-2.21048033165337,
-2.20868690476235,-2.20581693278741,-2.19890107411085,-2.14626117479252,
-2.1200537036965,-2.10867059178548,-2.10639388181172,-2.10513660242519,
-2.10406542169799,-2.10271902780342,-2.1001033673971,-2.08416512341129,
-2.07847906392991,-2.06417027831973,-2.03128355126708,-2.0147214613364,
-2.0044113905213,-2.00116283204631,-1.99908956992277,-1.99714892184211,
-1.99460775452005,-1.99031268376186,-1.95517547731458,-1.90618873829942,
-1.89651929532217,-1.89435012157751,-1.89311629951435,-1.89204235453933,
-1.89066280893114,-1.88843968609813,-1.87605207030594,-1.8729889090395,
-1.87279059541371,-1.86592304485023,-1.85219045972894,-1.8193075068519,
-1.80275161124286,-1.79244413964882,-1.78919573134311,-1.78712240432094,
-1.78518158257353,-1.78264002490765,-1.77834392916455,-1.74314884891007,
-1.69397734468337,-1.68451769984892,-1.68236311321726,-1.68113244848262,
-1.68005792827272,-1.67867327477203,-1.67577973947107,-1.6497449430723,
-1.61157746531009,-1.58254918462702,-1.57815351942445,-1.57582991862997,
-1.57391828909574,-1.57169413805559,-1.56786583439451,-1.5528043005564,
-1.50063521466255,-1.48178940586435,-1.47249345335754,-1.47035052877893,
-1.4691224038069,-1.4680474168998,-1.46665862069468,-1.46374396626898,-1.43369740855554,
-1.38235508191602,-1.36901471600201,-1.36545962391766,-1.36331844013418,
-1.36139713145788,-1.35895376713785,-1.35507915828794,-1.33400470217004,
-1.27618798964858,-1.26122697294337,-1.25979252647547),.UNSPECIFIED.);
#840=B_SPLINE_CURVE_WITH_KNOTS('',3,(#81530,#81531,#81532,#81533),
 .UNSPECIFIED.,.F.,.F.,(4,4),(120.339865595025,120.689851222995),
 .UNSPECIFIED.);
#841=B_SPLINE_CURVE_WITH_KNOTS('',3,(#81534,#81535,#81536,#81537,#81538,
#81539,#81540,#81541,#81542,#81543,#81544,#81545,#81546,#81547,#81548,#81549,
#81550,#81551,#81552,#81553,#81554,#81555,#81556,#81557,#81558,#81559,#81560,
#81561,#81562,#81563,#81564,#81565,#81566,#81567,#81568,#81569,#81570,#81571,
#81572,#81573,#81574,#81575,#81576,#81577,#81578,#81579,#81580,#81581,#81582,
#81583,#81584,#81585,#81586,#81587,#81588,#81589,#81590,#81591,#81592,#81593,
#81594,#81595,#81596,#81597,#81598,#81599,#81600,#81601,#81602,#81603,#81604,
#81605,#81606,#81607,#81608,#81609,#81610,#81611,#81612,#81613,#81614,#81615,
#81616,#81617,#81618,#81619,#81620,#81621,#81622,#81623,#81624,#81625,#81626,
#81627,#81628,#81629,#81630,#81631,#81632,#81633,#81634,#81635,#81636,#81637,
#81638,#81639,#81640,#81641,#81642,#81643,#81644,#81645,#81646,#81647,#81648,
#81649,#81650,#81651,#81652,#81653,#81654,#81655,#81656,#81657,#81658,#81659,
#81660,#81661,#81662,#81663,#81664,#81665,#81666,#81667,#81668,#81669,#81670,
#81671,#81672,#81673,#81674,#81675,#81676,#81677,#81678,#81679,#81680,#81681,
#81682,#81683,#81684,#81685,#81686,#81687,#81688,#81689,#81690,#81691,#81692,
#81693,#81694,#81695,#81696,#81697,#81698,#81699,#81700,#81701,#81702,#81703,
#81704,#81705,#81706,#81707,#81708,#81709,#81710,#81711,#81712,#81713,#81714,
#81715,#81716,#81717,#81718,#81719,#81720,#81721,#81722,#81723,#81724,#81725,
#81726,#81727,#81728,#81729,#81730,#81731,#81732,#81733,#81734,#81735,#81736,
#81737,#81738,#81739,#81740,#81741,#81742,#81743,#81744,#81745,#81746,#81747,
#81748,#81749,#81750,#81751),.UNSPECIFIED.,.F.,.F.,(4,2,2,2,2,2,2,2,2,2,
2,2,2,2,2,2,2,2,2,2,2,2,2,2,2,2,2,2,2,2,2,2,2,2,2,2,2,2,2,2,2,2,2,2,2,2,
2,2,2,2,2,2,2,2,2,2,2,2,2,2,2,2,2,2,2,2,2,2,2,2,2,2,2,2,2,2,2,2,2,2,2,2,
2,2,2,2,2,2,2,2,2,2,2,2,2,2,2,2,2,2,2,2,2,2,2,2,2,2,4),(-2.66761347800519,
-2.6433834721182,-2.63625151418383,-2.6344605986207,-2.63324562918053,-2.63223654706512,
-2.63116196370503,-2.62977592206083,-2.62687490453753,-2.59995438394439,
-2.58627120477344,-2.57475044801003,-2.54617410255535,-2.53227597603649,
-2.5286724497231,-2.52652058051867,-2.52460130391527,-2.52217626522362,
-2.5174445027455,-2.48000718468932,-2.42965580471258,-2.42318147430023,
-2.42128999998669,-2.42027902641582,-2.41920575391483,-2.41783408622734,
-2.41563718858464,-2.40380140420529,-2.34640651839376,-2.32984068112255,
-2.31952892163212,-2.31628017359891,-2.31420687278027,-2.31226624627227,
-2.30972519057587,-2.3054304953408,-2.2703212410984,-2.2214212514753,-2.21164967386911,
-2.20947348073862,-2.20823811664349,-2.20716439935445,-2.20578719881336,
-2.20293145037008,-2.1667815175419,-2.1340772828521,-2.11161423548992,-2.105973787024,
-2.10340493239071,-2.10146685306004,-2.09963943268177,-2.09709478730645,
-2.09043627800359,-2.03479837324969,-2.01062429006053,-1.99977076078248,
-1.99752493983372,-1.99627428726215,-1.99520235380513,-1.99384681784614,
-1.9911890366621,-1.97420781840533,-1.92397680279609,-1.90639062592672,
-1.89562347727925,-1.89232338664344,-1.8902387379499,-1.88830232422253,
-1.88578792521051,-1.88158501522212,-1.85135605137762,-1.79985750068206,
-1.78786948078818,-1.78555919209865,-1.78429455517402,-1.78322379469047,
-1.78188637381476,-1.77980165691238,-1.7697077673214,-1.76421756231126,
-1.75679091328359,-1.7432832209496,-1.71040118646671,-1.69384734487439,
-1.68354068589893,-1.6802922854624,-1.67821890379077,-1.67627798896135,
-1.67373624889946,-1.66943970920898,-1.63422230751653,-1.5849768578298,
-1.57559915897596,-1.57345035128136,-1.57222092901265,-1.57114615644823,
-1.56975941623923,-1.56751267435131,-1.55467956045432,-1.55251360859266,
-1.50523272964611,-1.47670829575112,-1.47029626611204,-1.46759105332923,
-1.46562983216923,-1.46383623793925,-1.4609666551701,-1.45405513324635,
-1.40847046428017),.UNSPECIFIED.);
#842=B_SPLINE_CURVE_WITH_KNOTS('',3,(#81753,#81754,#81755,#81756,#81757,
#81758,#81759,#81760,#81761,#81762,#81763,#81764,#81765,#81766,#81767,#81768,
#81769,#81770,#81771,#81772,#81773,#81774,#81775,#81776,#81777,#81778,#81779,
#81780,#81781,#81782,#81783,#81784,#81785,#81786,#81787,#81788,#81789,#81790,
#81791,#81792,#81793,#81794,#81795,#81796,#81797,#81798,#81799,#81800,#81801,
#81802,#81803,#81804,#81805,#81806,#81807,#81808,#81809,#81810,#81811,#81812,
#81813,#81814,#81815,#81816,#81817,#81818,#81819,#81820,#81821,#81822,#81823,
#81824,#81825,#81826,#81827,#81828,#81829,#81830,#81831,#81832,#81833,#81834,
#81835,#81836,#81837,#81838,#81839,#81840,#81841,#81842,#81843,#81844,#81845,
#81846,#81847,#81848,#81849,#81850,#81851,#81852,#81853,#81854,#81855,#81856,
#81857,#81858,#81859,#81860,#81861,#81862,#81863,#81864,#81865,#81866,#81867,
#81868,#81869,#81870,#81871,#81872,#81873,#81874,#81875,#81876,#81877,#81878,
#81879,#81880,#81881,#81882,#81883,#81884,#81885,#81886,#81887,#81888,#81889,
#81890,#81891,#81892,#81893,#81894,#81895,#81896,#81897,#81898,#81899,#81900,
#81901,#81902,#81903,#81904,#81905,#81906,#81907,#81908,#81909,#81910,#81911,
#81912,#81913,#81914,#81915,#81916,#81917,#81918,#81919,#81920,#81921,#81922,
#81923,#81924,#81925,#81926,#81927,#81928,#81929,#81930,#81931,#81932,#81933,
#81934,#81935,#81936,#81937,#81938,#81939,#81940,#81941,#81942,#81943,#81944,
#81945,#81946,#81947,#81948,#81949,#81950,#81951,#81952,#81953,#81954,#81955,
#81956,#81957,#81958,#81959,#81960,#81961,#81962,#81963,#81964,#81965,#81966,
#81967,#81968,#81969,#81970,#81971,#81972,#81973,#81974),.UNSPECIFIED.,
 .F.,.F.,(4,2,2,2,2,2,2,2,2,2,2,2,2,2,2,2,2,2,2,2,2,2,2,2,2,2,2,2,2,2,2,
2,2,2,2,2,2,2,2,2,2,2,2,2,2,2,2,2,2,2,2,2,2,2,2,2,2,2,2,2,2,2,2,2,2,2,2,
2,2,2,2,2,2,2,2,2,2,2,2,2,2,2,2,2,2,2,2,2,2,2,2,2,2,2,2,2,2,2,2,2,2,2,2,
2,2,2,2,2,2,2,4),(-1.25979252647547,-1.25887889341592,-1.25747705737434,
-1.25639764392859,-1.25519095057337,-1.25314477252933,-1.24508712466656,
-1.22990744614211,-1.19000994758103,-1.15896508172533,-1.15474340551486,
-1.15222338942829,-1.15028591448972,-1.14820333179291,-1.14491332875123,
-1.13423934940233,-1.11686744616279,-1.06816234198595,-1.06164762621188,
-1.04902404099949,-1.04678821408002,-1.04540474022874,-1.04433028019705,
-1.04309873277261,-1.04094033831612,-1.03142837623245,-0.982273139227336,
-0.947076376235956,-0.942779910067417,-0.940238221103645,-0.938297338737498,
-0.936223984487176,-0.932975610658268,-0.922668813952225,-0.906116845268339,
-0.873264580199634,-0.860348600354246,-0.837642694366873,-0.834789000078278,
-0.833412181479801,-0.832338472363633,-0.83110279901225,-0.828925284820705,
-0.819135261721587,-0.77022351376216,-0.735105339481279,-0.730810309447051,
-0.72826917455433,-0.726328545106829,-0.724255296039391,-0.7210067425078,
-0.710696472033711,-0.694136163459701,-0.661279012089867,-0.647506749294093,
-0.640733385971472,-0.638821061207603,-0.625183769865074,-0.62289719329886,
-0.621513569018754,-0.620436718197538,-0.619219996360079,-0.617127934419265,
-0.608503208895952,-0.591697035856527,-0.549706679495292,-0.52286696538262,
-0.518749929312503,-0.516260844577871,-0.514328456616962,-0.512232714107069,
-0.50888172952339,-0.497641368345566,-0.478966723314332,-0.438839923941719,
-0.41380087582269,-0.410918952487877,-0.409536720207729,-0.408462617229743,
-0.407230796527176,-0.405070307433445,-0.395523297753743,-0.346412592340616,
-0.311234327402151,-0.306939055184372,-0.304398034491327,-0.302457640524534,
-0.300384786772966,-0.297137152755538,-0.28683232985951,-0.270283175851369,
-0.237936898606343,-0.201815507226788,-0.198960473064593,-0.197583584042405,
-0.196557069340875,-0.195363682822098,-0.193380726592143,-0.190940963612911,
-0.185982559260592,-0.17243164223367,-0.149608806289563,-0.103071661430291,
-0.0958752135165292,-0.0929587241486494,-0.091156918417348,-0.0892033949999929,
-0.0865388798007457,-0.0803614985460654,-0.0537590801016044,-0.000629603543800122),
 .UNSPECIFIED.);
#843=B_SPLINE_CURVE_WITH_KNOTS('',3,(#81975,#81976,#81977,#81978,#81979,
#81980,#81981,#81982,#81983,#81984,#81985,#81986,#81987,#81988,#81989,#81990,
#81991,#81992,#81993,#81994,#81995,#81996,#81997,#81998),.UNSPECIFIED.,
 .F.,.F.,(4,2,2,2,2,2,2,2,2,2,2,4),(-2.66790098184336,-2.65984464261496,
-2.65548769960189,-2.65407479042277,-2.65300760105439,-2.65197745200527,
-2.65079760878932,-2.64887250690142,-2.64280732657753,-2.64152539353864,
-2.63372545384238,-2.59364855829229),.UNSPECIFIED.);
#844=B_SPLINE_CURVE_WITH_KNOTS('',3,(#82004,#82005,#82006,#82007,#82008,
#82009,#82010,#82011,#82012,#82013,#82014,#82015,#82016),.UNSPECIFIED.,
 .F.,.F.,(4,3,3,3,4),(114.057240355702,114.163813747114,114.270250447716,
114.376547360525,114.406671945289),.UNSPECIFIED.);
#845=B_SPLINE_CURVE_WITH_KNOTS('',3,(#82017,#82018,#82019,#82020,#82021,
#82022,#82023,#82024,#82025,#82026),.UNSPECIFIED.,.F.,.F.,(4,1,1,1,1,1,
1,4),(114.406674973147,114.866191745616,115.865028195577,116.863864645539,
117.862701095501,118.861537545463,119.860373995425,120.339865595025),
 .UNSPECIFIED.);
#846=B_SPLINE_CURVE_WITH_KNOTS('',3,(#82027,#82028,#82029,#82030,#82031,
#82032,#82033,#82034,#82035,#82036,#82037,#82038,#82039,#82040,#82041,#82042,
#82043,#82044,#82045,#82046,#82047,#82048,#82049,#82050,#82051,#82052,#82053,
#82054,#82055,#82056,#82057,#82058,#82059,#82060,#82061,#82062,#82063,#82064,
#82065,#82066,#82067,#82068,#82069,#82070,#82071,#82072,#82073,#82074,#82075,
#82076,#82077,#82078,#82079,#82080,#82081,#82082,#82083,#82084,#82085,#82086,
#82087,#82088,#82089,#82090,#82091,#82092,#82093,#82094,#82095,#82096,#82097,
#82098,#82099,#82100,#82101,#82102,#82103,#82104,#82105,#82106,#82107,#82108,
#82109,#82110,#82111,#82112,#82113,#82114,#82115,#82116,#82117,#82118,#82119,
#82120,#82121,#82122,#82123,#82124,#82125,#82126,#82127,#82128,#82129,#82130,
#82131,#82132,#82133,#82134,#82135,#82136,#82137,#82138,#82139,#82140,#82141,
#82142,#82143,#82144,#82145,#82146,#82147,#82148,#82149,#82150,#82151,#82152,
#82153,#82154,#82155,#82156,#82157,#82158,#82159,#82160,#82161,#82162,#82163,
#82164,#82165,#82166,#82167,#82168,#82169,#82170,#82171,#82172,#82173,#82174,
#82175,#82176,#82177,#82178,#82179,#82180,#82181,#82182,#82183,#82184,#82185,
#82186,#82187,#82188,#82189,#82190,#82191,#82192,#82193,#82194,#82195,#82196,
#82197,#82198,#82199,#82200,#82201,#82202,#82203,#82204,#82205,#82206,#82207,
#82208,#82209,#82210,#82211,#82212,#82213,#82214,#82215,#82216,#82217,#82218,
#82219,#82220,#82221,#82222,#82223,#82224,#82225,#82226,#82227,#82228,#82229,
#82230,#82231,#82232,#82233,#82234,#82235,#82236,#82237,#82238,#82239,#82240,
#82241,#82242,#82243,#82244,#82245,#82246,#82247,#82248,#82249,#82250,#82251,
#82252,#82253,#82254,#82255,#82256,#82257,#82258,#82259,#82260,#82261,#82262,
#82263,#82264,#82265,#82266,#82267,#82268,#82269,#82270,#82271,#82272,#82273,
#82274,#82275,#82276,#82277,#82278,#82279,#82280,#82281,#82282,#82283,#82284,
#82285,#82286,#82287,#82288,#82289,#82290),.UNSPECIFIED.,.F.,.F.,(4,2,2,
2,2,2,2,2,2,2,2,2,2,2,2,2,2,2,2,2,2,2,2,2,2,2,2,2,2,2,2,2,2,2,2,2,2,2,2,
2,2,2,2,2,2,2,2,2,2,2,2,2,2,2,2,2,2,2,2,2,2,2,2,2,2,2,2,2,2,2,2,2,2,2,2,
2,2,2,2,2,2,2,2,2,2,2,2,2,2,2,2,2,2,2,2,2,2,2,2,2,2,2,2,2,2,2,2,2,2,2,2,
2,2,2,2,2,2,2,2,2,2,2,2,2,2,2,2,2,2,2,2,4),(-2.59364855829229,-2.5805250390893,
-2.56278409515015,-2.55194824308276,-2.54864010448277,-2.54655336619433,
-2.54461707343816,-2.54210575134297,-2.53791439225231,-2.50842858115089,
-2.46731095672715,-2.45187633184749,-2.44646213612818,-2.44386337344784,
-2.44175675651997,-2.44054411539259,-2.44054100113675,-2.44053786796906,
-2.44053471576331,-2.440531544221,-2.44052835331933,-2.44052514307576,-2.44052191317927,
-2.44051866364419,-2.44051539419197,-2.4405121047115,-2.44050879501797,
-2.44050546497834,-2.44050212737287,-2.44049877521803,-2.44049540179566,
-2.44049199573067,-2.43946512739101,-2.43808765114628,-2.43523064398115,
-2.39912900337228,-2.36640698650285,-2.3439172832933,-2.33827312953013,
-2.33570353886459,-2.33376529201392,-2.33193799891083,-2.32939398900985,
-2.32273989542432,-2.26705329049152,-2.2429091628729,-2.23206353727476,
-2.22981813779165,-2.22856755012391,-2.22749556769191,-2.22613983566474,
-2.22399542335479,-2.21297854205454,-2.16170673761884,-2.13301944249611,
-2.12658814075178,-2.12387975860036,-2.12191804118312,-2.12012523265721,
-2.11725960484551,-2.11037157391679,-2.0573357314304,-2.03139671812569,
-2.02008110211527,-2.01780803637586,-2.01655144579858,-2.01548004876671,
-2.01413236059077,-2.01151118107485,-1.99547737576824,-1.99012770017464,
-1.97558900395009,-1.94269530041915,-1.92612790666373,-1.91581505838574,
-1.9125659036276,-1.91049232794615,-1.90855143342184,-1.90601001128875,
-1.90171466200994,-1.86659546915743,-1.81767306039634,-1.80791878915001,
-1.80574357444182,-1.80450832216617,-1.80343441801579,-1.80205660640985,
-1.79919831262477,-1.76327229888415,-1.73048510814842,-1.70789681308268,
-1.70223904576694,-1.69966679498596,-1.69772798077336,-1.69590121023253,
-1.69335962498487,-1.68672200580071,-1.63085911057923,-1.59803594974168,
-1.5944896466977,-1.5929853778273,-1.59189393470636,-1.59086651402607,-1.58911619747208,
-1.58433683795399,-1.5471606601068,-1.49689563116333,-1.49049358079696,
-1.48778997636317,-1.48582897324537,-1.48403492493844,-1.48116319051874,
-1.47423911293729,-1.42167206835065,-1.39539895020632,-1.38399813355596,
-1.381720029709,-1.38046226719308,-1.37939084842721,-1.37804437606064,-1.37542921060009,
-1.35950919466378,-1.35500709880457,-1.33444481736832,-1.28609239079606,
-1.27894364697813,-1.2760345128509,-1.27423358169825,-1.27227811319839,
-1.26960574452449,-1.26338653378267,-1.25991862954624),.UNSPECIFIED.);
#847=B_SPLINE_CURVE_WITH_KNOTS('',3,(#82296,#82297,#82298,#82299,#82300,
#82301,#82302,#82303,#82304,#82305,#82306,#82307,#82308,#82309,#82310,#82311,
#82312,#82313,#82314,#82315),.UNSPECIFIED.,.F.,.F.,(4,2,2,2,2,2,2,2,2,4),
(-0.0747504805022791,-0.0610229393326167,-0.0562870043262844,-0.0545435809193945,
-0.0535177049891406,-0.0524257922462895,-0.0509174391141034,-0.0492296202934677,
-0.0462824094859165,-0.000629118857166747),.UNSPECIFIED.);
#848=B_SPLINE_CURVE_WITH_KNOTS('',3,(#82316,#82317,#82318,#82319,#82320,
#82321,#82322,#82323,#82324,#82325,#82326,#82327,#82328,#82329,#82330,#82331,
#82332,#82333,#82334,#82335,#82336,#82337,#82338,#82339,#82340,#82341,#82342,
#82343,#82344,#82345,#82346,#82347,#82348,#82349,#82350,#82351,#82352,#82353,
#82354,#82355,#82356,#82357,#82358,#82359,#82360,#82361,#82362,#82363,#82364,
#82365,#82366,#82367,#82368,#82369,#82370,#82371,#82372,#82373,#82374,#82375,
#82376,#82377,#82378,#82379,#82380,#82381,#82382,#82383,#82384,#82385,#82386,
#82387,#82388,#82389,#82390,#82391,#82392,#82393,#82394,#82395,#82396,#82397,
#82398,#82399,#82400,#82401,#82402,#82403,#82404,#82405,#82406,#82407,#82408,
#82409,#82410,#82411,#82412,#82413,#82414,#82415,#82416,#82417,#82418,#82419,
#82420,#82421,#82422,#82423,#82424,#82425,#82426,#82427,#82428,#82429,#82430,
#82431,#82432,#82433,#82434,#82435,#82436,#82437,#82438,#82439,#82440,#82441,
#82442,#82443,#82444,#82445,#82446,#82447,#82448,#82449,#82450,#82451,#82452,
#82453,#82454,#82455,#82456,#82457,#82458,#82459,#82460,#82461,#82462,#82463,
#82464,#82465,#82466,#82467,#82468,#82469,#82470,#82471,#82472,#82473,#82474,
#82475,#82476,#82477,#82478,#82479,#82480,#82481,#82482,#82483,#82484,#82485,
#82486,#82487,#82488,#82489,#82490,#82491,#82492,#82493,#82494,#82495,#82496),
 .UNSPECIFIED.,.F.,.F.,(4,3,3,3,3,3,3,3,3,3,3,3,3,3,3,3,3,3,3,3,3,3,3,3,
3,3,3,3,3,3,3,3,3,3,3,3,3,3,3,3,3,3,3,3,3,3,3,3,3,3,3,3,3,3,3,3,3,3,3,3,
4),(108.12348663811,108.225421296431,108.327291076164,108.429131491865,
108.530978014042,108.632930880402,108.734945943836,108.837130903885,108.873173045844,
108.976567782892,109.079809065007,109.1829290304,109.285983598609,109.389006806967,
109.492032649639,109.595165416418,109.698354507828,109.801726501209,109.872009495806,
109.975404232854,110.078645514969,110.181765480361,110.28482004857,110.387843256928,
110.490869099601,110.594001866379,110.697190957789,110.80056295117,110.870845945768,
110.974240682816,111.077481964931,111.180601930324,111.283656498532,111.38667970689,
111.489705549562,111.59283831634,111.69602740775,111.799399401132,111.86968239573,
111.973077132778,112.076318414893,112.179438380285,112.282492948494,112.385516156852,
112.488541999524,112.591674766302,112.694863857712,112.798235851094,112.868518845692,
112.97191358274,113.075154864855,113.178274830248,113.281329398457,113.384352606815,
113.487378449488,113.590511216266,113.693700307676,113.797072301057,113.867355295654,
113.974272639427,114.057240355702),.UNSPECIFIED.);
#849=B_SPLINE_CURVE_WITH_KNOTS('',3,(#82498,#82499,#82500,#82501,#82502,
#82503,#82504,#82505,#82506,#82507,#82508,#82509,#82510,#82511,#82512,#82513,
#82514,#82515,#82516,#82517,#82518,#82519,#82520,#82521,#82522,#82523,#82524,
#82525,#82526,#82527,#82528,#82529,#82530,#82531,#82532,#82533,#82534,#82535,
#82536,#82537,#82538,#82539,#82540,#82541,#82542,#82543,#82544,#82545,#82546,
#82547,#82548,#82549,#82550,#82551,#82552,#82553,#82554,#82555,#82556,#82557,
#82558,#82559,#82560,#82561,#82562,#82563,#82564,#82565,#82566,#82567,#82568,
#82569,#82570,#82571,#82572,#82573,#82574,#82575,#82576,#82577,#82578,#82579,
#82580,#82581,#82582,#82583,#82584,#82585,#82586,#82587,#82588,#82589,#82590,
#82591,#82592,#82593,#82594,#82595,#82596,#82597,#82598,#82599,#82600,#82601,
#82602,#82603,#82604,#82605,#82606,#82607,#82608,#82609,#82610,#82611,#82612,
#82613,#82614,#82615,#82616,#82617,#82618,#82619,#82620,#82621,#82622,#82623,
#82624,#82625,#82626,#82627,#82628,#82629,#82630,#82631,#82632,#82633,#82634,
#82635,#82636,#82637,#82638,#82639,#82640,#82641,#82642,#82643,#82644,#82645,
#82646,#82647,#82648,#82649,#82650,#82651,#82652,#82653,#82654,#82655,#82656,
#82657,#82658,#82659,#82660,#82661,#82662,#82663,#82664,#82665,#82666,#82667,
#82668,#82669,#82670,#82671,#82672,#82673,#82674,#82675,#82676,#82677,#82678,
#82679,#82680,#82681,#82682,#82683,#82684,#82685,#82686,#82687,#82688,#82689,
#82690,#82691,#82692,#82693,#82694,#82695,#82696,#82697,#82698,#82699,#82700,
#82701,#82702,#82703,#82704,#82705,#82706,#82707,#82708,#82709),
 .UNSPECIFIED.,.F.,.F.,(4,2,2,2,2,2,2,2,2,2,2,2,2,2,2,2,2,2,2,2,2,2,2,2,
2,2,2,2,2,2,2,2,2,2,2,2,2,2,2,2,2,2,2,2,2,2,2,2,2,2,2,2,2,2,2,2,2,2,2,2,
2,2,2,2,2,2,2,2,2,2,2,2,2,2,2,2,2,2,2,2,2,2,2,2,2,2,2,2,2,2,2,2,2,2,2,2,
2,2,2,2,2,2,2,2,2,4),(-1.25991862954624,-1.23645521925533,-1.19593125822682,
-1.17294040471037,-1.17008513560625,-1.16870790614013,-1.16763404066988,
-1.16639837265882,-1.16422131132843,-1.15444067563811,-1.10551390453343,
-1.07038842872259,-1.06609282550099,-1.06355136321527,-1.06161049049882,
-1.05953698808853,-1.05628805127453,-1.04597667964511,-1.02941471206419,
-0.996553805928168,-0.982812168797365,-0.975961407222502,-0.975646420836586,
-0.970049533759383,-0.960061038061395,-0.957983607580622,-0.956648423118684,
-0.955577779236245,-0.954311322888828,-0.951992600776219,-0.939846099323988,
-0.88673354569945,-0.858174934537224,-0.854013049428049,-0.85151072086313,
-0.849576244313483,-0.847486387470819,-0.844162406496959,-0.833175585406915,
-0.815089360683986,-0.765144238560623,-0.748663330845422,-0.746024894072714,
-0.744673561711632,-0.743602000668175,-0.742348381533631,-0.740088675562478,
-0.729000855570218,-0.703939740295079,-0.649591388671133,-0.64280991145098,
-0.639962033145629,-0.638172545032308,-0.636208169548954,-0.633484504793157,
-0.626961278490919,-0.597498020898061,-0.552845290504222,-0.536651814362358,
-0.534024869022705,-0.532676044821793,-0.531604703459345,-0.530349293969498,
-0.528081183446334,-0.516848145105593,-0.491226590976862,-0.437702094390137,
-0.43085143562835,-0.427992189719632,-0.426200712641789,-0.424238313712536,
-0.421525052967838,-0.415063422307978,-0.36106306295883,-0.324938440896721,
-0.322081711649332,-0.320704373514572,-0.319630703165592,-0.318395575619336,
-0.316220222184403,-0.306459759801705,-0.257528429502025,-0.222411501761677,
-0.217733600619659,-0.215348296429087,-0.21348532827958,-0.211693434578673,
-0.208570626975831,-0.199301969640913,-0.184975038790322,-0.124596350285011,
-0.112277586646131,-0.110058294587506,-0.108679938431036,-0.107606156828923,
-0.106371671010484,-0.10419928597395,-0.0944824056770145,-0.0455133626512183,
-0.0267278933747515,-0.0187639939523813,-0.00802108700685602,-0.00466632877118399,
-0.00258130087386857,-0.00128118378991342,-0.000628942634120881),
 .UNSPECIFIED.);
#850=B_SPLINE_CURVE_WITH_KNOTS('',3,(#82710,#82711,#82712,#82713,#82714,
#82715,#82716,#82717,#82718,#82719,#82720,#82721,#82722),.UNSPECIFIED.,
 .F.,.F.,(4,3,3,3,4),(-104.372003947921,-104.263735348689,-104.155311094115,
-104.04663122551,-104.0225253952),.UNSPECIFIED.);
#851=B_SPLINE_CURVE_WITH_KNOTS('',3,(#82727,#82728,#82729,#82730,#82731,
#82732,#82733,#82734,#82735,#82736,#82737,#82738,#82739,#82740,#82741,#82742,
#82743,#82744,#82745,#82746,#82747,#82748,#82749,#82750,#82751,#82752,#82753,
#82754,#82755,#82756,#82757,#82758,#82759,#82760,#82761,#82762,#82763,#82764,
#82765,#82766,#82767,#82768,#82769,#82770,#82771,#82772,#82773,#82774,#82775,
#82776,#82777,#82778,#82779,#82780,#82781,#82782,#82783,#82784,#82785,#82786,
#82787,#82788,#82789,#82790,#82791,#82792,#82793,#82794,#82795,#82796,#82797,
#82798,#82799,#82800,#82801,#82802,#82803,#82804,#82805,#82806,#82807,#82808,
#82809,#82810,#82811,#82812,#82813,#82814,#82815,#82816,#82817,#82818,#82819,
#82820,#82821,#82822,#82823,#82824,#82825,#82826,#82827,#82828,#82829,#82830,
#82831,#82832,#82833,#82834,#82835,#82836,#82837,#82838,#82839,#82840,#82841,
#82842,#82843,#82844,#82845,#82846,#82847,#82848,#82849,#82850,#82851,#82852,
#82853,#82854,#82855,#82856,#82857,#82858,#82859,#82860,#82861,#82862,#82863,
#82864,#82865,#82866,#82867,#82868,#82869,#82870,#82871,#82872,#82873,#82874,
#82875,#82876,#82877,#82878,#82879,#82880,#82881,#82882,#82883,#82884,#82885,
#82886,#82887,#82888,#82889,#82890,#82891,#82892,#82893,#82894,#82895,#82896,
#82897,#82898,#82899,#82900,#82901,#82902,#82903,#82904,#82905,#82906,#82907,
#82908,#82909,#82910,#82911,#82912,#82913,#82914,#82915,#82916,#82917,#82918,
#82919,#82920,#82921,#82922,#82923,#82924,#82925,#82926,#82927,#82928,#82929,
#82930,#82931,#82932,#82933,#82934,#82935,#82936,#82937,#82938,#82939,#82940,
#82941,#82942,#82943,#82944,#82945,#82946),.UNSPECIFIED.,.F.,.F.,(4,2,2,
2,2,2,2,2,2,2,2,2,2,2,2,2,2,2,2,2,2,2,2,2,2,2,2,2,2,2,2,2,2,2,2,2,2,2,2,
2,2,2,2,2,2,2,2,2,2,2,2,2,2,2,2,2,2,2,2,2,2,2,2,2,2,2,2,2,2,2,2,2,2,2,2,
2,2,2,2,2,2,2,2,2,2,2,2,2,2,2,2,2,2,2,2,2,2,2,2,2,2,2,2,2,2,2,2,2,2,4),
(-1.40835487586409,-1.37307254728489,-1.33396207527971,-1.33297747199585,
-1.32826978968844,-1.32653031595748,-1.32550498997712,-1.32441215896202,
-1.32290008464717,-1.31930842896567,-1.2801659607581,-1.23134370594005,
-1.22421241397689,-1.22130615321221,-1.21950571385886,-1.21754976278718,
-1.21487490376253,-1.20864154415778,-1.18159616220365,-1.14087028279378,
-1.1182087231562,-1.11535576454838,-1.1139789642684,-1.11290511105388,-1.11166909292598,
-1.10949054261241,-1.09968874450466,-1.05077807375701,-1.01565732978512,
-1.01136167371651,-1.00882015692626,-1.00687922919932,-1.00480565503874,
-1.0015565786924,-0.99124453560085,-0.974681271831154,-0.941818715289484,
-0.928012375820401,-0.921312578881244,-0.905865009656025,-0.903497106721849,
-0.902089528389204,-0.901009372704753,-0.899805921533892,-0.897774110450924,
-0.889883781872256,-0.875166301535708,-0.846103477790437,-0.80369816067887,
-0.799404689283116,-0.796863862784888,-0.794923115277172,-0.792849397165536,
-0.789599392462951,-0.779278473780594,-0.762695310525479,-0.729817092444805,
-0.714521678298897,-0.709793778042114,-0.693941561463135,-0.691328748944117,
-0.689982891872275,-0.688911647877477,-0.687653730721892,-0.685374419074443,
-0.673948878376576,-0.647572475905596,-0.595122290963193,-0.588188791751799,
-0.58531574748797,-0.583521640495918,-0.581561187945153,-0.578859458774007,
-0.572467088305548,-0.526046672481506,-0.484947948273069,-0.480263096992574,
-0.478527315905961,-0.477502865242331,-0.476409860876519,-0.474895739295401,
-0.471290874706858,-0.432949787507504,-0.383317382558082,-0.376221663602101,
-0.373321734996011,-0.371522741093519,-0.369566399214206,-0.366887466226095,
-0.360806593162104,-0.352445785423339,-0.301551359242862,-0.270313240909897,
-0.267401273694885,-0.26601309675877,-0.26493828099778,-0.26371001605091,
-0.261566046985676,-0.252414963091736,-0.20366641682457,-0.167704289702535,
-0.162982355725928,-0.160559557235303,-0.15864067571755,-0.156487801785095,
-0.15425804633715,-0.146612093118065,-0.121083042999811,-0.100337614673059,
-0.0747504805022791),.UNSPECIFIED.);
#852=B_SPLINE_CURVE_WITH_KNOTS('',3,(#82948,#82949,#82950,#82951,#82952,
#82953,#82954,#82955,#82956,#82957,#82958,#82959,#82960,#82961,#82962,#82963,
#82964,#82965,#82966,#82967,#82968,#82969,#82970,#82971,#82972,#82973,#82974,
#82975,#82976,#82977,#82978,#82979,#82980,#82981,#82982,#82983,#82984,#82985,
#82986,#82987,#82988,#82989,#82990,#82991,#82992,#82993,#82994,#82995,#82996,
#82997,#82998,#82999,#83000,#83001,#83002,#83003,#83004,#83005,#83006,#83007,
#83008,#83009,#83010,#83011,#83012,#83013,#83014,#83015,#83016,#83017,#83018,
#83019,#83020,#83021,#83022,#83023,#83024,#83025,#83026,#83027,#83028,#83029,
#83030,#83031,#83032,#83033,#83034,#83035,#83036,#83037,#83038,#83039,#83040,
#83041,#83042,#83043,#83044,#83045,#83046,#83047,#83048,#83049,#83050,#83051,
#83052,#83053,#83054,#83055,#83056,#83057,#83058,#83059,#83060,#83061,#83062,
#83063,#83064,#83065,#83066,#83067,#83068,#83069,#83070,#83071,#83072,#83073,
#83074,#83075,#83076,#83077,#83078,#83079,#83080,#83081,#83082,#83083,#83084,
#83085,#83086,#83087,#83088,#83089,#83090,#83091,#83092,#83093,#83094,#83095,
#83096,#83097,#83098,#83099,#83100,#83101,#83102,#83103,#83104,#83105,#83106,
#83107,#83108,#83109,#83110,#83111,#83112,#83113,#83114,#83115,#83116,#83117,
#83118,#83119,#83120,#83121,#83122,#83123,#83124,#83125,#83126,#83127,#83128),
 .UNSPECIFIED.,.F.,.F.,(4,3,3,3,3,3,3,3,3,3,3,3,3,3,3,3,3,3,3,3,3,3,3,3,
3,3,3,3,3,3,3,3,3,3,3,3,3,3,3,3,3,3,3,3,3,3,3,3,3,3,3,3,3,3,3,3,3,3,3,3,
4),(-104.0225253952,-103.913514251962,-103.878990796035,-103.775596058987,
-103.672354776872,-103.569234811479,-103.46618024327,-103.363157034912,
-103.26013119224,-103.156998425461,-103.053809334052,-102.95043734067,-102.880154346073,
-102.776759609025,-102.67351832691,-102.570398361518,-102.467343793309,
-102.364320584951,-102.261294742279,-102.1581619755,-102.054972884091,-101.951600890709,
-101.881317896111,-101.777923159063,-101.674681876948,-101.571561911556,
-101.468507343347,-101.365484134989,-101.262458292316,-101.159325525538,
-101.056136434129,-100.952764440747,-100.882481446149,-100.779086709101,
-100.675845426986,-100.572725461594,-100.469670893385,-100.366647685027,
-100.263621842355,-100.160489075577,-100.057299984167,-99.9539279907856,
-99.8836449961874,-99.7802502591395,-99.6770089770246,-99.5738890116323,
-99.4708344434235,-99.3678112350658,-99.2647853923932,-99.1616526256151,
-99.0584635342054,-98.9550915408238,-98.8848085462256,-98.7829332776308,
-98.6811932844012,-98.5795525376359,-98.4779751499172,-98.3763829554482,
-98.2747883682234,-98.1730805291731,-98.0888188327624),.UNSPECIFIED.);
#853=B_SPLINE_CURVE_WITH_KNOTS('',3,(#83129,#83130,#83131,#83132,#83133),
 .UNSPECIFIED.,.F.,.F.,(4,1,4),(-98.0888186411165,-97.8859720962637,-97.7379482607811),
 .UNSPECIFIED.);
#854=B_SPLINE_CURVE_WITH_KNOTS('',3,(#83139,#83140,#83141,#83142,#83143,
#83144,#83145,#83146,#83147,#83148,#83149,#83150,#83151,#83152,#83153,#83154,
#83155,#83156,#83157,#83158,#83159,#83160),.UNSPECIFIED.,.F.,.F.,(4,2,2,
2,2,2,2,2,2,2,4),(-0.0750517120858235,-0.0634020277063106,-0.0604359040533312,
-0.0436144771006821,-0.039999553992989,-0.0376361162171469,-0.035722518033051,
-0.0339209987346118,-0.0317709121351228,-0.0286342834260186,-0.000628475014750037),
 .UNSPECIFIED.);
#855=B_SPLINE_CURVE_WITH_KNOTS('',3,(#83161,#83162,#83163,#83164,#83165,
#83166,#83167,#83168,#83169,#83170,#83171,#83172,#83173,#83174,#83175,#83176,
#83177,#83178,#83179,#83180,#83181,#83182,#83183,#83184,#83185,#83186,#83187,
#83188,#83189,#83190,#83191,#83192,#83193,#83194,#83195,#83196,#83197,#83198,
#83199,#83200,#83201,#83202,#83203,#83204,#83205,#83206,#83207,#83208,#83209,
#83210,#83211,#83212,#83213,#83214,#83215,#83216,#83217,#83218,#83219,#83220,
#83221,#83222,#83223,#83224,#83225,#83226,#83227,#83228,#83229,#83230,#83231,
#83232,#83233,#83234,#83235,#83236,#83237,#83238,#83239,#83240,#83241,#83242,
#83243,#83244,#83245,#83246,#83247,#83248,#83249,#83250,#83251,#83252,#83253,
#83254,#83255,#83256,#83257,#83258,#83259,#83260,#83261,#83262,#83263,#83264,
#83265,#83266,#83267,#83268,#83269,#83270,#83271,#83272,#83273,#83274,#83275,
#83276,#83277,#83278,#83279,#83280,#83281,#83282,#83283,#83284,#83285,#83286,
#83287,#83288,#83289,#83290,#83291,#83292,#83293,#83294,#83295,#83296,#83297,
#83298,#83299,#83300,#83301,#83302,#83303,#83304,#83305,#83306,#83307,#83308,
#83309,#83310,#83311,#83312,#83313,#83314,#83315,#83316,#83317,#83318,#83319,
#83320,#83321,#83322,#83323,#83324,#83325,#83326,#83327,#83328,#83329,#83330,
#83331,#83332,#83333,#83334,#83335,#83336,#83337,#83338,#83339,#83340,#83341,
#83342,#83343,#83344,#83345,#83346,#83347,#83348,#83349,#83350,#83351,#83352,
#83353,#83354,#83355,#83356,#83357,#83358,#83359,#83360,#83361,#83362,#83363,
#83364,#83365,#83366,#83367,#83368,#83369,#83370,#83371,#83372,#83373,#83374,
#83375,#83376,#83377,#83378,#83379,#83380,#83381,#83382,#83383,#83384,#83385,
#83386,#83387,#83388),.UNSPECIFIED.,.F.,.F.,(4,2,2,2,2,2,2,2,2,2,2,2,2,
2,2,2,2,2,2,2,2,2,2,2,2,2,2,2,2,2,2,2,2,2,2,2,2,2,2,2,2,2,2,2,2,2,2,2,2,
2,2,2,2,2,2,2,2,2,2,2,2,2,2,2,2,2,2,2,2,2,2,2,2,2,2,2,2,2,2,2,2,2,2,2,2,
2,2,2,2,2,2,2,2,2,2,2,2,2,2,2,2,2,2,2,2,2,2,2,2,2,2,2,2,4),(-2.66755899473746,
-2.62215929206862,-2.60376763862076,-2.5999431884763,-2.59839239054727,
-2.59729261961806,-2.59627719827611,-2.59458840791125,-2.59020935864258,
-2.54255191463499,-2.52187306040523,-2.50663692968774,-2.50017771203682,
-2.49523147431694,-2.49279720522105,-2.49087093917742,-2.48901472241989,
-2.48581672251949,-2.47680447926813,-2.47485034215988,-2.42390161802967,
-2.40007108825067,-2.38930996178348,-2.38706958386249,-2.38582003686064,
-2.38474786226029,-2.38339049507671,-2.38124088461108,-2.37014161526378,
-2.31886838062625,-2.29025511326364,-2.28383242204779,-2.28112537803136,
-2.27916379858666,-2.2773705440319,-2.27450295806638,-2.26760376844898,
-2.21470811541589,-2.18866667499769,-2.17732466173618,-2.17504996632096,
-2.17379296755879,-2.17272152144797,-2.17137415200738,-2.16875471082167,
-2.15275264889233,-2.14725920587629,-2.13282348362516,-2.09992862296215,
-2.08336147074205,-2.07304853117276,-2.06979921902794,-2.06772551199458,
-2.06578447280967,-2.06324282992762,-2.05894703732975,-2.02381486464612,
-1.9748564687468,-1.96513987893544,-1.96296714396137,-1.96173238309113,
-1.96065831835236,-1.95927953159331,-1.95641656331132,-1.93305391234053,
-1.93132070759586,-1.89233867299868,-1.86585625168617,-1.85969299423361,
-1.8570302462541,-1.85507639146389,-1.85327314106256,-1.85035175567705,
-1.8431305892157,-1.7986072322274,-1.78473478757679,-1.7632763083891,-1.75318372698607,
-1.7509856781239,-1.74974535666655,-1.74867205554724,-1.74730153252362,
-1.74510873485366,-1.73333953949705,-1.72962684187481,-1.72236556462697,
-1.67901009008891,-1.66042268288153,-1.64921987459312,-1.64587221244242,
-1.64377679842947,-1.64184352623267,-1.63935164542618,-1.63522643190573,
-1.60809056197531,-1.56616637123774,-1.54954736546721,-1.54098478408796,
-1.53889723340756,-1.53768129444079,-1.53660390223726,-1.53521797734135,
-1.53292427092712,-1.51915032403464,-1.50784479514911,-1.46844818120244,
-1.44187537797694,-1.43570086564228,-1.43303615732892,-1.43108195640327,
-1.42927915351008,-1.42636020670049,-1.41915354266117,-1.40835487586409),
 .UNSPECIFIED.);
#856=B_SPLINE_CURVE_WITH_KNOTS('',3,(#83390,#83391,#83392,#83393,#83394,
#83395,#83396,#83397,#83398,#83399),.UNSPECIFIED.,.F.,.F.,(4,1,1,1,1,1,
1,4),(-97.7379482607811,-96.8871356463018,-95.88829919634,-94.8894627463781,
-93.8906262964162,-92.8917898464543,-91.8929533964925,-91.8056333339369),
 .UNSPECIFIED.);
#857=B_SPLINE_CURVE_WITH_KNOTS('',3,(#83400,#83401,#83402,#83403,#83404,
#83405,#83406,#83407),.UNSPECIFIED.,.F.,.F.,(4,2,2,4),(-2.66776547017807,
-2.61548873906283,-2.59714121576297,-2.59332753526453),.UNSPECIFIED.);
#858=B_SPLINE_CURVE_WITH_KNOTS('',3,(#83412,#83413,#83414,#83415,#83416,
#83417,#83418,#83419,#83420,#83421,#83422,#83423,#83424,#83425,#83426,#83427,
#83428,#83429,#83430,#83431,#83432,#83433,#83434,#83435,#83436,#83437,#83438,
#83439,#83440,#83441,#83442,#83443,#83444,#83445,#83446,#83447,#83448,#83449,
#83450,#83451,#83452,#83453,#83454,#83455,#83456,#83457,#83458,#83459,#83460,
#83461,#83462,#83463,#83464,#83465,#83466,#83467,#83468,#83469,#83470,#83471,
#83472,#83473,#83474,#83475,#83476,#83477,#83478,#83479,#83480,#83481,#83482,
#83483,#83484,#83485,#83486,#83487,#83488,#83489,#83490,#83491,#83492,#83493,
#83494,#83495,#83496,#83497,#83498,#83499,#83500,#83501,#83502,#83503,#83504,
#83505,#83506,#83507,#83508,#83509,#83510,#83511,#83512,#83513,#83514,#83515,
#83516,#83517,#83518,#83519,#83520,#83521,#83522,#83523,#83524,#83525,#83526,
#83527,#83528,#83529,#83530,#83531,#83532,#83533,#83534,#83535,#83536,#83537,
#83538,#83539,#83540,#83541,#83542,#83543,#83544,#83545,#83546,#83547,#83548,
#83549,#83550,#83551,#83552,#83553,#83554,#83555,#83556,#83557,#83558,#83559,
#83560,#83561,#83562,#83563,#83564,#83565,#83566,#83567,#83568,#83569,#83570,
#83571,#83572,#83573,#83574,#83575,#83576,#83577,#83578,#83579,#83580,#83581,
#83582,#83583,#83584,#83585,#83586,#83587,#83588,#83589,#83590,#83591,#83592,
#83593,#83594,#83595,#83596,#83597,#83598,#83599,#83600,#83601,#83602,#83603,
#83604,#83605,#83606,#83607,#83608,#83609,#83610,#83611,#83612,#83613,#83614,
#83615,#83616,#83617,#83618,#83619,#83620,#83621,#83622,#83623,#83624,#83625,
#83626,#83627),.UNSPECIFIED.,.F.,.F.,(4,2,2,2,2,2,2,2,2,2,2,2,2,2,2,2,2,
2,2,2,2,2,2,2,2,2,2,2,2,2,2,2,2,2,2,2,2,2,2,2,2,2,2,2,2,2,2,2,2,2,2,2,2,
2,2,2,2,2,2,2,2,2,2,2,2,2,2,2,2,2,2,2,2,2,2,2,2,2,2,2,2,2,2,2,2,2,2,2,2,
2,2,2,2,2,2,2,2,2,2,2,2,2,2,2,2,2,2,4),(-1.40856932496091,-1.37753543614885,
-1.33437665872906,-1.31573900030673,-1.31200628105946,-1.30960637168692,
-1.30768960262075,-1.30552204984672,-1.30184745235688,-1.28708453682466,
-1.25915948466983,-1.20936256225145,-1.20515960863439,-1.20349963378921,
-1.20248984116764,-1.20138559868045,-1.19981061234075,-1.19583470689363,
-1.17602204218857,-1.14710923645267,-1.10479029204916,-1.10049517751206,
-1.09795393697261,-1.09601319479084,-1.09393979420465,-1.09069093835791,
-1.0803791611172,-1.06381591158189,-1.03095512643785,-1.01703005374874,
-1.01060148456783,-0.995017911007972,-0.992416338826959,-0.991072945979837,
-0.99000190330379,-0.988742175491111,-0.986454345015537,-0.974876083362637,
-0.947885913239259,-0.896303645033721,-0.889312818094277,-0.886430389790255,
-0.884634631904765,-0.882675737586507,-0.87998228355691,-0.873638165877028,
-0.84567906161521,-0.799179368654382,-0.78306850279216,-0.780441838941246,
-0.779093059198093,-0.778021700664243,-0.776766210287376,-0.774497799671683,
-0.763260155420916,-0.737621065911922,-0.684120162797436,-0.677267357996391,
-0.674407723119932,-0.672616149473194,-0.670653763373107,-0.667940738500816,
-0.661480709013897,-0.607538476784662,-0.571348324193975,-0.568493619247127,
-0.567116661797381,-0.566043008375619,-0.564807584295391,-0.562630952565983,
-0.55285224398874,-0.503935138393193,-0.468823866111901,-0.464525059002833,
-0.46198292431333,-0.460042242078175,-0.457969625370875,-0.454723499923555,
-0.44443303529533,-0.42791602817502,-0.371222226226515,-0.35872312561734,
-0.356494177284,-0.355112912291896,-0.354038852235543,-0.35280628338611,
-0.350642590999413,-0.341051024996288,-0.291975395867075,-0.256812360397262,
-0.252513848564328,-0.249971815410669,-0.248031168632203,-0.246240519509763,
-0.243303174701344,-0.235328940876774,-0.223525728322634,-0.190999542299758,
-0.150078407933012,-0.145387637920967,-0.143651113228751,-0.142626620497403,
-0.141533908642349,-0.140020743409252,-0.136420703033798,-0.0985274293922583,
-0.075735778076427,-0.0750517120858235),.UNSPECIFIED.);
#859=B_SPLINE_CURVE_WITH_KNOTS('',3,(#83628,#83629,#83630,#83631,#83632,
#83633,#83634,#83635,#83636,#83637,#83638,#83639,#83640,#83641,#83642,#83643,
#83644,#83645,#83646,#83647,#83648,#83649,#83650,#83651,#83652,#83653,#83654,
#83655,#83656,#83657,#83658,#83659,#83660,#83661,#83662,#83663,#83664,#83665,
#83666,#83667,#83668,#83669,#83670,#83671,#83672,#83673,#83674,#83675,#83676,
#83677,#83678,#83679,#83680,#83681,#83682,#83683,#83684,#83685,#83686,#83687,
#83688,#83689,#83690,#83691,#83692,#83693,#83694,#83695,#83696,#83697,#83698,
#83699,#83700,#83701,#83702,#83703,#83704,#83705,#83706,#83707,#83708,#83709,
#83710,#83711,#83712,#83713,#83714,#83715,#83716,#83717,#83718,#83719,#83720,
#83721,#83722,#83723,#83724,#83725,#83726,#83727,#83728,#83729,#83730,#83731,
#83732,#83733,#83734,#83735,#83736,#83737,#83738,#83739,#83740,#83741,#83742,
#83743,#83744,#83745,#83746,#83747,#83748,#83749,#83750,#83751,#83752,#83753,
#83754,#83755,#83756,#83757,#83758,#83759,#83760,#83761,#83762,#83763,#83764,
#83765,#83766,#83767,#83768,#83769,#83770,#83771,#83772,#83773,#83774,#83775,
#83776,#83777,#83778,#83779,#83780,#83781,#83782,#83783,#83784,#83785,#83786,
#83787,#83788,#83789,#83790,#83791,#83792,#83793,#83794,#83795,#83796,#83797,
#83798,#83799,#83800,#83801,#83802,#83803,#83804,#83805,#83806,#83807,#83808,
#83809,#83810,#83811,#83812,#83813,#83814,#83815,#83816,#83817,#83818,#83819,
#83820,#83821,#83822,#83823,#83824,#83825,#83826,#83827,#83828,#83829,#83830,
#83831,#83832,#83833,#83834,#83835,#83836,#83837,#83838,#83839,#83840,#83841,
#83842,#83843,#83844,#83845,#83846,#83847,#83848,#83849,#83850,#83851,#83852,
#83853,#83854,#83855,#83856,#83857,#83858,#83859,#83860,#83861,#83862,#83863,
#83864,#83865,#83866,#83867,#83868,#83869,#83870,#83871,#83872,#83873,#83874,
#83875,#83876,#83877,#83878,#83879,#83880,#83881,#83882,#83883,#83884,#83885,
#83886,#83887,#83888,#83889,#83890,#83891,#83892,#83893,#83894,#83895,#83896,
#83897,#83898,#83899),.UNSPECIFIED.,.F.,.F.,(4,2,2,2,2,2,2,2,2,2,2,2,2,
2,2,2,2,2,2,2,2,2,2,2,2,2,2,2,2,2,2,2,2,2,2,2,2,2,2,2,2,2,2,2,2,2,2,2,2,
2,2,2,2,2,2,2,2,2,2,2,2,2,2,2,2,2,2,2,2,2,2,2,2,2,2,2,2,2,2,2,2,2,2,2,2,
2,2,2,2,2,2,2,2,2,2,2,2,2,2,2,2,2,2,2,2,2,2,2,2,2,2,2,2,2,2,2,2,2,2,2,2,
2,2,2,2,2,2,2,2,2,2,2,2,2,2,4),(-2.59332753526453,-2.58604272140604,-2.58270693816439,
-2.5806146222872,-2.57868125454311,-2.57618511262564,-2.57204387356041,
-2.54424358251689,-2.5020144615368,-2.48613393383352,-2.48061668953957,
-2.47798287951046,-2.47587129426084,-2.4746488810723,-2.47464532648293,
-2.47464175810497,-2.47463817596284,-2.47463457982111,-2.47463071128106,
-2.47462677538248,-2.47462277065502,-2.47461869567567,-2.47461454885354,
-2.47461032863313,-2.47460603362575,-2.47460166216701,-2.47459721247322,
-2.47459268293298,-2.47458807165657,-2.4745833768235,-2.47457859663824,
-2.47457372915854,-2.47354854823527,-2.47217419824068,-2.46933247020453,
-2.4324211405773,-2.4008118662466,-2.3842491625337,-2.37393905210402,-2.37069066332947,
-2.36861755328192,-2.36667707829501,-2.36413618198753,-2.35984166871282,
-2.32472230221683,-2.27578630969899,-2.26606285126058,-2.26389008000958,
-2.26265553054566,-2.26158179848073,-2.26020363344686,-2.25734262753862,
-2.23404573343154,-2.22174771777207,-2.18886060901367,-2.17229758466922,
-2.16198714947012,-2.15873859178091,-2.15666535793356,-2.15472475582895,
-2.15218367685695,-2.14788881851329,-2.11276178546471,-2.06380576078331,
-2.05410161024298,-2.05193007164809,-2.05069574502374,-2.04962190040874,
-2.04824318995788,-2.04537966827013,-2.00941117954529,-1.95514326922882,
-1.94873698692295,-1.94603301867958,-1.94407227005156,-1.94227881183604,
-1.93940880109859,-1.93249290780156,-1.87984542234686,-1.85364247756406,
-1.84226041877107,-1.83998373772502,-1.83872645003023,-1.83765524751299,
-1.8363088075184,-1.83369300264878,-1.81775261430373,-1.81207173027847,
-1.76791434511493,-1.74936380567546,-1.73817766206365,-1.73483233658984,
-1.73273779450941,-1.7308049254761,-1.7283130033667,-1.7241865081184,-1.69696510608635,
-1.65487193717336,-1.63845567834265,-1.62996335994081,-1.62788176391822,
-1.62666734280498,-1.62558997700872,-1.62420238242251,-1.62190237600633,
-1.60798933621419,-1.60636834810441,-1.60500975276388,-1.59754427077589,
-1.58574630989523,-1.55288290017062,-1.53634916157398,-1.52605188088118,
-1.52280476471924,-1.52073180074514,-1.5187909944066,-1.51624898862964,
-1.51195108538526,-1.47659208651493,-1.42743051949544,-1.4181151048594,
-1.4159709222603,-1.41474259569936,-1.41366777097751,-1.41227963111758,
-1.40936793066897,-1.37753518108014,-1.33437642004894,-1.31573877104263,
-1.31200605425729,-1.30960614657258,-1.30768937892502,-1.30552182783276,
-1.30184723338871,-1.28708433298769,-1.25997080151201),.UNSPECIFIED.);
#860=B_SPLINE_CURVE_WITH_KNOTS('',3,(#83905,#83906,#83907,#83908,#83909),
 .UNSPECIFIED.,.F.,.F.,(4,1,4),(82.6397394574315,82.9034253468356,82.9907454093913),
 .UNSPECIFIED.);
#861=B_SPLINE_CURVE_WITH_KNOTS('',3,(#83910,#83911,#83912,#83913,#83914,
#83915,#83916,#83917,#83918,#83919,#83920,#83921,#83922,#83923,#83924,#83925,
#83926,#83927,#83928,#83929,#83930,#83931,#83932,#83933,#83934,#83935,#83936,
#83937,#83938,#83939,#83940,#83941,#83942,#83943,#83944,#83945,#83946,#83947,
#83948,#83949,#83950,#83951,#83952,#83953,#83954,#83955,#83956,#83957,#83958,
#83959,#83960,#83961,#83962,#83963,#83964,#83965,#83966,#83967,#83968,#83969,
#83970,#83971,#83972,#83973,#83974,#83975,#83976,#83977,#83978,#83979,#83980,
#83981,#83982,#83983,#83984,#83985,#83986,#83987,#83988,#83989,#83990,#83991,
#83992,#83993,#83994,#83995,#83996,#83997,#83998,#83999,#84000,#84001,#84002,
#84003,#84004,#84005,#84006,#84007,#84008,#84009,#84010,#84011,#84012,#84013,
#84014,#84015,#84016,#84017,#84018,#84019,#84020,#84021,#84022,#84023,#84024,
#84025,#84026,#84027,#84028,#84029,#84030,#84031,#84032,#84033,#84034,#84035,
#84036,#84037,#84038,#84039,#84040,#84041,#84042,#84043,#84044,#84045,#84046,
#84047,#84048,#84049,#84050,#84051,#84052,#84053,#84054,#84055,#84056,#84057,
#84058,#84059,#84060,#84061,#84062,#84063,#84064,#84065,#84066,#84067,#84068,
#84069,#84070,#84071,#84072,#84073,#84074,#84075,#84076,#84077,#84078,#84079,
#84080,#84081,#84082,#84083,#84084,#84085,#84086,#84087,#84088,#84089,#84090,
#84091,#84092,#84093,#84094,#84095,#84096,#84097,#84098,#84099,#84100,#84101,
#84102,#84103,#84104,#84105,#84106,#84107,#84108,#84109,#84110,#84111,#84112,
#84113,#84114,#84115,#84116,#84117,#84118,#84119,#84120,#84121,#84122,#84123,
#84124,#84125,#84126,#84127,#84128,#84129,#84130,#84131,#84132,#84133,#84134,
#84135,#84136,#84137,#84138,#84139,#84140,#84141,#84142,#84143,#84144,#84145,
#84146,#84147,#84148,#84149,#84150,#84151,#84152,#84153,#84154,#84155,#84156,
#84157,#84158,#84159,#84160,#84161,#84162,#84163,#84164,#84165),
 .UNSPECIFIED.,.F.,.F.,(4,2,2,2,2,2,2,2,2,2,2,2,2,2,2,2,2,2,2,2,2,2,2,2,
2,2,2,2,2,2,2,2,2,2,2,2,2,2,2,2,2,2,2,2,2,2,2,2,2,2,2,2,2,2,2,2,2,2,2,2,
2,2,2,2,2,2,2,2,2,2,2,2,2,2,2,2,2,2,2,2,2,2,2,2,2,2,2,2,2,2,2,2,2,2,2,2,
2,2,2,2,2,2,2,2,2,2,2,2,2,2,2,2,2,2,2,2,2,2,2,2,2,2,2,2,2,2,2,4),(-2.66783332377647,
-2.61564214598672,-2.59723508098817,-2.58611069517746,-2.58277199335766,
-2.58067893953301,-2.57874563411728,-2.57625061549819,-2.57211350181238,
-2.54447923335572,-2.50218480438026,-2.48622223875291,-2.48068593668643,
-2.47804556179293,-2.47592965463349,-2.47470621549526,-2.47470267000306,
-2.47469911096232,-2.47469553816781,-2.47469195165705,-2.47468835133991,
-2.47468446315151,-2.47468050715029,-2.47467648191082,-2.47467238588093,
-2.47466821771319,-2.47466397579209,-2.47465965849242,-2.47465526417203,
-2.47465079116621,-2.47464623767288,-2.47464160202744,-2.47463688241049,
-2.47463207674742,-2.47360824688145,-2.47223647282876,-2.46940783145152,
-2.43186080881884,-2.40255942178994,-2.37839554315062,-2.37252897073714,
-2.36991916296777,-2.36797474773041,-2.36615912463568,-2.36365902174291,
-2.35727484377884,-2.29920250318749,-2.27659273967936,-2.26617046426924,
-2.2639514909605,-2.26270677441483,-2.26163431559197,-2.26027087279878,
-2.25748458055384,-2.23740819260861,-2.19455466466653,-2.16700963873722,
-2.16071622685985,-2.15803143271454,-2.1560740845448,-2.15427644663709,
-2.15138372890445,-2.14433095227195,-2.09387723167345,-2.05630415343087,
-2.05272440615339,-2.05121460198596,-2.05012238409171,-2.04909681596941,
-2.04735518562612,-2.04263149798945,-2.00238929811358,-1.95513209844072,
-1.94873720900797,-1.94603516014328,-1.94407474979468,-1.94228087443214,
-1.93940861073604,-1.93247909119843,-1.88001945152264,-1.85368423493556,
-1.84226877993537,-1.83999018882601,-1.83873248222893,-1.83766130778611,
-1.83631539250319,-1.83370204194143,-1.81782624216145,-1.81303239894487,
-1.76784553711486,-1.74934089879086,-1.73817446959149,-1.7348312422891,
-1.73273716392597,-1.73080414496727,-1.72831122132682,-1.72418131817348,
-1.69682711648576,-1.65453192776829,-1.63835940965027,-1.62995128134607,
-1.62787644307332,-1.62666352117122,-1.62558582731251,-1.62419566345088,
-1.6218869252826,-1.60779514032835,-1.60650289106458,-1.60500052111857,
-1.59754568222509,-1.58574671518815,-1.55288327876266,-1.53634952170758,
-1.52605223069659,-1.52280511182253,-1.52073214624075,-1.51879133848219,
-1.51624933096568,-1.5119514250411,-1.47659242780067,-1.42743081628971,
-1.41811539257215,-1.41597120822893,-1.41474288072132,-1.41366805520194,
-1.41227991434118,-1.40936821188941,-1.40856932496091),.UNSPECIFIED.);
#862=B_SPLINE_CURVE_WITH_KNOTS('',3,(#84167,#84168,#84169,#84170,#84171,
#84172,#84173,#84174,#84175,#84176,#84177,#84178,#84179,#84180,#84181,#84182,
#84183,#84184,#84185,#84186,#84187,#84188,#84189,#84190,#84191,#84192,#84193,
#84194,#84195,#84196,#84197,#84198,#84199,#84200,#84201,#84202,#84203,#84204,
#84205,#84206,#84207,#84208,#84209,#84210,#84211,#84212,#84213,#84214,#84215,
#84216,#84217,#84218,#84219,#84220,#84221,#84222,#84223,#84224,#84225,#84226,
#84227,#84228,#84229,#84230,#84231,#84232,#84233,#84234,#84235,#84236,#84237,
#84238,#84239,#84240,#84241,#84242,#84243,#84244,#84245,#84246,#84247,#84248,
#84249,#84250,#84251,#84252,#84253,#84254,#84255,#84256,#84257,#84258,#84259,
#84260,#84261,#84262,#84263,#84264,#84265,#84266,#84267,#84268,#84269,#84270,
#84271,#84272,#84273,#84274,#84275,#84276,#84277,#84278,#84279,#84280,#84281,
#84282,#84283,#84284,#84285,#84286,#84287,#84288,#84289,#84290,#84291,#84292,
#84293,#84294,#84295,#84296,#84297,#84298,#84299,#84300,#84301,#84302,#84303,
#84304,#84305,#84306,#84307,#84308,#84309,#84310,#84311,#84312,#84313,#84314,
#84315,#84316,#84317,#84318,#84319,#84320,#84321,#84322,#84323,#84324,#84325,
#84326,#84327,#84328,#84329,#84330,#84331,#84332,#84333,#84334,#84335,#84336,
#84337,#84338,#84339,#84340,#84341,#84342,#84343,#84344,#84345,#84346,#84347,
#84348,#84349,#84350,#84351,#84352,#84353,#84354,#84355,#84356,#84357,#84358,
#84359,#84360,#84361,#84362,#84363,#84364,#84365,#84366,#84367,#84368,#84369,
#84370,#84371,#84372,#84373,#84374,#84375,#84376,#84377,#84378,#84379,#84380,
#84381,#84382),.UNSPECIFIED.,.F.,.F.,(4,2,2,2,2,2,2,2,2,2,2,2,2,2,2,2,2,
2,2,2,2,2,2,2,2,2,2,2,2,2,2,2,2,2,2,2,2,2,2,2,2,2,2,2,2,2,2,2,2,2,2,2,2,
2,2,2,2,2,2,2,2,2,2,2,2,2,2,2,2,2,2,2,2,2,2,2,2,2,2,2,2,2,2,2,2,2,2,2,2,
2,2,2,2,2,2,2,2,2,2,2,2,2,2,2,2,2,2,4),(-1.25997080151201,-1.25915931516951,
-1.20936239081794,-1.20515944182619,-1.20349946847035,-1.20248967664927,
-1.20138543494635,-1.19981044958039,-1.19583454584559,-1.17602188455216,
-1.14710910079787,-1.10479018260538,-1.10049507090556,-1.09795383215206,
-1.09601309139939,-1.09393969240468,-1.09069083919058,-1.08037907156495,
-1.06381583893288,-1.03095507917741,-1.01703065887685,-1.01060068296542,
-0.995017815824003,-0.992416275187708,-0.991072889737169,-0.990001848249544,
-0.988742116367917,-0.986454264495089,-0.974875597907575,-0.947883774590537,
-0.896303860887372,-0.8893128934105,-0.886430443104705,-0.884634682141149,
-0.882675792949477,-0.879982361414452,-0.873638368776958,-0.845680281583233,
-0.799190527300124,-0.783069970251435,-0.78044247775776,-0.779093520367573,
-0.778022150678918,-0.776766797655267,-0.774499016245602,-0.76327220566548,
-0.737675201382725,-0.684113304354058,-0.677265455766238,-0.674406638539597,
-0.672615213852687,-0.670652697978992,-0.667938954844861,-0.661474646410106,
-0.607384724107681,-0.571356490359434,-0.568496370848481,-0.567118351271025,
-0.566044597040419,-0.564809877739583,-0.562636449235622,-0.552904502334806,
-0.503947924152347,-0.468806688720381,-0.464517287132083,-0.461977879737483,
-0.460037645928899,-0.457963923376715,-0.454712755279172,-0.444378370302155,
-0.427764255914947,-0.371064364763453,-0.358708582439002,-0.356487302632965,
-0.355108350939898,-0.354034517687593,-0.352800437326769,-0.350629874308427,
-0.34093930465962,-0.29194827702703,-0.256811872620156,-0.25251362990003,
-0.249971674950569,-0.248031041291889,-0.246240392883459,-0.243302951930731,
-0.235328044223839,-0.223523527455889,-0.190998694030786,-0.150078466355593,
-0.145387650131162,-0.143651118608479,-0.142626624664606,-0.141533913915671,
-0.14002075414421,-0.136420744922919,-0.0985306498520224,-0.0757357801641774,
-0.0634020321937908,-0.0604357376939238,-0.0436144584964585,-0.0399995456229471,
-0.0376361112330499,-0.0357225135970766,-0.0339209942593315,-0.0317709059834869,
-0.0286342728390913,-0.000628476974914811),.UNSPECIFIED.);
#863=B_SPLINE_CURVE_WITH_KNOTS('',3,(#84383,#84384,#84385,#84386,#84387,
#84388,#84389,#84390,#84391,#84392,#84393,#84394,#84395,#84396,#84397,#84398,
#84399,#84400),.UNSPECIFIED.,.F.,.F.,(4,2,2,2,2,2,2,2,4),(-2.6675682063545,
-2.62399424995869,-2.60401305473231,-2.60001889487262,-2.59844083514121,
-2.59733583662049,-2.59632642690663,-2.59466920107051,-2.59342127676457),
 .UNSPECIFIED.);
#864=B_SPLINE_CURVE_WITH_KNOTS('',3,(#84406,#84407,#84408,#84409,#84410,
#84411,#84412,#84413,#84414,#84415,#84416,#84417,#84418),.UNSPECIFIED.,
 .F.,.F.,(4,3,3,3,4),(76.3573194355999,76.4589087585747,76.5605127542266,
76.6622237698669,76.7075599105224),.UNSPECIFIED.);
#865=B_SPLINE_CURVE_WITH_KNOTS('',3,(#84419,#84420,#84421,#84422,#84423,
#84424,#84425,#84426,#84427,#84428),.UNSPECIFIED.,.F.,.F.,(4,1,1,1,1,1,
1,4),(76.7075601022117,76.9104066470643,77.9092430970262,78.9080795469881,
79.90691599695,80.9057524469119,81.9045888968737,82.6397394574315),
 .UNSPECIFIED.);
#866=B_SPLINE_CURVE_WITH_KNOTS('',3,(#84429,#84430,#84431,#84432,#84433,
#84434,#84435,#84436,#84437,#84438,#84439,#84440,#84441,#84442,#84443,#84444,
#84445,#84446,#84447,#84448,#84449,#84450,#84451,#84452,#84453,#84454,#84455,
#84456,#84457,#84458,#84459,#84460,#84461,#84462,#84463,#84464,#84465,#84466,
#84467,#84468,#84469,#84470,#84471,#84472,#84473,#84474,#84475,#84476,#84477,
#84478,#84479,#84480,#84481,#84482,#84483,#84484,#84485,#84486,#84487,#84488,
#84489,#84490,#84491,#84492,#84493,#84494,#84495,#84496,#84497,#84498,#84499,
#84500,#84501,#84502,#84503,#84504,#84505,#84506,#84507,#84508,#84509,#84510,
#84511,#84512,#84513,#84514,#84515,#84516,#84517,#84518,#84519,#84520,#84521,
#84522,#84523,#84524,#84525,#84526,#84527,#84528,#84529,#84530,#84531,#84532,
#84533,#84534,#84535,#84536,#84537,#84538,#84539,#84540,#84541,#84542,#84543,
#84544,#84545,#84546,#84547,#84548,#84549,#84550,#84551,#84552,#84553,#84554,
#84555,#84556,#84557,#84558,#84559,#84560,#84561,#84562,#84563,#84564,#84565,
#84566,#84567,#84568,#84569,#84570,#84571,#84572,#84573,#84574,#84575,#84576,
#84577,#84578,#84579,#84580,#84581,#84582,#84583,#84584,#84585,#84586,#84587,
#84588,#84589,#84590,#84591,#84592,#84593,#84594,#84595,#84596,#84597,#84598,
#84599,#84600,#84601,#84602,#84603,#84604,#84605,#84606,#84607,#84608,#84609,
#84610,#84611,#84612,#84613,#84614,#84615,#84616,#84617,#84618,#84619,#84620,
#84621,#84622,#84623,#84624,#84625,#84626,#84627,#84628,#84629,#84630,#84631,
#84632,#84633,#84634,#84635,#84636,#84637,#84638,#84639,#84640,#84641,#84642,
#84643,#84644,#84645,#84646,#84647,#84648,#84649,#84650,#84651,#84652,#84653,
#84654,#84655,#84656),.UNSPECIFIED.,.F.,.F.,(4,2,2,2,2,2,2,2,2,2,2,2,2,
2,2,2,2,2,2,2,2,2,2,2,2,2,2,2,2,2,2,2,2,2,2,2,2,2,2,2,2,2,2,2,2,2,2,2,2,
2,2,2,2,2,2,2,2,2,2,2,2,2,2,2,2,2,2,2,2,2,2,2,2,2,2,2,2,2,2,2,2,2,2,2,2,
2,2,2,2,2,2,2,2,2,2,2,2,2,2,2,2,2,2,2,2,2,2,2,2,2,2,2,2,4),(-2.59342127676457,
-2.59048347284373,-2.54045199528121,-2.51630178484054,-2.50447831747976,
-2.49650002328404,-2.49355707467113,-2.49176590198081,-2.48982514440233,
-2.48728500586137,-2.48299429910268,-2.44777540686383,-2.39856697908379,
-2.3891424325095,-2.38699017674455,-2.38575994222461,-2.38468521307211,
-2.38329952089089,-2.38040111992613,-2.35385739992858,-2.31526623638961,
-2.29654057056957,-2.28527861604887,-2.28192471693209,-2.27982794224699,
-2.27789513903704,-2.27540626891932,-2.27129123399137,-2.24455521972296,
-2.20210370055799,-2.18556312888556,-2.17702741818053,-2.17494201465344,
-2.17372656058519,-2.172649081184,-2.1712623768787,-2.16896599724637,-2.15513638327683,
-2.10779708797665,-2.07839186059568,-2.07187523012424,-2.06915229639498,
-2.06718772501885,-2.06539756810838,-2.06254755632007,-2.05575554413522,
-2.0015313401453,-1.97640103482375,-1.96529343999646,-1.96303224305336,
-1.96177812980237,-1.96070635366049,-1.95935500803608,-1.95671731284662,
-1.94026815262134,-1.93129592700923,-1.892333429793,-1.86585500528528,-1.85969224367934,
-1.85702958086473,-1.85507573992727,-1.85327246813406,-1.85035097167035,
-1.84312915331335,-1.79883075419771,-1.78472735817278,-1.76327449280604,
-1.75318355352458,-1.75098561310118,-1.74974531556408,-1.74867201157841,
-1.7473014542876,-1.74510854310032,-1.73333758204521,-1.72962677565314,
-1.72236564461493,-1.67901010743369,-1.6604227014912,-1.64921989415206,
-1.64587223247618,-1.64377681881014,-1.64184354696978,-1.63935166667531,
-1.63522645412308,-1.60809060366594,-1.56616641310786,-1.54954739157589,
-1.54098480514965,-1.53889725431586,-1.53768131544922,-1.53660392346626,
-1.53521799903576,-1.53292429377116,-1.51915036506596,-1.50784474710706,
-1.46844818572822,-1.44187539589865,-1.43570088566117,-1.43303617799437,
-1.4310819774494,-1.42927917484296,-1.42636022835657,-1.41915356445291,
-1.37307258371222,-1.33396209739049,-1.33297755094329,-1.32826982515185,
-1.32653034500397,-1.32550501788735,-1.32441218791099,-1.32290011871591,
-1.31930849215528,-1.28017021908768,-1.25968440107285),.UNSPECIFIED.);
#867=B_SPLINE_CURVE_WITH_KNOTS('',3,(#84662,#84663,#84664,#84665,#84666,
#84667,#84668,#84669,#84670,#84671,#84672,#84673,#84674,#84675,#84676,#84677),
 .UNSPECIFIED.,.F.,.F.,(4,2,2,2,2,2,2,4),(-0.0749587606043023,-0.0267279161832551,
-0.0187640096720314,-0.00802108930702553,-0.00466632912088836,-0.00258130053910898,
-0.00128118358441392,-0.000628940636314346),.UNSPECIFIED.);
#868=B_SPLINE_CURVE_WITH_KNOTS('',3,(#84678,#84679,#84680,#84681,#84682,
#84683,#84684,#84685,#84686,#84687,#84688,#84689,#84690,#84691,#84692,#84693,
#84694,#84695,#84696,#84697,#84698,#84699,#84700,#84701,#84702,#84703,#84704,
#84705,#84706,#84707,#84708,#84709,#84710,#84711,#84712,#84713,#84714,#84715,
#84716,#84717,#84718,#84719,#84720,#84721,#84722,#84723,#84724,#84725,#84726,
#84727,#84728,#84729,#84730,#84731,#84732,#84733,#84734,#84735,#84736,#84737,
#84738,#84739,#84740,#84741,#84742,#84743,#84744,#84745,#84746,#84747,#84748,
#84749,#84750,#84751,#84752,#84753,#84754,#84755,#84756,#84757,#84758,#84759,
#84760,#84761,#84762,#84763,#84764,#84765,#84766,#84767,#84768,#84769,#84770,
#84771,#84772,#84773,#84774,#84775,#84776,#84777,#84778,#84779,#84780,#84781,
#84782,#84783,#84784,#84785,#84786,#84787,#84788,#84789,#84790,#84791,#84792,
#84793,#84794,#84795,#84796,#84797,#84798,#84799,#84800,#84801,#84802,#84803,
#84804,#84805,#84806,#84807,#84808,#84809,#84810,#84811,#84812,#84813,#84814,
#84815,#84816,#84817,#84818,#84819,#84820,#84821,#84822,#84823,#84824,#84825,
#84826,#84827,#84828,#84829,#84830,#84831,#84832,#84833,#84834,#84835,#84836,
#84837,#84838,#84839,#84840,#84841,#84842,#84843,#84844,#84845,#84846,#84847,
#84848,#84849,#84850,#84851,#84852,#84853,#84854,#84855,#84856,#84857,#84858),
 .UNSPECIFIED.,.F.,.F.,(4,3,3,3,3,3,3,3,3,3,3,3,3,3,3,3,3,3,3,3,3,3,3,3,
3,3,3,3,3,3,3,3,3,3,3,3,3,3,3,3,3,3,3,3,3,3,3,3,3,3,3,3,3,3,3,3,3,3,3,3,
4),(70.4243747954073,70.5325790413761,70.6410991164245,70.7497863837826,
70.8587740112805,70.9173879472931,71.020782684341,71.124023966456,71.2271439318483,
71.3301985000572,71.433221708415,71.5362475510875,71.6393803178656,71.7425694092754,
71.8459414026571,71.916224397255,72.0196191343029,72.1228604164179,72.2259803818102,
72.3290349500191,72.4320581583768,72.5350840010493,72.6382167678273,72.7414058592371,
72.8447778526187,72.9150608472168,73.0184555842647,73.1216968663798,73.2248168317721,
73.327871399981,73.4308946083388,73.5339204510113,73.6370532177894,73.7402423091992,
73.8436143025809,73.9138972971787,74.0172920342266,74.1205333163417,74.2236532817339,
74.3267078499429,74.4297310583006,74.5327569009731,74.6358896677512,74.739078759161,
74.8424507525426,74.9127337471406,75.0161284841885,75.1193697663036,75.2224897316958,
75.3255442999048,75.4285675082625,75.531593350935,75.6347261177131,75.7379152091229,
75.8412872025045,75.9115701971025,76.0134810050448,76.1152211478867,76.2168630906399,
76.3184433457415,76.3573194355999),.UNSPECIFIED.);
#869=B_SPLINE_CURVE_WITH_KNOTS('',3,(#84860,#84861,#84862,#84863,#84864,
#84865,#84866,#84867,#84868,#84869,#84870,#84871,#84872,#84873,#84874,#84875,
#84876,#84877,#84878,#84879,#84880,#84881,#84882,#84883,#84884,#84885,#84886,
#84887,#84888,#84889,#84890,#84891,#84892,#84893,#84894,#84895,#84896,#84897,
#84898,#84899,#84900,#84901,#84902,#84903,#84904,#84905,#84906,#84907,#84908,
#84909,#84910,#84911,#84912,#84913,#84914,#84915,#84916,#84917,#84918,#84919,
#84920,#84921,#84922,#84923,#84924,#84925,#84926,#84927,#84928,#84929,#84930,
#84931,#84932,#84933,#84934,#84935,#84936,#84937,#84938,#84939,#84940,#84941,
#84942,#84943,#84944,#84945,#84946,#84947,#84948,#84949,#84950,#84951,#84952,
#84953,#84954,#84955,#84956,#84957,#84958,#84959,#84960,#84961,#84962,#84963,
#84964,#84965,#84966,#84967,#84968,#84969,#84970,#84971,#84972,#84973,#84974,
#84975,#84976,#84977,#84978,#84979,#84980,#84981,#84982,#84983,#84984,#84985,
#84986,#84987,#84988,#84989,#84990,#84991,#84992,#84993,#84994,#84995,#84996,
#84997,#84998,#84999,#85000,#85001,#85002,#85003,#85004,#85005,#85006,#85007,
#85008,#85009,#85010,#85011,#85012,#85013,#85014,#85015,#85016,#85017,#85018,
#85019,#85020,#85021,#85022,#85023,#85024,#85025,#85026,#85027,#85028,#85029,
#85030,#85031,#85032,#85033,#85034,#85035,#85036,#85037,#85038,#85039,#85040,
#85041,#85042,#85043,#85044,#85045,#85046,#85047,#85048,#85049,#85050,#85051,
#85052,#85053,#85054,#85055,#85056,#85057,#85058,#85059,#85060,#85061,#85062,
#85063,#85064,#85065,#85066,#85067,#85068,#85069,#85070,#85071,#85072,#85073,
#85074,#85075),.UNSPECIFIED.,.F.,.F.,(4,2,2,2,2,2,2,2,2,2,2,2,2,2,2,2,2,
2,2,2,2,2,2,2,2,2,2,2,2,2,2,2,2,2,2,2,2,2,2,2,2,2,2,2,2,2,2,2,2,2,2,2,2,
2,2,2,2,2,2,2,2,2,2,2,2,2,2,2,2,2,2,2,2,2,2,2,2,2,2,2,2,2,2,2,2,2,2,2,2,
2,2,2,2,2,2,2,2,2,2,2,2,2,2,2,2,2,2,4),(-1.25968440107285,-1.23134347578101,
-1.22421236147874,-1.22130613077246,-1.21950569718235,-1.21754974221429,
-1.214874859563,-1.20864136135389,-1.18159485028042,-1.14086664256386,-1.11820860043456,
-1.11535572835216,-1.11397894521092,-1.11290509378181,-1.11166906463371,
-1.10949046358634,-1.09968791701672,-1.05077788475576,-1.0156573381461,
-1.01136168517331,-1.00882016949855,-1.00687924221377,-1.00480566813094,
-1.00155659108614,-0.991244538944737,-0.97468125440176,-0.941818681000237,
-0.92801074099284,-0.921314654636271,-0.905865157336135,-0.903497179120168,
-0.902089578970233,-0.901009420370377,-0.899805981254557,-0.89777422375533,
-0.889884513358211,-0.875168727792606,-0.846104339448585,-0.803698147926956,
-0.799404688600541,-0.796863865827195,-0.794923119199462,-0.792849400123064,
-0.789599389932939,-0.77927842035718,-0.76269514373061,-0.729816832146161,
-0.714514095931957,-0.709793811429688,-0.693941568281681,-0.691328755516341,
-0.68998289852579,-0.68891165470866,-0.687653737904237,-0.685374427258513,
-0.673948899363318,-0.647572546076294,-0.595122289395258,-0.588188795527061,
-0.58531575244097,-0.583521645885682,-0.581561193574165,-0.578859464301349,
-0.572467091586332,-0.52604566064621,-0.484947992336852,-0.480263111631424,
-0.478527326250482,-0.477502874864194,-0.476409871273696,-0.474895753303722,
-0.471290909056834,-0.432951879871835,-0.383317243140413,-0.376221625973913,
-0.373321714677207,-0.371522724177452,-0.369566380190154,-0.366887433827155,
-0.360806482143914,-0.352445538208922,-0.301550797636007,-0.270313243057044,
-0.267401275346587,-0.266013098458514,-0.264938282866957,-0.26371001827139,
-0.261566050199208,-0.252414976638071,-0.203666464120236,-0.167704290948247,
-0.162982357055917,-0.160559558829926,-0.15864067763351,-0.156487804181213,
-0.154258049270772,-0.146612099116105,-0.121083046665255,-0.100337619252734,
-0.0610229402433785,-0.0562870055113607,-0.0545435823234888,-0.0535177065565094,
-0.0524257940207308,-0.0509174412395485,-0.0492296228409805,-0.0462824128736715,
-0.000629120905446686),.UNSPECIFIED.);
#870=B_SPLINE_CURVE_WITH_KNOTS('',3,(#85076,#85077,#85078,#85079,#85080,
#85081,#85082,#85083,#85084,#85085,#85086,#85087,#85088),.UNSPECIFIED.,
 .F.,.F.,(4,3,3,3,4),(-66.6728921052185,-66.5709585796818,-66.4690950147619,
-66.3672509448715,-66.322858757962),.UNSPECIFIED.);
#871=B_SPLINE_CURVE_WITH_KNOTS('',3,(#85093,#85094,#85095,#85096,#85097,
#85098,#85099,#85100,#85101,#85102,#85103,#85104,#85105,#85106,#85107,#85108,
#85109,#85110,#85111,#85112,#85113,#85114,#85115,#85116,#85117,#85118,#85119,
#85120,#85121,#85122,#85123,#85124,#85125,#85126,#85127,#85128,#85129,#85130,
#85131,#85132,#85133,#85134,#85135,#85136,#85137,#85138,#85139,#85140,#85141,
#85142,#85143,#85144,#85145,#85146,#85147,#85148,#85149,#85150,#85151,#85152,
#85153,#85154,#85155,#85156,#85157,#85158,#85159,#85160,#85161,#85162,#85163,
#85164,#85165,#85166,#85167,#85168,#85169,#85170,#85171,#85172,#85173,#85174,
#85175,#85176,#85177,#85178,#85179,#85180,#85181,#85182,#85183,#85184,#85185,
#85186,#85187,#85188,#85189,#85190,#85191,#85192,#85193,#85194,#85195,#85196,
#85197,#85198,#85199,#85200,#85201,#85202,#85203,#85204,#85205,#85206,#85207,
#85208,#85209,#85210,#85211,#85212,#85213,#85214,#85215,#85216,#85217,#85218,
#85219,#85220,#85221,#85222,#85223,#85224,#85225,#85226,#85227,#85228,#85229,
#85230,#85231,#85232,#85233,#85234,#85235,#85236,#85237,#85238,#85239,#85240,
#85241,#85242,#85243,#85244,#85245,#85246,#85247,#85248,#85249,#85250,#85251,
#85252,#85253,#85254,#85255,#85256,#85257,#85258,#85259,#85260,#85261,#85262,
#85263,#85264,#85265,#85266,#85267,#85268,#85269,#85270,#85271,#85272,#85273,
#85274,#85275,#85276,#85277,#85278,#85279,#85280,#85281,#85282,#85283,#85284,
#85285,#85286,#85287,#85288,#85289,#85290,#85291,#85292,#85293,#85294,#85295,
#85296,#85297,#85298,#85299,#85300,#85301,#85302,#85303,#85304,#85305,#85306,
#85307,#85308,#85309,#85310,#85311,#85312,#85313,#85314,#85315,#85316,#85317,
#85318,#85319,#85320,#85321,#85322,#85323,#85324,#85325,#85326,#85327,#85328),
 .UNSPECIFIED.,.F.,.F.,(4,2,2,2,2,2,2,2,2,2,2,2,2,2,2,2,2,2,2,2,2,2,2,2,
2,2,2,2,2,2,2,2,2,2,2,2,2,2,2,2,2,2,2,2,2,2,2,2,2,2,2,2,2,2,2,2,2,2,2,2,
2,2,2,2,2,2,2,2,2,2,2,2,2,2,2,2,2,2,2,2,2,2,2,2,2,2,2,2,2,2,2,2,2,2,2,2,
2,2,2,2,2,2,2,2,2,2,2,2,2,2,2,2,2,2,2,2,2,4),(-1.40860718540471,-1.39545808993048,
-1.38405624528616,-1.38177793059313,-1.3805200509377,-1.37944853194231,
-1.37810193303849,-1.37548652011566,-1.35956495703151,-1.35506264588485,
-1.33449830662054,-1.28614136850048,-1.2789919571089,-1.27608255110672,
-1.27428145157858,-1.27232580019934,-1.26965318149743,-1.26343338839415,
-1.23649954831244,-1.19597179011588,-1.17297882026764,-1.17012328492731,
-1.16874592682677,-1.1676719609531,-1.16643617728359,-1.16425891186825,
-1.15447735403195,-1.10554601526657,-1.07041727374431,-1.06612126926768,
-1.063579569456,-1.06163851526854,-1.05956481891129,-1.05631557804374,-1.04600323997315,
-1.0294397184734,-0.99657573807322,-0.982832105893307,-0.97598240220263,
-0.975672104818647,-0.970158116277952,-0.960090031442436,-0.958006977478143,
-0.956669998370231,-0.955599167368023,-0.954333955366218,-0.952021328308135,
-0.93999299257142,-0.888103875649836,-0.858245896180985,-0.854050891734989,
-0.851538739815541,-0.849602590843724,-0.847516780118267,-0.844211760805237,
-0.833400814558471,-0.815717905738926,-0.765188925544749,-0.748664645534886,
-0.746024308779368,-0.744672487254501,-0.743600790811616,-0.742347304807065,
-0.740088573175662,-0.729020101582865,-0.704034607495391,-0.649565231152326,
-0.64279328250916,-0.639946816886022,-0.638157450646532,-0.636192587999127,
-0.633467098953572,-0.626933960763457,-0.597388862372985,-0.557146604210194,
-0.552471553511539,-0.536616903204568,-0.534004059815459,-0.532658204128811,
-0.53158697035396,-0.530329075783386,-0.528049832044696,-0.516625192277147,
-0.490252175671931,-0.437797642683444,-0.430864864546959,-0.427991956806278,
-0.42619788771247,-0.424237438622548,-0.421535644843532,-0.415142795035289,
-0.368523243439547,-0.32763686859989,-0.322943240982788,-0.321206137539336,
-0.320181434593666,-0.319088610059422,-0.317575470945896,-0.313976333882245,
-0.276223914328954,-0.225951975819304,-0.218893242814937,-0.216053511747662,
-0.214086005908784,-0.212152793090381,-0.210202190533758,-0.205221672264368,
-0.167218897660105,-0.126530071387855,-0.112454765384175,-0.110146844098719,
-0.108756903288708,-0.107679218613484,-0.1064661349924,-0.104390619277934,
-0.0959745790071875,-0.0797771645789183,-0.0749587606043023),
 .UNSPECIFIED.);
#872=B_SPLINE_CURVE_WITH_KNOTS('',3,(#85330,#85331,#85332,#85333,#85334,
#85335,#85336,#85337,#85338,#85339,#85340,#85341,#85342,#85343,#85344,#85345,
#85346,#85347,#85348,#85349,#85350,#85351,#85352,#85353,#85354,#85355,#85356,
#85357,#85358,#85359,#85360,#85361,#85362,#85363,#85364,#85365,#85366,#85367,
#85368,#85369,#85370,#85371,#85372,#85373,#85374,#85375,#85376,#85377,#85378,
#85379,#85380,#85381,#85382,#85383,#85384,#85385,#85386,#85387,#85388,#85389,
#85390,#85391,#85392,#85393,#85394,#85395,#85396,#85397,#85398,#85399,#85400,
#85401,#85402,#85403,#85404,#85405,#85406,#85407,#85408,#85409,#85410,#85411,
#85412,#85413,#85414,#85415,#85416,#85417,#85418,#85419,#85420,#85421,#85422,
#85423,#85424,#85425,#85426,#85427,#85428,#85429,#85430,#85431,#85432,#85433,
#85434,#85435,#85436,#85437,#85438,#85439,#85440,#85441,#85442,#85443,#85444,
#85445,#85446,#85447,#85448,#85449,#85450,#85451,#85452,#85453,#85454,#85455,
#85456,#85457,#85458,#85459,#85460,#85461,#85462,#85463,#85464,#85465,#85466,
#85467,#85468,#85469,#85470,#85471,#85472,#85473,#85474,#85475,#85476,#85477,
#85478,#85479,#85480,#85481,#85482,#85483,#85484,#85485,#85486,#85487,#85488,
#85489,#85490,#85491,#85492,#85493,#85494,#85495,#85496,#85497,#85498,#85499,
#85500,#85501,#85502,#85503,#85504,#85505,#85506,#85507),.UNSPECIFIED.,
 .F.,.F.,(4,3,3,3,3,3,3,3,3,3,3,3,3,3,3,3,3,3,3,3,3,3,3,3,3,3,3,3,3,3,3,
3,3,3,3,3,3,3,3,3,3,3,3,3,3,3,3,3,3,3,3,3,3,3,3,3,3,3,3,4),(-66.322858757962,
-66.2209269068389,-66.1189508263109,-66.0167874108514,-65.9232056974837,
-65.8198109604357,-65.7165696783206,-65.6134497129282,-65.5103951447193,
-65.4073719363614,-65.3043460936888,-65.2012133269107,-65.0980242355009,
-64.9946522421192,-64.9243692475218,-64.820974510474,-64.7177332283587,
-64.6146132629665,-64.5115586947577,-64.4085354864001,-64.3055096437274,
-64.2023768769493,-64.0991877855396,-63.995815792158,-63.92553279756,-63.8221380605121,
-63.718896778397,-63.6157768130047,-63.5127222447958,-63.4096990364381,
-63.3066731937655,-63.2035404269875,-63.1003513355777,-62.9969793421961,
-62.9266963475981,-62.8233016105501,-62.7200603284353,-62.6169403630429,
-62.513885794834,-62.4108625864763,-62.3078367438037,-62.2047039770256,
-62.1015148856157,-61.998142892234,-61.9278598976362,-61.8244651605883,
-61.7212238784734,-61.6181039130811,-61.5150493448724,-61.4120261365148,
-61.3090002938418,-61.2058675270639,-61.1026784356542,-60.9993064422726,
-60.9290234476744,-60.8220651862382,-60.7139755891884,-60.6074364851714,
-60.4985716416052,-60.3897067980389),.UNSPECIFIED.);
#873=B_SPLINE_CURVE_WITH_KNOTS('',3,(#85508,#85509,#85510,#85511),
 .UNSPECIFIED.,.F.,.F.,(4,4),(-60.3897037700498,-60.0402339961103),
 .UNSPECIFIED.);
#874=B_SPLINE_CURVE_WITH_KNOTS('',3,(#85517,#85518,#85519,#85520,#85521,
#85522),.UNSPECIFIED.,.F.,.F.,(4,2,4),(-0.0750400054689081,-0.0533928212318036,
-0.000629601363601487),.UNSPECIFIED.);
#875=B_SPLINE_CURVE_WITH_KNOTS('',3,(#85523,#85524,#85525,#85526,#85527,
#85528,#85529,#85530,#85531,#85532,#85533,#85534,#85535,#85536,#85537,#85538,
#85539,#85540,#85541,#85542,#85543,#85544,#85545,#85546,#85547,#85548,#85549,
#85550,#85551,#85552,#85553,#85554,#85555,#85556,#85557,#85558,#85559,#85560,
#85561,#85562,#85563,#85564,#85565,#85566,#85567,#85568,#85569,#85570,#85571,
#85572,#85573,#85574,#85575,#85576,#85577,#85578,#85579,#85580,#85581,#85582,
#85583,#85584,#85585,#85586,#85587,#85588,#85589,#85590,#85591,#85592,#85593,
#85594,#85595,#85596,#85597,#85598,#85599,#85600,#85601,#85602,#85603,#85604,
#85605,#85606,#85607,#85608,#85609,#85610,#85611,#85612,#85613,#85614,#85615,
#85616,#85617,#85618,#85619,#85620,#85621,#85622,#85623,#85624,#85625,#85626,
#85627,#85628,#85629,#85630,#85631,#85632,#85633,#85634,#85635,#85636,#85637,
#85638,#85639,#85640,#85641,#85642,#85643,#85644,#85645,#85646,#85647,#85648,
#85649,#85650,#85651,#85652,#85653,#85654,#85655,#85656,#85657,#85658,#85659,
#85660,#85661,#85662,#85663,#85664,#85665,#85666,#85667,#85668,#85669,#85670,
#85671,#85672,#85673,#85674,#85675,#85676,#85677,#85678,#85679,#85680,#85681,
#85682,#85683,#85684,#85685,#85686,#85687,#85688,#85689,#85690,#85691,#85692,
#85693,#85694,#85695,#85696,#85697,#85698,#85699,#85700,#85701,#85702,#85703,
#85704,#85705,#85706,#85707,#85708,#85709,#85710,#85711,#85712,#85713,#85714,
#85715,#85716,#85717,#85718,#85719,#85720,#85721,#85722,#85723,#85724,#85725,
#85726,#85727,#85728,#85729,#85730,#85731,#85732,#85733,#85734,#85735,#85736,
#85737,#85738,#85739,#85740,#85741,#85742,#85743,#85744,#85745,#85746,#85747,
#85748,#85749,#85750,#85751,#85752,#85753,#85754,#85755,#85756,#85757,#85758,
#85759,#85760,#85761,#85762,#85763,#85764,#85765,#85766,#85767,#85768,#85769,
#85770,#85771,#85772,#85773,#85774),.UNSPECIFIED.,.F.,.F.,(4,2,2,2,2,2,
2,2,2,2,2,2,2,2,2,2,2,2,2,2,2,2,2,2,2,2,2,2,2,2,2,2,2,2,2,2,2,2,2,2,2,2,
2,2,2,2,2,2,2,2,2,2,2,2,2,2,2,2,2,2,2,2,2,2,2,2,2,2,2,2,2,2,2,2,2,2,2,2,
2,2,2,2,2,2,2,2,2,2,2,2,2,2,2,2,2,2,2,2,2,2,2,2,2,2,2,2,2,2,2,2,2,2,2,2,
2,2,2,2,2,2,2,2,2,2,2,4),(-2.66809500613749,-2.66003737079873,-2.65567972419421,
-2.65426658705818,-2.65319922550382,-2.65216891022884,-2.65098887662144,
-2.64906346401233,-2.64299730418109,-2.64171516263787,-2.63391396391436,
-2.58086173899162,-2.56301613163371,-2.55213395024574,-2.54882039643755,
-2.54673224354217,-2.54479601378358,-2.54228671783658,-2.53810299894828,
-2.50874889582129,-2.46751320115535,-2.452047531728,-2.44662577265192,-2.44402429013868,
-2.44191582684355,-2.44070265038365,-2.44069954126522,-2.44069641315407,
-2.44069326608247,-2.44069009995937,-2.44068691443319,-2.44068370945783,
-2.44068048479903,-2.44067724042621,-2.44067397628221,-2.44067069219663,
-2.44066738796819,-2.44066406353025,-2.44066073156736,-2.44065738525505,
-2.44065401781087,-2.44065062905198,-2.44064720769557,-2.43961927545029,
-2.43823982570499,-2.4353731301731,-2.39981442473688,-2.36690462497572,
-2.344124633947,-2.33844102161752,-2.3358640429016,-2.33392451108213,-2.33209915097093,
-2.3295628695129,-2.32295878519058,-2.26677128155561,-2.24294981956697,
-2.23219106010818,-2.22995079072762,-2.22870125010139,-2.22762904750754,
-2.22627160190742,-2.22412178656339,-2.21301973096917,-2.16174691742912,
-2.13313406475128,-2.12671135454216,-2.1240042704081,-2.122042650224,-2.12024935039312,
-2.11738167453837,-2.11048217807699,-2.05758353202986,-2.03154305390505,
-2.02020117751967,-2.01792645294227,-2.01666943047337,-2.01559795954986,
-2.0142505530444,-2.01163102257304,-1.99562806976032,-1.9901364525329,-1.97569906836753,
-1.94280344370365,-1.92623589621873,-1.91592271366936,-1.91267332660119,
-1.91059957214408,-1.90865848884485,-1.90611678859568,-1.9018208999285,
-1.8666880603306,-1.81772896417468,-1.80801166462807,-1.80583884657001,
-1.80460405019258,-1.80352996207818,-1.80215115513934,-1.79928817885767,
-1.7632764622433,-1.73051723134771,-1.7079751678773,-1.70232341243381,-1.69975212318208,
-1.69781331258464,-1.69598601545781,-1.69344284687175,-1.68679602284043,
-1.63101292099283,-1.59811451212367,-1.59456756021743,-1.59306309617033,
-1.59197154165544,-1.59094404025414,-1.58919363814061,-1.58441434265556,
-1.54724248996085,-1.49696430469026,-1.49056164232697,-1.48785778282483,
-1.48589659592665,-1.48410238033114,-1.48123037997351,-1.47430567066695,
-1.42173351548525,-1.40860718540471),.UNSPECIFIED.);
#876=B_SPLINE_CURVE_WITH_KNOTS('',3,(#85776,#85777,#85778,#85779,#85780,
#85781,#85782,#85783,#85784,#85785),.UNSPECIFIED.,.F.,.F.,(4,1,1,1,1,1,
1,4),(-60.0402339961103,-59.9301869977125,-58.9313505477506,-57.9325140977887,
-56.9336776478269,-55.934841197865,-54.9360047479031,-54.1065275196808),
 .UNSPECIFIED.);
#877=B_SPLINE_CURVE_WITH_KNOTS('',3,(#85786,#85787,#85788,#85789,#85790,
#85791,#85792,#85793,#85794,#85795,#85796,#85797,#85798,#85799,#85800,#85801,
#85802,#85803,#85804,#85805,#85806,#85807),.UNSPECIFIED.,.F.,.F.,(4,2,2,
2,2,2,2,2,2,2,4),(-2.66746648764681,-2.64323635106775,-2.63610435627689,
-2.63431343163605,-2.63309845601206,-2.63208936873757,-2.63101477987198,
-2.62962873109103,-2.62672769851142,-2.59980703035293,-2.59336498099373),
 .UNSPECIFIED.);
#878=B_SPLINE_CURVE_WITH_KNOTS('',3,(#85812,#85813,#85814,#85815,#85816,
#85817,#85818,#85819,#85820,#85821,#85822,#85823,#85824,#85825,#85826,#85827,
#85828,#85829,#85830,#85831,#85832,#85833,#85834,#85835,#85836,#85837,#85838,
#85839,#85840,#85841,#85842,#85843,#85844,#85845,#85846,#85847,#85848,#85849,
#85850,#85851,#85852,#85853,#85854,#85855,#85856,#85857,#85858,#85859,#85860,
#85861,#85862,#85863,#85864,#85865,#85866,#85867,#85868,#85869,#85870,#85871,
#85872,#85873,#85874,#85875,#85876,#85877,#85878,#85879,#85880,#85881,#85882,
#85883,#85884,#85885,#85886,#85887,#85888,#85889,#85890,#85891,#85892,#85893,
#85894,#85895,#85896,#85897,#85898,#85899,#85900,#85901,#85902,#85903,#85904,
#85905,#85906,#85907,#85908,#85909,#85910,#85911,#85912,#85913,#85914,#85915,
#85916,#85917,#85918,#85919,#85920,#85921,#85922,#85923,#85924,#85925,#85926,
#85927,#85928,#85929,#85930,#85931,#85932,#85933,#85934,#85935,#85936,#85937,
#85938,#85939,#85940,#85941,#85942,#85943,#85944,#85945,#85946,#85947,#85948,
#85949,#85950,#85951,#85952,#85953,#85954,#85955,#85956,#85957,#85958,#85959,
#85960,#85961,#85962,#85963,#85964,#85965,#85966,#85967,#85968,#85969,#85970,
#85971,#85972,#85973,#85974,#85975,#85976,#85977,#85978,#85979,#85980,#85981,
#85982,#85983,#85984,#85985,#85986,#85987,#85988,#85989,#85990,#85991,#85992,
#85993,#85994,#85995,#85996,#85997,#85998,#85999,#86000,#86001,#86002,#86003,
#86004,#86005,#86006,#86007,#86008,#86009,#86010,#86011,#86012,#86013,#86014,
#86015,#86016,#86017,#86018,#86019,#86020,#86021,#86022,#86023,#86024,#86025,
#86026,#86027,#86028,#86029,#86030,#86031,#86032,#86033,#86034,#86035,#86036,
#86037,#86038,#86039,#86040,#86041,#86042,#86043,#86044,#86045,#86046,#86047,
#86048,#86049,#86050,#86051,#86052,#86053),.UNSPECIFIED.,.F.,.F.,(4,2,2,
2,2,2,2,2,2,2,2,2,2,2,2,2,2,2,2,2,2,2,2,2,2,2,2,2,2,2,2,2,2,2,2,2,2,2,2,
2,2,2,2,2,2,2,2,2,2,2,2,2,2,2,2,2,2,2,2,2,2,2,2,2,2,2,2,2,2,2,2,2,2,2,2,
2,2,2,2,2,2,2,2,2,2,2,2,2,2,2,2,2,2,2,2,2,2,2,2,2,2,2,2,2,2,2,2,2,2,2,2,
2,2,2,2,2,2,2,2,2,4),(-1.40838688772306,-1.38230244357366,-1.3689629544219,
-1.36540809648996,-1.3632670538202,-1.3613458718201,-1.35890266866713,-1.3550283155242,
-1.33395525283396,-1.27614236927097,-1.26118233595888,-1.2588344111419,
-1.25743266749409,-1.2563533252078,-1.2551467114111,-1.25310066828271,-1.24504355176718,
-1.22986487393631,-1.18997000193031,-1.1589272040029,-1.15470580671402,
-1.15218595694187,-1.15024860976343,-1.14816616428751,-1.14487637778995,
-1.13420309883885,-1.11683233307578,-1.06813033440054,-1.06161521720435,
-1.04899334516723,-1.04675771195742,-1.04537434325928,-1.04429995546135,
-1.04306848022654,-1.04091018720103,-1.03139827240251,-0.982246778625874,
-0.947052503044537,-0.94275632244464,-0.940214801714153,-0.938274047406892,
-0.936200829559232,-0.932952668602648,-0.922646540217495,-0.906095637795037,
-0.873245520663565,-0.860327841072428,-0.837625961972406,-0.834772518271112,
-0.833395802704332,-0.832322165531018,-0.831086565469334,-0.828909157661812,
-0.819119234990314,-0.770211171374527,-0.735095479701707,-0.730800735191928,
-0.728259768505998,-0.72631926709606,-0.724246154408423,-0.720997813714003,
-0.710688211446137,-0.694128968940473,-0.661273965145536,-0.647500265802612,
-0.640732865430314,-0.639125212782759,-0.625206095140421,-0.622905976907174,
-0.62151840927512,-0.620441125137846,-0.61922687568498,-0.617145737159202,
-0.608657739676505,-0.59225104333614,-0.550125200292749,-0.522888990514207,
-0.518762151511242,-0.516270269944921,-0.514337569265241,-0.512243345501892,
-0.508898821763093,-0.497717993373553,-0.479181723901062,-0.434933754979829,
-0.413700363030104,-0.410884809280078,-0.409515665871969,-0.408442841512717,
-0.407202392723714,-0.40500245852627,-0.394872764219282,-0.373279481527361,
-0.365786413232853,-0.314761438692117,-0.307738844509065,-0.304851387375707,
-0.303054887736032,-0.301097089088425,-0.298408602847309,-0.292092278485095,
-0.264359179113338,-0.222328372943981,-0.201736020462186,-0.198933982706451,
-0.197567544224861,-0.196546512687276,-0.195348174400184,-0.193343619419814,
-0.190871317984728,-0.185820315614274,-0.171894974603336,-0.15129838099146,
-0.103002734319542,-0.0958553337604737,-0.092947074412366,-0.0911467847291241,
-0.0891920915881641,-0.0865209243899677,-0.0803051558083365,-0.0750400054689081),
 .UNSPECIFIED.);
#879=B_SPLINE_CURVE_WITH_KNOTS('',3,(#86054,#86055,#86056,#86057,#86058,
#86059,#86060,#86061,#86062,#86063,#86064,#86065,#86066,#86067,#86068,#86069,
#86070,#86071,#86072,#86073,#86074,#86075,#86076,#86077,#86078,#86079,#86080,
#86081,#86082,#86083,#86084,#86085,#86086,#86087,#86088,#86089,#86090,#86091,
#86092,#86093,#86094,#86095,#86096,#86097,#86098,#86099,#86100,#86101,#86102,
#86103,#86104,#86105,#86106,#86107,#86108,#86109,#86110,#86111,#86112,#86113,
#86114,#86115,#86116,#86117,#86118,#86119,#86120,#86121,#86122,#86123,#86124,
#86125,#86126,#86127,#86128,#86129,#86130,#86131,#86132,#86133,#86134,#86135,
#86136,#86137,#86138,#86139,#86140,#86141,#86142,#86143,#86144,#86145,#86146,
#86147,#86148,#86149,#86150,#86151,#86152,#86153,#86154,#86155,#86156,#86157,
#86158,#86159,#86160,#86161,#86162,#86163,#86164,#86165,#86166,#86167,#86168,
#86169,#86170,#86171,#86172,#86173,#86174,#86175,#86176,#86177,#86178,#86179,
#86180,#86181,#86182,#86183,#86184,#86185,#86186,#86187,#86188,#86189,#86190,
#86191,#86192,#86193,#86194,#86195,#86196,#86197,#86198,#86199,#86200,#86201,
#86202,#86203,#86204,#86205,#86206,#86207,#86208,#86209,#86210,#86211,#86212,
#86213,#86214,#86215,#86216,#86217,#86218,#86219,#86220,#86221,#86222,#86223,
#86224,#86225,#86226,#86227,#86228,#86229,#86230,#86231,#86232,#86233,#86234,
#86235,#86236,#86237,#86238,#86239,#86240,#86241,#86242,#86243,#86244,#86245,
#86246,#86247,#86248,#86249,#86250,#86251,#86252,#86253,#86254,#86255,#86256,
#86257,#86258,#86259,#86260,#86261,#86262,#86263,#86264,#86265,#86266,#86267,
#86268,#86269,#86270,#86271,#86272,#86273,#86274,#86275,#86276,#86277,#86278,
#86279,#86280,#86281,#86282,#86283,#86284,#86285),.UNSPECIFIED.,.F.,.F.,
(4,2,2,2,2,2,2,2,2,2,2,2,2,2,2,2,2,2,2,2,2,2,2,2,2,2,2,2,2,2,2,2,2,2,2,
2,2,2,2,2,2,2,2,2,2,2,2,2,2,2,2,2,2,2,2,2,2,2,2,2,2,2,2,2,2,2,2,2,2,2,2,
2,2,2,2,2,2,2,2,2,2,2,2,2,2,2,2,2,2,2,2,2,2,2,2,2,2,2,2,2,2,2,2,2,2,2,2,
2,2,2,2,2,2,2,2,4),(-2.59336498099373,-2.58612377715144,-2.57460295655263,
-2.54602644095796,-2.53212826401375,-2.52852472099612,-2.52637284115968,
-2.52445355466388,-2.52202850292267,-2.51729671326334,-2.47985852346038,
-2.42950698100758,-2.4230330905425,-2.42114165560786,-2.42013068020849,
-2.41905739996276,-2.41768570023441,-2.41548870872608,-2.40365158526575,
-2.34625429950801,-2.32969062991946,-2.31937983627995,-2.31613118864746,
-2.3140579029223,-2.31211725613926,-2.30957612426245,-2.30528118904737,
-2.2701552012624,-2.2212038755009,-2.21149260018589,-2.20932053545729,-2.20808607523894,
-2.20701222055165,-2.20563363609001,-2.2027708554975,-2.16714451094693,
-2.13426170118579,-2.11770520689291,-2.10739755892156,-2.10414919953203,
-2.10207592884624,-2.10013517747864,-2.09759373743708,-2.09329789758949,
-2.05811272113606,-2.00897230617553,-1.99947907606189,-1.99732216214529,
-1.99609100999797,-1.99501660919084,-1.9936328259664,-1.99139573413456,
-1.9787459135555,-1.97653424229513,-1.97434496400237,-1.92392173045384,
-1.90628615561207,-1.89549731307634,-1.89219485829476,-1.89010970551398,
-1.88817350573697,-1.88566035165332,-1.88146164769916,-1.85141490721498,
-1.79974588301394,-1.78774089675046,-1.78542972168894,-1.78416490230857,
-1.78309416754148,-1.7817570060096,-1.77967310600665,-1.76959088583284,
-1.76408849451663,-1.75666055670907,-1.74315355697832,-1.71027191066444,
-1.69371826756403,-1.68341173156511,-1.68016336965071,-1.67809001251601,
-1.67614912062268,-1.67360741055167,-1.66931092146314,-1.6340939351491,
-1.5848491215704,-1.57547147075961,-1.57332268396228,-1.57209327523349,
-1.57101851553897,-1.56963179330887,-1.56738508325563,-1.55455222370681,
-1.55238617999346,-1.50510585335559,-1.47658175093414,-1.47016979631437,
-1.46746461537597,-1.46550341737666,-1.46370984438008,-1.46084029569995,
-1.45392885652446,-1.40119783292654,-1.37504354039233,-1.36367304688529,
-1.36139677139001,-1.36013945244606,-1.35906806863937,-1.35772120402661,
-1.3551039967121,-1.33914203000199,-1.33419803675157,-1.32855203675639,
-1.28159297975054,-1.28014689813355,-1.26110770786606,-1.25972990448764),
 .UNSPECIFIED.);
#880=B_SPLINE_CURVE_WITH_KNOTS('',3,(#86291,#86292,#86293,#86294,#86295,
#86296,#86297,#86298,#86299,#86300,#86301,#86302,#86303,#86304,#86305,#86306),
 .UNSPECIFIED.,.F.,.F.,(4,2,2,2,2,2,2,4),(-0.0747633067458267,-0.0741278680970252,
-0.0730557645895703,-0.0718087286992157,-0.0695788634709163,-0.0589815407426049,
-0.0357413577562223,-0.00062954340747806),.UNSPECIFIED.);
#881=B_SPLINE_CURVE_WITH_KNOTS('',3,(#86307,#86308,#86309,#86310,#86311,
#86312,#86313,#86314,#86315,#86316,#86317,#86318,#86319,#86320,#86321,#86322,
#86323,#86324,#86325,#86326,#86327,#86328,#86329,#86330,#86331,#86332,#86333,
#86334,#86335,#86336,#86337,#86338,#86339,#86340,#86341,#86342,#86343,#86344,
#86345,#86346,#86347,#86348,#86349,#86350,#86351,#86352,#86353,#86354,#86355,
#86356,#86357,#86358,#86359,#86360,#86361,#86362,#86363,#86364,#86365,#86366,
#86367,#86368,#86369,#86370,#86371,#86372,#86373,#86374,#86375,#86376,#86377,
#86378,#86379,#86380,#86381,#86382,#86383,#86384,#86385,#86386,#86387,#86388,
#86389,#86390,#86391,#86392,#86393,#86394,#86395,#86396,#86397,#86398,#86399,
#86400,#86401,#86402,#86403,#86404,#86405,#86406,#86407,#86408,#86409,#86410,
#86411,#86412,#86413,#86414,#86415,#86416,#86417,#86418,#86419,#86420,#86421,
#86422,#86423,#86424,#86425,#86426,#86427,#86428,#86429,#86430,#86431,#86432,
#86433,#86434,#86435,#86436,#86437,#86438,#86439,#86440,#86441,#86442,#86443,
#86444,#86445,#86446,#86447,#86448,#86449,#86450,#86451,#86452,#86453,#86454,
#86455,#86456,#86457,#86458,#86459,#86460,#86461,#86462,#86463,#86464,#86465,
#86466,#86467,#86468,#86469,#86470,#86471,#86472,#86473,#86474,#86475,#86476,
#86477,#86478,#86479,#86480,#86481,#86482,#86483,#86484,#86485,#86486,#86487,
#86488,#86489,#86490,#86491,#86492,#86493,#86494,#86495,#86496,#86497,#86498,
#86499,#86500,#86501,#86502,#86503,#86504,#86505,#86506,#86507,#86508,#86509,
#86510,#86511,#86512,#86513,#86514,#86515,#86516,#86517,#86518,#86519,#86520,
#86521,#86522,#86523,#86524,#86525,#86526,#86527,#86528,#86529,#86530,#86531,
#86532,#86533,#86534,#86535,#86536,#86537,#86538,#86539,#86540,#86541,#86542,
#86543,#86544,#86545,#86546,#86547,#86548,#86549,#86550,#86551,#86552,#86553,
#86554,#86555,#86556,#86557,#86558,#86559,#86560,#86561,#86562,#86563,#86564,
#86565,#86566,#86567,#86568,#86569,#86570,#86571,#86572,#86573,#86574),
 .UNSPECIFIED.,.F.,.F.,(4,2,2,2,2,2,2,2,2,2,2,2,2,2,2,2,2,2,2,2,2,2,2,2,
2,2,2,2,2,2,2,2,2,2,2,2,2,2,2,2,2,2,2,2,2,2,2,2,2,2,2,2,2,2,2,2,2,2,2,2,
2,2,2,2,2,2,2,2,2,2,2,2,2,2,2,2,2,2,2,2,2,2,2,2,2,2,2,2,2,2,2,2,2,2,2,2,
2,2,2,2,2,2,2,2,2,2,2,2,2,2,2,2,2,2,2,2,2,2,2,2,2,2,2,2,2,2,2,2,2,2,2,2,
2,4),(-2.66773872145495,-2.64241252558027,-2.63928554969506,-2.63713947602669,
-2.63533867351105,-2.63342472947524,-2.63105557271983,-2.62742202621152,
-2.61031671120093,-2.59812617594819,-2.55348115611806,-2.53501219789282,
-2.53117993176174,-2.52962817609444,-2.52852850087925,-2.52751377117936,
-2.5258273549798,-2.52146094153608,-2.47375191666192,-2.44446095946491,
-2.43444799925098,-2.42965975435597,-2.42576618372853,-2.42356262739359,
-2.42354995819552,-2.4235368515971,-2.42352329137586,-2.42350926072277,
-2.42349473912475,-2.42347970994217,-2.42346415578335,-2.4234480568527,
-2.42343139254774,-2.42341414145426,-2.42339628125805,-2.42337778868366,
-2.4233586395713,-2.42333880874003,-2.42331826995378,-2.42329699594181,
-2.42327495825973,-2.42325212674527,-2.42323282571979,-2.42321027756231,
-2.42318393277581,-2.42315314833329,-2.42311717188563,-2.42307512336121,
-2.42302736684747,-2.42108673959665,-2.41854502817043,-2.41424775666325,
-2.37918547353218,-2.33040402256907,-2.32049585296989,-2.31831050487343,
-2.31707318244614,-2.31599982764569,-2.31462578450445,-2.3124207068573,
-2.30036184922826,-2.24416348853271,-2.22062564956556,-2.21484159161938,
-2.21224675635151,-2.21030485039764,-2.20848530346745,-2.20596988674875,
-2.1994925453796,-2.14221577091108,-2.11910848208663,-2.10854717635702,
-2.10631954953316,-2.10507298661917,-2.10400080970302,-2.10264013901542,
-2.0999577347487,-2.08228655993597,-2.033887122098,-2.00890354709408,-2.0029308528024,
-2.00030214126094,-1.99835463635392,-1.99654399145709,-1.99406302454134,
-1.98779240179784,-1.92885811313851,-1.90677667843905,-1.89650476019713,
-1.89429543948097,-1.89305285336334,-1.89198016977548,-1.89061377415086,
-1.88843395598268,-1.87682215435673,-1.87294119289219,-1.87270452445276,
-1.8658392028681,-1.85210677914542,-1.81922599238434,-1.80267118267403,
-1.79236438822734,-1.78911619381477,-1.78704300342312,-1.78510230965067,
-1.78256091967883,-1.77826510762717,-1.74307236981169,-1.69390412678815,
-1.68444508453741,-1.68229063846524,-1.68106005453799,-1.6799856052173,
-1.67860104349444,-1.67570770147822,-1.64967487965741,-1.6115097133864,
-1.58248330931025,-1.578087932836,-1.57576448500794,-1.57385298149189,-1.57162897726566,
-1.56780092678016,-1.55274039453732,-1.50057476592015,-1.48173019249633,
-1.47243485082074,-1.47029206737946,-1.46906402334406,-1.46798910731072,
-1.466600402696,-1.46368594057752,-1.43364138024875,-1.40838688772306),
 .UNSPECIFIED.);
#882=B_SPLINE_CURVE_WITH_KNOTS('',3,(#86576,#86577,#86578,#86579,#86580,
#86581,#86582,#86583,#86584,#86585,#86586,#86587,#86588,#86589,#86590,#86591,
#86592,#86593,#86594,#86595,#86596,#86597,#86598,#86599,#86600,#86601,#86602,
#86603,#86604,#86605,#86606,#86607,#86608,#86609,#86610,#86611,#86612,#86613,
#86614,#86615,#86616,#86617,#86618,#86619,#86620,#86621,#86622,#86623,#86624,
#86625,#86626,#86627,#86628,#86629,#86630,#86631,#86632,#86633,#86634,#86635,
#86636,#86637,#86638,#86639,#86640,#86641,#86642,#86643,#86644,#86645,#86646,
#86647,#86648,#86649,#86650,#86651,#86652,#86653,#86654,#86655,#86656,#86657,
#86658,#86659,#86660,#86661,#86662,#86663,#86664,#86665,#86666,#86667,#86668,
#86669,#86670,#86671,#86672,#86673,#86674,#86675,#86676,#86677,#86678,#86679,
#86680,#86681,#86682,#86683,#86684,#86685,#86686,#86687,#86688,#86689,#86690,
#86691,#86692,#86693,#86694,#86695,#86696,#86697,#86698,#86699,#86700,#86701,
#86702,#86703,#86704,#86705,#86706,#86707,#86708,#86709,#86710,#86711,#86712,
#86713,#86714,#86715,#86716,#86717,#86718,#86719,#86720,#86721,#86722,#86723,
#86724,#86725,#86726,#86727,#86728,#86729,#86730,#86731,#86732,#86733,#86734,
#86735,#86736,#86737,#86738,#86739,#86740,#86741,#86742,#86743,#86744,#86745,
#86746,#86747,#86748,#86749,#86750,#86751,#86752,#86753,#86754,#86755,#86756,
#86757,#86758,#86759,#86760,#86761,#86762,#86763,#86764,#86765,#86766,#86767,
#86768,#86769,#86770,#86771,#86772,#86773,#86774,#86775,#86776,#86777,#86778,
#86779,#86780,#86781,#86782,#86783,#86784,#86785,#86786,#86787,#86788,#86789,
#86790,#86791,#86792,#86793),.UNSPECIFIED.,.F.,.F.,(4,2,2,2,2,2,2,2,2,2,
2,2,2,2,2,2,2,2,2,2,2,2,2,2,2,2,2,2,2,2,2,2,2,2,2,2,2,2,2,2,2,2,2,2,2,2,
2,2,2,2,2,2,2,2,2,2,2,2,2,2,2,2,2,2,2,2,2,2,2,2,2,2,2,2,2,2,2,2,2,2,2,2,
2,2,2,2,2,2,2,2,2,2,2,2,2,2,2,2,2,2,2,2,2,2,2,2,2,2,4),(-1.25972990448764,
-1.25734657803934,-1.2549378371491,-1.25302008873775,-1.25085789112559,
-1.24720806171467,-1.23275541257723,-1.18236867555363,-1.15270122528572,
-1.14978674158883,-1.14839798039503,-1.14732299543195,-1.14609485382689,
-1.14395184167295,-1.13465490831496,-1.11580348097264,-1.07535035023734,
-1.06307169323884,-1.0484919271737,-1.04470596277304,-1.04249151506882,
-1.04057923218866,-1.03824355543878,-1.03379049295154,-1.00275461896363,
-0.95477787149643,-0.940188171153965,-0.937855789338092,-0.936458547161109,
-0.935379753962438,-0.934170502638011,-0.932112819458008,-0.923917714333937,
-0.908352379753073,-0.866771560268404,-0.854701250343117,-0.836944102576898,
-0.833267479208628,-0.830884677684527,-0.828969179144978,-0.826789683687461,
-0.823061780392079,-0.807615908699947,-0.75602335284784,-0.728679195530954,
-0.725774719653931,-0.724387870099407,-0.723313046637944,-0.722083613211083,
-0.719934882333577,-0.710559332764686,-0.661284102723659,-0.626051785632179,
-0.621754785433216,-0.619212915369639,-0.617271972336409,-0.615198628524614,
-0.611950428120897,-0.601645504903761,-0.58509780259168,-0.552248689487846,
-0.539755468425894,-0.516621377773021,-0.513763443981024,-0.512385776512252,
-0.511311967519572,-0.510076813766818,-0.507901732814191,-0.498147754683301,
-0.449204440910873,-0.414076862766473,-0.40978089006016,-0.407239455898081,
-0.405298746730069,-0.403225556779169,-0.399977397106138,-0.389670915418459,
-0.373119106130488,-0.340268621774019,-0.327240925826132,-0.31850684934553,
-0.304211592955686,-0.30189193036109,-0.300498556793765,-0.299420448437986,
-0.298209391337645,-0.296142923050037,-0.287837897838107,-0.271958943551731,
-0.225888947742334,-0.20163851679482,-0.197623479772591,-0.195164524654203,
-0.193294488448743,-0.19126637998537,-0.188075034363523,-0.184319691678446,
-0.177183092180901,-0.159610048660014,-0.109454259189925,-0.0924346847407807,
-0.0897757999029687,-0.0884201282119508,-0.0873483077285469,-0.0860980469878534,
-0.0838535675899181,-0.0730192674453548,-0.0489118854442952,-0.000629479492146207),
 .UNSPECIFIED.);
#883=B_SPLINE_CURVE_WITH_KNOTS('',3,(#86794,#86795,#86796,#86797,#86798,
#86799,#86800,#86801,#86802,#86803,#86804,#86805,#86806,#86807,#86808,#86809,
#86810,#86811,#86812,#86813,#86814,#86815),.UNSPECIFIED.,.F.,.F.,(4,2,2,
2,2,2,2,2,2,2,4),(-2.66777374952406,-2.65998003102873,-2.65468366447004,
-2.65224032161588,-2.6503584941431,-2.64851781255906,-2.64669143457867,
-2.64415107708231,-2.63895997732565,-2.62644993719922,-2.59336156192323),
 .UNSPECIFIED.);
#884=B_SPLINE_CURVE_WITH_KNOTS('',3,(#86820,#86821,#86822,#86823,#86824,
#86825,#86826,#86827,#86828,#86829,#86830,#86831,#86832,#86833,#86834,#86835,
#86836,#86837,#86838,#86839,#86840,#86841,#86842,#86843,#86844,#86845,#86846,
#86847,#86848,#86849,#86850,#86851,#86852,#86853,#86854,#86855,#86856,#86857,
#86858,#86859,#86860,#86861,#86862,#86863,#86864,#86865,#86866,#86867,#86868,
#86869,#86870,#86871,#86872,#86873,#86874,#86875,#86876,#86877,#86878,#86879,
#86880,#86881,#86882,#86883,#86884,#86885,#86886,#86887,#86888,#86889,#86890,
#86891,#86892,#86893,#86894,#86895,#86896,#86897,#86898,#86899,#86900,#86901,
#86902,#86903,#86904,#86905,#86906,#86907,#86908,#86909,#86910,#86911,#86912,
#86913,#86914,#86915,#86916,#86917,#86918,#86919,#86920,#86921,#86922,#86923,
#86924,#86925,#86926,#86927,#86928,#86929,#86930,#86931,#86932,#86933,#86934,
#86935,#86936,#86937,#86938,#86939,#86940,#86941,#86942,#86943,#86944,#86945,
#86946,#86947,#86948,#86949,#86950,#86951,#86952,#86953,#86954,#86955,#86956,
#86957,#86958,#86959,#86960,#86961,#86962,#86963,#86964,#86965,#86966,#86967,
#86968,#86969,#86970,#86971,#86972,#86973,#86974,#86975,#86976,#86977,#86978,
#86979,#86980,#86981,#86982,#86983,#86984,#86985,#86986,#86987,#86988,#86989,
#86990,#86991,#86992,#86993,#86994,#86995,#86996,#86997,#86998,#86999,#87000,
#87001,#87002,#87003,#87004,#87005,#87006,#87007,#87008,#87009,#87010,#87011,
#87012,#87013,#87014,#87015,#87016,#87017,#87018,#87019,#87020,#87021,#87022,
#87023,#87024,#87025,#87026,#87027,#87028,#87029,#87030,#87031,#87032,#87033,
#87034,#87035,#87036,#87037,#87038,#87039,#87040,#87041),.UNSPECIFIED.,
 .F.,.F.,(4,2,2,2,2,2,2,2,2,2,2,2,2,2,2,2,2,2,2,2,2,2,2,2,2,2,2,2,2,2,2,
2,2,2,2,2,2,2,2,2,2,2,2,2,2,2,2,2,2,2,2,2,2,2,2,2,2,2,2,2,2,2,2,2,2,2,2,
2,2,2,2,2,2,2,2,2,2,2,2,2,2,2,2,2,2,2,2,2,2,2,2,2,2,2,2,2,2,2,2,2,2,2,2,
2,2,2,2,2,2,2,4),(-1.4084593254711,-1.36760689910925,-1.35571434309166,
-1.35117925453299,-1.34787084561134,-1.34640836269805,-1.34532365970278,
-1.34413477147142,-1.34216882516782,-1.33576371835975,-1.33420781199927,
-1.31962127788188,-1.26057978066336,-1.24627009272878,-1.24250840802672,
-1.24029957652405,-1.2383869228092,-1.23604419783816,-1.23155727455813,
-1.19919559199268,-1.15901192704814,-1.15407997627054,-1.13813083897073,
-1.13551432467702,-1.13416761743711,-1.13309625339311,-1.13183884103811,
-1.12956208907755,-1.11818343024146,-1.09199414519246,-1.0392716360922,
-1.03235709909658,-1.02948706073595,-1.02769341606812,-1.02573233367823,
-1.0230276595747,-1.0166185298546,-0.988121510261783,-0.937199226502322,
-0.92570675954955,-0.923533677672336,-0.922169221180612,-0.921096560420311,
-0.919852296675333,-0.917635805323615,-0.907255903943466,-0.884795019387741,
-0.82642782159497,-0.820075908530418,-0.817581030184306,-0.815766627036285,
-0.813821099518584,-0.811205575278863,-0.805308102231652,-0.780912575796105,
-0.730249222676817,-0.714074343533306,-0.711447954441862,-0.710099173965592,
-0.709027740462902,-0.707772076114364,-0.705503132941652,-0.694258425547811,
-0.6685932424672,-0.615123230736673,-0.608267079429076,-0.605406761343438,
-0.603614966737304,-0.601652505505277,-0.598939683635388,-0.592481599269618,
-0.538617341485635,-0.50233491230343,-0.499482648454923,-0.498106108188645,
-0.497032422355204,-0.495796556867449,-0.493618179733451,-0.483815567668126,
-0.434914230461427,-0.399786211719122,-0.395498602433246,-0.392959614744107,
-0.391019331782558,-0.388945197683011,-0.385692633640207,-0.37534745817258,
-0.358709933410719,-0.325788728069424,-0.307655482357201,-0.290153304075602,
-0.287476857138846,-0.286117435821882,-0.285045331244668,-0.283797813777857,
-0.281565897735133,-0.270936652621915,-0.247581560903225,-0.191918008431791,
-0.184489505918061,-0.181533193263817,-0.17972387503256,-0.177894703239262,
-0.175384812180395,-0.170035012739241,-0.162922483422438,-0.145434472534502,
-0.0957467128170975,-0.0781669160271442,-0.0754878194857416,-0.0747633067458267),
 .UNSPECIFIED.);
#885=B_SPLINE_CURVE_WITH_KNOTS('',3,(#87042,#87043,#87044,#87045,#87046,
#87047,#87048,#87049,#87050,#87051,#87052,#87053,#87054,#87055,#87056,#87057,
#87058,#87059,#87060,#87061,#87062,#87063,#87064,#87065,#87066,#87067,#87068,
#87069,#87070,#87071,#87072,#87073,#87074,#87075,#87076,#87077,#87078,#87079,
#87080,#87081,#87082,#87083,#87084,#87085,#87086,#87087,#87088,#87089,#87090,
#87091,#87092,#87093,#87094,#87095,#87096,#87097,#87098,#87099,#87100,#87101,
#87102,#87103,#87104,#87105,#87106,#87107,#87108,#87109,#87110,#87111,#87112,
#87113,#87114,#87115,#87116,#87117,#87118,#87119,#87120,#87121,#87122,#87123,
#87124,#87125,#87126,#87127,#87128,#87129,#87130,#87131,#87132,#87133,#87134,
#87135,#87136,#87137,#87138,#87139,#87140,#87141,#87142,#87143,#87144,#87145,
#87146,#87147,#87148,#87149,#87150,#87151,#87152,#87153,#87154,#87155,#87156,
#87157,#87158,#87159,#87160,#87161,#87162,#87163,#87164,#87165,#87166,#87167,
#87168,#87169,#87170,#87171,#87172,#87173,#87174,#87175,#87176,#87177,#87178,
#87179,#87180,#87181,#87182,#87183,#87184,#87185,#87186,#87187,#87188,#87189,
#87190,#87191,#87192,#87193,#87194,#87195,#87196,#87197,#87198,#87199,#87200,
#87201,#87202,#87203,#87204,#87205,#87206,#87207,#87208,#87209,#87210,#87211,
#87212,#87213,#87214,#87215,#87216,#87217,#87218,#87219,#87220,#87221,#87222,
#87223,#87224,#87225,#87226,#87227,#87228,#87229,#87230,#87231,#87232,#87233,
#87234,#87235,#87236,#87237,#87238,#87239,#87240,#87241,#87242,#87243,#87244,
#87245,#87246,#87247,#87248,#87249,#87250,#87251,#87252,#87253,#87254,#87255,
#87256,#87257,#87258,#87259,#87260,#87261,#87262,#87263,#87264,#87265,#87266,
#87267,#87268,#87269,#87270,#87271,#87272,#87273,#87274,#87275,#87276,#87277,
#87278,#87279,#87280,#87281,#87282,#87283,#87284,#87285,#87286,#87287,#87288,
#87289,#87290,#87291,#87292,#87293,#87294,#87295,#87296,#87297,#87298,#87299,
#87300,#87301,#87302,#87303,#87304,#87305,#87306,#87307,#87308,#87309,#87310,
#87311),.UNSPECIFIED.,.F.,.F.,(4,2,2,2,2,2,2,2,2,2,2,2,2,2,2,2,2,2,2,2,
2,2,2,2,2,2,2,2,2,2,2,2,2,2,2,2,2,2,2,2,2,2,2,2,2,2,2,2,2,2,2,2,2,2,2,2,
2,2,2,2,2,2,2,2,2,2,2,2,2,2,2,2,2,2,2,2,2,2,2,2,2,2,2,2,2,2,2,2,2,2,2,2,
2,2,2,2,2,2,2,2,2,2,2,2,2,2,2,2,2,2,2,2,2,2,2,2,2,2,2,2,2,2,2,2,2,2,2,2,
2,2,2,2,2,2,4),(-2.59336156192323,-2.57478143052137,-2.55593934383233,-2.54664458212764,
-2.54450174744568,-2.54327364423961,-2.54219865697171,-2.54080983467589,
-2.53789503501006,-2.50819909521878,-2.45775098895474,-2.44826218015948,
-2.44365500757166,-2.43987599389533,-2.43770533927899,-2.43768964522469,
-2.43767339861842,-2.4376565793801,-2.43763916662259,-2.4376211387297,-2.43760247330996,
-2.43758314717443,-2.4375631362795,-2.43754241572724,-2.43752095971209,
-2.43749874147679,-2.43747573263685,-2.43745569688231,-2.43743234721676,
-2.43740514153362,-2.43737345187315,-2.43733655193289,-2.43729360345781,
-2.43723939236148,-2.43529871969985,-2.43275677192872,-2.42845870417978,
-2.39333805620597,-2.34438012315355,-2.33468140182116,-2.33251030840455,
-2.33127611547429,-2.33020231057727,-2.32882355086259,-2.3259595807232,
-2.29000856849919,-2.25724261206533,-2.23468164815311,-2.22902810391243,
-2.22645693900437,-2.22451860391383,-2.22269203547157,-2.22015033129157,
-2.21351002015316,-2.15770272017822,-2.13364361485811,-2.12282133203953,
-2.12057750414133,-2.11932733480963,-2.11825542928027,-2.11689943314798,
-2.11475392602736,-2.10371704588551,-2.05250246420806,-2.02379370546777,
-2.01736014566069,-2.01465154303585,-2.01268993094642,-2.01089740094624,
-2.00803261471736,-2.00114866010443,-1.94807395082249,-1.92216817173204,
-1.91086149371006,-1.90858910201151,-1.90733273324799,-1.90626143377121,
-1.90491375171595,-1.90229224110401,-1.8862505578491,-1.8809612549938,-1.86637614080143,
-1.83348514191239,-1.81691872735997,-1.80660660076346,-1.80335773302879,
-1.80128435485331,-1.79934365526262,-1.79680250289913,-1.7925076421135,
-1.75739675969618,-1.708494036339,-1.69872315354024,-1.69654695124879,-1.69531155671128,
-1.69423779681118,-1.69286052051344,-1.69000454240626,-1.66720803090501,
-1.61159834211153,-1.59558698556985,-1.59181759916656,-1.58962918187653,
-1.58771503082604,-1.58534582137417,-1.58171257528808,-1.56461629029267,
-1.55654719992905,-1.52173742237,-1.49768870195535,-1.48686947392944,-1.4846259238267,
-1.48337585942629,-1.48230401313248,-1.48094805250604,-1.47828783658503,
-1.46123461091314,-1.44262325791515,-1.40966792875342,-1.39302313838362,
-1.38267571410956,-1.37942287949061,-1.37734868383741,-1.37540842168779,
-1.37286957539999,-1.36858249232163,-1.3340022010121,-1.27803793126164,
-1.27376421689344,-1.27209268463666,-1.27108068241409,-1.26997837560242,
-1.26841349788512,-1.26450107762448,-1.2598478307819),.UNSPECIFIED.);
#886=B_SPLINE_CURVE_WITH_KNOTS('',3,(#87317,#87318,#87319,#87320,#87321,
#87322,#87323,#87324,#87325,#87326,#87327,#87328,#87329,#87330,#87331,#87332,
#87333,#87334),.UNSPECIFIED.,.F.,.F.,(4,2,2,2,2,2,2,2,4),(-0.0751187453612548,
-0.0651105012340861,-0.06037386076549,-0.0579480733786947,-0.0560290630418665,
-0.0538783933071959,-0.0516516907416782,-0.0483298715753922,-0.000628983619687466),
 .UNSPECIFIED.);
#887=B_SPLINE_CURVE_WITH_KNOTS('',3,(#87335,#87336,#87337,#87338,#87339,
#87340,#87341,#87342,#87343,#87344,#87345,#87346,#87347,#87348,#87349,#87350,
#87351,#87352,#87353,#87354,#87355,#87356,#87357,#87358,#87359,#87360,#87361,
#87362,#87363,#87364,#87365,#87366,#87367,#87368,#87369,#87370,#87371,#87372,
#87373,#87374,#87375,#87376,#87377,#87378,#87379,#87380,#87381,#87382,#87383,
#87384,#87385,#87386,#87387,#87388,#87389,#87390,#87391,#87392,#87393,#87394,
#87395,#87396,#87397,#87398,#87399,#87400,#87401,#87402,#87403,#87404,#87405,
#87406,#87407,#87408,#87409,#87410,#87411,#87412,#87413,#87414,#87415,#87416,
#87417,#87418,#87419,#87420,#87421,#87422,#87423,#87424,#87425,#87426,#87427,
#87428,#87429,#87430,#87431,#87432,#87433,#87434,#87435,#87436,#87437,#87438,
#87439,#87440,#87441,#87442,#87443,#87444,#87445,#87446,#87447,#87448,#87449,
#87450,#87451,#87452,#87453,#87454,#87455,#87456,#87457,#87458,#87459,#87460,
#87461,#87462,#87463,#87464,#87465,#87466,#87467,#87468,#87469,#87470,#87471,
#87472,#87473,#87474,#87475,#87476,#87477,#87478,#87479,#87480,#87481,#87482,
#87483,#87484,#87485,#87486,#87487,#87488,#87489,#87490,#87491,#87492,#87493,
#87494,#87495,#87496,#87497,#87498,#87499,#87500,#87501,#87502,#87503,#87504,
#87505,#87506,#87507,#87508,#87509,#87510,#87511,#87512,#87513,#87514,#87515,
#87516,#87517,#87518,#87519,#87520,#87521,#87522,#87523,#87524,#87525,#87526,
#87527,#87528,#87529,#87530,#87531,#87532,#87533,#87534,#87535,#87536,#87537,
#87538,#87539,#87540,#87541,#87542,#87543,#87544,#87545,#87546,#87547,#87548,
#87549,#87550,#87551,#87552,#87553,#87554,#87555,#87556),.UNSPECIFIED.,
 .F.,.F.,(4,2,2,2,2,2,2,2,2,2,2,2,2,2,2,2,2,2,2,2,2,2,2,2,2,2,2,2,2,2,2,
2,2,2,2,2,2,2,2,2,2,2,2,2,2,2,2,2,2,2,2,2,2,2,2,2,2,2,2,2,2,2,2,2,2,2,2,
2,2,2,2,2,2,2,2,2,2,2,2,2,2,2,2,2,2,2,2,2,2,2,2,2,2,2,2,2,2,2,2,2,2,2,2,
2,2,2,2,2,2,2,4),(-2.66770883390819,-2.62475437947397,-2.62182039698666,
-2.62013764316661,-2.61863271120716,-2.61754110563343,-2.61651378655355,
-2.61476419075559,-2.60998994102848,-2.57253353119947,-2.55111147084882,
-2.52277528452494,-2.5163024293871,-2.51417823115161,-2.51209832105435,
-2.51015950891412,-2.50763229531544,-2.50338650214394,-2.47116894427638,
-2.43568387162433,-2.41824496460406,-2.40942522411099,-2.4073250254246,
-2.40609673682713,-2.40502162768412,-2.40363270124937,-2.40071787126955,
-2.37055198924443,-2.31898104760483,-2.31037045964199,-2.30414811920189,
-2.30144314075866,-2.29948181255181,-2.29768792960418,-2.29481746895974,
-2.28790168012843,-2.23521529940548,-2.20902243734717,-2.19764164563069,
-2.1953645979624,-2.19410702490264,-2.1930355290242,-2.19168865638841,-2.18907182343594,
-2.17312088523044,-2.16870947085322,-2.1212960017337,-2.09763170555318,
-2.09182996308736,-2.08923137140871,-2.08728831601194,-2.08546889697837,
-2.08295556451277,-2.07649410279332,-2.01901926601932,-2.01352901529623,
-1.99464804991438,-1.98534047415626,-1.98319650409771,-1.98196804304497,
-1.9808929335475,-1.97950420539227,-1.97659049297645,-1.94574484197275,
-1.91160705879477,-1.89279440974746,-1.88149507036608,-1.87813705797889,
-1.87603926792662,-1.87410658231444,-1.87161933169763,-1.86751013870077,
-1.84101288018382,-1.7987996740724,-1.78190320528097,-1.77324605356108,
-1.77115096679496,-1.76993330747051,-1.76885618478708,-1.76747291670273,
-1.76518837826371,-1.75160543176326,-1.74979161422262,-1.70241888116661,
-1.67144365740888,-1.66699164886286,-1.66465602632956,-1.66274353610972,
-1.66052856524602,-1.65674101830539,-1.64214654861088,-1.62988100369963,
-1.58946989164561,-1.57061614481818,-1.56131733084317,-1.55917404804256,
-1.55794576633558,-1.55687067391552,-1.55548178319651,-1.5525670779959,
-1.52372979537384,-1.48561863062846,-1.46809306001602,-1.45735195754653,
-1.45405428450517,-1.45196987343531,-1.45003278989325,-1.44751625700801,
-1.44330699841092,-1.41283233438342,-1.4084593254711),.UNSPECIFIED.);
#888=B_SPLINE_CURVE_WITH_KNOTS('',3,(#87558,#87559,#87560,#87561,#87562,
#87563,#87564,#87565,#87566,#87567,#87568,#87569,#87570,#87571,#87572,#87573,
#87574,#87575,#87576,#87577,#87578,#87579,#87580,#87581,#87582,#87583,#87584,
#87585,#87586,#87587,#87588,#87589,#87590,#87591,#87592,#87593,#87594,#87595,
#87596,#87597,#87598,#87599,#87600,#87601,#87602,#87603,#87604,#87605,#87606,
#87607,#87608,#87609,#87610,#87611,#87612,#87613,#87614,#87615,#87616,#87617,
#87618,#87619,#87620,#87621,#87622,#87623,#87624,#87625,#87626,#87627,#87628,
#87629,#87630,#87631,#87632,#87633,#87634,#87635,#87636,#87637,#87638,#87639,
#87640,#87641,#87642,#87643,#87644,#87645,#87646,#87647,#87648,#87649,#87650,
#87651,#87652,#87653,#87654,#87655,#87656,#87657,#87658,#87659,#87660,#87661,
#87662,#87663,#87664,#87665,#87666,#87667,#87668,#87669,#87670,#87671,#87672,
#87673,#87674,#87675,#87676,#87677,#87678,#87679,#87680,#87681,#87682,#87683,
#87684,#87685,#87686,#87687,#87688,#87689,#87690,#87691,#87692,#87693,#87694,
#87695,#87696,#87697,#87698,#87699,#87700,#87701,#87702,#87703,#87704,#87705,
#87706,#87707,#87708,#87709,#87710,#87711,#87712,#87713,#87714,#87715,#87716,
#87717,#87718,#87719,#87720,#87721,#87722,#87723,#87724,#87725,#87726,#87727,
#87728,#87729,#87730,#87731,#87732,#87733,#87734,#87735,#87736,#87737,#87738,
#87739,#87740,#87741,#87742,#87743,#87744,#87745,#87746,#87747,#87748,#87749,
#87750,#87751,#87752,#87753,#87754,#87755,#87756,#87757,#87758,#87759,#87760,
#87761,#87762,#87763,#87764,#87765,#87766,#87767,#87768,#87769,#87770,#87771,
#87772,#87773,#87774,#87775,#87776,#87777,#87778,#87779,#87780,#87781,#87782,
#87783,#87784,#87785,#87786,#87787,#87788,#87789,#87790,#87791,#87792,#87793,
#87794,#87795,#87796,#87797,#87798,#87799,#87800,#87801,#87802,#87803,#87804,
#87805,#87806,#87807,#87808,#87809,#87810,#87811,#87812,#87813,#87814,#87815,
#87816,#87817,#87818,#87819,#87820,#87821,#87822,#87823,#87824,#87825,#87826,
#87827,#87828,#87829),.UNSPECIFIED.,.F.,.F.,(4,2,2,2,2,2,2,2,2,2,2,2,2,
2,2,2,2,2,2,2,2,2,2,2,2,2,2,2,2,2,2,2,2,2,2,2,2,2,2,2,2,2,2,2,2,2,2,2,2,
2,2,2,2,2,2,2,2,2,2,2,2,2,2,2,2,2,2,2,2,2,2,2,2,2,2,2,2,2,2,2,2,2,2,2,2,
2,2,2,2,2,2,2,2,2,2,2,2,2,2,2,2,2,2,2,2,2,2,2,2,2,2,2,2,2,2,2,2,2,2,2,2,
2,2,2,2,2,2,2,2,2,2,2,2,2,2,4),(-1.2598478307819,-1.24528929234835,-1.1889169518329,
-1.17207227593167,-1.16845566072013,-1.16609162636776,-1.16417788367051,
-1.16198579247119,-1.15819960366846,-1.14195347226029,-1.08448120487193,
-1.07950865620043,-1.0635235292766,-1.06090524041075,-1.05955822062563,
-1.05848692416541,-1.05722995783808,-1.05495494653949,-1.04360421005489,
-1.01752345922582,-0.964653835092965,-0.957751193963408,-0.954883266774759,
-0.953090119321,-0.951128920320106,-0.948422876009794,-0.942004785276161,
-0.91343052938435,-0.862235796005543,-0.85107622247357,-0.848923187726734,
-0.847564892259753,-0.846492810145333,-0.845244325579734,-0.843008214191392,
-0.832312720154088,-0.808717499380194,-0.752157189499822,-0.74559191523724,
-0.743062108439144,-0.741238682966653,-0.73929868715275,-0.736716775439302,
-0.731004511911674,-0.708010054349212,-0.674995329328759,-0.65397405074336,
-0.639432548045239,-0.637102678852817,-0.635706346157752,-0.634627890714361,
-0.633418611436055,-0.631359981455373,-0.623149413636835,-0.607538527463072,
-0.565819259417715,-0.537126733153774,-0.532961633694862,-0.530458475445625,
-0.52852400770821,-0.526434805620254,-0.523113253335846,-0.512147136109772,
-0.494107901067988,-0.443946508571429,-0.427608372243173,-0.424975729079608,
-0.42362570905684,-0.422554323276223,-0.42129990873719,-0.419036243486443,
-0.407878555369356,-0.382547883822278,-0.328603155968634,-0.32178776827569,
-0.318934408159038,-0.317144042427059,-0.315180779553109,-0.312462489029747,
-0.30597053637577,-0.29698364226265,-0.245936659350276,-0.215997823684719,
-0.213149026927364,-0.211767348847781,-0.210714957827224,-0.210704912418351,
-0.210695176616752,-0.210685727169198,-0.210676543231602,-0.210667605835312,
-0.210658897893402,-0.210650403950862,-0.210642109808122,-0.210634002554713,
-0.210626070366007,-0.210618302312035,-0.210610688405847,-0.210603219397911,
-0.210595886676978,-0.21058868220452,-0.210581598612733,-0.210574629069274,
-0.210567767032783,-0.210561006531983,-0.210554341949679,-0.2105477679807,
-0.210541279592807,-0.210534872074776,-0.21052854103106,-0.21052228227184,
-0.210516091863237,-0.210509966007037,-0.210503901164927,-0.210497893989959,
-0.210491941191575,-0.210486039768665,-0.210480186773141,-0.210474379385115,
-0.209210206527847,-0.206817809032165,-0.193151295846991,-0.156400889779779,
-0.113382385035125,-0.109096409479968,-0.106558041419045,-0.104618031374231,
-0.102543994241103,-0.0992911748388577,-0.0889417362901918,-0.0722940605167449,
-0.0417947654359074,-0.00539400818564538,-0.00193479222001944,-0.000864069735648079,
-0.000629066024222938),.UNSPECIFIED.);
#889=B_SPLINE_CURVE_WITH_KNOTS('',3,(#87830,#87831,#87832,#87833,#87834,
#87835,#87836,#87837,#87838,#87839,#87840,#87841,#87842,#87843,#87844,#87845),
 .UNSPECIFIED.,.F.,.F.,(4,3,3,3,3,4),(-28.973780262141,-28.9662570488944,
-28.8628842312553,-28.7596459044043,-28.6565264336762,-28.6232428001367),
 .UNSPECIFIED.);
#890=B_SPLINE_CURVE_WITH_KNOTS('',3,(#87850,#87851,#87852,#87853,#87854,
#87855,#87856,#87857,#87858,#87859,#87860,#87861,#87862,#87863,#87864,#87865,
#87866,#87867,#87868,#87869,#87870,#87871,#87872,#87873,#87874,#87875,#87876,
#87877,#87878,#87879,#87880,#87881,#87882,#87883,#87884,#87885,#87886,#87887,
#87888,#87889,#87890,#87891,#87892,#87893,#87894,#87895,#87896,#87897,#87898,
#87899,#87900,#87901,#87902,#87903,#87904,#87905,#87906,#87907,#87908,#87909,
#87910,#87911,#87912,#87913,#87914,#87915,#87916,#87917,#87918,#87919,#87920,
#87921,#87922,#87923,#87924,#87925,#87926,#87927,#87928,#87929,#87930,#87931,
#87932,#87933,#87934,#87935,#87936,#87937,#87938,#87939,#87940,#87941,#87942,
#87943,#87944,#87945,#87946,#87947,#87948,#87949,#87950,#87951,#87952,#87953,
#87954,#87955,#87956,#87957,#87958,#87959,#87960,#87961,#87962,#87963,#87964,
#87965,#87966,#87967,#87968,#87969,#87970,#87971,#87972,#87973,#87974,#87975,
#87976,#87977,#87978,#87979,#87980,#87981,#87982,#87983,#87984,#87985,#87986,
#87987,#87988,#87989,#87990,#87991,#87992,#87993,#87994,#87995,#87996,#87997,
#87998,#87999,#88000,#88001,#88002,#88003,#88004,#88005,#88006,#88007,#88008,
#88009,#88010,#88011,#88012,#88013,#88014,#88015,#88016,#88017,#88018,#88019,
#88020,#88021,#88022,#88023,#88024,#88025,#88026,#88027,#88028,#88029,#88030,
#88031,#88032,#88033,#88034,#88035,#88036,#88037,#88038,#88039,#88040,#88041,
#88042,#88043,#88044,#88045,#88046,#88047,#88048,#88049,#88050,#88051,#88052,
#88053,#88054,#88055,#88056,#88057,#88058,#88059,#88060,#88061,#88062,#88063,
#88064,#88065,#88066,#88067,#88068,#88069,#88070,#88071,#88072,#88073,#88074,
#88075,#88076,#88077,#88078,#88079),.UNSPECIFIED.,.F.,.F.,(4,2,2,2,2,2,
2,2,2,2,2,2,2,2,2,2,2,2,2,2,2,2,2,2,2,2,2,2,2,2,2,2,2,2,2,2,2,2,2,2,2,2,
2,2,2,2,2,2,2,2,2,2,2,2,2,2,2,2,2,2,2,2,2,2,2,2,2,2,2,2,2,2,2,2,2,2,2,2,
2,2,2,2,2,2,2,2,2,2,2,2,2,2,2,2,2,2,2,2,2,2,2,2,2,2,2,2,2,2,2,2,2,2,2,2,
4),(-1.40850153180492,-1.36250266792624,-1.34494718878491,-1.33419300667973,
-1.33089396069365,-1.32880929375025,-1.32687239494307,-1.32431321406307,
-1.31872670134852,-1.31130334259201,-1.29270174146163,-1.24997366761145,
-1.2273458145331,-1.22449368388517,-1.2231170476229,-1.22204321147614,-1.22080708773443,
-1.21862805117604,-1.20881907582038,-1.15991453630915,-1.12479584722585,
-1.12050022469114,-1.11795871973547,-1.11601779643587,-1.11394422253493,
-1.11069513726152,-1.10038298714613,-1.08381947663768,-1.05095674662274,
-1.03712853846431,-1.03047927309802,-1.01500557839671,-1.01240852061588,
-1.01106603294309,-1.00999495536059,-1.00873430560225,-1.00644253944657,
-0.994796209914545,-0.967531040131002,-0.947346484138139,-0.912838732964867,
-0.908552107360215,-0.906013234804672,-0.904072770255018,-0.90199818027652,
-0.898744353772751,-0.888390524142,-0.871734651222027,-0.838795741074562,
-0.82007236579395,-0.803159000758074,-0.800503827905399,-0.799148848740516,
-0.798076953647933,-0.796825889660074,-0.79457817768722,-0.783693760074211,
-0.759401953478156,-0.703899695701145,-0.697224656244714,-0.694677436365725,
-0.692849337799291,-0.690911613820067,-0.688345046551784,-0.682716977631982,
-0.67522336157879,-0.65636360023919,-0.626448513375451,-0.604721939855228,
-0.590952696337158,-0.588659664226564,-0.587274112310235,-0.586196990964432,
-0.584981347491901,-0.582894265567584,-0.57433331247896,-0.557714673050792,
-0.51552930042313,-0.48862337974378,-0.484504558176909,-0.482014905507422,
-0.480082380799827,-0.477986794396815,-0.474636721032121,-0.463405649177908,
-0.444752960510814,-0.416482353160889,-0.379486197159405,-0.376648554453402,
-0.375274992402946,-0.374201702432199,-0.372964110749879,-0.370777445489433,
-0.361223097587746,-0.312152855856071,-0.276986607863795,-0.272691418201515,
-0.270150396569206,-0.268209973218679,-0.26613706028445,-0.262889275515635,
-0.25277870278595,-0.236574232997193,-0.198328815996906,-0.167652335617237,
-0.164739946834172,-0.163351838439206,-0.16227719980241,-0.161049276032689,
-0.159757267485298,-0.155110071347819,-0.128864883232683,-0.106990879308478,
-0.105559660604484,-0.0751187453612548),.UNSPECIFIED.);
#891=B_SPLINE_CURVE_WITH_KNOTS('',3,(#88081,#88082,#88083,#88084,#88085,
#88086,#88087,#88088,#88089,#88090,#88091,#88092,#88093,#88094,#88095,#88096,
#88097,#88098,#88099,#88100,#88101,#88102,#88103,#88104,#88105,#88106,#88107,
#88108,#88109,#88110,#88111,#88112,#88113,#88114,#88115,#88116,#88117,#88118,
#88119,#88120,#88121,#88122,#88123,#88124,#88125,#88126,#88127,#88128,#88129,
#88130,#88131,#88132,#88133,#88134,#88135,#88136,#88137,#88138,#88139,#88140,
#88141,#88142,#88143,#88144,#88145,#88146,#88147,#88148,#88149,#88150,#88151,
#88152,#88153,#88154,#88155,#88156,#88157,#88158,#88159,#88160,#88161,#88162,
#88163,#88164,#88165,#88166,#88167,#88168,#88169,#88170,#88171,#88172,#88173,
#88174,#88175,#88176,#88177,#88178,#88179,#88180,#88181,#88182,#88183,#88184,
#88185,#88186,#88187,#88188,#88189,#88190,#88191,#88192,#88193,#88194,#88195,
#88196,#88197,#88198,#88199,#88200,#88201,#88202,#88203,#88204,#88205,#88206,
#88207,#88208,#88209,#88210,#88211,#88212,#88213,#88214,#88215,#88216,#88217,
#88218,#88219,#88220,#88221,#88222,#88223,#88224,#88225,#88226,#88227,#88228,
#88229,#88230,#88231,#88232,#88233,#88234,#88235,#88236,#88237,#88238,#88239,
#88240,#88241,#88242,#88243,#88244,#88245,#88246,#88247,#88248,#88249,#88250,
#88251,#88252,#88253,#88254,#88255,#88256,#88257,#88258,#88259,#88260,#88261),
 .UNSPECIFIED.,.F.,.F.,(4,3,3,3,3,3,3,3,3,3,3,3,3,3,3,3,3,3,3,3,3,3,3,3,
3,3,3,3,3,3,3,3,3,3,3,3,3,3,3,3,3,3,3,3,3,3,3,3,3,3,3,3,3,3,3,3,3,3,3,3,
4),(-28.6232428001367,-28.5202020676114,-28.4171817229006,-28.3141477785777,
-28.2110001876892,-28.1077864190661,-28.0043998217136,-27.9674205989325,
-27.864025861899,-27.7607845797985,-27.657664614421,-27.554610046227,-27.4515868378843,
-27.348560995227,-27.245428228464,-27.1422391370694,-27.0388671437028,-26.9685841489706,
-26.8651894118465,-26.7619481296552,-26.6588281641867,-26.5557735959016,
-26.452750387468,-26.3497245447198,-26.2465917778671,-26.1434026863831,
-26.0400306929288,-25.9697476990087,-25.8663529620659,-25.7631116800558,
-25.6599917147673,-25.5569371466616,-25.4539139384064,-25.3508880958353,
-25.2477553291566,-25.1445662378452,-25.0411942445592,-24.9709112490469,
-24.8675165120623,-24.764275230012,-24.6611552646861,-24.5581006965446,
-24.4550774882552,-24.3520516456518,-24.2489188789436,-24.1457297876041,
-24.0423577942929,-23.972074799085,-23.8686800615146,-23.7654387788755,
-23.6623188129591,-23.5592642442264,-23.4562410353459,-23.3532151921524,
-23.2500824248597,-23.146893332938,-23.0435213390546,-22.9732383491231,
-22.8444301460866,-22.7177283293138,-22.6905949549614),.UNSPECIFIED.);
#892=B_SPLINE_CURVE_WITH_KNOTS('',3,(#88262,#88263,#88264,#88265),
 .UNSPECIFIED.,.F.,.F.,(4,4),(-22.6905949549614,-22.3411472771506),
 .UNSPECIFIED.);
#893=B_SPLINE_CURVE_WITH_KNOTS('',3,(#88271,#88272,#88273,#88274,#88275,
#88276,#88277,#88278,#88279,#88280,#88281,#88282,#88283,#88284,#88285,#88286,
#88287,#88288),.UNSPECIFIED.,.F.,.F.,(4,2,2,2,2,2,2,2,4),(-0.0747374473528612,
-0.04412382595158,-0.0412117156485017,-0.0398236209285753,-0.0387489379637731,
-0.0375209019896154,-0.036228756208033,-0.0342507643538522,-0.000628700947229318),
 .UNSPECIFIED.);
#894=B_SPLINE_CURVE_WITH_KNOTS('',3,(#88289,#88290,#88291,#88292,#88293,
#88294,#88295,#88296,#88297,#88298,#88299,#88300,#88301,#88302,#88303,#88304,
#88305,#88306,#88307,#88308,#88309,#88310,#88311,#88312,#88313,#88314,#88315,
#88316,#88317,#88318,#88319,#88320,#88321,#88322,#88323,#88324,#88325,#88326,
#88327,#88328,#88329,#88330,#88331,#88332,#88333,#88334,#88335,#88336,#88337,
#88338,#88339,#88340,#88341,#88342,#88343,#88344,#88345,#88346,#88347,#88348,
#88349,#88350,#88351,#88352,#88353,#88354,#88355,#88356,#88357,#88358,#88359,
#88360,#88361,#88362,#88363,#88364,#88365,#88366,#88367,#88368,#88369,#88370,
#88371,#88372,#88373,#88374,#88375,#88376,#88377,#88378,#88379,#88380,#88381,
#88382,#88383,#88384,#88385,#88386,#88387,#88388,#88389,#88390,#88391,#88392,
#88393,#88394,#88395,#88396,#88397,#88398,#88399,#88400,#88401,#88402,#88403,
#88404,#88405,#88406,#88407,#88408,#88409,#88410,#88411,#88412,#88413,#88414,
#88415,#88416,#88417,#88418,#88419,#88420,#88421,#88422,#88423,#88424,#88425,
#88426,#88427,#88428,#88429,#88430,#88431,#88432,#88433,#88434,#88435,#88436,
#88437,#88438,#88439,#88440,#88441,#88442,#88443,#88444,#88445,#88446,#88447,
#88448,#88449,#88450,#88451,#88452,#88453,#88454,#88455,#88456,#88457,#88458,
#88459,#88460,#88461,#88462,#88463,#88464,#88465,#88466,#88467,#88468,#88469,
#88470,#88471,#88472,#88473,#88474,#88475,#88476,#88477,#88478,#88479,#88480,
#88481,#88482,#88483,#88484,#88485,#88486,#88487,#88488,#88489,#88490,#88491,
#88492,#88493,#88494,#88495,#88496,#88497,#88498,#88499,#88500,#88501,#88502,
#88503,#88504,#88505,#88506,#88507,#88508),.UNSPECIFIED.,.F.,.F.,(4,2,2,
2,2,2,2,2,2,2,2,2,2,2,2,2,2,2,2,2,2,2,2,2,2,2,2,2,2,2,2,2,2,2,2,2,2,2,2,
2,2,2,2,2,2,2,2,2,2,2,2,2,2,2,2,2,2,2,2,2,2,2,2,2,2,2,2,2,2,2,2,2,2,2,2,
2,2,2,2,2,2,2,2,2,2,2,2,2,2,2,2,2,2,2,2,2,2,2,2,2,2,2,2,2,2,2,2,2,2,4),
(-2.66802904969001,-2.63755774389658,-2.6110418457987,-2.60487466067178,
-2.60221136333042,-2.60025753768377,-2.59845461781743,-2.59553444665161,
-2.58831963533694,-2.54291704431415,-2.52278593755294,-2.50657158531799,
-2.49817521853025,-2.49612782426245,-2.49489968701426,-2.49382468719195,
-2.49243587130156,-2.48952116456729,-2.45949023876327,-2.40819232067015,
-2.39936297756314,-2.39296024987529,-2.39025661551927,-2.38829568401878,
-2.38650176556769,-2.38363037935178,-2.37670786679604,-2.324126944789,-2.29786687814242,
-2.28646960463217,-2.28419178777279,-2.28293412750553,-2.28186276177362,
-2.28051631274538,-2.27790106567353,-2.26197752629999,-2.25748987063338,
-2.21495986223702,-2.18434884153593,-2.17990718751521,-2.17757390691457,
-2.17566176417161,-2.17344542745107,-2.16965122176219,-2.15497798465485,
-2.14272683561657,-2.10721237745275,-2.08476869321325,-2.07439290602801,
-2.07217670138004,-2.07093249920516,-2.06985983366734,-2.0684952881174,
-2.06579533980039,-2.04761467920952,-2.02952801031757,-1.99679796239865,
-1.97429793992573,-1.96865218839525,-1.96608218613366,-1.96414375748969,
-1.96231638762754,-1.9597724228585,-1.9531193589139,-1.8974130695201,-1.87327725586826,
-1.86243353454152,-1.86018812810855,-1.85893748043094,-1.85786541198845,
-1.85650952682316,-1.85436478916682,-1.84334447379542,-1.79204460878004,
-1.76337818485223,-1.75694913947586,-1.75424101398548,-1.75227923067451,
-1.75048618869259,-1.74761981083507,-1.74072802435933,-1.68773031081081,
-1.66175996773514,-1.65043601167667,-1.64816234295048,-1.64690556307631,
-1.645834092069,-1.64448642212537,-1.64186560534487,-1.62583988317903,-1.62044303705025,
-1.60593861968782,-1.57304280848175,-1.5502861793192,-1.54460557757692,
-1.54202907056096,-1.5400895318011,-1.53826389985079,-1.53572681601022,
-1.52911815609688,-1.47296827102802,-1.44911913430193,-1.43835263235197,
-1.43611180790494,-1.43486210661223,-1.43378985815367,-1.43243247262926,
-1.42976671205318,-1.41257999831609,-1.40850153180492),.UNSPECIFIED.);
#895=B_SPLINE_CURVE_WITH_KNOTS('',3,(#88510,#88511,#88512,#88513,#88514,
#88515,#88516,#88517,#88518,#88519),.UNSPECIFIED.,.F.,.F.,(4,1,1,1,1,1,
1,4),(-22.3411472771506,-21.9744018991612,-20.9755654491994,-19.9767289992375,
-18.9778925492756,-17.9790560993137,-16.9802196493519,-16.4074096477818),
 .UNSPECIFIED.);
#896=B_SPLINE_CURVE_WITH_KNOTS('',3,(#88520,#88521,#88522,#88523,#88524,
#88525),.UNSPECIFIED.,.F.,.F.,(4,2,4),(-2.66742168930548,-2.60891632352633,
-2.59315595267277),.UNSPECIFIED.);
#897=B_SPLINE_CURVE_WITH_KNOTS('',3,(#88530,#88531,#88532,#88533,#88534,
#88535,#88536,#88537,#88538,#88539,#88540,#88541,#88542,#88543,#88544,#88545,
#88546,#88547,#88548,#88549,#88550,#88551,#88552,#88553,#88554,#88555,#88556,
#88557,#88558,#88559,#88560,#88561,#88562,#88563,#88564,#88565,#88566,#88567,
#88568,#88569,#88570,#88571,#88572,#88573,#88574,#88575,#88576,#88577,#88578,
#88579,#88580,#88581,#88582,#88583,#88584,#88585,#88586,#88587,#88588,#88589,
#88590,#88591,#88592,#88593,#88594,#88595,#88596,#88597,#88598,#88599,#88600,
#88601,#88602,#88603,#88604,#88605,#88606,#88607,#88608,#88609,#88610,#88611,
#88612,#88613,#88614,#88615,#88616,#88617,#88618,#88619,#88620,#88621,#88622,
#88623,#88624,#88625,#88626,#88627,#88628,#88629,#88630,#88631,#88632,#88633,
#88634,#88635,#88636,#88637,#88638,#88639,#88640,#88641,#88642,#88643,#88644,
#88645,#88646,#88647,#88648,#88649,#88650,#88651,#88652,#88653,#88654,#88655,
#88656,#88657,#88658,#88659,#88660,#88661,#88662,#88663,#88664,#88665,#88666,
#88667,#88668,#88669,#88670,#88671,#88672,#88673,#88674,#88675,#88676,#88677,
#88678,#88679,#88680,#88681,#88682,#88683,#88684,#88685,#88686,#88687,#88688,
#88689,#88690,#88691,#88692,#88693,#88694,#88695,#88696,#88697,#88698,#88699,
#88700,#88701,#88702,#88703,#88704,#88705,#88706,#88707,#88708,#88709,#88710,
#88711,#88712,#88713,#88714,#88715,#88716,#88717,#88718,#88719,#88720,#88721,
#88722,#88723,#88724,#88725,#88726,#88727,#88728,#88729,#88730,#88731,#88732,
#88733,#88734,#88735,#88736,#88737,#88738,#88739,#88740,#88741,#88742,#88743,
#88744,#88745,#88746,#88747,#88748,#88749,#88750,#88751,#88752,#88753,#88754,
#88755,#88756,#88757),.UNSPECIFIED.,.F.,.F.,(4,2,2,2,2,2,2,2,2,2,2,2,2,
2,2,2,2,2,2,2,2,2,2,2,2,2,2,2,2,2,2,2,2,2,2,2,2,2,2,2,2,2,2,2,2,2,2,2,2,
2,2,2,2,2,2,2,2,2,2,2,2,2,2,2,2,2,2,2,2,2,2,2,2,2,2,2,2,2,2,2,2,2,2,2,2,
2,2,2,2,2,2,2,2,2,2,2,2,2,2,2,2,2,2,2,2,2,2,2,2,2,2,2,2,4),(-1.40833650609706,
-1.3649437306449,-1.33389381709473,-1.31584387047142,-1.31314824084025,
-1.31178459144683,-1.31071196445864,-1.30946704779559,-1.30724773180197,
-1.29682452600705,-1.27421113791659,-1.21608710496737,-1.20970344861157,
-1.20720318981174,-1.20538733098271,-1.20344254810514,-1.20083203889336,
-1.19496299129987,-1.1707865138568,-1.12030328273454,-1.11987263331321,
-1.10368575152951,-1.10105877473431,-1.09970982450841,-1.09863833001689,
-1.09738268167455,-1.09511396777183,-1.08387445595086,-1.05823025922132,
-1.00472618569253,-0.997872335794782,-0.995012325098936,-0.993220533540396,
-0.991257922917696,-0.988544613707199,-0.982084031750929,-0.928143104171845,
-0.891939834625717,-0.889085064613198,-0.887708000231669,-0.886634227682866,
-0.885398626158178,-0.883221586824627,-0.873439475014806,-0.824518597785424,
-0.789396346049497,-0.785101093367893,-0.782559837634135,-0.780619122208955,
-0.778545787427025,-0.775297112459875,-0.764986566013361,-0.748425920597504,
-0.715567628486558,-0.701829267242749,-0.694974244682334,-0.694646738812136,
-0.688836527048918,-0.679050447296629,-0.676987308449316,-0.675656580996106,
-0.674586232869739,-0.673316269086304,-0.670980995979987,-0.658511789946157,
-0.601784247668701,-0.592637781831421,-0.576122516071506,-0.572529065390159,
-0.570172304108043,-0.568259201161152,-0.566062052669969,-0.562252383520181,
-0.545669852662471,-0.485258319331414,-0.46770889562479,-0.46503072363384,
-0.463670913620932,-0.462598753705616,-0.461351460183848,-0.459120655746634,
-0.448509962292842,-0.425222459498542,-0.368183702264911,-0.3616740559574,
-0.359153296358345,-0.357332297268636,-0.355391083321029,-0.352801024332959,
-0.347043664672101,-0.298622221255579,-0.296632139941095,-0.277730750328994,
-0.271008271974131,-0.255576068838208,-0.253209102980117,-0.251801933881499,
-0.250722003063835,-0.24951870369754,-0.247527743032982,-0.240021742540941,
-0.226283927436843,-0.195002955852307,-0.180519452277464,-0.153157428159492,
-0.149027139595264,-0.146534157834852,-0.144601186953499,-0.142507252777016,
-0.139164453911593,-0.128001196418437,-0.0983529125791534,-0.0750367835752176,
-0.0747374473528612),.UNSPECIFIED.);
#898=B_SPLINE_CURVE_WITH_KNOTS('',3,(#88758,#88759,#88760,#88761,#88762,
#88763,#88764,#88765,#88766,#88767,#88768,#88769,#88770,#88771,#88772,#88773,
#88774,#88775,#88776,#88777,#88778,#88779,#88780,#88781,#88782,#88783,#88784,
#88785,#88786,#88787,#88788,#88789,#88790,#88791,#88792,#88793,#88794,#88795,
#88796,#88797,#88798,#88799,#88800,#88801,#88802,#88803,#88804,#88805,#88806,
#88807,#88808,#88809,#88810,#88811,#88812,#88813,#88814,#88815,#88816,#88817,
#88818,#88819,#88820,#88821,#88822,#88823,#88824,#88825,#88826,#88827,#88828,
#88829,#88830,#88831,#88832,#88833,#88834,#88835,#88836,#88837,#88838,#88839,
#88840,#88841,#88842,#88843,#88844,#88845,#88846,#88847,#88848,#88849,#88850,
#88851,#88852,#88853,#88854,#88855,#88856,#88857,#88858,#88859,#88860,#88861,
#88862,#88863,#88864,#88865,#88866,#88867,#88868,#88869,#88870,#88871,#88872,
#88873,#88874,#88875,#88876,#88877,#88878,#88879,#88880,#88881,#88882,#88883,
#88884,#88885,#88886,#88887,#88888,#88889,#88890,#88891,#88892,#88893,#88894,
#88895,#88896,#88897,#88898,#88899,#88900,#88901,#88902,#88903,#88904,#88905,
#88906,#88907,#88908,#88909,#88910,#88911,#88912,#88913,#88914,#88915,#88916,
#88917,#88918,#88919,#88920,#88921,#88922,#88923,#88924,#88925,#88926,#88927,
#88928,#88929,#88930,#88931,#88932,#88933,#88934,#88935,#88936,#88937,#88938,
#88939,#88940,#88941,#88942,#88943,#88944,#88945,#88946,#88947,#88948,#88949,
#88950,#88951,#88952,#88953,#88954,#88955,#88956,#88957,#88958,#88959,#88960,
#88961,#88962,#88963,#88964,#88965,#88966,#88967,#88968,#88969,#88970,#88971,
#88972,#88973,#88974,#88975,#88976,#88977,#88978,#88979,#88980,#88981,#88982,
#88983,#88984,#88985,#88986,#88987,#88988,#88989,#88990,#88991),
 .UNSPECIFIED.,.F.,.F.,(4,2,2,2,2,2,2,2,2,2,2,2,2,2,2,2,2,2,2,2,2,2,2,2,
2,2,2,2,2,2,2,2,2,2,2,2,2,2,2,2,2,2,2,2,2,2,2,2,2,2,2,2,2,2,2,2,2,2,2,2,
2,2,2,2,2,2,2,2,2,2,2,2,2,2,2,2,2,2,2,2,2,2,2,2,2,2,2,2,2,2,2,2,2,2,2,2,
2,2,2,2,2,2,2,2,2,2,2,2,2,2,2,2,2,2,2,2,4),(-2.59315595267277,-2.59007765348889,
-2.58078448014978,-2.57864198523523,-2.57741407255166,-2.5763392499272,
-2.57495063749772,-2.57203626725213,-2.54226196803104,-2.49162801649512,
-2.48229546831666,-2.47774314132557,-2.47500475818302,-2.47252037497173,
-2.47064428591098,-2.46881788930564,-2.46627675620113,-2.45963991309685,
-2.40381682376284,-2.37976748382818,-2.36894790729867,-2.36670426759488,
-2.36545415076778,-2.36438225062132,-2.36302621301197,-2.36088056030463,
-2.34984120667498,-2.29863208912856,-2.26992327818169,-2.26348974737613,
-2.26078116271369,-2.25881956543299,-2.25702705011501,-2.25416228960172,
-2.24727840622048,-2.19420723025399,-2.1682997778496,-2.1569927404807,-2.15472034886713,
-2.15346398977869,-2.1523927173179,-2.15104508838411,-2.14842370523333,
-2.13238313327305,-2.12707697857598,-2.11250769039387,-2.07961732011986,
-2.06305117077562,-2.05273924478465,-2.04949046821774,-2.04741715562264,
-2.04547652282287,-2.04293546598963,-2.03864078566131,-2.00353527573851,
-1.95465270383452,-1.94486021660141,-1.9426825914827,-1.94144691070569,
-1.94037323520611,-1.93899650495304,-1.93614316750176,-1.91345110774454,
-1.87272400097021,-1.84568071029017,-1.83944854449809,-1.83677417344399,
-1.83481857270971,-1.83301845523671,-1.83011270095119,-1.82298260427717,
-1.77422260113915,-1.73505265691647,-1.73147802556188,-1.72996901940272,
-1.72887685602193,-1.72785086826456,-1.72610764576359,-1.7213745084549,
-1.6818016663528,-1.63388992437694,-1.62749311299658,-1.62479053606767,
-1.62282984421461,-1.62103578076845,-1.61816336590095,-1.61123424153424,
-1.55875510904605,-1.53242866434402,-1.52101503125635,-1.51873640051769,
-1.51747861786064,-1.51640744490045,-1.51506158223072,-1.51244823431088,
-1.49656815555236,-1.49069806144923,-1.4466670116864,-1.42810815085144,
-1.41691845241822,-1.41357285948488,-1.41147833394793,-1.40954560690936,
-1.40705404709314,-1.40292854555846,-1.37574265801168,-1.33373204453707,
-1.3276351152182,-1.30978754662863,-1.30709916239073,-1.30573723397509,
-1.30466495293353,-1.30341928395598,-1.30119586143113,-1.29070305718652,
-1.26784057085319,-1.25960927882884),.UNSPECIFIED.);
#899=B_SPLINE_CURVE_WITH_KNOTS('',3,(#88997,#88998,#88999,#89000,#89001,
#89002,#89003,#89004,#89005,#89006,#89007,#89008,#89009,#89010,#89011,#89012,
#89013,#89014,#89015,#89016,#89017,#89018,#89019,#89020,#89021,#89022,#89023,
#89024,#89025,#89026,#89027,#89028,#89029,#89030,#89031,#89032,#89033,#89034,
#89035,#89036,#89037,#89038,#89039,#89040,#89041,#89042,#89043,#89044,#89045,
#89046,#89047,#89048,#89049,#89050,#89051,#89052,#89053,#89054,#89055,#89056,
#89057,#89058,#89059,#89060,#89061,#89062,#89063,#89064,#89065,#89066,#89067,
#89068,#89069,#89070,#89071,#89072,#89073,#89074,#89075,#89076,#89077,#89078,
#89079,#89080,#89081,#89082,#89083,#89084,#89085,#89086,#89087,#89088,#89089,
#89090,#89091,#89092,#89093,#89094,#89095,#89096,#89097,#89098,#89099,#89100,
#89101,#89102),.UNSPECIFIED.,.F.,.F.,(4,3,3,3,3,3,3,3,3,3,3,3,3,3,3,3,3,
3,3,3,3,3,3,3,3,3,3,3,3,3,3,3,3,3,3,4),(-3.4905420525369,-3.38888724890093,
-3.28714616891576,-3.1853635306981,-3.08340260642831,-2.99650934988562,
-2.89298804639364,-2.7896177431212,-2.6863657748023,-2.58317744783227,-2.4800189405397,
-2.37685647276338,-2.2735860348565,-2.17025847843688,-2.06674831927576,
-1.99767289992375,-1.89536969270601,-1.79322053934975,-1.69118879043613,
-1.58921974834484,-1.48727804733066,-1.38532836211997,-1.28325632553546,
-1.18112129116516,-1.0787805560955,-0.998836449961877,-0.892562651586185,
-0.780992320137912,-0.67507184468024,-0.56925096547428,-0.463501942676278,
-0.357797126152519,-0.25207917949123,-0.14635615172218,-0.0405601678050039,
0.),.UNSPECIFIED.);
#900=B_SPLINE_CURVE_WITH_KNOTS('',3,(#89105,#89106,#89107,#89108,#89109,
#89110,#89111,#89112,#89113,#89114,#89115,#89116,#89117,#89118,#89119,#89120,
#89121,#89122,#89123,#89124,#89125,#89126,#89127,#89128,#89129,#89130,#89131,
#89132,#89133,#89134,#89135,#89136,#89137,#89138,#89139,#89140,#89141,#89142,
#89143,#89144,#89145,#89146,#89147,#89148,#89149,#89150,#89151,#89152,#89153,
#89154,#89155,#89156,#89157,#89158,#89159,#89160,#89161,#89162,#89163,#89164,
#89165,#89166,#89167,#89168,#89169,#89170,#89171,#89172,#89173,#89174,#89175,
#89176,#89177,#89178,#89179,#89180,#89181,#89182,#89183,#89184,#89185,#89186,
#89187,#89188,#89189,#89190,#89191,#89192,#89193,#89194,#89195,#89196,#89197,
#89198,#89199,#89200,#89201,#89202,#89203,#89204,#89205,#89206,#89207,#89208,
#89209,#89210,#89211,#89212,#89213,#89214,#89215,#89216,#89217,#89218,#89219,
#89220,#89221,#89222,#89223,#89224,#89225,#89226,#89227,#89228,#89229,#89230,
#89231,#89232,#89233,#89234,#89235,#89236,#89237,#89238,#89239,#89240,#89241,
#89242,#89243,#89244,#89245,#89246,#89247,#89248,#89249,#89250,#89251,#89252,
#89253,#89254,#89255,#89256,#89257,#89258,#89259,#89260,#89261,#89262,#89263,
#89264),.UNSPECIFIED.,.F.,.F.,(4,3,3,3,3,3,3,3,3,3,3,3,3,3,3,3,3,3,3,3,
3,3,3,3,3,3,3,3,3,3,3,3,3,3,3,3,3,3,3,3,3,3,3,3,3,3,3,3,3,3,3,3,3,4),(2.00878451784277,
2.11210385922517,2.21526978906692,2.31831430239263,2.42129361283959,2.52424186610781,
2.6271931648727,2.7302492654409,2.83336236205173,2.93665172410155,2.99650934988563,
3.10008230044163,3.20350555624704,3.30681221854458,3.41005628885965,3.51327152250986,
3.61649163431351,3.71982077793715,3.82320772460323,3.92677776279771,3.99534579984751,
4.09860814851249,4.20171513491833,4.30469859633615,4.40761536822811,4.51049968437655,
4.61338573414336,4.71637827780366,4.81942668398311,4.9226588076143,4.99418224980939,
5.09760357317468,5.20087154158791,5.30401821033476,5.40709947808644,5.51014934245976,
5.61320175788194,5.7163607823649,5.81957599567372,5.92297359909411,5.99301869977127,
6.09643423501026,6.19969678171232,6.30283860648639,6.40591538895671,6.50896113435575,
6.61200980509544,6.71516569207009,6.81837810297349,6.92177347981606,6.99185514973315,
7.09672279617372,7.20139614944408,7.2430409600995),.UNSPECIFIED.);
#901=B_SPLINE_CURVE_WITH_KNOTS('',3,(#89270,#89271,#89272,#89273,#89274,
#89275,#89276,#89277,#89278,#89279,#89280,#89281,#89282,#89283,#89284,#89285,
#89286,#89287,#89288,#89289,#89290,#89291,#89292,#89293,#89294,#89295),
 .UNSPECIFIED.,.F.,.F.,(4,2,2,2,2,2,2,2,2,2,2,2,4),(-0.0747573406682046,
-0.0739377203326066,-0.0616380686667433,-0.0559587372308882,-0.0377856382278336,
-0.0350634541223838,-0.0337175330335355,-0.0326484453300257,-0.0316335735595502,
-0.0303960837955203,-0.0285521200295371,-0.0215327131587606,-0.000655551428707696),
 .UNSPECIFIED.);
#902=B_SPLINE_CURVE_WITH_KNOTS('',3,(#89297,#89298,#89299,#89300,#89301,
#89302,#89303,#89304,#89305,#89306,#89307,#89308,#89309,#89310,#89311,#89312,
#89313,#89314,#89315,#89316,#89317,#89318,#89319,#89320,#89321,#89322,#89323,
#89324,#89325,#89326,#89327,#89328,#89329,#89330,#89331,#89332,#89333,#89334,
#89335,#89336,#89337,#89338,#89339,#89340,#89341,#89342,#89343,#89344,#89345,
#89346,#89347,#89348,#89349,#89350,#89351,#89352,#89353,#89354,#89355,#89356,
#89357,#89358,#89359,#89360,#89361,#89362,#89363,#89364,#89365,#89366,#89367,
#89368,#89369,#89370,#89371,#89372,#89373,#89374,#89375,#89376,#89377,#89378,
#89379,#89380,#89381,#89382,#89383,#89384,#89385,#89386,#89387,#89388,#89389,
#89390,#89391,#89392,#89393,#89394,#89395,#89396,#89397,#89398,#89399,#89400,
#89401,#89402,#89403,#89404,#89405,#89406,#89407,#89408,#89409,#89410,#89411,
#89412,#89413,#89414),.UNSPECIFIED.,.F.,.F.,(4,3,3,3,3,3,3,3,3,3,3,3,3,
3,3,3,3,3,3,3,3,3,3,3,3,3,3,3,3,3,3,3,3,3,3,3,3,3,3,4),(170.955339710339,
171.060905920727,171.162663398209,171.264353087631,171.366010720348,171.467671979169,
171.569433774406,171.671256095758,171.773239610404,171.799869393442,171.903390296067,
172.006760196182,172.110011759924,172.213199681674,172.316357783713,172.419519846812,
172.522789883762,172.626117040711,172.729626807232,172.798705843404,172.901009858667,
173.003159822786,173.105192383572,173.207162238204,173.309104751679,173.411055248523,
173.513128090537,173.615263928529,173.717605455249,173.797542293366,173.90381549814,
174.015385903789,174.121305781442,174.227126064404,174.332874494259,174.438578722884,
174.544296093967,174.650018553652,174.755813985758,174.796378743328),
 .UNSPECIFIED.);
#903=B_SPLINE_CURVE_WITH_KNOTS('',3,(#89418,#89419,#89420,#89421,#89422,
#89423,#89424,#89425,#89426,#89427,#89428,#89429,#89430,#89431,#89432,#89433,
#89434,#89435,#89436,#89437,#89438,#89439,#89440,#89441,#89442,#89443,#89444,
#89445,#89446,#89447,#89448,#89449,#89450,#89451,#89452,#89453,#89454,#89455,
#89456,#89457,#89458,#89459,#89460,#89461,#89462,#89463,#89464,#89465,#89466,
#89467,#89468,#89469,#89470,#89471,#89472,#89473,#89474,#89475,#89476,#89477,
#89478,#89479,#89480,#89481,#89482,#89483,#89484,#89485,#89486,#89487,#89488,
#89489,#89490,#89491,#89492,#89493,#89494,#89495,#89496,#89497,#89498,#89499,
#89500,#89501,#89502,#89503,#89504,#89505,#89506,#89507,#89508,#89509,#89510,
#89511,#89512,#89513,#89514,#89515,#89516,#89517,#89518,#89519,#89520,#89521,
#89522,#89523,#89524,#89525,#89526,#89527,#89528,#89529,#89530,#89531,#89532,
#89533,#89534,#89535,#89536,#89537,#89538,#89539,#89540,#89541,#89542,#89543,
#89544,#89545,#89546,#89547,#89548,#89549,#89550,#89551,#89552,#89553,#89554,
#89555,#89556,#89557,#89558,#89559,#89560,#89561,#89562,#89563,#89564,#89565,
#89566,#89567,#89568,#89569,#89570,#89571,#89572,#89573,#89574,#89575,#89576,
#89577,#89578,#89579,#89580,#89581,#89582,#89583,#89584,#89585,#89586),
 .UNSPECIFIED.,.F.,.F.,(4,3,3,3,3,3,3,3,3,3,3,3,3,3,3,3,3,3,3,3,3,3,3,3,
3,3,3,3,3,3,3,3,3,3,3,3,3,3,3,3,3,3,3,3,3,3,3,3,3,3,3,3,3,3,3,3,4),(-172.787594226707,
-172.684274547493,-172.581108276202,-172.478063417649,-172.375083759813,
-172.272135157488,-172.169183508487,-172.066127058214,-171.963013611671,
-171.859723903019,-171.799869393442,-171.696296383671,-171.592873066918,
-171.489566341367,-171.386322206412,-171.283106906827,-171.179886727883,
-171.076557515714,-170.973170499612,-170.8696003913,-170.80103294348,-170.697770746273,
-170.594663913509,-170.491680608289,-170.388763994098,-170.285879836938,
-170.182993947235,-170.08000156422,-169.976953319269,-169.873721356035,
-169.802196493519,-169.698775105051,-169.595507070885,-169.492360335737,
-169.38927900122,-169.286229069815,-169.183176587192,-169.080017495714,
-168.976802215422,-168.873404545781,-168.803360043557,-168.699944492337,
-168.59668192921,-168.493540087422,-168.390463287585,-168.287417524489,
-168.184368835746,-168.081212930417,-167.978000500935,-167.874605105352,
-167.804523593595,-167.699671782329,-167.594987983093,-167.490464931131,
-167.386036707514,-167.281667197445,-167.203857020092),.UNSPECIFIED.);
#904=B_SPLINE_CURVE_WITH_KNOTS('',3,(#89587,#89588,#89589,#89590,#89591,
#89592,#89593,#89594),.UNSPECIFIED.,.F.,.F.,(4,2,2,4),(-2.66749859469711,
-2.6454579420985,-2.59658607096104,-2.59330052944419),.UNSPECIFIED.);
#905=B_SPLINE_CURVE_WITH_KNOTS('',3,(#89599,#89600,#89601,#89602,#89603,
#89604,#89605,#89606,#89607,#89608,#89609,#89610,#89611,#89612,#89613,#89614,
#89615,#89616,#89617,#89618,#89619,#89620,#89621,#89622,#89623,#89624,#89625,
#89626,#89627,#89628,#89629,#89630,#89631,#89632,#89633,#89634,#89635,#89636,
#89637,#89638,#89639,#89640,#89641,#89642,#89643,#89644,#89645,#89646,#89647,
#89648,#89649,#89650,#89651,#89652,#89653,#89654,#89655,#89656,#89657,#89658,
#89659,#89660,#89661,#89662,#89663,#89664,#89665,#89666,#89667,#89668,#89669,
#89670,#89671,#89672,#89673,#89674,#89675,#89676,#89677,#89678,#89679,#89680,
#89681,#89682,#89683,#89684,#89685,#89686,#89687,#89688,#89689,#89690,#89691,
#89692,#89693,#89694,#89695,#89696,#89697,#89698,#89699,#89700,#89701,#89702,
#89703,#89704,#89705,#89706,#89707,#89708,#89709,#89710,#89711,#89712,#89713,
#89714,#89715,#89716,#89717,#89718,#89719,#89720,#89721,#89722,#89723,#89724,
#89725,#89726,#89727,#89728,#89729,#89730,#89731,#89732,#89733,#89734,#89735,
#89736,#89737,#89738,#89739,#89740,#89741,#89742,#89743,#89744,#89745,#89746,
#89747,#89748,#89749,#89750,#89751,#89752,#89753,#89754,#89755,#89756,#89757,
#89758,#89759,#89760,#89761,#89762,#89763,#89764,#89765,#89766,#89767,#89768,
#89769,#89770,#89771,#89772,#89773,#89774,#89775,#89776,#89777,#89778,#89779,
#89780,#89781,#89782,#89783,#89784,#89785,#89786,#89787,#89788,#89789,#89790,
#89791,#89792,#89793,#89794,#89795,#89796,#89797,#89798,#89799,#89800,#89801,
#89802,#89803,#89804,#89805,#89806,#89807,#89808,#89809,#89810,#89811,#89812,
#89813,#89814,#89815,#89816,#89817,#89818,#89819,#89820,#89821,#89822,#89823,
#89824),.UNSPECIFIED.,.F.,.F.,(4,2,2,2,2,2,2,2,2,2,2,2,2,2,2,2,2,2,2,2,
2,2,2,2,2,2,2,2,2,2,2,2,2,2,2,2,2,2,2,2,2,2,2,2,2,2,2,2,2,2,2,2,2,2,2,2,
2,2,2,2,2,2,2,2,2,2,2,2,2,2,2,2,2,2,2,2,2,2,2,2,2,2,2,2,2,2,2,2,2,2,2,2,
2,2,2,2,2,2,2,2,2,2,2,2,2,2,2,2,2,2,2,2,4),(-1.4081797897497,-1.40705404679594,
-1.40292854329057,-1.37574263320905,-1.33373204799533,-1.32763515619996,
-1.30978755234181,-1.30709916585643,-1.30573723651142,-1.30466495482482,
-1.30341928514225,-1.3011958614881,-1.29070305355408,-1.26784055652197,
-1.21011174840212,-1.20367847815884,-1.20117011677497,-1.19935225864924,
-1.19740896745055,-1.19480676077392,-1.18898303817082,-1.1651496956684,
-1.11614975325961,-1.09779133852374,-1.09505199725553,-1.09369780772592,
-1.09262570707542,-1.09137329073468,-1.08912119386837,-1.07817671240186,
-1.05366063720509,-0.998557317290027,-0.991850133661388,-0.989297520826545,
-0.98746765461196,-0.985529978993057,-0.982966721625732,-0.977358981402691,
-0.929074830132709,-0.888723629879558,-0.884011280685756,-0.882271307972931,
-0.881246023907791,-0.880154587919307,-0.878645291924542,-0.875062764192125,
-0.870037629013388,-0.856213724031729,-0.833863298665177,-0.787184837339988,
-0.779989343016949,-0.77707434241061,-0.775273826062298,-0.773322000949637,
-0.770660358982095,-0.764492288721172,-0.737949645692169,-0.698620518806667,
-0.687287343230985,-0.673503592179244,-0.671211207901103,-0.669826477407413,
-0.668750026953921,-0.667534893878322,-0.665449548519146,-0.656907908561592,
-0.64034708537071,-0.598277945699114,-0.571099480893947,-0.566971963994991,
-0.564479142149618,-0.562545400661154,-0.560449734724247,-0.557102213120062,
-0.545904425499174,-0.527329100099386,-0.484807662015825,-0.462028639108672,
-0.45917070499224,-0.457792035941198,-0.456715771265631,-0.455474801951997,
-0.453287245031174,-0.443435837807844,-0.394233153757333,-0.359839085039991,
-0.355551374847713,-0.353009378459771,-0.351065006828444,-0.348984721023599,
-0.345718697498416,-0.335297050035028,-0.318505517073179,-0.258883054465735,
-0.249294071881424,-0.247244741970683,-0.245918126656749,-0.244851087490946,
-0.243841364981986,-0.241868965805794,-0.234450932566741,-0.220917475641148,
-0.192337496364564,-0.147271544802984,-0.143024716885642,-0.140506642976319,
-0.138580632964851,-0.136520189151481,-0.133286020099834,-0.122977037585246,
-0.106384424931836,-0.0845184170571751,-0.0747573406682046),
 .UNSPECIFIED.);
#906=B_SPLINE_CURVE_WITH_KNOTS('',3,(#89825,#89826,#89827,#89828,#89829,
#89830,#89831,#89832,#89833,#89834,#89835,#89836,#89837,#89838,#89839,#89840,
#89841,#89842,#89843,#89844,#89845,#89846,#89847,#89848,#89849,#89850,#89851,
#89852,#89853,#89854,#89855,#89856,#89857,#89858,#89859,#89860,#89861,#89862,
#89863,#89864,#89865,#89866,#89867,#89868,#89869,#89870,#89871,#89872,#89873,
#89874,#89875,#89876,#89877,#89878,#89879,#89880,#89881,#89882,#89883,#89884,
#89885,#89886,#89887,#89888,#89889,#89890,#89891,#89892,#89893,#89894,#89895,
#89896,#89897,#89898,#89899,#89900,#89901,#89902,#89903,#89904,#89905,#89906,
#89907,#89908,#89909,#89910,#89911,#89912,#89913,#89914,#89915,#89916,#89917,
#89918,#89919,#89920,#89921,#89922,#89923,#89924,#89925,#89926,#89927,#89928,
#89929,#89930,#89931,#89932,#89933,#89934,#89935,#89936,#89937,#89938,#89939,
#89940,#89941,#89942,#89943,#89944,#89945,#89946,#89947,#89948,#89949,#89950,
#89951,#89952,#89953,#89954,#89955,#89956,#89957,#89958,#89959,#89960,#89961,
#89962,#89963,#89964,#89965,#89966,#89967,#89968,#89969,#89970,#89971,#89972,
#89973,#89974,#89975,#89976,#89977,#89978,#89979,#89980,#89981,#89982,#89983,
#89984,#89985,#89986,#89987,#89988,#89989,#89990,#89991,#89992,#89993,#89994,
#89995,#89996,#89997,#89998,#89999,#90000,#90001,#90002,#90003,#90004,#90005,
#90006,#90007,#90008,#90009,#90010,#90011,#90012,#90013,#90014,#90015,#90016,
#90017,#90018,#90019,#90020,#90021,#90022,#90023,#90024,#90025,#90026,#90027,
#90028,#90029,#90030,#90031,#90032,#90033,#90034,#90035,#90036,#90037,#90038,
#90039,#90040,#90041,#90042,#90043,#90044,#90045,#90046,#90047,#90048,#90049,
#90050,#90051,#90052,#90053,#90054,#90055,#90056),.UNSPECIFIED.,.F.,.F.,
(4,2,2,2,2,2,2,2,2,2,2,2,2,2,2,2,2,2,2,2,2,2,2,2,2,2,2,2,2,2,2,2,2,2,2,
2,2,2,2,2,2,2,2,2,2,2,2,2,2,2,2,2,2,2,2,2,2,2,2,2,2,2,2,2,2,2,2,2,2,2,2,
2,2,2,2,2,2,2,2,2,2,2,2,2,2,2,2,2,2,2,2,2,2,2,2,2,2,2,2,2,2,2,2,2,2,2,2,
2,2,2,2,2,2,2,2,4),(-2.59330052944419,-2.5868644382203,-2.58469323017153,
-2.5834597768618,-2.58238632325697,-2.58100820152467,-2.57814812648601,
-2.5420719383805,-2.50934246107363,-2.49296682459146,-2.48617192045704,
-2.48254547277301,-2.47944475000296,-2.4774380642021,-2.47549668507091,
-2.4729549099574,-2.46865955728029,-2.43366865647229,-2.38476726569877,
-2.37493625771775,-2.37275508398981,-2.37151813660649,-2.37044414131561,
-2.36906779445472,-2.3662171602355,-2.3298371603387,-2.2760372359654,-2.26958139117063,
-2.26686894554222,-2.26490655399863,-2.26311468811663,-2.2602539510892,
-2.25339519278051,-2.19997525375406,-2.17429633869993,-2.16304748871616,
-2.16077849703701,-2.15952290263944,-2.15845162975484,-2.1571031699405,
-2.15447767294023,-2.13831910533727,-2.09182445546661,-2.06385943680202,
-2.05751531889227,-2.05482203950276,-2.05286334176837,-2.05106781737619,
-2.04818587158402,-2.04119678880736,-1.98962010799096,-1.96265217495558,
-1.95107900283809,-1.94879167624671,-1.94753214900358,-1.94646113758936,
-1.94511764403119,-1.9425157239211,-1.92692673856165,-1.92044462760632,
-1.90654399156092,-1.8736598281375,-1.85710189143986,-1.84679336718953,
-1.84354474019463,-1.84147129836726,-1.839530385679,-1.83698873148448,-1.8326925176529,
-1.79749302106063,-1.74825035671139,-1.73886485807531,-1.73671544191209,
-1.73548585696091,-1.73441111209588,-1.73302459258726,-1.73012150501854,
-1.69805408790132,-1.66516506158529,-1.64633732657471,-1.63885274041799,
-1.63323030387704,-1.6306646562713,-1.62872695437746,-1.62689838542254,
-1.62434971995038,-1.61766602359586,-1.5622722677374,-1.53793035801725,
-1.52703149046051,-1.52478284395909,-1.52353153216006,-1.52245959751839,
-1.52110478414218,-1.51845058324905,-1.50156782970789,-1.48278043140398,
-1.44981441597523,-1.43316116010444,-1.42280939229993,-1.41955568845442,
-1.41748105804103,-1.41554047322765,-1.41300132605133,-1.40871400722063,
-1.36495318354359,-1.33390211915214,-1.3158515009014,-1.31315577159364,
-1.31179207184918,-1.31071940527398,-1.30947444268109,-1.30725504495263,
-1.29683145802611,-1.2742172493562,-1.25973288661493),.UNSPECIFIED.);
#907=B_SPLINE_CURVE_WITH_KNOTS('',3,(#90062,#90063,#90064,#90065),
 .UNSPECIFIED.,.F.,.F.,(4,4),(158.039785789401,158.388969095546),
 .UNSPECIFIED.);
#908=B_SPLINE_CURVE_WITH_KNOTS('',3,(#90066,#90067,#90068,#90069,#90070,
#90071,#90072,#90073,#90074,#90075,#90076,#90077,#90078,#90079,#90080,#90081,
#90082,#90083,#90084,#90085,#90086,#90087,#90088,#90089,#90090,#90091,#90092,
#90093,#90094,#90095,#90096,#90097,#90098,#90099,#90100,#90101,#90102,#90103,
#90104,#90105,#90106,#90107,#90108,#90109,#90110,#90111,#90112,#90113,#90114,
#90115,#90116,#90117,#90118,#90119,#90120,#90121,#90122,#90123,#90124,#90125,
#90126,#90127,#90128,#90129,#90130,#90131,#90132,#90133,#90134,#90135,#90136,
#90137,#90138,#90139,#90140,#90141,#90142,#90143,#90144,#90145,#90146,#90147,
#90148,#90149,#90150,#90151,#90152,#90153,#90154,#90155,#90156,#90157,#90158,
#90159,#90160,#90161,#90162,#90163,#90164,#90165,#90166,#90167,#90168,#90169,
#90170,#90171,#90172,#90173,#90174,#90175,#90176,#90177,#90178,#90179,#90180,
#90181,#90182,#90183,#90184,#90185,#90186,#90187,#90188,#90189,#90190,#90191,
#90192,#90193,#90194,#90195,#90196,#90197,#90198,#90199,#90200,#90201,#90202,
#90203,#90204,#90205,#90206,#90207,#90208,#90209,#90210,#90211,#90212,#90213,
#90214,#90215,#90216,#90217,#90218,#90219,#90220,#90221,#90222,#90223,#90224,
#90225,#90226,#90227,#90228,#90229,#90230,#90231,#90232,#90233,#90234,#90235,
#90236,#90237,#90238,#90239,#90240,#90241,#90242,#90243,#90244,#90245,#90246,
#90247,#90248,#90249,#90250,#90251,#90252,#90253,#90254,#90255,#90256,#90257,
#90258,#90259,#90260,#90261,#90262,#90263,#90264,#90265,#90266,#90267,#90268,
#90269,#90270,#90271,#90272,#90273,#90274,#90275),.UNSPECIFIED.,.F.,.F.,
(4,2,2,2,2,2,2,2,2,2,2,2,2,2,2,2,2,2,2,2,2,2,2,2,2,2,2,2,2,2,2,2,2,2,2,
2,2,2,2,2,2,2,2,2,2,2,2,2,2,2,2,2,2,2,2,2,2,2,2,2,2,2,2,2,2,2,2,2,2,2,2,
2,2,2,2,2,2,2,2,2,2,2,2,2,2,2,2,2,2,2,2,2,2,2,2,2,2,2,2,2,2,2,2,2,4),(-2.66742166532822,
-2.60891629431464,-2.59007759965161,-2.58078441649076,-2.57864191987016,
-2.57741400629466,-2.57633918293723,-2.57495056961282,-2.57203619767363,
-2.54225892562651,-2.49161776942559,-2.48229089683831,-2.47774055884935,
-2.47500299241396,-2.47251919503927,-2.4706432007799,-2.46881661986733,
-2.4662747913464,-2.45963351799724,-2.40385355530975,-2.37977593050351,
-2.36894872217324,-2.36670461920435,-2.36545440107624,-2.36438251077472,
-2.36302660964724,-2.36088140526517,-2.34984929619756,-2.29862561393848,
-2.26992229051696,-2.26348941257987,-2.2607809377382,-2.25881936010741,
-2.25702682155979,-2.25416193435291,-2.24727728246947,-2.19421613294384,
-2.16830170531865,-2.15699288850901,-2.15472039428576,-2.15346401275327,
-2.15239274193152,-2.15104514151731,-2.14842389176343,-2.1323854468327,
-2.12706553014289,-2.11250729619373,-2.07961705160713,-2.06305105501089,
-2.052739197494,-2.04949042823377,-2.0474171168656,-2.04547648279748,-2.04293542081362,
-2.03864072394683,-2.00353402401563,-1.95464777307175,-1.94485963447044,
-1.94268230549169,-1.94144668958548,-1.94037300444971,-1.93899617558637,
-1.93614233737396,-1.91342989016208,-1.87271609682472,-1.84567950042459,
-1.83944815818842,-1.83677392874418,-1.83481835251845,-1.83301820237483,
-1.83011227275717,-1.82298113247133,-1.7742477543539,-1.73505282196107,
-1.73147807388371,-1.72996904762295,-1.72887688066177,-1.72785089843548,
-1.72610770396323,-1.7213747511041,-1.68178083770795,-1.63388986142474,
-1.6274930935136,-1.62479052386571,-1.62282983325471,-1.62103576815868,
-1.61816334456911,-1.61123416775846,-1.55875577244843,-1.53242881078123,
-1.52101504710523,-1.518736408709,-1.51747862427611,-1.5164074510596,-1.5150615897315,
-1.51244824985317,-1.49656852752491,-1.49069764502866,-1.44666704061987,
-1.42810816395616,-1.41691845749845,-1.41357286260411,-1.41147833591662,
-1.40954560786303,-1.4081797897497),.UNSPECIFIED.);
#909=B_SPLINE_CURVE_WITH_KNOTS('',3,(#90277,#90278,#90279,#90280,#90281,
#90282,#90283,#90284,#90285,#90286,#90287,#90288,#90289,#90290,#90291,#90292,
#90293,#90294,#90295,#90296,#90297,#90298,#90299,#90300,#90301,#90302,#90303,
#90304,#90305,#90306,#90307,#90308,#90309,#90310,#90311,#90312,#90313,#90314,
#90315,#90316,#90317,#90318,#90319,#90320,#90321,#90322,#90323,#90324,#90325,
#90326,#90327,#90328,#90329,#90330,#90331,#90332,#90333,#90334,#90335,#90336,
#90337,#90338,#90339,#90340,#90341,#90342,#90343,#90344,#90345,#90346,#90347,
#90348,#90349,#90350,#90351,#90352,#90353,#90354,#90355,#90356,#90357,#90358,
#90359,#90360,#90361,#90362,#90363,#90364,#90365,#90366,#90367,#90368,#90369,
#90370,#90371,#90372,#90373,#90374,#90375,#90376,#90377,#90378,#90379,#90380,
#90381,#90382,#90383,#90384,#90385,#90386,#90387,#90388,#90389,#90390,#90391,
#90392,#90393,#90394,#90395,#90396,#90397,#90398,#90399,#90400,#90401,#90402,
#90403,#90404,#90405,#90406,#90407,#90408,#90409,#90410,#90411,#90412,#90413,
#90414,#90415,#90416,#90417,#90418,#90419,#90420,#90421,#90422,#90423,#90424,
#90425,#90426,#90427,#90428,#90429,#90430,#90431,#90432,#90433,#90434,#90435,
#90436,#90437,#90438,#90439,#90440,#90441,#90442,#90443,#90444,#90445,#90446,
#90447,#90448,#90449,#90450,#90451,#90452,#90453,#90454,#90455,#90456,#90457,
#90458,#90459,#90460,#90461,#90462,#90463,#90464,#90465,#90466,#90467,#90468,
#90469,#90470,#90471,#90472,#90473,#90474,#90475,#90476,#90477,#90478,#90479,
#90480,#90481,#90482,#90483,#90484,#90485,#90486,#90487,#90488,#90489,#90490,
#90491,#90492,#90493,#90494),.UNSPECIFIED.,.F.,.F.,(4,2,2,2,2,2,2,2,2,2,
2,2,2,2,2,2,2,2,2,2,2,2,2,2,2,2,2,2,2,2,2,2,2,2,2,2,2,2,2,2,2,2,2,2,2,2,
2,2,2,2,2,2,2,2,2,2,2,2,2,2,2,2,2,2,2,2,2,2,2,2,2,2,2,2,2,2,2,2,2,2,2,2,
2,2,2,2,2,2,2,2,2,2,2,2,2,2,2,2,2,2,2,2,2,2,2,2,2,2,4),(-1.25973288661493,
-1.21609102900778,-1.20970713987316,-1.20720678920522,-1.20539086341582,
-1.2034460086005,-1.20083540243935,-1.19496613525091,-1.17078874386512,
-1.12030360124663,-1.1198718858852,-1.10368544639769,-1.10105841432207,
-1.09970942323476,-1.09863788976092,-1.09738218819883,-1.09511335897906,
-1.08387288766232,-1.05822562808826,-1.00472263010325,-0.997868278970091,
-0.995008121823537,-0.993216256726692,-0.991253580237683,-0.988540206969882,
-0.982079601166141,-0.928143971185043,-0.891931386762398,-0.889076756241666,
-0.887699689127835,-0.886625881524295,-0.885390202485962,-0.883212937621884,
-0.873428338083152,-0.82450744678719,-0.789384468975772,-0.78508906511928,
-0.782547717715193,-0.780606931002825,-0.778533518822625,-0.775284719997248,
-0.764973758756719,-0.748412426730895,-0.715552856294598,-0.701808196570598,
-0.694966711579718,-0.694678201475862,-0.689570275476756,-0.679120560118283,
-0.677012539820711,-0.675667992911381,-0.674596860609576,-0.673337992108514,
-0.671054196041308,-0.65954849637835,-0.632851307566126,-0.580856958608613,
-0.573892440975401,-0.571014328735491,-0.56921933296634,-0.567259729978056,
-0.564562494512965,-0.558196344731607,-0.530055119346326,-0.482629510166844,
-0.476764228666177,-0.4670299106766,-0.464970429658426,-0.463640820803762,
-0.462570511786875,-0.461299580938961,-0.458959845461074,-0.446402754509434,
-0.388606908516483,-0.381963461977945,-0.364258386221868,-0.360585764722962,
-0.358204522639127,-0.356289599767679,-0.354110024598494,-0.350380157895714,
-0.334899452064879,-0.283061726071859,-0.256023268574076,-0.253121793407635,
-0.251735740873461,-0.250661241279027,-0.249431849008249,-0.247325610837725,
-0.238412497268297,-0.220688901717591,-0.192467064558443,-0.153492447207531,
-0.14875578850538,-0.146329879720163,-0.144410718331475,-0.142259821620451,
-0.138659930148412,-0.124800709222653,-0.0975397305688386,-0.0749682922101801,
-0.0441240160777874,-0.0412117837959577,-0.0398236655310865,-0.0387489802648021,
-0.0375209594861392,-0.0362288352709404,-0.0342508952684674,-0.000628703082161277),
 .UNSPECIFIED.);
#910=B_SPLINE_CURVE_WITH_KNOTS('',3,(#90495,#90496,#90497,#90498,#90499,
#90500,#90501,#90502,#90503,#90504,#90505,#90506,#90507,#90508,#90509,#90510,
#90511,#90512),.UNSPECIFIED.,.F.,.F.,(4,2,2,2,2,2,2,2,4),(-2.66821958497409,
-2.63796945984048,-2.61126613950847,-2.60507567789451,-2.6024083434344,
-2.60045381523792,-2.59865183150659,-2.59573671182581,-2.59373671315012),
 .UNSPECIFIED.);
#911=B_SPLINE_CURVE_WITH_KNOTS('',3,(#90518,#90519,#90520,#90521,#90522,
#90523,#90524,#90525,#90526,#90527,#90528,#90529,#90530),.UNSPECIFIED.,
 .F.,.F.,(4,3,3,3,4),(151.755345396259,151.823140394205,151.95194859726,
152.078650414049,152.105783788367),.UNSPECIFIED.);
#912=B_SPLINE_CURVE_WITH_KNOTS('',3,(#90531,#90532,#90533,#90534,#90535,
#90536,#90537,#90538,#90539,#90540),.UNSPECIFIED.,.F.,.F.,(4,1,1,1,1,1,
1,4),(152.105783788367,152.821976844167,153.820813294129,154.81964974409,
155.818486194052,156.817322644014,157.816159093976,158.039785789401),
 .UNSPECIFIED.);
#913=B_SPLINE_CURVE_WITH_KNOTS('',3,(#90541,#90542,#90543,#90544,#90545,
#90546,#90547,#90548,#90549,#90550,#90551,#90552,#90553,#90554,#90555,#90556,
#90557,#90558,#90559,#90560,#90561,#90562,#90563,#90564,#90565,#90566,#90567,
#90568,#90569,#90570,#90571,#90572,#90573,#90574,#90575,#90576,#90577,#90578,
#90579,#90580,#90581,#90582,#90583,#90584,#90585,#90586,#90587,#90588,#90589,
#90590,#90591,#90592,#90593,#90594,#90595,#90596,#90597,#90598,#90599,#90600,
#90601,#90602,#90603,#90604,#90605,#90606,#90607,#90608,#90609,#90610,#90611,
#90612,#90613,#90614,#90615,#90616,#90617,#90618,#90619,#90620,#90621,#90622,
#90623,#90624,#90625,#90626,#90627,#90628,#90629,#90630,#90631,#90632,#90633,
#90634,#90635,#90636,#90637,#90638,#90639,#90640,#90641,#90642,#90643,#90644,
#90645,#90646,#90647,#90648,#90649,#90650,#90651,#90652,#90653,#90654,#90655,
#90656,#90657,#90658,#90659,#90660,#90661,#90662,#90663,#90664,#90665,#90666,
#90667,#90668,#90669,#90670,#90671,#90672,#90673,#90674,#90675,#90676,#90677,
#90678,#90679,#90680,#90681,#90682,#90683,#90684,#90685,#90686,#90687,#90688,
#90689,#90690,#90691,#90692,#90693,#90694,#90695,#90696,#90697,#90698,#90699,
#90700,#90701,#90702,#90703,#90704,#90705,#90706,#90707,#90708,#90709,#90710,
#90711,#90712,#90713,#90714,#90715,#90716,#90717,#90718,#90719,#90720,#90721,
#90722,#90723,#90724,#90725,#90726,#90727,#90728,#90729,#90730,#90731,#90732,
#90733,#90734,#90735,#90736,#90737,#90738,#90739,#90740,#90741,#90742,#90743,
#90744,#90745,#90746,#90747,#90748,#90749,#90750,#90751,#90752,#90753,#90754,
#90755,#90756,#90757,#90758,#90759,#90760,#90761,#90762),.UNSPECIFIED.,
 .F.,.F.,(4,2,2,2,2,2,2,2,2,2,2,2,2,2,2,2,2,2,2,2,2,2,2,2,2,2,2,2,2,2,2,
2,2,2,2,2,2,2,2,2,2,2,2,2,2,2,2,2,2,2,2,2,2,2,2,2,2,2,2,2,2,2,2,2,2,2,2,
2,2,2,2,2,2,2,2,2,2,2,2,2,2,2,2,2,2,2,2,2,2,2,2,2,2,2,2,2,2,2,2,2,2,2,2,
2,2,2,2,2,2,2,4),(-2.59373671315012,-2.5885519066095,-2.54144355714508,
-2.51722412424279,-2.5050149229938,-2.49811631989247,-2.49617311223199,
-2.49515834494911,-2.49408693164924,-2.49274001307796,-2.4901226509639,
-2.47415863689511,-2.46978685897904,-2.42630149968854,-2.39931492302155,
-2.3930894522106,-2.39041606572864,-2.38846047946461,-2.3866598821561,-2.38375225793744,
-2.37661209459938,-2.32808667121904,-2.28870985303142,-2.28511725563706,
-2.28360510789293,-2.28251234203669,-2.28148717219389,-2.27974816493781,
-2.2750429161707,-2.23449993456854,-2.18634894413985,-2.1807425250122,-2.17817981629052,
-2.17624254297965,-2.1744130567236,-2.17186098219802,-2.16515526905852,
-2.10999239957505,-2.08549800701937,-2.07455840148644,-2.07230726977264,
-2.07105539593064,-2.06998348286275,-2.06862933946845,-2.06589031332082,
-2.0475474466011,-2.02964507883391,-1.99690756912366,-1.97439761841213,
-1.96875036813469,-1.9661799996026,-1.96424142342186,-1.96241400913326,
-1.95987013454753,-1.95321821753177,-1.89749321116305,-1.87336612025167,
-1.86252449021087,-1.86027911629667,-1.8590284306805,-1.85795629518206,
-1.85660028092841,-1.85445525614602,-1.84343170659804,-1.79212690887746,
-1.76346286191477,-1.75703392161832,-1.75432571791138,-1.75236383347144,
-1.7505706684644,-1.74770402737221,-1.74081126317658,-1.68781786469749,
-1.66184078828374,-1.65051483902675,-1.64824095990395,-1.64698408922861,
-1.64591255628575,-1.64456482815435,-1.6419439561885,-1.62591896321951,
-1.62051407716177,-1.60601449268855,-1.57311679546957,-1.55035891717881,
-1.5446779925067,-1.54210133553019,-1.54016168247121,-1.53833594190101,
-1.53579870545865,-1.52918963838033,-1.47303657279827,-1.44918592382808,
-1.43841875724763,-1.4361777985978,-1.43492802304568,-1.4338557112365,-1.43249824599391,
-1.42983233030584,-1.41264466940409,-1.36256430977398,-1.34500777813006,
-1.33425295364739,-1.33095371188329,-1.32886892153168,-1.32693190827543,
-1.32437257649212,-1.3187857356506,-1.31136194166418,-1.29275925442224,
-1.25991250331722),.UNSPECIFIED.);
#914=B_SPLINE_CURVE_WITH_KNOTS('',3,(#90768,#90769,#90770,#90771,#90772,
#90773,#90774,#90775,#90776,#90777,#90778,#90779,#90780,#90781),
 .UNSPECIFIED.,.F.,.F.,(4,2,2,2,2,2,4),(-0.074917573155471,-0.0721518777810642,
-0.0417414976932024,-0.00539305516346449,-0.00193455376436665,-0.000863977439296385,
-0.000629063808748724),.UNSPECIFIED.);
#915=B_SPLINE_CURVE_WITH_KNOTS('',3,(#90782,#90783,#90784,#90785,#90786,
#90787,#90788,#90789,#90790,#90791,#90792,#90793,#90794,#90795,#90796,#90797,
#90798,#90799,#90800,#90801,#90802,#90803,#90804,#90805,#90806,#90807,#90808,
#90809,#90810,#90811,#90812,#90813,#90814,#90815,#90816,#90817,#90818,#90819,
#90820,#90821,#90822,#90823,#90824,#90825,#90826,#90827,#90828,#90829,#90830,
#90831,#90832,#90833,#90834,#90835,#90836,#90837,#90838,#90839,#90840,#90841,
#90842,#90843,#90844,#90845,#90846,#90847,#90848,#90849,#90850,#90851,#90852,
#90853,#90854,#90855,#90856,#90857,#90858,#90859,#90860,#90861,#90862,#90863,
#90864,#90865,#90866,#90867,#90868,#90869,#90870,#90871,#90872,#90873,#90874,
#90875,#90876,#90877,#90878,#90879,#90880,#90881,#90882,#90883,#90884,#90885,
#90886,#90887,#90888,#90889,#90890,#90891,#90892,#90893,#90894,#90895,#90896,
#90897,#90898,#90899,#90900,#90901,#90902,#90903,#90904,#90905,#90906,#90907,
#90908,#90909,#90910,#90911,#90912,#90913,#90914,#90915,#90916,#90917,#90918,
#90919,#90920,#90921,#90922,#90923,#90924,#90925,#90926,#90927,#90928,#90929,
#90930,#90931,#90932,#90933,#90934,#90935,#90936,#90937,#90938,#90939,#90940,
#90941,#90942,#90943,#90944,#90945,#90946,#90947,#90948,#90949,#90950,#90951,
#90952,#90953,#90954,#90955,#90956,#90957,#90958,#90959,#90960,#90961,#90962),
 .UNSPECIFIED.,.F.,.F.,(4,3,3,3,3,3,3,3,3,3,3,3,3,3,3,3,3,3,3,3,3,3,3,3,
3,3,3,3,3,3,3,3,3,3,3,3,3,3,3,3,3,3,3,3,3,3,3,3,3,3,3,3,3,3,3,3,3,3,3,3,
4),(145.822598481187,145.830121694434,145.93351643147,146.036757713573,
146.139877678953,146.24293224715,146.345955455496,146.448981298156,146.552114064923,
146.655303156322,146.758675149692,146.828958144396,146.932352881429,147.03559416353,
147.138714128907,147.241768697101,147.344791905443,147.4478177481,147.550950514863,
147.654139606258,147.757511599624,147.827794594357,147.931189331481,148.034430613671,
148.137550579139,148.240605147424,148.343628355857,148.446654198605,148.549786965457,
148.652976056941,148.756348050394,148.826631044319,148.930025781262,149.033267063273,
149.136387028563,149.239441596669,149.342464804925,149.445490647497,149.548623414176,
149.651812505488,149.755184498775,149.825467494281,149.928862231266,150.032103513317,
150.135223478643,150.238278046785,150.341301255075,150.444327097679,150.547459864388,
150.650648955728,150.75402094904,150.824303944243,150.927703487107,151.031158725751,
151.134277032305,151.237328082822,151.340345915983,151.444095786052,151.547200179005,
151.651272787632,151.755345396259),.UNSPECIFIED.);
#916=B_SPLINE_CURVE_WITH_KNOTS('',3,(#90964,#90965,#90966,#90967,#90968,
#90969,#90970,#90971,#90972,#90973,#90974,#90975,#90976,#90977,#90978,#90979,
#90980,#90981,#90982,#90983,#90984,#90985,#90986,#90987,#90988,#90989,#90990,
#90991,#90992,#90993,#90994,#90995,#90996,#90997,#90998,#90999,#91000,#91001,
#91002,#91003,#91004,#91005,#91006,#91007,#91008,#91009,#91010,#91011,#91012,
#91013,#91014,#91015,#91016,#91017,#91018,#91019,#91020,#91021,#91022,#91023,
#91024,#91025,#91026,#91027,#91028,#91029,#91030,#91031,#91032,#91033,#91034,
#91035,#91036,#91037,#91038,#91039,#91040,#91041,#91042,#91043,#91044,#91045,
#91046,#91047,#91048,#91049,#91050,#91051,#91052,#91053,#91054,#91055,#91056,
#91057,#91058,#91059,#91060,#91061,#91062,#91063,#91064,#91065,#91066,#91067,
#91068,#91069,#91070,#91071,#91072,#91073,#91074,#91075,#91076,#91077,#91078,
#91079,#91080,#91081,#91082,#91083,#91084,#91085,#91086,#91087,#91088,#91089,
#91090,#91091,#91092,#91093,#91094,#91095,#91096,#91097,#91098,#91099,#91100,
#91101,#91102,#91103,#91104,#91105,#91106,#91107,#91108,#91109,#91110,#91111,
#91112,#91113,#91114,#91115,#91116,#91117,#91118,#91119,#91120,#91121,#91122,
#91123,#91124,#91125,#91126,#91127,#91128,#91129,#91130,#91131,#91132,#91133,
#91134,#91135,#91136,#91137,#91138,#91139,#91140,#91141,#91142,#91143,#91144,
#91145,#91146,#91147,#91148,#91149,#91150,#91151,#91152,#91153,#91154,#91155,
#91156,#91157,#91158,#91159,#91160,#91161,#91162,#91163,#91164,#91165,#91166,
#91167,#91168,#91169,#91170,#91171,#91172,#91173,#91174,#91175,#91176,#91177,
#91178,#91179,#91180,#91181,#91182,#91183,#91184,#91185,#91186,#91187),
 .UNSPECIFIED.,.F.,.F.,(4,2,2,2,2,2,2,2,2,2,2,2,2,2,2,2,2,2,2,2,2,2,2,2,
2,2,2,2,2,2,2,2,2,2,2,2,2,2,2,2,2,2,2,2,2,2,2,2,2,2,2,2,2,2,2,2,2,2,2,2,
2,2,2,2,2,2,2,2,2,2,2,2,2,2,2,2,2,2,2,2,2,2,2,2,2,2,2,2,2,2,2,2,2,2,2,2,
2,2,2,2,2,2,2,2,2,2,2,2,2,2,2,4),(-1.25991250331722,-1.25002813172122,-1.22739940627457,
-1.22454711829876,-1.22317040286594,-1.22209650344233,-1.22086030515237,
-1.2186811330972,-1.20887147997461,-1.15996413031623,-1.12484337567231,
-1.12054749914052,-1.11800584391394,-1.11606480586091,-1.1139911093724,
-1.11074183203824,-1.10042907261466,-1.0838645839366,-1.05099990909305,
-1.03717125190871,-1.03052074071258,-1.01504656714291,-1.01244937440331,
-1.01110681137823,-1.0100356707126,-1.0087749432634,-1.00648302703673,-0.994835746195091,
-0.967567893194984,-0.947382757239736,-0.912873674362607,-0.908586806373821,
-0.906047786917541,-0.904107208166566,-0.902032494225878,-0.898778469395456,
-0.888423975695388,-0.871767003261979,-0.838826047861659,-0.820097788600979,
-0.803187225981111,-0.800532039099481,-0.799177010426617,-0.798105054208289,
-0.796853893602148,-0.794605944819627,-0.783719158342336,-0.759419477194735,
-0.703923634882994,-0.697247249399042,-0.694699731403431,-0.692871485664991,
-0.690933666987531,-0.688367078274858,-0.682739383699102,-0.6752465152499,
-0.656390000490043,-0.626123162780596,-0.603712281586419,-0.590881821532613,
-0.588635417285089,-0.587248847445616,-0.586174186400526,-0.584944877850398,
-0.582796222107857,-0.573418765837406,-0.524153447857989,-0.488926995616057,
-0.484630621662475,-0.482089118915688,-0.480148454556145,-0.478075406677634,
-0.474827666243869,-0.464524171507818,-0.447978733805499,-0.417105330677107,
-0.397465074860393,-0.379318159348492,-0.376619772926513,-0.375255700043835,
-0.374183243301061,-0.37293910482788,-0.370722563288281,-0.360689042936503,
-0.312017030045687,-0.276983409152321,-0.272689986985027,-0.270149477771124,
-0.268209138599189,-0.266136017776191,-0.262887285387177,-0.252768494669576,
-0.236546077612513,-0.198322587460796,-0.167652355216197,-0.164739955529095,
-0.163351845156246,-0.16227720647158,-0.161049284316136,-0.159757277992429,
-0.155110106732141,-0.128864893842154,-0.106990886444038,-0.105560222755592,
-0.0651104975484208,-0.0603738601673643,-0.0579480736817614,-0.0560290637262798,
-0.0538783940734142,-0.0516516914803666,-0.0483298719004753,-0.0006289855317579),
 .UNSPECIFIED.);
#917=B_SPLINE_CURVE_WITH_KNOTS('',3,(#91188,#91189,#91190,#91191,#91192,
#91193,#91194,#91195,#91196,#91197,#91198,#91199,#91200,#91201,#91202,#91203,
#91204,#91205,#91206,#91207),.UNSPECIFIED.,.F.,.F.,(4,2,2,2,2,2,2,2,2,4),
(-2.66776155019002,-2.62480392487054,-2.62186972745952,-2.62018685021,-2.61868180779369,
-2.61759012196051,-2.61656272724315,-2.61481300241367,-2.61003839935785,
-2.59362782388558),.UNSPECIFIED.);
#918=B_SPLINE_CURVE_WITH_KNOTS('',3,(#91212,#91213,#91214,#91215,#91216,
#91217,#91218,#91219,#91220,#91221,#91222,#91223,#91224,#91225,#91226,#91227,
#91228,#91229,#91230,#91231,#91232,#91233,#91234,#91235,#91236,#91237,#91238,
#91239,#91240,#91241,#91242,#91243,#91244,#91245,#91246,#91247,#91248,#91249,
#91250,#91251,#91252,#91253,#91254,#91255,#91256,#91257,#91258,#91259,#91260,
#91261,#91262,#91263,#91264,#91265,#91266,#91267,#91268,#91269,#91270,#91271,
#91272,#91273,#91274,#91275,#91276,#91277,#91278,#91279,#91280,#91281,#91282,
#91283,#91284,#91285,#91286,#91287,#91288,#91289,#91290,#91291,#91292,#91293,
#91294,#91295,#91296,#91297,#91298,#91299,#91300,#91301,#91302,#91303,#91304,
#91305,#91306,#91307,#91308,#91309,#91310,#91311,#91312,#91313,#91314,#91315,
#91316,#91317,#91318,#91319,#91320,#91321,#91322,#91323,#91324,#91325,#91326,
#91327,#91328,#91329,#91330,#91331,#91332,#91333,#91334,#91335,#91336,#91337,
#91338,#91339,#91340,#91341,#91342,#91343,#91344,#91345,#91346,#91347,#91348,
#91349,#91350,#91351,#91352,#91353,#91354,#91355,#91356,#91357,#91358,#91359,
#91360,#91361,#91362,#91363,#91364,#91365,#91366,#91367,#91368,#91369,#91370,
#91371,#91372,#91373,#91374,#91375,#91376,#91377,#91378,#91379,#91380,#91381,
#91382,#91383,#91384,#91385,#91386,#91387,#91388,#91389,#91390,#91391,#91392,
#91393,#91394,#91395,#91396,#91397,#91398,#91399,#91400,#91401,#91402,#91403,
#91404,#91405,#91406,#91407,#91408,#91409,#91410,#91411,#91412,#91413,#91414,
#91415,#91416,#91417,#91418,#91419,#91420,#91421,#91422,#91423,#91424,#91425,
#91426,#91427,#91428,#91429,#91430,#91431,#91432,#91433,#91434,#91435,#91436,
#91437,#91438,#91439,#91440,#91441,#91442,#91443,#91444,#91445,#91446,#91447,
#91448,#91449,#91450,#91451,#91452,#91453,#91454,#91455,#91456,#91457,#91458,
#91459,#91460,#91461,#91462,#91463,#91464,#91465,#91466,#91467,#91468,#91469,
#91470,#91471,#91472,#91473,#91474,#91475,#91476,#91477,#91478,#91479,#91480,
#91481,#91482,#91483,#91484,#91485,#91486,#91487,#91488,#91489,#91490,#91491,
#91492,#91493,#91494,#91495,#91496,#91497,#91498,#91499,#91500,#91501,#91502,
#91503),.UNSPECIFIED.,.F.,.F.,(4,2,2,2,2,2,2,2,2,2,2,2,2,2,2,2,2,2,2,2,
2,2,2,2,2,2,2,2,2,2,2,2,2,2,2,2,2,2,2,2,2,2,2,2,2,2,2,2,2,2,2,2,2,2,2,2,
2,2,2,2,2,2,2,2,2,2,2,2,2,2,2,2,2,2,2,2,2,2,2,2,2,2,2,2,2,2,2,2,2,2,2,2,
2,2,2,2,2,2,2,2,2,2,2,2,2,2,2,2,2,2,2,2,2,2,2,2,2,2,2,2,2,2,2,2,2,2,2,2,
2,2,2,2,2,2,2,2,2,2,2,2,2,2,2,2,2,4),(-1.40850263276381,-1.39306960650067,
-1.38272141396964,-1.37946833818062,-1.37739398881794,-1.37545358293386,
-1.37291454863777,-1.36862714823561,-1.33404430226293,-1.27807589774523,
-1.27380186776896,-1.2721302118413,-1.27111813467408,-1.27001574616159,
-1.26845075233166,-1.26453804111152,-1.24532482158701,-1.18894817501761,
-1.17210239448734,-1.16848552089998,-1.16612131436722,-1.16420743009777,
-1.16201517432855,-1.15822869517727,-1.14198122170515,-1.08450354925769,
-1.07953139272385,-1.06354559320653,-1.06092713862079,-1.05958002512239,
-1.05850864967895,-1.05725158550547,-1.05497638394429,-1.04362442710341,
-1.01754024734705,-0.964668867744824,-0.957765554845653,-0.954897388799684,
-0.953104103693257,-0.951142763526614,-0.94843654163411,-0.942018110998607,
-0.913442873113261,-0.862247029074522,-0.85108306084867,-0.848929648340678,
-0.847571185754394,-0.846499019082565,-0.845250490378984,-0.843014434882705,
-0.832321750132846,-0.808737936343438,-0.752153096626779,-0.74558954398186,
-0.743059903887193,-0.741236436515012,-0.739296246194381,-0.73671381893069,
-0.730999356023087,-0.707989940413683,-0.674964337528586,-0.653790273629086,
-0.639415317281718,-0.637089629359933,-0.635694469611654,-0.634616103399286,
-0.633406012254734,-0.631343979448014,-0.623093436484699,-0.60736981153309,
-0.565372529404616,-0.537089951379794,-0.532935397739698,-0.530435236908605,
-0.528501113236433,-0.526410322838754,-0.523082025283081,-0.512054952853508,
-0.493875879415992,-0.444530095327261,-0.427621884538517,-0.424967090879969,
-0.423612265100394,-0.422540470539185,-0.421289499927994,-0.41904189577949,
-0.408156841471152,-0.383861158966252,-0.328373211450144,-0.321697882679927,
-0.319150756769556,-0.317322788963908,-0.315385261708537,-0.312819053600094,
-0.3071921717625,-0.299700372490152,-0.280846477358196,-0.243379611800286,
-0.215989461150098,-0.213146930991104,-0.2117665626231,-0.210714902543605,
-0.210704908166831,-0.210695219542147,-0.210685813785961,-0.210676670313867,
-0.210667770546727,-0.210659097713162,-0.210650636523358,-0.210642372995015,
-0.210634294452222,-0.210626389153954,-0.210618646320887,-0.21061105611836,
-0.210603609337558,-0.210596297508208,-0.210589112793029,-0.210582047896446,
-0.210575095924169,-0.210568250483994,-0.210561505639592,-0.21055485581026,
-0.210548295784861,-0.210541820529687,-0.21053542544248,-0.210529106212553,
-0.210522858613384,-0.210516678751372,-0.210510562912216,-0.210504507472682,
-0.21049850917729,-0.210492564804552,-0.210486671239849,-0.210480825664762,
-0.209218777563569,-0.206836330089074,-0.193388474596719,-0.157804786601052,
-0.113366713485948,-0.109089406061395,-0.106553552524982,-0.104613951666928,
-0.102538881528046,-0.0992813619648698,-0.0888907940615931,-0.074917573155471),
 .UNSPECIFIED.);
#919=B_SPLINE_CURVE_WITH_KNOTS('',3,(#91504,#91505,#91506,#91507,#91508,
#91509,#91510,#91511,#91512,#91513,#91514,#91515,#91516,#91517,#91518,#91519,
#91520,#91521,#91522,#91523,#91524,#91525,#91526,#91527,#91528,#91529,#91530,
#91531,#91532,#91533,#91534,#91535,#91536,#91537,#91538,#91539,#91540,#91541,
#91542,#91543,#91544,#91545,#91546,#91547,#91548,#91549,#91550,#91551,#91552,
#91553,#91554,#91555,#91556,#91557,#91558,#91559,#91560,#91561,#91562,#91563,
#91564,#91565,#91566,#91567,#91568,#91569,#91570,#91571,#91572,#91573,#91574,
#91575,#91576,#91577,#91578,#91579,#91580,#91581,#91582,#91583,#91584,#91585,
#91586,#91587,#91588,#91589,#91590,#91591,#91592,#91593,#91594,#91595,#91596,
#91597,#91598,#91599,#91600,#91601,#91602,#91603,#91604,#91605,#91606,#91607,
#91608,#91609,#91610,#91611,#91612,#91613,#91614,#91615,#91616,#91617,#91618,
#91619,#91620,#91621,#91622,#91623,#91624,#91625,#91626,#91627,#91628,#91629,
#91630,#91631,#91632,#91633,#91634,#91635,#91636,#91637,#91638,#91639,#91640,
#91641,#91642,#91643,#91644,#91645,#91646,#91647,#91648,#91649,#91650,#91651,
#91652,#91653,#91654,#91655,#91656,#91657,#91658,#91659,#91660,#91661,#91662,
#91663,#91664,#91665,#91666,#91667,#91668,#91669,#91670,#91671,#91672,#91673,
#91674,#91675,#91676,#91677,#91678,#91679,#91680,#91681,#91682,#91683,#91684,
#91685,#91686,#91687,#91688,#91689,#91690,#91691,#91692,#91693,#91694,#91695,
#91696,#91697,#91698,#91699,#91700,#91701,#91702,#91703,#91704,#91705,#91706,
#91707,#91708,#91709,#91710,#91711,#91712,#91713,#91714,#91715,#91716,#91717,
#91718,#91719,#91720,#91721,#91722,#91723,#91724,#91725,#91726,#91727,#91728,
#91729),.UNSPECIFIED.,.F.,.F.,(4,2,2,2,2,2,2,2,2,2,2,2,2,2,2,2,2,2,2,2,
2,2,2,2,2,2,2,2,2,2,2,2,2,2,2,2,2,2,2,2,2,2,2,2,2,2,2,2,2,2,2,2,2,2,2,2,
2,2,2,2,2,2,2,2,2,2,2,2,2,2,2,2,2,2,2,2,2,2,2,2,2,2,2,2,2,2,2,2,2,2,2,2,
2,2,2,2,2,2,2,2,2,2,2,2,2,2,2,2,2,2,2,2,4),(-2.59362782388558,-2.57257925030196,
-2.55115577851568,-2.5228183915866,-2.51634429103098,-2.51421986332297,
-2.51213975030339,-2.51020081444974,-2.50767353314413,-2.50342783372285,
-2.47122885075476,-2.43578620023354,-2.41829769048525,-2.40946119833998,
-2.40735964264383,-2.40613099296778,-2.40505584991846,-2.40366725197709,
-2.40075442504182,-2.36926629053877,-2.3184592597984,-2.31014901888898,
-2.3040998529636,-2.3014246241393,-2.29946850945367,-2.29766799802435,-2.29476178318676,
-2.28763143438713,-2.23880480649687,-2.19967629084255,-2.19610106332546,
-2.19459175429153,-2.19349936616057,-2.19247321713409,-2.19072970000656,
-2.18599565714715,-2.14618181156768,-2.09848204321019,-2.09208421069137,
-2.08938116470109,-2.08742012077934,-2.08562572765126,-2.08275277023494,
-2.07582227592471,-2.02333086177869,-1.9969984583142,-1.98558223788631,
-1.98330310124768,-1.98204504118789,-1.98097353402213,-1.97962716041026,
-1.9770128019396,-1.96112406487979,-1.95269722264833,-1.91136684888007,
-1.89271083159245,-1.88147841142933,-1.8781274666877,-1.87603123828051,
-1.87409805635767,-1.87160746720959,-1.86748693128449,-1.84054434892272,
-1.79861302725543,-1.78184939889946,-1.77323732522018,-1.77114577576153,
-1.76992890075814,-1.76885161693807,-1.76746704023715,-1.76517806504482,
-1.75150394292382,-1.74978242849758,-1.70241593615213,-1.67144142341111,
-1.66698943453022,-1.66465381635431,-1.6627413266828,-1.66052635305962,
-1.65673879311931,-1.64214417233858,-1.6298786516596,-1.58946761081467,
-1.57061392260565,-1.56131512761951,-1.55917184644827,-1.55794356523527,
-1.55686847296439,-1.5554795820761,-1.55256487524529,-1.52372643522699,
-1.4856166908261,-1.46809095165913,-1.4573497752477,-1.45405209439119,-1.45196768183834,
-1.45003059930798,-1.44751407113299,-1.4433048278966,-1.41283082291991,
-1.36760469595528,-1.35571214220384,-1.35117705443448,-1.34786864607341,
-1.34640616341106,-1.34532146060471,-1.3441325725923,-1.34216662668467,
-1.33576152148236,-1.3342056133521,-1.31961907874268,-1.260577564675,-1.25976204361674),
 .UNSPECIFIED.);
#920=B_SPLINE_CURVE_WITH_KNOTS('',3,(#91735,#91736,#91737,#91738,#91739,
#91740,#91741,#91742),.UNSPECIFIED.,.F.,.F.,(4,2,2,4),(-0.0748537111811377,
-0.0742481347811158,-0.0252918437645686,-0.00062946485106353),
 .UNSPECIFIED.);
#921=B_SPLINE_CURVE_WITH_KNOTS('',3,(#91743,#91744,#91745,#91746,#91747,
#91748,#91749,#91750,#91751,#91752,#91753,#91754,#91755,#91756,#91757,#91758,
#91759,#91760,#91761,#91762,#91763,#91764,#91765,#91766,#91767,#91768,#91769,
#91770,#91771,#91772,#91773,#91774,#91775,#91776,#91777,#91778,#91779,#91780,
#91781,#91782,#91783,#91784,#91785,#91786,#91787,#91788,#91789,#91790,#91791,
#91792,#91793,#91794,#91795,#91796,#91797,#91798,#91799,#91800,#91801,#91802,
#91803,#91804,#91805,#91806,#91807,#91808,#91809,#91810,#91811,#91812,#91813,
#91814,#91815,#91816,#91817,#91818,#91819,#91820,#91821,#91822,#91823,#91824,
#91825,#91826,#91827,#91828,#91829,#91830,#91831,#91832,#91833,#91834,#91835,
#91836,#91837,#91838,#91839,#91840,#91841,#91842,#91843,#91844,#91845,#91846,
#91847,#91848,#91849,#91850,#91851,#91852,#91853,#91854,#91855,#91856,#91857,
#91858,#91859,#91860,#91861,#91862,#91863,#91864,#91865,#91866,#91867,#91868,
#91869,#91870,#91871,#91872,#91873,#91874,#91875,#91876,#91877,#91878,#91879,
#91880,#91881,#91882,#91883,#91884,#91885,#91886,#91887,#91888,#91889,#91890,
#91891,#91892,#91893,#91894,#91895,#91896,#91897,#91898,#91899,#91900,#91901,
#91902,#91903,#91904,#91905,#91906,#91907,#91908,#91909,#91910,#91911,#91912,
#91913,#91914,#91915,#91916,#91917,#91918,#91919,#91920,#91921,#91922,#91923,
#91924,#91925,#91926,#91927,#91928,#91929,#91930,#91931,#91932,#91933,#91934,
#91935,#91936,#91937,#91938,#91939,#91940,#91941,#91942,#91943,#91944,#91945,
#91946,#91947,#91948,#91949,#91950,#91951,#91952,#91953,#91954,#91955,#91956,
#91957,#91958,#91959,#91960,#91961,#91962,#91963,#91964,#91965,#91966,#91967,
#91968,#91969,#91970,#91971,#91972,#91973,#91974,#91975,#91976,#91977,#91978,
#91979,#91980,#91981,#91982,#91983,#91984,#91985,#91986,#91987,#91988,#91989,
#91990,#91991,#91992,#91993,#91994,#91995,#91996,#91997,#91998,#91999,#92000),
 .UNSPECIFIED.,.F.,.F.,(4,2,2,2,2,2,2,2,2,2,2,2,2,2,2,2,2,2,2,2,2,2,2,2,
2,2,2,2,2,2,2,2,2,2,2,2,2,2,2,2,2,2,2,2,2,2,2,2,2,2,2,2,2,2,2,2,2,2,2,2,
2,2,2,2,2,2,2,2,2,2,2,2,2,2,2,2,2,2,2,2,2,2,2,2,2,2,2,2,2,2,2,2,2,2,2,2,
2,2,2,2,2,2,2,2,2,2,2,2,2,2,2,2,2,2,2,2,2,2,2,2,2,2,2,2,2,2,2,2,4),(-2.66791417378201,
-2.66011988777631,-2.65482313930386,-2.65237961614905,-2.65049765042171,
-2.64865683449738,-2.64683032342862,-2.64428978233245,-2.63909831227884,
-2.62658735449175,-2.5749150821746,-2.55607160762977,-2.54677616300546,
-2.54463317126834,-2.54340497810905,-2.54232991213756,-2.54094098819484,
-2.53802597530639,-2.50832788054379,-2.4578760875252,-2.4483865807636,-2.44377906975308,
-2.43999977866059,-2.43782896495123,-2.43781326973063,-2.43779702190874,
-2.43778020143896,-2.43776278742412,-2.43774475824523,-2.43772609151703,
-2.43770676403998,-2.43768675171188,-2.43766602962809,-2.43764457202056,
-2.43762235216574,-2.43759934167047,-2.43757930447203,-2.43755595309751,
-2.43752874547583,-2.43749705356636,-2.43746015098454,-2.43741719944656,
-2.43736298553626,-2.43542216926865,-2.43288003452889,-2.42858165316826,
-2.39345884284186,-2.34449859829081,-2.33479760947715,-2.33262624841412,
-2.3313919405314,-2.33031805948839,-2.32893923323287,-2.32607523268267,
-2.2901166619028,-2.25734989063278,-2.23478976319528,-2.22913613951212,
-2.22656484650643,-2.22462637742261,-2.22279965521206,-2.22025769292186,
-2.21361644443353,-2.15780940066184,-2.1337456447536,-2.12292178675442,
-2.12067774575561,-2.11942747359353,-2.11835548969604,-2.11699940698459,
-2.11485378640741,-2.10381682253215,-2.05259701171859,-2.02388666735185,
-2.01745269554198,-2.01474390319664,-2.01278214780467,-2.01098948279204,
-2.0081244719523,-2.00123993179152,-1.94816229749233,-1.92225391450773,
-1.91094622475129,-1.90867365474704,-1.90741719076193,-1.90634581212781,
-1.90499803307594,-1.90237634137701,-1.88633367703237,-1.88104245191794,
-1.86645752599065,-1.83356411220798,-1.81699649221149,-1.8066836117489,
-1.80343450454297,-1.80136097306187,-1.79942012963745,-1.79687878844678,
-1.79258360740925,-1.75746994548861,-1.70856299624024,-1.69879210687913,
-1.6966157924424,-1.69538031718803,-1.69430647621343,-1.69292908163961,
-1.69007280912309,-1.66727127306139,-1.611660506485,-1.59564836420045,-1.59187872760401,
-1.58969015458288,-1.5877758610531,-1.58540646714517,-1.58177292300582,
-1.56467493167577,-1.55660605266961,-1.52179402174411,-1.49774304356339,
-1.48692288587444,-1.48467916179566,-1.48342900309034,-1.4823570775557,
-1.48100101874928,-1.47834061639203,-1.46128641298507,-1.44267340483334,
-1.40971563401133,-1.40850263276381),.UNSPECIFIED.);
#922=B_SPLINE_CURVE_WITH_KNOTS('',3,(#92002,#92003,#92004,#92005,#92006,
#92007,#92008,#92009,#92010,#92011,#92012,#92013,#92014,#92015,#92016,#92017,
#92018,#92019,#92020,#92021,#92022,#92023,#92024,#92025,#92026,#92027,#92028,
#92029,#92030,#92031,#92032,#92033,#92034,#92035,#92036,#92037,#92038,#92039,
#92040,#92041,#92042,#92043,#92044,#92045,#92046,#92047,#92048,#92049,#92050,
#92051,#92052,#92053,#92054,#92055,#92056,#92057,#92058,#92059,#92060,#92061,
#92062,#92063,#92064,#92065,#92066,#92067,#92068,#92069,#92070,#92071,#92072,
#92073,#92074,#92075,#92076,#92077,#92078,#92079,#92080,#92081,#92082,#92083,
#92084,#92085,#92086,#92087,#92088,#92089,#92090,#92091,#92092,#92093,#92094,
#92095,#92096,#92097,#92098,#92099,#92100,#92101,#92102,#92103,#92104,#92105,
#92106,#92107,#92108,#92109,#92110,#92111,#92112,#92113,#92114,#92115,#92116,
#92117,#92118,#92119,#92120,#92121,#92122,#92123,#92124,#92125,#92126,#92127,
#92128,#92129,#92130,#92131,#92132,#92133,#92134,#92135,#92136,#92137,#92138,
#92139,#92140,#92141,#92142,#92143,#92144,#92145,#92146,#92147,#92148,#92149,
#92150,#92151,#92152,#92153,#92154,#92155,#92156,#92157,#92158,#92159,#92160,
#92161,#92162,#92163,#92164,#92165,#92166,#92167,#92168,#92169,#92170,#92171,
#92172,#92173,#92174,#92175,#92176,#92177,#92178,#92179,#92180,#92181,#92182,
#92183,#92184,#92185,#92186,#92187,#92188,#92189,#92190,#92191,#92192,#92193,
#92194,#92195,#92196,#92197,#92198,#92199,#92200,#92201,#92202,#92203,#92204,
#92205,#92206,#92207,#92208,#92209,#92210,#92211),.UNSPECIFIED.,.F.,.F.,
(4,2,2,2,2,2,2,2,2,2,2,2,2,2,2,2,2,2,2,2,2,2,2,2,2,2,2,2,2,2,2,2,2,2,2,
2,2,2,2,2,2,2,2,2,2,2,2,2,2,2,2,2,2,2,2,2,2,2,2,2,2,2,2,2,2,2,2,2,2,2,2,
2,2,2,2,2,2,2,2,2,2,2,2,2,2,2,2,2,2,2,2,2,2,2,2,2,2,2,2,2,2,2,2,2,4),(-1.25976204361674,
-1.24626789056776,-1.24250620752153,-1.24029737663238,-1.23838472323266,
-1.23604199837598,-1.23155507448113,-1.19919334391832,-1.15901178270338,
-1.15407895720171,-1.13812873676784,-1.13551216621872,-1.1341654469943,
-1.13309408235513,-1.13183667968111,-1.12955997168365,-1.11818207834973,
-1.09199581744802,-1.03926899084753,-1.03235477190914,-1.02948478617842,
-1.02769115130942,-1.02573006110216,-1.02302534229468,-1.01661594655854,
-0.988116698680607,-0.93718442266636,-0.925703276043635,-0.923530854995222,
-0.922166599381747,-0.921093955434373,-0.919849550069128,-0.917632410998708,
-0.907242337329322,-0.884745543786685,-0.826436712066803,-0.820077262709895,
-0.817581121950843,-0.815766391624696,-0.813821068532292,-0.811206787351942,
-0.805316257970909,-0.780974088587364,-0.730305840290646,-0.71407588728807,
-0.711447286952908,-0.710098030610435,-0.709026564900586,-0.707771263015832,
-0.705503988348638,-0.694288065155435,-0.668734702193589,-0.615102399043116,
-0.608259434399044,-0.605401288048424,-0.603609886083817,-0.601647074328424,
-0.598932331757705,-0.592462826313168,-0.538201382963245,-0.502341072333416,
-0.499482572086244,-0.498104806605431,-0.497031003408468,-0.495795949084924,
-0.49362126492952,-0.483872723874646,-0.43492573468846,-0.399782611955477,
-0.395494880052352,-0.392955855919747,-0.391015565965953,-0.388941444641914,
-0.385688942987294,-0.375344324635835,-0.358708038445344,-0.32578784281186,
-0.307703638288777,-0.290152223210228,-0.287474033309213,-0.286114239796449,
-0.285042105394494,-0.283794855511992,-0.281564166852736,-0.270954727217956,
-0.247671400600385,-0.191963501212568,-0.184499084404424,-0.181536679834136,
-0.17972621909234,-0.177896302471686,-0.175389705980593,-0.170057324587429,
-0.162973596288587,-0.145587511867453,-0.0967120992549064,-0.0782146044816004,
-0.0754712688757332,-0.074116472291463,-0.0730447648057392,-0.0717939694947669,
-0.0695468645916382,-0.0586677900867371,-0.0343929976268521,-0.000629544711740993),
 .UNSPECIFIED.);
#923=B_SPLINE_CURVE_WITH_KNOTS('',3,(#92212,#92213,#92214,#92215,#92216,
#92217,#92218,#92219,#92220,#92221,#92222,#92223,#92224,#92225,#92226,#92227,
#92228,#92229,#92230,#92231,#92232,#92233),.UNSPECIFIED.,.F.,.F.,(4,2,2,
2,2,2,2,2,2,2,4),(-2.66775452449513,-2.64242641789711,-2.63929920756027,
-2.6371529728418,-2.63535203504439,-2.63343794716631,-2.63106861207781,
-2.62743479154457,-2.61032817670121,-2.5981367253121,-2.5933285988703),
 .UNSPECIFIED.);
#924=B_SPLINE_CURVE_WITH_KNOTS('',3,(#92238,#92239,#92240,#92241,#92242,
#92243,#92244,#92245,#92246,#92247,#92248,#92249,#92250,#92251,#92252,#92253,
#92254,#92255,#92256,#92257,#92258,#92259,#92260,#92261,#92262,#92263,#92264,
#92265,#92266,#92267,#92268,#92269,#92270,#92271,#92272,#92273,#92274,#92275,
#92276,#92277,#92278,#92279,#92280,#92281,#92282,#92283,#92284,#92285,#92286,
#92287,#92288,#92289,#92290,#92291,#92292,#92293,#92294,#92295,#92296,#92297,
#92298,#92299,#92300,#92301,#92302,#92303,#92304,#92305,#92306,#92307,#92308,
#92309,#92310,#92311,#92312,#92313,#92314,#92315,#92316,#92317,#92318,#92319,
#92320,#92321,#92322,#92323,#92324,#92325,#92326,#92327,#92328,#92329,#92330,
#92331,#92332,#92333,#92334,#92335,#92336,#92337,#92338,#92339,#92340,#92341,
#92342,#92343,#92344,#92345,#92346,#92347,#92348,#92349,#92350,#92351,#92352,
#92353,#92354,#92355,#92356,#92357,#92358,#92359,#92360,#92361,#92362,#92363,
#92364,#92365,#92366,#92367,#92368,#92369,#92370,#92371,#92372,#92373,#92374,
#92375,#92376,#92377,#92378,#92379,#92380,#92381,#92382,#92383,#92384,#92385,
#92386,#92387,#92388,#92389,#92390,#92391,#92392,#92393,#92394,#92395,#92396,
#92397,#92398,#92399,#92400,#92401,#92402,#92403,#92404,#92405,#92406,#92407,
#92408,#92409,#92410,#92411,#92412,#92413,#92414,#92415,#92416,#92417,#92418,
#92419,#92420,#92421,#92422,#92423,#92424,#92425,#92426,#92427,#92428,#92429,
#92430,#92431,#92432,#92433,#92434,#92435,#92436,#92437,#92438,#92439,#92440,
#92441,#92442,#92443,#92444,#92445,#92446,#92447,#92448,#92449,#92450,#92451,
#92452,#92453,#92454,#92455,#92456,#92457,#92458,#92459,#92460,#92461,#92462,
#92463,#92464,#92465,#92466,#92467,#92468,#92469,#92470,#92471),
 .UNSPECIFIED.,.F.,.F.,(4,2,2,2,2,2,2,2,2,2,2,2,2,2,2,2,2,2,2,2,2,2,2,2,
2,2,2,2,2,2,2,2,2,2,2,2,2,2,2,2,2,2,2,2,2,2,2,2,2,2,2,2,2,2,2,2,2,2,2,2,
2,2,2,2,2,2,2,2,2,2,2,2,2,2,2,2,2,2,2,2,2,2,2,2,2,2,2,2,2,2,2,2,2,2,2,2,
2,2,2,2,2,2,2,2,2,2,2,2,2,2,2,2,2,2,2,2,4),(-1.40847047624389,-1.40132353743621,
-1.37516892029172,-1.36379828879407,-1.36152198615809,-1.36026465228302,
-1.35919325578629,-1.35784637524951,-1.35522913707094,-1.33926698399098,
-1.33432293362518,-1.32867696470249,-1.28171646060601,-1.28027359363999,
-1.26123211568003,-1.25747075147992,-1.25506192387486,-1.2531441471841,
-1.25098196098015,-1.24733225562943,-1.23288148699016,-1.18249250495218,
-1.15282399940257,-1.14990948108709,-1.14852070342273,-1.14744570571998,
-1.14621754955971,-1.14407451199863,-1.13477746815999,-1.11592581565445,
-1.07547220613324,-1.06319340351377,-1.04861348388434,-1.04482747636013,
-1.04261300281901,-1.04070069725353,-1.03836499232274,-1.03391187464162,
-1.00287553876273,-0.954897375402384,-0.940308395336562,-0.937976024716122,
-0.93657877735863,-0.935499972890641,-0.934290700817501,-0.932232964378333,
-0.924037414039032,-0.908470911388692,-0.866886481247444,-0.837982824145689,
-0.833811354540374,-0.831306003015753,-0.829370803329042,-0.827281765548493,
-0.823962525089069,-0.813022721552837,-0.795045740404755,-0.744623372304772,
-0.728417185128947,-0.725789296870255,-0.724440098321774,-0.723368517189738,
-0.722112893355214,-0.719844564322076,-0.708613860326878,-0.683005317714944,
-0.629442127697143,-0.622592155377476,-0.6197326437578,-0.617940839776557,
-0.615977953404556,-0.613263780767158,-0.606798844079358,-0.552721149169341,
-0.516660503930821,-0.51380070335242,-0.512422583726572,-0.511348632467156,
-0.510113552226802,-0.507939167386879,-0.498197653159695,-0.449237789918328,
-0.414102810569857,-0.409806355515815,-0.407264645382177,-0.405323730871823,
-0.403250326791116,-0.40000184254462,-0.389694422842742,-0.37314119418427,
-0.340287527160839,-0.327286384381564,-0.304664081988268,-0.301812395071588,
-0.300435955411729,-0.299362264349971,-0.298126298268855,-0.295947517236464,
-0.286139319552388,-0.237241787200406,-0.202131568657589,-0.197834505157912,
-0.195292756386959,-0.193351997355742,-0.191344263310538,-0.188242470562931,
-0.18461585200755,-0.1778196522977,-0.161438230576098,-0.128729478564262,
-0.0927003701199963,-0.0898402860636551,-0.0884622742363991,-0.0873885216651818,
-0.0861537993203325,-0.0839803536168609,-0.0748537111811377),
 .UNSPECIFIED.);
#925=B_SPLINE_CURVE_WITH_KNOTS('',3,(#92472,#92473,#92474,#92475,#92476,
#92477,#92478,#92479,#92480,#92481,#92482,#92483,#92484,#92485,#92486,#92487,
#92488,#92489,#92490,#92491,#92492,#92493,#92494,#92495,#92496,#92497,#92498,
#92499,#92500,#92501,#92502,#92503,#92504,#92505,#92506,#92507,#92508,#92509,
#92510,#92511,#92512,#92513,#92514,#92515,#92516,#92517,#92518,#92519,#92520,
#92521,#92522,#92523,#92524,#92525,#92526,#92527,#92528,#92529,#92530,#92531,
#92532,#92533,#92534,#92535,#92536,#92537,#92538,#92539,#92540,#92541,#92542,
#92543,#92544,#92545,#92546,#92547,#92548,#92549,#92550,#92551,#92552,#92553,
#92554,#92555,#92556,#92557,#92558,#92559,#92560,#92561,#92562,#92563,#92564,
#92565,#92566,#92567,#92568,#92569,#92570,#92571,#92572,#92573,#92574,#92575,
#92576,#92577,#92578,#92579,#92580,#92581,#92582,#92583,#92584,#92585,#92586,
#92587,#92588,#92589,#92590,#92591,#92592,#92593,#92594,#92595,#92596,#92597,
#92598,#92599,#92600,#92601,#92602,#92603,#92604,#92605,#92606,#92607,#92608,
#92609,#92610,#92611,#92612,#92613,#92614,#92615,#92616,#92617,#92618,#92619,
#92620,#92621,#92622,#92623,#92624,#92625,#92626,#92627,#92628,#92629,#92630,
#92631,#92632,#92633,#92634,#92635,#92636,#92637,#92638,#92639,#92640,#92641,
#92642,#92643,#92644,#92645,#92646,#92647,#92648,#92649,#92650,#92651,#92652,
#92653,#92654,#92655,#92656,#92657,#92658,#92659,#92660,#92661,#92662,#92663,
#92664,#92665,#92666,#92667,#92668,#92669,#92670,#92671,#92672,#92673,#92674,
#92675,#92676,#92677,#92678,#92679,#92680,#92681,#92682,#92683,#92684,#92685,
#92686,#92687,#92688,#92689,#92690,#92691,#92692,#92693,#92694,#92695,#92696,
#92697,#92698,#92699),.UNSPECIFIED.,.F.,.F.,(4,2,2,2,2,2,2,2,2,2,2,2,2,
2,2,2,2,2,2,2,2,2,2,2,2,2,2,2,2,2,2,2,2,2,2,2,2,2,2,2,2,2,2,2,2,2,2,2,2,
2,2,2,2,2,2,2,2,2,2,2,2,2,2,2,2,2,2,2,2,2,2,2,2,2,2,2,2,2,2,2,2,2,2,2,2,
2,2,2,2,2,2,2,2,2,2,2,2,2,2,2,2,2,2,2,2,2,2,2,2,2,2,2,2,4),(-2.5933285988703,
-2.5713850135869,-2.53465311063345,-2.53109031662975,-2.52958349833753,
-2.52849187727579,-2.52746562274084,-2.52572015644279,-2.52097054031788,
-2.48223390396735,-2.45387433170764,-2.43819312672754,-2.43160235540862,
-2.42655929218752,-2.42411494514773,-2.42218777269432,-2.42033606711082,
-2.41715941167392,-2.40829252768649,-2.40629415126029,-2.34856880498957,
-2.32972682356652,-2.32043266344886,-2.31829012472644,-2.317062216487,-2.31598741641377,
-2.31459885778916,-2.31168468857804,-2.28166275286212,-2.23038397264264,
-2.22154907325308,-2.21514345516761,-2.21243963202807,-2.21047893936624,
-2.20868549839706,-2.20581544124244,-2.19889905323656,-2.14626659808653,
-2.12005397553798,-2.10866956701911,-2.10639278493715,-2.10513549074595,
-2.10406431256044,-2.10271794113495,-2.1001023809276,-2.08416605388714,
-2.07847457312878,-2.06416907003625,-2.0312824157178,-2.01472038767583,
-2.00441034798618,-2.00116179537938,-1.99908853605496,-1.99714788992904,
-1.99460672420656,-1.99031165400152,-1.95517416366392,-1.90618645682308,
-1.8965182238893,-1.89434913551788,-1.89311533307694,-1.89204138658685,
-1.89066181467709,-1.88843860206047,-1.87604928123388,-1.8729879344285,
-1.87278968000235,-1.86592217170183,-1.85218958767901,-1.81930667198492,
-1.80275079500559,-1.79244333503107,-1.78919493039683,-1.78712160572002,
-1.78518078616931,-1.78263923138216,-1.77834314051044,-1.74314810052261,
-1.69397665233024,-1.68451701778498,-1.68236243356225,-1.68113177021427,
-1.68005725122178,-1.67867259929824,-1.67577906732336,-1.64974430551735,
-1.61157686690087,-1.58254861834206,-1.57815295809465,-1.57582935992611,
-1.57391773255557,-1.57169358403674,-1.56786528472473,-1.55280376810564,
-1.50063474161939,-1.48178895401521,-1.47249301199153,-1.47035008983546,
-1.46912196625316,-1.46804698056332,-1.4666581859312,-1.46374353480768,
-1.43369701143151,-1.38235474301257,-1.36901439214692,-1.36545930408266,
-1.36331812272215,-1.36139681622109,-1.35895345466862,-1.35507885020997,
-1.33400441802887,-1.27618777129635,-1.26122677147129,-1.25979232650984),
 .UNSPECIFIED.);
#926=B_SPLINE_CURVE_WITH_KNOTS('',3,(#92705,#92706,#92707,#92708),
 .UNSPECIFIED.,.F.,.F.,(4,4),(120.339865594546,120.689851222923),
 .UNSPECIFIED.);
#927=B_SPLINE_CURVE_WITH_KNOTS('',3,(#92709,#92710,#92711,#92712,#92713,
#92714,#92715,#92716,#92717,#92718,#92719,#92720,#92721,#92722,#92723,#92724,
#92725,#92726,#92727,#92728,#92729,#92730,#92731,#92732,#92733,#92734,#92735,
#92736,#92737,#92738,#92739,#92740,#92741,#92742,#92743,#92744,#92745,#92746,
#92747,#92748,#92749,#92750,#92751,#92752,#92753,#92754,#92755,#92756,#92757,
#92758,#92759,#92760,#92761,#92762,#92763,#92764,#92765,#92766,#92767,#92768,
#92769,#92770,#92771,#92772,#92773,#92774,#92775,#92776,#92777,#92778,#92779,
#92780,#92781,#92782,#92783,#92784,#92785,#92786,#92787,#92788,#92789,#92790,
#92791,#92792,#92793,#92794,#92795,#92796,#92797,#92798,#92799,#92800,#92801,
#92802,#92803,#92804,#92805,#92806,#92807,#92808,#92809,#92810,#92811,#92812,
#92813,#92814,#92815,#92816,#92817,#92818,#92819,#92820,#92821,#92822,#92823,
#92824,#92825,#92826,#92827,#92828,#92829,#92830,#92831,#92832,#92833,#92834,
#92835,#92836,#92837,#92838,#92839,#92840,#92841,#92842,#92843,#92844,#92845,
#92846,#92847,#92848,#92849,#92850,#92851,#92852,#92853,#92854,#92855,#92856,
#92857,#92858,#92859,#92860,#92861,#92862,#92863,#92864,#92865,#92866,#92867,
#92868,#92869,#92870,#92871,#92872,#92873,#92874,#92875,#92876,#92877,#92878,
#92879,#92880,#92881,#92882,#92883,#92884,#92885,#92886,#92887,#92888,#92889,
#92890,#92891,#92892,#92893,#92894,#92895,#92896,#92897,#92898,#92899,#92900,
#92901,#92902,#92903,#92904,#92905,#92906,#92907,#92908,#92909,#92910,#92911,
#92912,#92913,#92914,#92915,#92916,#92917,#92918,#92919,#92920,#92921,#92922,
#92923,#92924,#92925,#92926),.UNSPECIFIED.,.F.,.F.,(4,2,2,2,2,2,2,2,2,2,
2,2,2,2,2,2,2,2,2,2,2,2,2,2,2,2,2,2,2,2,2,2,2,2,2,2,2,2,2,2,2,2,2,2,2,2,
2,2,2,2,2,2,2,2,2,2,2,2,2,2,2,2,2,2,2,2,2,2,2,2,2,2,2,2,2,2,2,2,2,2,2,2,
2,2,2,2,2,2,2,2,2,2,2,2,2,2,2,2,2,2,2,2,2,2,2,2,2,2,4),(-2.6676132306845,
-2.64338324964044,-2.63625129884618,-2.63446038505705,-2.63324541682247,
-2.63223633571066,-2.6311617534206,-2.62977571315959,-2.6268746985405,-2.59995420508059,
-2.58627103785683,-2.57475029045549,-2.54617396108281,-2.53227586374139,
-2.52867234232268,-2.52652047555009,-2.52460120080779,-2.52217616405178,
-2.51744440404228,-2.48000654891398,-2.4296553031146,-2.42318139015113,
-2.42128996035042,-2.42027899069394,-2.4192057173042,-2.4178340292279,-2.41563706192836,
-2.40380017738245,-2.34640349851753,-2.32983966017304,-2.31952880759204,
-2.31628016582027,-2.31420688969781,-2.31226625601916,-2.30972514723753,
-2.30543026435078,-2.27030646223537,-2.2213615195394,-2.21164313595713,
-2.2094705913563,-2.2082360302315,-2.20716219796055,-2.20578378645264,-2.20292186238522,
-2.16686121967266,-2.13412928611118,-2.11162313130751,-2.10597684092514,
-2.10340691167659,-2.10146866777271,-2.09964156741848,-2.09709813098796,
-2.09044736649844,-2.03473181990158,-2.01060894251548,-1.99976919264833,
-1.99752420514233,-1.99627373433666,-1.99520178269729,-1.99384600061808,
-1.99118706889081,-1.9741750205537,-1.92396840007978,-1.90638766610325,
-1.89562291339788,-1.89232308685835,-1.89023849623266,-1.88830206139456,
-1.88578752850923,-1.88158416064999,-1.85133516455136,-1.79985544975948,
-1.78786931914926,-1.78555913142079,-1.78429451629283,-1.7832237543346,
-1.7818863064808,-1.77980150186393,-1.76970633312755,-1.76421748453725,
-1.75679098752139,-1.74328323594381,-1.71040120074048,-1.69384735844554,
-1.68354069909977,-1.68029229857287,-1.67821891684895,-1.67627800197455,
-1.67373626185901,-1.66943972208803,-1.63422231967192,-1.58497686288309,
-1.57559917072624,-1.57345036347776,-1.57222094128947,-1.57114616868146,
-1.56975942826541,-1.56751268574364,-1.55467956023738,-1.55251362126544,
-1.50523274194232,-1.47670830799613,-1.47029627829055,-1.46759106545853,
-1.46562984425439,-1.46383624997819,-1.46096666712225,-1.45405514491847,
-1.40847047624389),.UNSPECIFIED.);
#928=B_SPLINE_CURVE_WITH_KNOTS('',3,(#92928,#92929,#92930,#92931,#92932,
#92933,#92934,#92935,#92936,#92937,#92938,#92939,#92940,#92941,#92942,#92943,
#92944,#92945,#92946,#92947,#92948,#92949,#92950,#92951,#92952,#92953,#92954,
#92955,#92956,#92957,#92958,#92959,#92960,#92961,#92962,#92963,#92964,#92965,
#92966,#92967,#92968,#92969,#92970,#92971,#92972,#92973,#92974,#92975,#92976,
#92977,#92978,#92979,#92980,#92981,#92982,#92983,#92984,#92985,#92986,#92987,
#92988,#92989,#92990,#92991,#92992,#92993,#92994,#92995,#92996,#92997,#92998,
#92999,#93000,#93001,#93002,#93003,#93004,#93005,#93006,#93007,#93008,#93009,
#93010,#93011,#93012,#93013,#93014,#93015,#93016,#93017,#93018,#93019,#93020,
#93021,#93022,#93023,#93024,#93025,#93026,#93027,#93028,#93029,#93030,#93031,
#93032,#93033,#93034,#93035,#93036,#93037,#93038,#93039,#93040,#93041,#93042,
#93043,#93044,#93045,#93046,#93047,#93048,#93049,#93050,#93051,#93052,#93053,
#93054,#93055,#93056,#93057,#93058,#93059,#93060,#93061,#93062,#93063,#93064,
#93065,#93066,#93067,#93068,#93069,#93070,#93071,#93072,#93073,#93074,#93075,
#93076,#93077,#93078,#93079,#93080,#93081,#93082,#93083,#93084,#93085,#93086,
#93087,#93088,#93089,#93090,#93091,#93092,#93093,#93094,#93095,#93096,#93097,
#93098,#93099,#93100,#93101,#93102,#93103,#93104,#93105,#93106,#93107,#93108,
#93109,#93110,#93111,#93112,#93113,#93114,#93115,#93116,#93117,#93118,#93119,
#93120,#93121,#93122,#93123,#93124,#93125,#93126,#93127,#93128,#93129,#93130,
#93131,#93132,#93133,#93134,#93135,#93136,#93137,#93138,#93139,#93140,#93141,
#93142,#93143,#93144,#93145,#93146,#93147,#93148,#93149),.UNSPECIFIED.,
 .F.,.F.,(4,2,2,2,2,2,2,2,2,2,2,2,2,2,2,2,2,2,2,2,2,2,2,2,2,2,2,2,2,2,2,
2,2,2,2,2,2,2,2,2,2,2,2,2,2,2,2,2,2,2,2,2,2,2,2,2,2,2,2,2,2,2,2,2,2,2,2,
2,2,2,2,2,2,2,2,2,2,2,2,2,2,2,2,2,2,2,2,2,2,2,2,2,2,2,2,2,2,2,2,2,2,2,2,
2,2,2,2,2,2,2,4),(-1.25979232650984,-1.25887869460015,-1.257476860145,-1.25639744792124,
-1.25519075593238,-1.25314458020512,-1.24508694146706,-1.22990728012695,
-1.19000982666574,-1.15896499636262,-1.15474332494294,-1.15222331171263,
-1.15028583896795,-1.14820325862736,-1.14491325930357,-1.13423929197516,
-1.11686740825185,-1.06816235716437,-1.06164763258783,-1.0490240788199,
-1.04678825533364,-1.04540478332008,-1.04433032453203,-1.04309877832677,
-1.04094038551765,-1.03142842291219,-0.982273251324694,-0.947076531422124,
-0.942780070160903,-0.940238384086857,-0.93829750391988,-0.936224152011337,
-0.932975781834942,-0.922668996577683,-0.906117046141392,-0.873264817914013,
-0.860348802374789,-0.837642971990654,-0.834789282164727,-0.83341246536707,
-0.832338757489996,-0.83110308537762,-0.828925572918464,-0.819135550155312,
-0.770223866655688,-0.735105735444874,-0.730810710321477,-0.728269578319782,
-0.726328951071264,-0.724255704345183,-0.721007154466157,-0.710696895442398,
-0.694136605118975,-0.661279490593475,-0.64750719754613,-0.640733949821207,
-0.638831069639443,-0.62518506433143,-0.622898065909665,-0.62151431800853,
-0.620437452947476,-0.619220807393344,-0.617129085688284,-0.608508670809888,
-0.59171518152647,-0.549743130652129,-0.522869190623174,-0.518751294507463,
-0.516261958164872,-0.514329534457623,-0.512233912916489,-0.50888346897489,
-0.497648193390317,-0.478985423521949,-0.438419364079774,-0.413804379442228,
-0.410920235105802,-0.409537569025515,-0.40846342264519,-0.407231882225821,
-0.405072666057842,-0.395543776896042,-0.346417434759987,-0.311234436668114,
-0.306939103201581,-0.304398064758778,-0.302457667881574,-0.300384821339433,
-0.297137220157524,-0.286832682948307,-0.270284160281976,-0.237937392265993,
-0.201815491921998,-0.198960466844357,-0.197583579605201,-0.196557065839457,
-0.195363678496637,-0.193380718674547,-0.190940950290321,-0.185982530594728,
-0.172431551898505,-0.149608300831557,-0.103071676025014,-0.0958752177108702,
-0.0929587265886628,-0.0911569205292869,-0.0892033973504025,-0.0865388835416779,
-0.0803615103261198,-0.0537591566479666,-0.00062960350502436),
 .UNSPECIFIED.);
#929=B_SPLINE_CURVE_WITH_KNOTS('',3,(#93150,#93151,#93152,#93153,#93154,
#93155,#93156,#93157,#93158,#93159,#93160,#93161,#93162,#93163,#93164,#93165,
#93166,#93167,#93168,#93169,#93170,#93171,#93172,#93173),.UNSPECIFIED.,
 .F.,.F.,(4,2,2,2,2,2,2,2,2,2,2,4),(-2.66811719344424,-2.66005991212222,
-2.65570245956423,-2.65428938514948,-2.65322207097606,-2.65219180145323,
-2.65101182025699,-2.64908649323056,-2.64302060358045,-2.64173852058932,
-2.63393766869622,-2.59385608721132),.UNSPECIFIED.);
#930=B_SPLINE_CURVE_WITH_KNOTS('',3,(#93179,#93180,#93181,#93182,#93183,
#93184,#93185,#93186,#93187,#93188,#93189,#93190,#93191),.UNSPECIFIED.,
 .F.,.F.,(4,3,3,3,4),(114.057240355212,114.163813746624,114.270250447226,
114.376547360035,114.406671945289),.UNSPECIFIED.);
#931=B_SPLINE_CURVE_WITH_KNOTS('',3,(#93192,#93193,#93194,#93195,#93196,
#93197,#93198,#93199,#93200,#93201),.UNSPECIFIED.,.F.,.F.,(4,1,1,1,1,1,
1,4),(114.406674973133,114.866191745616,115.865028195577,116.863864645539,
117.862701095501,118.861537545463,119.860373995425,120.339865594546),
 .UNSPECIFIED.);
#932=B_SPLINE_CURVE_WITH_KNOTS('',3,(#93202,#93203,#93204,#93205,#93206,
#93207,#93208,#93209,#93210,#93211,#93212,#93213,#93214,#93215,#93216,#93217,
#93218,#93219,#93220,#93221,#93222,#93223,#93224,#93225,#93226,#93227,#93228,
#93229,#93230,#93231,#93232,#93233,#93234,#93235,#93236,#93237,#93238,#93239,
#93240,#93241,#93242,#93243,#93244,#93245,#93246,#93247,#93248,#93249,#93250,
#93251,#93252,#93253,#93254,#93255,#93256,#93257,#93258,#93259,#93260,#93261,
#93262,#93263,#93264,#93265,#93266,#93267,#93268,#93269,#93270,#93271,#93272,
#93273,#93274,#93275,#93276,#93277,#93278,#93279,#93280,#93281,#93282,#93283,
#93284,#93285,#93286,#93287,#93288,#93289,#93290,#93291,#93292,#93293,#93294,
#93295,#93296,#93297,#93298,#93299,#93300,#93301,#93302,#93303,#93304,#93305,
#93306,#93307,#93308,#93309,#93310,#93311,#93312,#93313,#93314,#93315,#93316,
#93317,#93318,#93319,#93320,#93321,#93322,#93323,#93324,#93325,#93326,#93327,
#93328,#93329,#93330,#93331,#93332,#93333,#93334,#93335,#93336,#93337,#93338,
#93339,#93340,#93341,#93342,#93343,#93344,#93345,#93346,#93347,#93348,#93349,
#93350,#93351,#93352,#93353,#93354,#93355,#93356,#93357,#93358,#93359,#93360,
#93361,#93362,#93363,#93364,#93365,#93366,#93367,#93368,#93369,#93370,#93371,
#93372,#93373,#93374,#93375,#93376,#93377,#93378,#93379,#93380,#93381,#93382,
#93383,#93384,#93385,#93386,#93387,#93388,#93389,#93390,#93391,#93392,#93393,
#93394,#93395,#93396,#93397,#93398,#93399,#93400,#93401,#93402,#93403,#93404,
#93405,#93406,#93407,#93408,#93409,#93410,#93411,#93412,#93413,#93414,#93415,
#93416,#93417,#93418,#93419,#93420,#93421,#93422,#93423,#93424,#93425,#93426,
#93427,#93428,#93429,#93430,#93431,#93432,#93433,#93434,#93435,#93436,#93437,
#93438,#93439,#93440,#93441,#93442,#93443,#93444,#93445,#93446,#93447,#93448,
#93449,#93450,#93451,#93452,#93453,#93454,#93455,#93456,#93457,#93458,#93459,
#93460,#93461,#93462,#93463,#93464,#93465),.UNSPECIFIED.,.F.,.F.,(4,2,2,
2,2,2,2,2,2,2,2,2,2,2,2,2,2,2,2,2,2,2,2,2,2,2,2,2,2,2,2,2,2,2,2,2,2,2,2,
2,2,2,2,2,2,2,2,2,2,2,2,2,2,2,2,2,2,2,2,2,2,2,2,2,2,2,2,2,2,2,2,2,2,2,2,
2,2,2,2,2,2,2,2,2,2,2,2,2,2,2,2,2,2,2,2,2,2,2,2,2,2,2,2,2,2,2,2,2,2,2,2,
2,2,2,2,2,2,2,2,2,2,2,2,2,2,2,2,2,2,2,2,4),(-2.59385608721132,-2.58073141970544,
-2.56298814981683,-2.55215092037623,-2.54884238281251,-2.54675539781623,
-2.54481887954915,-2.5423072697976,-2.53811544119408,-2.50862542056458,
-2.46750352282329,-2.45206722689791,-2.44665242939645,-2.44405337358974,
-2.44194651736327,-2.44073373600743,-2.44073062156546,-2.44072748826993,
-2.44072433601563,-2.44072116450774,-2.44071797359581,-2.44071476316554,
-2.44071153318834,-2.44070828334381,-2.44070501359305,-2.44070172383806,
-2.44069841395613,-2.44069508393363,-2.44069174629681,-2.4406883941216,
-2.44068502069543,-2.4406816144313,-2.43965466462533,-2.43827707804931,
-2.43541983131054,-2.39931639114125,-2.36659149996972,-2.34409952785361,
-2.33845486533222,-2.33588506236258,-2.33394666324203,-2.33211923237434,
-2.32957503997356,-2.32292052484272,-2.2672286582859,-2.24308328186017,
-2.23223698312491,-2.22999141970881,-2.22874073730073,-2.22766867154095,
-2.22631283141247,-2.22416824302766,-2.21315034930059,-2.1618752647196,
-2.13318530443709,-2.1267534515289,-2.12404485052406,-2.12208297939977,
-2.12029003371052,-2.11742419385461,-2.11053569053077,-2.05749493328063,
-2.031554467432,-2.0202381164397,-2.01796488263818,-2.01670819640877,-2.01563671615603,
-2.01428892117752,-2.01166752769492,-1.99563230439476,-1.99028317553407,
-1.97574260730953,-1.94284634505356,-1.9262776566299,-1.91596400417879,
-1.91271459697753,-1.91064086041,-1.90869981544901,-1.90615819655644,-1.90186251522844,
-1.86674067372041,-1.81781469934133,-1.8080594027981,-1.80588400101227,
-1.80464864891295,-1.80357466208422,-1.80219674977035,-1.79933826555392,
-1.76340771202465,-1.73061857273192,-1.70802945119765,-1.70237137031944,
-1.69979894310503,-1.69785998213037,-1.6960330631888,-1.69349125523593,
-1.68685295790775,-1.63098734605901,-1.59816027156498,-1.59461368759316,
-1.59310930107685,-1.59201777316917,-1.59099027313349,-1.5892398223757,
-1.5844601020464,-1.54728119547981,-1.4970121043773,-1.49060955745954,-1.48790574339682,
-1.48594458825318,-1.48415040087986,-1.48127844389249,-1.47435382986105,
-1.42178270642939,-1.39550755450345,-1.38410585480144,-1.38182757439701,
-1.38056971438782,-1.37949821256404,-1.37815163580577,-1.37553626755946,
-1.35961501635281,-1.35511257552246,-1.33454869744324,-1.28619252276872,
-1.27904322479569,-1.27613386515458,-1.27433279439379,-1.27237717430474,
-1.26970459846511,-1.26348490559208,-1.26001673248898),.UNSPECIFIED.);
#933=B_SPLINE_CURVE_WITH_KNOTS('',3,(#93471,#93472,#93473,#93474,#93475,
#93476,#93477,#93478,#93479,#93480,#93481,#93482,#93483,#93484,#93485,#93486,
#93487,#93488,#93489,#93490),.UNSPECIFIED.,.F.,.F.,(4,2,2,2,2,2,2,2,2,4),
(-0.0747504804368338,-0.0610229392307608,-0.0562870041952136,-0.0545435807646292,
-0.0535177048167566,-0.0524257920513701,-0.0509174388803607,-0.049229620013134,
-0.0462824091130108,-0.000629118632090094),.UNSPECIFIED.);
#934=B_SPLINE_CURVE_WITH_KNOTS('',3,(#93491,#93492,#93493,#93494,#93495,
#93496,#93497,#93498,#93499,#93500,#93501,#93502,#93503,#93504,#93505,#93506,
#93507,#93508,#93509,#93510,#93511,#93512,#93513,#93514,#93515,#93516,#93517,
#93518,#93519,#93520,#93521,#93522,#93523,#93524,#93525,#93526,#93527,#93528,
#93529,#93530,#93531,#93532,#93533,#93534,#93535,#93536,#93537,#93538,#93539,
#93540,#93541,#93542,#93543,#93544,#93545,#93546,#93547,#93548,#93549,#93550,
#93551,#93552,#93553,#93554,#93555,#93556,#93557,#93558,#93559,#93560,#93561,
#93562,#93563,#93564,#93565,#93566,#93567,#93568,#93569,#93570,#93571,#93572,
#93573,#93574,#93575,#93576,#93577,#93578,#93579,#93580,#93581,#93582,#93583,
#93584,#93585,#93586,#93587,#93588,#93589,#93590,#93591,#93592,#93593,#93594,
#93595,#93596,#93597,#93598,#93599,#93600,#93601,#93602,#93603,#93604,#93605,
#93606,#93607,#93608,#93609,#93610,#93611,#93612,#93613,#93614,#93615,#93616,
#93617,#93618,#93619,#93620,#93621,#93622,#93623,#93624,#93625,#93626,#93627,
#93628,#93629,#93630,#93631,#93632,#93633,#93634,#93635,#93636,#93637,#93638,
#93639,#93640,#93641,#93642,#93643,#93644,#93645,#93646,#93647,#93648,#93649,
#93650,#93651,#93652,#93653,#93654,#93655,#93656,#93657,#93658,#93659,#93660,
#93661,#93662,#93663,#93664,#93665,#93666,#93667,#93668,#93669,#93670,#93671),
 .UNSPECIFIED.,.F.,.F.,(4,3,3,3,3,3,3,3,3,3,3,3,3,3,3,3,3,3,3,3,3,3,3,3,
3,3,3,3,3,3,3,3,3,3,3,3,3,3,3,3,3,3,3,3,3,3,3,3,3,3,3,3,3,3,3,3,3,3,3,3,
4),(108.12348663811,108.225421296431,108.327291076164,108.429131491865,
108.530978014042,108.632930880402,108.734945943835,108.837130903884,108.873173045844,
108.976567782892,109.079809065007,109.1829290304,109.285983598609,109.389006806967,
109.492032649639,109.595165416418,109.698354507828,109.80172650121,109.872009495806,
109.975404232854,110.078645514969,110.181765480362,110.284820048571,110.387843256928,
110.490869099601,110.594001866379,110.697190957789,110.800562951171,110.870845945768,
110.974240682816,111.077481964931,111.180601930323,111.283656498532,111.38667970689,
111.489705549562,111.59283831634,111.69602740775,111.799399401132,111.86968239573,
111.973077132778,112.076318414893,112.179438380285,112.282492948494,112.385516156852,
112.488541999524,112.591674766302,112.694863857712,112.798235851094,112.868518845692,
112.97191358274,113.075154864855,113.178274830247,113.281329398456,113.384352606814,
113.487378449486,113.590511216265,113.693700307674,113.797072301056,113.867355295654,
113.974272639427,114.057240355212),.UNSPECIFIED.);
#935=B_SPLINE_CURVE_WITH_KNOTS('',3,(#93673,#93674,#93675,#93676,#93677,
#93678,#93679,#93680,#93681,#93682,#93683,#93684,#93685,#93686,#93687,#93688,
#93689,#93690,#93691,#93692,#93693,#93694,#93695,#93696,#93697,#93698,#93699,
#93700,#93701,#93702,#93703,#93704,#93705,#93706,#93707,#93708,#93709,#93710,
#93711,#93712,#93713,#93714,#93715,#93716,#93717,#93718,#93719,#93720,#93721,
#93722,#93723,#93724,#93725,#93726,#93727,#93728,#93729,#93730,#93731,#93732,
#93733,#93734,#93735,#93736,#93737,#93738,#93739,#93740,#93741,#93742,#93743,
#93744,#93745,#93746,#93747,#93748,#93749,#93750,#93751,#93752,#93753,#93754,
#93755,#93756,#93757,#93758,#93759,#93760,#93761,#93762,#93763,#93764,#93765,
#93766,#93767,#93768,#93769,#93770,#93771,#93772,#93773,#93774,#93775,#93776,
#93777,#93778,#93779,#93780,#93781,#93782,#93783,#93784,#93785,#93786,#93787,
#93788,#93789,#93790,#93791,#93792,#93793,#93794,#93795,#93796,#93797,#93798,
#93799,#93800,#93801,#93802,#93803,#93804,#93805,#93806,#93807,#93808,#93809,
#93810,#93811,#93812,#93813,#93814,#93815,#93816,#93817,#93818,#93819,#93820,
#93821,#93822,#93823,#93824,#93825,#93826,#93827,#93828,#93829,#93830,#93831,
#93832,#93833,#93834,#93835,#93836,#93837,#93838,#93839,#93840,#93841,#93842,
#93843,#93844,#93845,#93846,#93847,#93848,#93849,#93850,#93851,#93852,#93853,
#93854,#93855,#93856,#93857,#93858,#93859,#93860,#93861,#93862,#93863,#93864,
#93865,#93866,#93867,#93868,#93869,#93870,#93871,#93872,#93873,#93874,#93875,
#93876,#93877,#93878,#93879,#93880,#93881,#93882,#93883,#93884),
 .UNSPECIFIED.,.F.,.F.,(4,2,2,2,2,2,2,2,2,2,2,2,2,2,2,2,2,2,2,2,2,2,2,2,
2,2,2,2,2,2,2,2,2,2,2,2,2,2,2,2,2,2,2,2,2,2,2,2,2,2,2,2,2,2,2,2,2,2,2,2,
2,2,2,2,2,2,2,2,2,2,2,2,2,2,2,2,2,2,2,2,2,2,2,2,2,2,2,2,2,2,2,2,2,2,2,2,
2,2,2,2,2,2,2,2,2,4),(-1.26001673248898,-1.23655150319919,-1.1960244005873,
-1.17303176546317,-1.17017627503209,-1.16879893880593,-1.16772499008992,
-1.16648922628762,-1.1643119961818,-1.15453060214934,-1.10560003838702,
-1.0704718400195,-1.06617590381112,-1.06363424451392,-1.0616932213409,-1.05961955819117,
-1.05637036951425,-1.04605819850218,-1.02949494693346,-0.996631493386167,
-0.982888777196495,-0.97603751757564,-0.975722598573606,-0.970126884729276,
-0.960136099439734,-0.958058402905608,-0.956723082636457,-0.955652354111854,
-0.95438582607862,-0.952067046950757,-0.93992193780193,-0.886829788270533,
-0.858243183207196,-0.854080297338155,-0.851577575854991,-0.849642918693378,
-0.847552988978721,-0.844229155057207,-0.833245225473433,-0.815166213195005,
-0.765171947559398,-0.748719770289822,-0.746082303757109,-0.744731118606094,
-0.743659491677619,-0.742405584500435,-0.740144827460915,-0.729041271701423,
-0.703921333791985,-0.649652501817749,-0.642863142352808,-0.640013817473809,
-0.63822396949094,-0.636259643748768,-0.633536870067639,-0.627019737160957,
-0.597610422704946,-0.547778395772928,-0.536270427898126,-0.534096518244313,
-0.532731845752754,-0.53165921532109,-0.530415215220287,-0.528199753886121,
-0.517834773527705,-0.495425778723237,-0.436976136933484,-0.430637133734412,
-0.428144493578436,-0.426330729075971,-0.424384955839965,-0.421767476504563,
-0.415858630299923,-0.391374517538276,-0.340791600172706,-0.324645044531388,
-0.322019897969256,-0.320671425051768,-0.319600062427207,-0.31834428032371,
-0.316074615292846,-0.304815993342912,-0.279095691977376,-0.225710228401517,
-0.218851161607306,-0.216045421859833,-0.214085270360473,-0.212146077489487,
-0.210185605847257,-0.20510920916554,-0.163994077671629,-0.115019541214979,
-0.110791312769733,-0.109127212088262,-0.10811666717333,-0.107013195298084,
-0.105442007963851,-0.101489753644222,-0.0819012664742417,-0.0267278938264957,
-0.0187639942637725,-0.00802108705316168,-0.00466632877897281,-0.00258130086811506,
-0.00128118378586622,-0.000628942594787886),.UNSPECIFIED.);
#936=B_SPLINE_CURVE_WITH_KNOTS('',3,(#93885,#93886,#93887,#93888,#93889,
#93890,#93891,#93892,#93893,#93894,#93895,#93896,#93897),.UNSPECIFIED.,
 .F.,.F.,(4,3,3,3,4),(-104.372003947921,-104.263735348689,-104.155311094115,
-104.04663122551,-104.022525394709),.UNSPECIFIED.);
#937=B_SPLINE_CURVE_WITH_KNOTS('',3,(#93902,#93903,#93904,#93905,#93906,
#93907,#93908,#93909,#93910,#93911,#93912,#93913,#93914,#93915,#93916,#93917,
#93918,#93919,#93920,#93921,#93922,#93923,#93924,#93925,#93926,#93927,#93928,
#93929,#93930,#93931,#93932,#93933,#93934,#93935,#93936,#93937,#93938,#93939,
#93940,#93941,#93942,#93943,#93944,#93945,#93946,#93947,#93948,#93949,#93950,
#93951,#93952,#93953,#93954,#93955,#93956,#93957,#93958,#93959,#93960,#93961,
#93962,#93963,#93964,#93965,#93966,#93967,#93968,#93969,#93970,#93971,#93972,
#93973,#93974,#93975,#93976,#93977,#93978,#93979,#93980,#93981,#93982,#93983,
#93984,#93985,#93986,#93987,#93988,#93989,#93990,#93991,#93992,#93993,#93994,
#93995,#93996,#93997,#93998,#93999,#94000,#94001,#94002,#94003,#94004,#94005,
#94006,#94007,#94008,#94009,#94010,#94011,#94012,#94013,#94014,#94015,#94016,
#94017,#94018,#94019,#94020,#94021,#94022,#94023,#94024,#94025,#94026,#94027,
#94028,#94029,#94030,#94031,#94032,#94033,#94034,#94035,#94036,#94037,#94038,
#94039,#94040,#94041,#94042,#94043,#94044,#94045,#94046,#94047,#94048,#94049,
#94050,#94051,#94052,#94053,#94054,#94055,#94056,#94057,#94058,#94059,#94060,
#94061,#94062,#94063,#94064,#94065,#94066,#94067,#94068,#94069,#94070,#94071,
#94072,#94073,#94074,#94075,#94076,#94077,#94078,#94079,#94080,#94081,#94082,
#94083,#94084,#94085,#94086,#94087,#94088,#94089,#94090,#94091,#94092,#94093,
#94094,#94095,#94096,#94097,#94098,#94099,#94100,#94101,#94102,#94103,#94104,
#94105,#94106,#94107,#94108,#94109,#94110,#94111,#94112,#94113,#94114,#94115,
#94116,#94117,#94118,#94119,#94120,#94121),.UNSPECIFIED.,.F.,.F.,(4,2,2,
2,2,2,2,2,2,2,2,2,2,2,2,2,2,2,2,2,2,2,2,2,2,2,2,2,2,2,2,2,2,2,2,2,2,2,2,
2,2,2,2,2,2,2,2,2,2,2,2,2,2,2,2,2,2,2,2,2,2,2,2,2,2,2,2,2,2,2,2,2,2,2,2,
2,2,2,2,2,2,2,2,2,2,2,2,2,2,2,2,2,2,2,2,2,2,2,2,2,2,2,2,2,2,2,2,2,2,4),
(-1.40835487559167,-1.37307254520199,-1.33396207472922,-1.33297746517486,
-1.32826978765958,-1.32653031463525,-1.32550498877885,-1.32441215764762,
-1.32290008276663,-1.31930842386976,-1.28016549281244,-1.23134373312473,
-1.22421242156571,-1.22130615748429,-1.21950571749395,-1.21754976684994,
-1.21487491042775,-1.2086415661001,-1.18159630862061,-1.14087068534051,
-1.11820873836828,-1.11535577022776,-1.1139789680588,-1.11290511464636,
-1.11166909773012,-1.10949055300009,-1.09968883730141,-1.05077809615156,
-1.01565733039017,-1.01136167397369,-1.00882015705595,-1.00687922927664,
-1.00480565510356,-1.00155657882795,-0.991244536713203,-0.974681275199111,
-0.941818720452031,-0.928012557124597,-0.921312351597458,-0.905864994709904,
-0.903497100064906,-0.902089524132845,-0.901009368767303,-0.89980591626645,
-0.897774099278516,-0.889883702582577,-0.875166035499657,-0.84610338411909,
-0.803698163326376,-0.799404690588919,-0.796863863675753,-0.794923116069078,
-0.792849398062927,-0.789599393966096,-0.779278480917498,-0.762695330217843,
-0.729817122474957,-0.714522520717224,-0.709793783754855,-0.693941562126337,
-0.69132874945633,-0.68998289233584,-0.688911648318208,-0.687653731154015,
-0.685374419532334,-0.673948879812471,-0.647572481410561,-0.595122290936872,
-0.588188792099026,-0.585315747864345,-0.583521640853107,-0.581561188251501,
-0.57885945895549,-0.572467087930835,-0.526046496549813,-0.484947955450101,
-0.480263099025422,-0.478527317137722,-0.477502866303812,-0.476409862013194,
-0.474895740954519,-0.471290879544853,-0.432950124987159,-0.383317359767356,
-0.376221657164208,-0.373321731259076,-0.371522737828785,-0.369566395509398,
-0.366887460196501,-0.360806573922974,-0.352445743392808,-0.301551263215531,
-0.270313240974031,-0.267401273577692,-0.266013096591154,-0.264938280807216,
-0.263710015850866,-0.261566046808897,-0.252414963614524,-0.203666418748164,
-0.167704289658466,-0.162982355603723,-0.16055955706944,-0.158640675515175,
-0.156487801539827,-0.154258046046508,-0.14661209264506,-0.121083042627241,
-0.100337614168057,-0.0747504804368338),.UNSPECIFIED.);
#938=B_SPLINE_CURVE_WITH_KNOTS('',3,(#94123,#94124,#94125,#94126,#94127,
#94128,#94129,#94130,#94131,#94132,#94133,#94134,#94135,#94136,#94137,#94138,
#94139,#94140,#94141,#94142,#94143,#94144,#94145,#94146,#94147,#94148,#94149,
#94150,#94151,#94152,#94153,#94154,#94155,#94156,#94157,#94158,#94159,#94160,
#94161,#94162,#94163,#94164,#94165,#94166,#94167,#94168,#94169,#94170,#94171,
#94172,#94173,#94174,#94175,#94176,#94177,#94178,#94179,#94180,#94181,#94182,
#94183,#94184,#94185,#94186,#94187,#94188,#94189,#94190,#94191,#94192,#94193,
#94194,#94195,#94196,#94197,#94198,#94199,#94200,#94201,#94202,#94203,#94204,
#94205,#94206,#94207,#94208,#94209,#94210,#94211,#94212,#94213,#94214,#94215,
#94216,#94217,#94218,#94219,#94220,#94221,#94222,#94223,#94224,#94225,#94226,
#94227,#94228,#94229,#94230,#94231,#94232,#94233,#94234,#94235,#94236,#94237,
#94238,#94239,#94240,#94241,#94242,#94243,#94244,#94245,#94246,#94247,#94248,
#94249,#94250,#94251,#94252,#94253,#94254,#94255,#94256,#94257,#94258,#94259,
#94260,#94261,#94262,#94263,#94264,#94265,#94266,#94267,#94268,#94269,#94270,
#94271,#94272,#94273,#94274,#94275,#94276,#94277,#94278,#94279,#94280,#94281,
#94282,#94283,#94284,#94285,#94286,#94287,#94288,#94289,#94290,#94291,#94292,
#94293,#94294,#94295,#94296,#94297,#94298,#94299,#94300,#94301,#94302,#94303),
 .UNSPECIFIED.,.F.,.F.,(4,3,3,3,3,3,3,3,3,3,3,3,3,3,3,3,3,3,3,3,3,3,3,3,
3,3,3,3,3,3,3,3,3,3,3,3,3,3,3,3,3,3,3,3,3,3,3,3,3,3,3,3,3,3,3,3,3,3,3,3,
4),(-104.022525394709,-103.913514251471,-103.878990796035,-103.775596058987,
-103.672354776872,-103.569234811479,-103.46618024327,-103.363157034912,
-103.260131192239,-103.156998425461,-103.053809334051,-102.950437340669,
-102.880154346073,-102.776759609025,-102.67351832691,-102.570398361518,
-102.467343793309,-102.364320584951,-102.261294742278,-102.1581619755,-102.05497288409,
-101.951600890709,-101.881317896111,-101.777923159063,-101.674681876948,
-101.571561911556,-101.468507343347,-101.365484134989,-101.262458292317,
-101.159325525539,-101.056136434129,-100.952764440747,-100.882481446149,
-100.779086709101,-100.675845426986,-100.572725461594,-100.469670893385,
-100.366647685027,-100.263621842355,-100.160489075577,-100.057299984167,
-99.9539279907855,-99.8836449961874,-99.7802502591395,-99.6770089770245,
-99.5738890116322,-99.4708344434233,-99.3678112350656,-99.264785392393,
-99.161652625615,-99.0584635342052,-98.9550915408236,-98.8848085462255,
-98.7829332776307,-98.681193284401,-98.5795525376357,-98.477975149917,-98.3763829554479,
-98.274788368223,-98.1730805291727,-98.0888188327633),.UNSPECIFIED.);
#939=B_SPLINE_CURVE_WITH_KNOTS('',3,(#94304,#94305,#94306,#94307,#94308),
 .UNSPECIFIED.,.F.,.F.,(4,1,4),(-98.0888186411165,-97.8859720962637,-97.7379482602774),
 .UNSPECIFIED.);
#940=B_SPLINE_CURVE_WITH_KNOTS('',3,(#94314,#94315,#94316,#94317,#94318,
#94319,#94320,#94321,#94322,#94323,#94324,#94325,#94326,#94327,#94328,#94329,
#94330,#94331,#94332,#94333,#94334,#94335),.UNSPECIFIED.,.F.,.F.,(4,2,2,
2,2,2,2,2,2,2,4),(-0.0750517120388601,-0.0634020272158219,-0.0604359224018296,
-0.0436144791537637,-0.0399995549168394,-0.0376361167675147,-0.0357225185227288,
-0.0339209992284383,-0.0317709128135895,-0.0286342845934152,-0.000628474799356472),
 .UNSPECIFIED.);
#941=B_SPLINE_CURVE_WITH_KNOTS('',3,(#94336,#94337,#94338,#94339,#94340,
#94341,#94342,#94343,#94344,#94345,#94346,#94347,#94348,#94349,#94350,#94351,
#94352,#94353,#94354,#94355,#94356,#94357,#94358,#94359,#94360,#94361,#94362,
#94363,#94364,#94365,#94366,#94367,#94368,#94369,#94370,#94371,#94372,#94373,
#94374,#94375,#94376,#94377,#94378,#94379,#94380,#94381,#94382,#94383,#94384,
#94385,#94386,#94387,#94388,#94389,#94390,#94391,#94392,#94393,#94394,#94395,
#94396,#94397,#94398,#94399,#94400,#94401,#94402,#94403,#94404,#94405,#94406,
#94407,#94408,#94409,#94410,#94411,#94412,#94413,#94414,#94415,#94416,#94417,
#94418,#94419,#94420,#94421,#94422,#94423,#94424,#94425,#94426,#94427,#94428,
#94429,#94430,#94431,#94432,#94433,#94434,#94435,#94436,#94437,#94438,#94439,
#94440,#94441,#94442,#94443,#94444,#94445,#94446,#94447,#94448,#94449,#94450,
#94451,#94452,#94453,#94454,#94455,#94456,#94457,#94458,#94459,#94460,#94461,
#94462,#94463,#94464,#94465,#94466,#94467,#94468,#94469,#94470,#94471,#94472,
#94473,#94474,#94475,#94476,#94477,#94478,#94479,#94480,#94481,#94482,#94483,
#94484,#94485,#94486,#94487,#94488,#94489,#94490,#94491,#94492,#94493,#94494,
#94495,#94496,#94497,#94498,#94499,#94500,#94501,#94502,#94503,#94504,#94505,
#94506,#94507,#94508,#94509,#94510,#94511,#94512,#94513,#94514,#94515,#94516,
#94517,#94518,#94519,#94520,#94521,#94522,#94523,#94524,#94525,#94526,#94527,
#94528,#94529,#94530,#94531,#94532,#94533,#94534,#94535,#94536,#94537,#94538,
#94539,#94540,#94541,#94542,#94543,#94544,#94545,#94546,#94547,#94548,#94549,
#94550,#94551,#94552,#94553,#94554,#94555,#94556,#94557),.UNSPECIFIED.,
 .F.,.F.,(4,2,2,2,2,2,2,2,2,2,2,2,2,2,2,2,2,2,2,2,2,2,2,2,2,2,2,2,2,2,2,
2,2,2,2,2,2,2,2,2,2,2,2,2,2,2,2,2,2,2,2,2,2,2,2,2,2,2,2,2,2,2,2,2,2,2,2,
2,2,2,2,2,2,2,2,2,2,2,2,2,2,2,2,2,2,2,2,2,2,2,2,2,2,2,2,2,2,2,2,2,2,2,2,
2,2,2,2,2,2,2,4),(-2.66763698055154,-2.62406132926978,-2.60408125324982,
-2.60008719792512,-2.59850914862046,-2.59740414699734,-2.59639472646751,
-2.59473746711411,-2.59055157721239,-2.5405210743688,-2.51637322760607,
-2.50454754215916,-2.49656808709728,-2.49362515114192,-2.49183396792167,
-2.48989323829761,-2.48735333064289,-2.4830634488436,-2.44793672455365,
-2.39902535700703,-2.38925433004982,-2.38707788654155,-2.38584232285153,
-2.38476839530661,-2.38339087700578,-2.38053430428018,-2.35748862309685,
-2.31189038376125,-2.28922915612821,-2.2835614525403,-2.28098732924355,
-2.27904817786268,-2.27722187816149,-2.27468221218954,-2.26805709348043,
-2.21208953581673,-2.18811951732637,-2.1773202970419,-2.17507749882885,
-2.17382737629828,-2.17275518583563,-2.17139841206732,-2.1692508923137,
-2.1581870041224,-2.10689039676946,-2.07825808558725,-2.07183293481812,
-2.06912537405989,-2.06716360905802,-2.06537031487206,-2.06250294852276,
-2.05560575299052,-2.00267094463175,-1.97665318563582,-1.96531689598131,
-1.96304242698115,-1.96178542969317,-1.96071390982458,-1.95936635215361,
-1.95674626440744,-1.94073469003329,-1.93573867539908,-1.93132393603383,
-1.89233935142684,-1.86585640669193,-1.85969308426041,-1.85703032509592,
-1.85507646846316,-1.85327322083275,-1.85035184993496,-1.8431307686578,
-1.79858280033235,-1.78473559685624,-1.76327650800007,-1.75318374826895,
-1.75098568762849,-1.74974536357142,-1.7486720627611,-1.74730154345496,
-1.74510875810344,-1.7333397544113,-1.72962685146761,-1.72236555834075,
-1.67901009052207,-1.66042268314643,-1.6492198747353,-1.64587221252619,
-1.64377679847104,-1.64184352623183,-1.63935164536473,-1.6352264317297,
-1.60809055958966,-1.56616636875005,-1.54954736470946,-1.54098478387904,
-1.53889723321266,-1.53768129423243,-1.53660390200266,-1.53521797705394,
-1.53292427051012,-1.51915032158516,-1.50784480255644,-1.46844818274825,
-1.44187537801273,-1.43570086543967,-1.43303615705244,-1.43108195608314,
-1.42927915315622,-1.42636020630751,-1.41915354224474,-1.40835487559167),
 .UNSPECIFIED.);
#942=B_SPLINE_CURVE_WITH_KNOTS('',3,(#94559,#94560,#94561,#94562,#94563,
#94564,#94565,#94566,#94567,#94568),.UNSPECIFIED.,.F.,.F.,(4,1,1,1,1,1,
1,4),(-97.7379482602774,-96.8871356463018,-95.8882991963399,-94.889462746378,
-93.8906262964162,-92.8917898464543,-91.8929533964924,-91.8056333339369),
 .UNSPECIFIED.);
#943=B_SPLINE_CURVE_WITH_KNOTS('',3,(#94569,#94570,#94571,#94572,#94573,
#94574,#94575,#94576),.UNSPECIFIED.,.F.,.F.,(4,2,2,4),(-2.66772514762063,
-2.61547416970725,-2.59711068312006,-2.59328853658183),.UNSPECIFIED.);
#944=B_SPLINE_CURVE_WITH_KNOTS('',3,(#94581,#94582,#94583,#94584,#94585,
#94586,#94587,#94588,#94589,#94590,#94591,#94592,#94593,#94594,#94595,#94596,
#94597,#94598,#94599,#94600,#94601,#94602,#94603,#94604,#94605,#94606,#94607,
#94608,#94609,#94610,#94611,#94612,#94613,#94614,#94615,#94616,#94617,#94618,
#94619,#94620,#94621,#94622,#94623,#94624,#94625,#94626,#94627,#94628,#94629,
#94630,#94631,#94632,#94633,#94634,#94635,#94636,#94637,#94638,#94639,#94640,
#94641,#94642,#94643,#94644,#94645,#94646,#94647,#94648,#94649,#94650,#94651,
#94652,#94653,#94654,#94655,#94656,#94657,#94658,#94659,#94660,#94661,#94662,
#94663,#94664,#94665,#94666,#94667,#94668,#94669,#94670,#94671,#94672,#94673,
#94674,#94675,#94676,#94677,#94678,#94679,#94680,#94681,#94682,#94683,#94684,
#94685,#94686,#94687,#94688,#94689,#94690,#94691,#94692,#94693,#94694,#94695,
#94696,#94697,#94698,#94699,#94700,#94701,#94702,#94703,#94704,#94705,#94706,
#94707,#94708,#94709,#94710,#94711,#94712,#94713,#94714,#94715,#94716,#94717,
#94718,#94719,#94720,#94721,#94722,#94723,#94724,#94725,#94726,#94727,#94728,
#94729,#94730,#94731,#94732,#94733,#94734,#94735,#94736,#94737,#94738,#94739,
#94740,#94741,#94742,#94743,#94744,#94745,#94746,#94747,#94748,#94749,#94750,
#94751,#94752,#94753,#94754,#94755,#94756,#94757,#94758,#94759,#94760,#94761,
#94762,#94763,#94764,#94765,#94766,#94767,#94768,#94769,#94770,#94771,#94772,
#94773,#94774,#94775,#94776,#94777,#94778,#94779,#94780,#94781,#94782,#94783,
#94784,#94785,#94786,#94787,#94788,#94789,#94790,#94791,#94792,#94793,#94794,
#94795,#94796),.UNSPECIFIED.,.F.,.F.,(4,2,2,2,2,2,2,2,2,2,2,2,2,2,2,2,2,
2,2,2,2,2,2,2,2,2,2,2,2,2,2,2,2,2,2,2,2,2,2,2,2,2,2,2,2,2,2,2,2,2,2,2,2,
2,2,2,2,2,2,2,2,2,2,2,2,2,2,2,2,2,2,2,2,2,2,2,2,2,2,2,2,2,2,2,2,2,2,2,2,
2,2,2,2,2,2,2,2,2,2,2,2,2,2,2,2,2,2,4),(-1.40856923606383,-1.37753534771955,
-1.33437657332176,-1.31573891594647,-1.3120061968455,-1.30960628755538,
-1.30768951854701,-1.30552196583,-1.30184736841551,-1.28708445286655,-1.25915940004959,
-1.20936248341951,-1.20515952976254,-1.20349955493878,-1.20248976234215,
-1.20138551989213,-1.19981053362183,-1.19583462843233,-1.17602196558166,
-1.14710916065381,-1.10479021809735,-1.10049510372887,-1.09795386327688,
-1.09601312115518,-1.09393972062583,-1.09069086485238,-1.08037908770372,
-1.06381583815358,-1.03095505388635,-1.01702991026295,-1.01060149811018,
-0.99501784778292,-0.992416272356635,-0.99107287879295,-0.990001836063541,
-0.988742108789686,-0.986454280833403,-0.974876064563483,-0.947886078247631,
-0.896303554775745,-0.889312743805389,-0.886430318131219,-0.884634560714498,
-0.882675665973707,-0.879982209663275,-0.873638078681677,-0.845678864518596,
-0.799178081163946,-0.783068285307751,-0.780441711403226,-0.77909295100005,
-0.778021593748141,-0.776766088572937,-0.774497609916402,-0.763258791406917,
-0.737615135793081,-0.684120852360988,-0.677267512448455,-0.674407789435915,
-0.672616199818987,-0.670653827861174,-0.667940880716456,-0.661481313481932,
-0.607554754257518,-0.571347485437789,-0.568493308914977,-0.567116455231962,
-0.566042811664781,-0.564807318673821,-0.56263037346325,-0.552847073374781,
-0.503933837770377,-0.468823844809091,-0.464525049280988,-0.461982917923506,
-0.460042236207826,-0.457969618093723,-0.454723486350996,-0.444432967339147,
-0.427915840221092,-0.371222029924013,-0.358723107565275,-0.356494168675288,
-0.355112906516237,-0.354038846722208,-0.352806275989511,-0.350642575110138,
-0.341050887842663,-0.2919753618443,-0.256812359758064,-0.252513848206065,
-0.249971815109268,-0.248031168310692,-0.246240519153969,-0.243303174156408,
-0.235328939247043,-0.223525724651994,-0.190999540386583,-0.150078407977255,
-0.145387637847395,-0.143651113117761,-0.142626620365515,-0.141533908489056,
-0.140020743226501,-0.136420702779226,-0.0985274263552539,-0.0757357778527809,
-0.0750517120388601),.UNSPECIFIED.);
#945=B_SPLINE_CURVE_WITH_KNOTS('',3,(#94797,#94798,#94799,#94800,#94801,
#94802,#94803,#94804,#94805,#94806,#94807,#94808,#94809,#94810,#94811,#94812,
#94813,#94814,#94815,#94816,#94817,#94818,#94819,#94820,#94821,#94822,#94823,
#94824,#94825,#94826,#94827,#94828,#94829,#94830,#94831,#94832,#94833,#94834,
#94835,#94836,#94837,#94838,#94839,#94840,#94841,#94842,#94843,#94844,#94845,
#94846,#94847,#94848,#94849,#94850,#94851,#94852,#94853,#94854,#94855,#94856,
#94857,#94858,#94859,#94860,#94861,#94862,#94863,#94864,#94865,#94866,#94867,
#94868,#94869,#94870,#94871,#94872,#94873,#94874,#94875,#94876,#94877,#94878,
#94879,#94880,#94881,#94882,#94883,#94884,#94885,#94886,#94887,#94888,#94889,
#94890,#94891,#94892,#94893,#94894,#94895,#94896,#94897,#94898,#94899,#94900,
#94901,#94902,#94903,#94904,#94905,#94906,#94907,#94908,#94909,#94910,#94911,
#94912,#94913,#94914,#94915,#94916,#94917,#94918,#94919,#94920,#94921,#94922,
#94923,#94924,#94925,#94926,#94927,#94928,#94929,#94930,#94931,#94932,#94933,
#94934,#94935,#94936,#94937,#94938,#94939,#94940,#94941,#94942,#94943,#94944,
#94945,#94946,#94947,#94948,#94949,#94950,#94951,#94952,#94953,#94954,#94955,
#94956,#94957,#94958,#94959,#94960,#94961,#94962,#94963,#94964,#94965,#94966,
#94967,#94968,#94969,#94970,#94971,#94972,#94973,#94974,#94975,#94976,#94977,
#94978,#94979,#94980,#94981,#94982,#94983,#94984,#94985,#94986,#94987,#94988,
#94989,#94990,#94991,#94992,#94993,#94994,#94995,#94996,#94997,#94998,#94999,
#95000,#95001,#95002,#95003,#95004,#95005,#95006,#95007,#95008,#95009,#95010,
#95011,#95012,#95013,#95014,#95015,#95016,#95017,#95018,#95019,#95020,#95021,
#95022,#95023,#95024,#95025,#95026,#95027,#95028,#95029,#95030,#95031,#95032,
#95033,#95034,#95035,#95036,#95037,#95038,#95039,#95040,#95041,#95042,#95043,
#95044,#95045,#95046,#95047,#95048,#95049,#95050,#95051,#95052,#95053,#95054,
#95055,#95056,#95057,#95058,#95059,#95060,#95061,#95062,#95063,#95064,#95065,
#95066,#95067,#95068,#95069,#95070),.UNSPECIFIED.,.F.,.F.,(4,2,2,2,2,2,
2,2,2,2,2,2,2,2,2,2,2,2,2,2,2,2,2,2,2,2,2,2,2,2,2,2,2,2,2,2,2,2,2,2,2,2,
2,2,2,2,2,2,2,2,2,2,2,2,2,2,2,2,2,2,2,2,2,2,2,2,2,2,2,2,2,2,2,2,2,2,2,2,
2,2,2,2,2,2,2,2,2,2,2,2,2,2,2,2,2,2,2,2,2,2,2,2,2,2,2,2,2,2,2,2,2,2,2,2,
2,2,2,2,2,2,2,2,2,2,2,2,2,2,2,2,2,2,2,2,2,2,4),(-2.59328853658183,-2.58600535494844,
-2.58266887539578,-2.58057642818646,-2.57864314721145,-2.57614740908341,
-2.57200747303872,-2.54425453014782,-2.50200628554234,-2.48610512911484,
-2.48058315091995,-2.47794773478339,-2.47583510493174,-2.47461246849111,
-2.47460891636769,-2.47460535047061,-2.47460177083311,-2.47459817731066,
-2.4745943200395,-2.47459039557256,-2.47458640246708,-2.47458233940881,
-2.47457820487136,-2.4745739972196,-2.47456971496081,-2.47456535648725,
-2.47456092015516,-2.47455640412381,-2.47455180666171,-2.47454712608477,
-2.47454236042841,-2.47453750779661,-2.47351268581807,-2.47213899916749,
-2.46930049460154,-2.43223374368189,-2.40047018286322,-2.37797733684563,
-2.37233324391901,-2.36976395145162,-2.36782603975058,-2.36599914366965,
-2.36345581671894,-2.35680429041609,-2.30111490358013,-2.27698401532335,
-2.26614276803842,-2.26389793128162,-2.262647608935,-2.26157582430046,-2.26022030442467,
-2.25807615650924,-2.24705912450343,-2.19580516494524,-2.16711833686923,
-2.16068765539593,-2.15797968196895,-2.15601831413085,-2.15422586190681,
-2.1513608837026,-2.14447482915395,-2.09143998963289,-2.0655120480464,-2.05420013507617,
-2.05192758608789,-2.05067125065163,-2.04960005262515,-2.04825259117729,
-2.04563178322568,-2.02959904215348,-2.02426125641956,-2.00971680617145,
-1.97682916778035,-1.9602647611674,-1.9499537921242,-1.94670523996688,-1.94463205138889,
-1.94269152097581,-1.94015057817655,-1.93585604478312,-1.90074428505616,
-1.85183366806679,-1.84207811610761,-1.83990309602701,-1.8386680283493,
-1.83759433212019,-1.83621684929797,-1.83335945110605,-1.81024465379414,
-1.76802196894324,-1.74940024809552,-1.7381835766657,-1.73483500762019,
-1.73273974756283,-1.73080710725478,-1.72831672515025,-1.72419547147613,
-1.69718015320056,-1.65528661855897,-1.63857253188948,-1.62997826973702,
-1.62788858529347,-1.62667237010685,-1.62559538417855,-1.62421082132829,
-1.62192110600651,-1.60822077698475,-1.6063709175413,-1.60500956888155,
-1.59754429260797,-1.5857463123036,-1.55288290217087,-1.53634916327188,
-1.52605188241343,-1.52280476620983,-1.52073180221146,-1.51879099585163,
-1.51624899004895,-1.51195108676669,-1.47659208805181,-1.42743052032568,
-1.41811510554275,-1.41597092291642,-1.41474259634102,-1.41366777160722,
-1.41227963173231,-1.40936793125375,-1.37753518125494,-1.33437642004195,
-1.3157387709112,-1.31200605408965,-1.30960614637965,-1.30768937871047,
-1.30552182759218,-1.30184723310008,-1.28708433244916,-1.2599708008188),
 .UNSPECIFIED.);
#946=B_SPLINE_CURVE_WITH_KNOTS('',3,(#95076,#95077,#95078,#95079,#95080),
 .UNSPECIFIED.,.F.,.F.,(4,1,4),(82.6397394568681,82.9034253468356,82.9907454093913),
 .UNSPECIFIED.);
#947=B_SPLINE_CURVE_WITH_KNOTS('',3,(#95081,#95082,#95083,#95084,#95085,
#95086,#95087,#95088,#95089,#95090,#95091,#95092,#95093,#95094,#95095,#95096,
#95097,#95098,#95099,#95100,#95101,#95102,#95103,#95104,#95105,#95106,#95107,
#95108,#95109,#95110,#95111,#95112,#95113,#95114,#95115,#95116,#95117,#95118,
#95119,#95120,#95121,#95122,#95123,#95124,#95125,#95126,#95127,#95128,#95129,
#95130,#95131,#95132,#95133,#95134,#95135,#95136,#95137,#95138,#95139,#95140,
#95141,#95142,#95143,#95144,#95145,#95146,#95147,#95148,#95149,#95150,#95151,
#95152,#95153,#95154,#95155,#95156,#95157,#95158,#95159,#95160,#95161,#95162,
#95163,#95164,#95165,#95166,#95167,#95168,#95169,#95170,#95171,#95172,#95173,
#95174,#95175,#95176,#95177,#95178,#95179,#95180,#95181,#95182,#95183,#95184,
#95185,#95186,#95187,#95188,#95189,#95190,#95191,#95192,#95193,#95194,#95195,
#95196,#95197,#95198,#95199,#95200,#95201,#95202,#95203,#95204,#95205,#95206,
#95207,#95208,#95209,#95210,#95211,#95212,#95213,#95214,#95215,#95216,#95217,
#95218,#95219,#95220,#95221,#95222,#95223,#95224,#95225,#95226,#95227,#95228,
#95229,#95230,#95231,#95232,#95233,#95234,#95235,#95236,#95237,#95238,#95239,
#95240,#95241,#95242,#95243,#95244,#95245,#95246,#95247,#95248,#95249,#95250,
#95251,#95252,#95253,#95254,#95255,#95256,#95257,#95258,#95259,#95260,#95261,
#95262,#95263,#95264,#95265,#95266,#95267,#95268,#95269,#95270,#95271,#95272,
#95273,#95274,#95275,#95276,#95277,#95278,#95279,#95280,#95281,#95282,#95283,
#95284,#95285,#95286,#95287,#95288,#95289,#95290,#95291,#95292,#95293,#95294,
#95295,#95296,#95297,#95298,#95299,#95300,#95301,#95302,#95303,#95304,#95305,
#95306,#95307,#95308,#95309,#95310,#95311,#95312,#95313,#95314,#95315,#95316,
#95317,#95318,#95319,#95320,#95321,#95322,#95323,#95324,#95325,#95326,#95327,
#95328,#95329,#95330,#95331,#95332,#95333,#95334,#95335,#95336),
 .UNSPECIFIED.,.F.,.F.,(4,2,2,2,2,2,2,2,2,2,2,2,2,2,2,2,2,2,2,2,2,2,2,2,
2,2,2,2,2,2,2,2,2,2,2,2,2,2,2,2,2,2,2,2,2,2,2,2,2,2,2,2,2,2,2,2,2,2,2,2,
2,2,2,2,2,2,2,2,2,2,2,2,2,2,2,2,2,2,2,2,2,2,2,2,2,2,2,2,2,2,2,2,2,2,2,2,
2,2,2,2,2,2,2,2,2,2,2,2,2,2,2,2,2,2,2,2,2,2,2,2,2,2,2,2,2,2,2,4),(-2.66780040318838,
-2.61551790977789,-2.59716970564285,-2.58607064758385,-2.58273462170918,
-2.58064213716017,-2.57870860232032,-2.57621222890874,-2.57207057156959,
-2.54426538375466,-2.50203381017613,-2.48615303607179,-2.48063557805295,
-2.4780016315159,-2.47588992400724,-2.47466741989728,-2.47466386489016,
-2.47466029622126,-2.47465671365226,-2.47465311723954,-2.47464924790979,
-2.4746453111953,-2.47464130566459,-2.47463722980043,-2.4746330821842,-2.47462886123928,
-2.47462456548351,-2.47462019315263,-2.4746157426227,-2.47461121211173,
-2.47460659981634,-2.47460190392262,-2.47459712275845,-2.47459225433639,
-2.47356702128603,-2.47219259175844,-2.46935060110709,-2.43244643100335,
-2.40084454662119,-2.38427063419762,-2.37395535867637,-2.37070630606194,
-2.36863300375729,-2.36669251132516,-2.36415182660582,-2.35985819626608,
-2.32481492744113,-2.27610713395617,-2.26610865268452,-2.26391722830508,
-2.26267855532423,-2.26160535599814,-2.2602332393536,-2.25740312238981,
-2.23560475967612,-2.19422095111495,-2.16695271661404,-2.16069314305251,
-2.15801416376571,-2.15605785333276,-2.15425893775005,-2.15135923276972,
-2.14426456299575,-2.0946777819443,-2.05630537544114,-2.05272022306183,
-2.05120950165274,-2.05011712916657,-2.04909182103223,-2.04735149707135,
-2.04263638471332,-2.00208399405331,-1.95512537277313,-1.94873124009659,
-1.9460293282421,-1.94406895064217,-1.94227505926827,-1.93940266956448,
-1.93247232764485,-1.88002504947992,-1.85368147982009,-1.84226394811427,
-1.83998524791738,-1.83872752180653,-1.83765635537541,-1.83631048147007,
-1.83369730300961,-1.81782808212738,-1.81196103643523,-1.76792203456759,
-1.74936661043314,-1.73817836764796,-1.73483281711261,-1.73273822411008,
-1.73080536922593,-1.72831355082763,-1.72418741219789,-1.69698007334459,
-1.65492989181173,-1.63847229080999,-1.62996575863749,-1.62788302762729,
-1.62666835416131,-1.6255910415935,-1.62420387356723,-1.62190531774929,
-1.608022288628,-1.60651774343736,-1.60499935810568,-1.59754569688297,-1.5857466200268,
-1.55288318433354,-1.53634942709176,-1.52605213609457,-1.52280501728472,
-1.52073205175766,-1.51879124405963,-1.51624923663557,-1.51195133089639,
-1.47659233779622,-1.42743072687935,-1.41811530320247,-1.41597111890691,
-1.41474279143201,-1.41366796594469,-1.41227982512901,-1.40936812278207,
-1.40856923606383),.UNSPECIFIED.);
#948=B_SPLINE_CURVE_WITH_KNOTS('',3,(#95338,#95339,#95340,#95341,#95342,
#95343,#95344,#95345,#95346,#95347,#95348,#95349,#95350,#95351,#95352,#95353,
#95354,#95355,#95356,#95357,#95358,#95359,#95360,#95361,#95362,#95363,#95364,
#95365,#95366,#95367,#95368,#95369,#95370,#95371,#95372,#95373,#95374,#95375,
#95376,#95377,#95378,#95379,#95380,#95381,#95382,#95383,#95384,#95385,#95386,
#95387,#95388,#95389,#95390,#95391,#95392,#95393,#95394,#95395,#95396,#95397,
#95398,#95399,#95400,#95401,#95402,#95403,#95404,#95405,#95406,#95407,#95408,
#95409,#95410,#95411,#95412,#95413,#95414,#95415,#95416,#95417,#95418,#95419,
#95420,#95421,#95422,#95423,#95424,#95425,#95426,#95427,#95428,#95429,#95430,
#95431,#95432,#95433,#95434,#95435,#95436,#95437,#95438,#95439,#95440,#95441,
#95442,#95443,#95444,#95445,#95446,#95447,#95448,#95449,#95450,#95451,#95452,
#95453,#95454,#95455,#95456,#95457,#95458,#95459,#95460,#95461,#95462,#95463,
#95464,#95465,#95466,#95467,#95468,#95469,#95470,#95471,#95472,#95473,#95474,
#95475,#95476,#95477,#95478,#95479,#95480,#95481,#95482,#95483,#95484,#95485,
#95486,#95487,#95488,#95489,#95490,#95491,#95492,#95493,#95494,#95495,#95496,
#95497,#95498,#95499,#95500,#95501,#95502,#95503,#95504,#95505,#95506,#95507,
#95508,#95509,#95510,#95511,#95512,#95513,#95514,#95515,#95516,#95517,#95518,
#95519,#95520,#95521,#95522,#95523,#95524,#95525,#95526,#95527,#95528,#95529,
#95530,#95531,#95532,#95533,#95534,#95535,#95536,#95537,#95538,#95539,#95540,
#95541,#95542,#95543,#95544,#95545,#95546,#95547,#95548,#95549,#95550,#95551,
#95552,#95553),.UNSPECIFIED.,.F.,.F.,(4,2,2,2,2,2,2,2,2,2,2,2,2,2,2,2,2,
2,2,2,2,2,2,2,2,2,2,2,2,2,2,2,2,2,2,2,2,2,2,2,2,2,2,2,2,2,2,2,2,2,2,2,2,
2,2,2,2,2,2,2,2,2,2,2,2,2,2,2,2,2,2,2,2,2,2,2,2,2,2,2,2,2,2,2,2,2,2,2,2,
2,2,2,2,2,2,2,2,2,2,2,2,2,2,2,2,2,2,4),(-1.2599708008188,-1.25915931404613,
-1.2093623898908,-1.20515944082174,-1.20349946744209,-1.2024896756088,-1.20138543389462,
-1.19981044851553,-1.1958345447609,-1.17602188346793,-1.14710909938688,
-1.10479018083132,-1.10049506909096,-1.09795383031137,-1.09601308953707,
-1.09393969051777,-1.09069083726277,-1.08037906948267,-1.06381583657343,
-1.03095507642963,-1.01703064325082,-1.01060069523947,-0.99501781415168,
-0.992416272899047,-0.991072887307461,-0.990001845800765,-0.988742114004146,
-0.986454262563982,-0.974875604050108,-0.947883813621921,-0.896303853404042,
-0.88931288873904,-0.886430438880445,-0.884634677984654,-0.882675788698833,
-0.879982356728087,-0.873638361634836,-0.845680254375092,-0.799190303148751,
-0.783069938021953,-0.780442462190926,-0.779093508375728,-0.778022138915881,
-0.776766783138712,-0.774498989100002,-0.763271961099305,-0.737674112670588,
-0.684113440102638,-0.677265491733396,-0.674406658048039,-0.672615230367634,
-0.67065271711738,-0.667938988470744,-0.661474766328608,-0.607387867162281,
-0.571356310839664,-0.56849630893015,-0.567118312414115,-0.566044560387861,
-0.564809825832879,-0.562636327992937,-0.552903371534513,-0.503947647622929,
-0.468806965956647,-0.464517412680411,-0.461977961282968,-0.460037720253713,
-0.457964015604134,-0.45471292912842,-0.444379256455963,-0.427766718973355,
-0.371066935348685,-0.35870882090716,-0.356487415483326,-0.355108425874969,
-0.354034588942138,-0.352800533488199,-0.350630083729614,-0.34094115553311,
-0.291948731762867,-0.256811880824043,-0.252513633573081,-0.249971677306362,
-0.248031043426507,-0.246240395005676,-0.243302955670095,-0.235328059303593,
-0.223523564485029,-0.190998708291966,-0.150078465375664,-0.145387649929409,
-0.143651118521622,-0.142626624597578,-0.141533913829228,-0.140020753964473,
-0.136420744214609,-0.0985305953414833,-0.0757357801255632,-0.0634020321071917,
-0.0604357409625306,-0.0436144588626216,-0.0399995457881178,-0.0376361113317291,
-0.0357225136846189,-0.0339209943472396,-0.0317709061040813,-0.0286342730469093,
-0.000628476936311304),.UNSPECIFIED.);
#949=B_SPLINE_CURVE_WITH_KNOTS('',3,(#95554,#95555,#95556,#95557,#95558,
#95559,#95560,#95561,#95562,#95563,#95564,#95565,#95566,#95567,#95568,#95569,
#95570,#95571),.UNSPECIFIED.,.F.,.F.,(4,2,2,2,2,2,2,2,4),(-2.66755959603529,
-2.62120144362155,-2.60363571981804,-2.59990254938237,-2.59836672373323,
-2.59726968673265,-2.59625060032127,-2.59454299008746,-2.59340588318677),
 .UNSPECIFIED.);
#950=B_SPLINE_CURVE_WITH_KNOTS('',3,(#95577,#95578,#95579,#95580,#95581,
#95582,#95583,#95584,#95585,#95586,#95587,#95588,#95589),.UNSPECIFIED.,
 .F.,.F.,(4,3,3,3,4),(76.3573194351122,76.4589087580869,76.5605127537386,
76.6622237693788,76.7075599105176),.UNSPECIFIED.);
#951=B_SPLINE_CURVE_WITH_KNOTS('',3,(#95590,#95591,#95592,#95593,#95594,
#95595,#95596,#95597,#95598,#95599),.UNSPECIFIED.,.F.,.F.,(4,1,1,1,1,1,
1,4),(76.7075601022117,76.9104066470643,77.9092430970262,78.9080795469881,
79.9069159969499,80.9057524469118,81.9045888968737,82.6397394568681),
 .UNSPECIFIED.);
#952=B_SPLINE_CURVE_WITH_KNOTS('',3,(#95600,#95601,#95602,#95603,#95604,
#95605,#95606,#95607,#95608,#95609,#95610,#95611,#95612,#95613,#95614,#95615,
#95616,#95617,#95618,#95619,#95620,#95621,#95622,#95623,#95624,#95625,#95626,
#95627,#95628,#95629,#95630,#95631,#95632,#95633,#95634,#95635,#95636,#95637,
#95638,#95639,#95640,#95641,#95642,#95643,#95644,#95645,#95646,#95647,#95648,
#95649,#95650,#95651,#95652,#95653,#95654,#95655,#95656,#95657,#95658,#95659,
#95660,#95661,#95662,#95663,#95664,#95665,#95666,#95667,#95668,#95669,#95670,
#95671,#95672,#95673,#95674,#95675,#95676,#95677,#95678,#95679,#95680,#95681,
#95682,#95683,#95684,#95685,#95686,#95687,#95688,#95689,#95690,#95691,#95692,
#95693,#95694,#95695,#95696,#95697,#95698,#95699,#95700,#95701,#95702,#95703,
#95704,#95705,#95706,#95707,#95708,#95709,#95710,#95711,#95712,#95713,#95714,
#95715,#95716,#95717,#95718,#95719,#95720,#95721,#95722,#95723,#95724,#95725,
#95726,#95727,#95728,#95729,#95730,#95731,#95732,#95733,#95734,#95735,#95736,
#95737,#95738,#95739,#95740,#95741,#95742,#95743,#95744,#95745,#95746,#95747,
#95748,#95749,#95750,#95751,#95752,#95753,#95754,#95755,#95756,#95757,#95758,
#95759,#95760,#95761,#95762,#95763,#95764,#95765,#95766,#95767,#95768,#95769,
#95770,#95771,#95772,#95773,#95774,#95775,#95776,#95777,#95778,#95779,#95780,
#95781,#95782,#95783,#95784,#95785,#95786,#95787,#95788,#95789,#95790,#95791,
#95792,#95793,#95794,#95795,#95796,#95797,#95798,#95799,#95800,#95801,#95802,
#95803,#95804,#95805,#95806,#95807,#95808,#95809,#95810,#95811,#95812,#95813,
#95814,#95815,#95816,#95817,#95818,#95819,#95820,#95821,#95822,#95823,#95824,
#95825,#95826,#95827,#95828,#95829,#95830,#95831,#95832,#95833,#95834,#95835),
 .UNSPECIFIED.,.F.,.F.,(4,2,2,2,2,2,2,2,2,2,2,2,2,2,2,2,2,2,2,2,2,2,2,2,
2,2,2,2,2,2,2,2,2,2,2,2,2,2,2,2,2,2,2,2,2,2,2,2,2,2,2,2,2,2,2,2,2,2,2,2,
2,2,2,2,2,2,2,2,2,2,2,2,2,2,2,2,2,2,2,2,2,2,2,2,2,2,2,2,2,2,2,2,2,2,2,2,
2,2,2,2,2,2,2,2,2,2,2,2,2,2,2,2,2,2,2,2,2,4),(-2.59340588318677,-2.59004423660487,
-2.54306658858682,-2.5229269865908,-2.50702016726606,-2.50036241947781,
-2.4952935381366,-2.49283512899737,-2.49090555118735,-2.48905817955765,
-2.48590554168906,-2.47720771247942,-2.47623867732846,-2.42660023042714,
-2.40067333012771,-2.3893602005497,-2.38708707027063,-2.38583036818752,
-2.38475883004618,-2.38341090575629,-2.38078909458786,-2.36474844614091,
-2.35942605859247,-2.31445345040613,-2.29625802577929,-2.28522426279168,
-2.28189473509369,-2.27980335788013,-2.27786881899704,-2.27536830200985,
-2.27121357898737,-2.24314199458864,-2.20093986094052,-2.18522736912133,
-2.17697939416692,-2.17491728352695,-2.17370700818838,-2.17262838938498,
-2.17123277416945,-2.16890605074208,-2.15452038519105,-2.15352883894173,
-2.10778334801586,-2.07838985863533,-2.07187460704002,-2.06915190389629,
-2.06718737487783,-2.06539717179839,-2.06254690361088,-2.05575334937012,
-2.00154684777688,-1.9764045095012,-1.96529377242664,-1.96303239086358,
-1.96177823745429,-1.9607064650167,-1.95935517262548,-1.95671772526564,
-1.9402748759459,-1.93129636558274,-1.89233352323295,-1.86585502833783,
-1.85969225800642,-1.85702959369709,-1.85507575252038,-1.85327248110821,
-1.85035098660948,-1.84312917975894,-1.79882622206036,-1.78472750953159,
-1.76327452968949,-1.75318355692263,-1.75098561428941,-1.74974531626441,
-1.74867201233729,-1.74730145574685,-1.7451085468767,-1.73333762184774,
-1.72962677687866,-1.72236564285951,-1.67901010698359,-1.66042270102561,
-1.64921989367379,-1.64587223199068,-1.64377681831943,-1.64184354647315,
-1.63935166617003,-1.63522645360109,-1.60809060278197,-1.56616641224731,
-1.54954739102426,-1.54098480469842,-1.53889725386835,-1.5376813150003,
-1.53660392301353,-1.53521799857436,-1.53292429328767,-1.51915036422728,
-1.50784474804067,-1.46844818562436,-1.44187539553467,-1.43570088525707,
-1.43303617757835,-1.43108197702624,-1.42927917441425,-1.4263602279219,
-1.41915356401649,-1.3730725829945,-1.33396209695869,-1.33297754939684,
-1.32826982446248,-1.32653034444181,-1.32550501734818,-1.32441218735223,
-1.32290011805811,-1.3193084909293,-1.28017013564396,-1.2596844006188),
 .UNSPECIFIED.);
#953=B_SPLINE_CURVE_WITH_KNOTS('',3,(#95841,#95842,#95843,#95844,#95845,
#95846,#95847,#95848,#95849,#95850,#95851,#95852,#95853,#95854,#95855,#95856,
#95857,#95858),.UNSPECIFIED.,.F.,.F.,(4,2,2,2,2,2,2,2,4),(-0.0749220714811919,
-0.0643002951613714,-0.0267279186973627,-0.018764011404856,-0.00802108956177915,
-0.0046663291600887,-0.00258130050280219,-0.00128118356189532,-0.000628940416801203),
 .UNSPECIFIED.);
#954=B_SPLINE_CURVE_WITH_KNOTS('',3,(#95859,#95860,#95861,#95862,#95863,
#95864,#95865,#95866,#95867,#95868,#95869,#95870,#95871,#95872,#95873,#95874,
#95875,#95876,#95877,#95878,#95879,#95880,#95881,#95882,#95883,#95884,#95885,
#95886,#95887,#95888,#95889,#95890,#95891,#95892,#95893,#95894,#95895,#95896,
#95897,#95898,#95899,#95900,#95901,#95902,#95903,#95904,#95905,#95906,#95907,
#95908,#95909,#95910,#95911,#95912,#95913,#95914,#95915,#95916,#95917,#95918,
#95919,#95920,#95921,#95922,#95923,#95924,#95925,#95926,#95927,#95928,#95929,
#95930,#95931,#95932,#95933,#95934,#95935,#95936,#95937,#95938,#95939,#95940,
#95941,#95942,#95943,#95944,#95945,#95946,#95947,#95948,#95949,#95950,#95951,
#95952,#95953,#95954,#95955,#95956,#95957,#95958,#95959,#95960,#95961,#95962,
#95963,#95964,#95965,#95966,#95967,#95968,#95969,#95970,#95971,#95972,#95973,
#95974,#95975,#95976,#95977,#95978,#95979,#95980,#95981,#95982,#95983,#95984,
#95985,#95986,#95987,#95988,#95989,#95990,#95991,#95992,#95993,#95994,#95995,
#95996,#95997,#95998,#95999,#96000,#96001,#96002,#96003,#96004,#96005,#96006,
#96007,#96008,#96009,#96010,#96011,#96012,#96013,#96014,#96015,#96016,#96017,
#96018,#96019,#96020,#96021,#96022,#96023,#96024,#96025,#96026,#96027,#96028,
#96029,#96030,#96031,#96032,#96033,#96034,#96035,#96036,#96037,#96038,#96039),
 .UNSPECIFIED.,.F.,.F.,(4,3,3,3,3,3,3,3,3,3,3,3,3,3,3,3,3,3,3,3,3,3,3,3,
3,3,3,3,3,3,3,3,3,3,3,3,3,3,3,3,3,3,3,3,3,3,3,3,3,3,3,3,3,3,3,3,3,3,3,3,
4),(70.4243747954073,70.5325790413758,70.6410991164241,70.7497863837822,
70.8587740112799,70.9173879472931,71.020782684341,71.124023966456,71.2271439318483,
71.3301985000572,71.4332217084149,71.5362475510874,71.6393803178655,71.7425694092753,
71.8459414026569,71.9162243972549,72.0196191343028,72.1228604164178,72.22598038181,
72.3290349500189,72.4320581583766,72.5350840010491,72.6382167678271,72.7414058592369,
72.8447778526185,72.9150608472168,73.0184555842648,73.1216968663798,73.2248168317721,
73.3278713999811,73.4308946083389,73.5339204510115,73.6370532177896,73.7402423091994,
73.8436143025811,73.9138972971787,74.0172920342266,74.1205333163416,74.2236532817339,
74.3267078499428,74.4297310583005,74.532756900973,74.6358896677511,74.7390787591609,
74.8424507525425,74.9127337471406,75.0161284841885,75.1193697663035,75.2224897316958,
75.3255442999047,75.4285675082624,75.5315933509349,75.6347261177129,75.7379152091227,
75.8412872025043,75.9115701971024,76.0134810050448,76.1152211478866,76.2168630906396,
76.3184433457412,76.3573194351122),.UNSPECIFIED.);
#955=B_SPLINE_CURVE_WITH_KNOTS('',3,(#96041,#96042,#96043,#96044,#96045,
#96046,#96047,#96048,#96049,#96050,#96051,#96052,#96053,#96054,#96055,#96056,
#96057,#96058,#96059,#96060,#96061,#96062,#96063,#96064,#96065,#96066,#96067,
#96068,#96069,#96070,#96071,#96072,#96073,#96074,#96075,#96076,#96077,#96078,
#96079,#96080,#96081,#96082,#96083,#96084,#96085,#96086,#96087,#96088,#96089,
#96090,#96091,#96092,#96093,#96094,#96095,#96096,#96097,#96098,#96099,#96100,
#96101,#96102,#96103,#96104,#96105,#96106,#96107,#96108,#96109,#96110,#96111,
#96112,#96113,#96114,#96115,#96116,#96117,#96118,#96119,#96120,#96121,#96122,
#96123,#96124,#96125,#96126,#96127,#96128,#96129,#96130,#96131,#96132,#96133,
#96134,#96135,#96136,#96137,#96138,#96139,#96140,#96141,#96142,#96143,#96144,
#96145,#96146,#96147,#96148,#96149,#96150,#96151,#96152,#96153,#96154,#96155,
#96156,#96157,#96158,#96159,#96160,#96161,#96162,#96163,#96164,#96165,#96166,
#96167,#96168,#96169,#96170,#96171,#96172,#96173,#96174,#96175,#96176,#96177,
#96178,#96179,#96180,#96181,#96182,#96183,#96184,#96185,#96186,#96187,#96188,
#96189,#96190,#96191,#96192,#96193,#96194,#96195,#96196,#96197,#96198,#96199,
#96200,#96201,#96202,#96203,#96204,#96205,#96206,#96207,#96208,#96209,#96210,
#96211,#96212,#96213,#96214,#96215,#96216,#96217,#96218,#96219,#96220,#96221,
#96222,#96223,#96224,#96225,#96226,#96227,#96228,#96229,#96230,#96231,#96232,
#96233,#96234,#96235,#96236,#96237,#96238,#96239,#96240,#96241,#96242,#96243,
#96244,#96245,#96246,#96247,#96248,#96249,#96250,#96251,#96252,#96253,#96254,
#96255,#96256),.UNSPECIFIED.,.F.,.F.,(4,2,2,2,2,2,2,2,2,2,2,2,2,2,2,2,2,
2,2,2,2,2,2,2,2,2,2,2,2,2,2,2,2,2,2,2,2,2,2,2,2,2,2,2,2,2,2,2,2,2,2,2,2,
2,2,2,2,2,2,2,2,2,2,2,2,2,2,2,2,2,2,2,2,2,2,2,2,2,2,2,2,2,2,2,2,2,2,2,2,
2,2,2,2,2,2,2,2,2,2,2,2,2,2,2,2,2,2,4),(-1.2596844006188,-1.23134348037588,
-1.22421236259465,-1.22130613130083,-1.21950569759933,-1.21754974270934,
-1.21487486052355,-1.20864136503829,-1.18159487613752,-1.1408667142172,
-1.11820860300803,-1.11535572922852,-1.113978945752,-1.11290509428865,-1.11166906535728,
-1.10949046530672,-1.09968793344074,-1.05077788864876,-1.01565733816867,
-1.01136168513588,-1.00882016943981,-1.0068792421472,-1.00480566806348,
-1.00155659103308,-0.991244539071412,-0.974681254939301,-0.941818681875961,
-0.928010773206015,-0.921314614232874,-0.9058651546604,-0.903497177917563,
-0.902089578195109,-0.901009419652921,-0.899805980301815,-0.897774221754095,
-0.889884499261976,-0.875168680537836,-0.846104322809252,-0.803698148398392,
-0.799404688837317,-0.796863865991712,-0.794923119346368,-0.792849400288268,
-0.789599390204754,-0.779278421619722,-0.762695147200479,-0.729816837435685,
-0.714514243732839,-0.709793809716609,-0.693941568323441,-0.691328755589958,
-0.689982898603794,-0.688911654783336,-0.687653737966812,-0.685374427280066,
-0.673948898758839,-0.647572543021168,-0.595122289837009,-0.58818879571284,
-0.585315752578351,-0.583521646009301,-0.581561193696602,-0.578859464446917,
-0.572467091901335,-0.526045725816737,-0.484947989958884,-0.480263111145685,
-0.478527326049579,-0.477502874716319,-0.476409871084484,-0.474895752896941,
-0.471290907393799,-0.432951749802275,-0.383317252134719,-0.376221628624632,
-0.373321716259422,-0.3715227255573,-0.36956638171457,-0.366887436208136,
-0.360806489500858,-0.352445554174214,-0.301550833652597,-0.270313243081288,
-0.267401275414166,-0.266013098530355,-0.264938282934619,-0.263710018326432,
-0.261566050213463,-0.25241497615479,-0.203666462142847,-0.167704290970596,
-0.162982357085103,-0.160559558854881,-0.158640677651432,-0.156487804187351,
-0.154258049263272,-0.146612099020315,-0.121083046625023,-0.100337619187811,
-0.0610229402291344,-0.0562870054891005,-0.0545435822959715,-0.0535177065254517,
-0.0524257939855512,-0.0509174411977632,-0.0492296227910852,-0.0462824128073364,
-0.000629120865108411),.UNSPECIFIED.);
#956=B_SPLINE_CURVE_WITH_KNOTS('',3,(#96257,#96258,#96259,#96260,#96261,
#96262,#96263,#96264,#96265,#96266,#96267,#96268,#96269),.UNSPECIFIED.,
 .F.,.F.,(4,3,3,3,4),(-66.6728921052185,-66.5709585796817,-66.4690950147616,
-66.3672509448711,-66.3228587574741),.UNSPECIFIED.);
#957=B_SPLINE_CURVE_WITH_KNOTS('',3,(#96274,#96275,#96276,#96277,#96278,
#96279,#96280,#96281,#96282,#96283,#96284,#96285,#96286,#96287,#96288,#96289,
#96290,#96291,#96292,#96293,#96294,#96295,#96296,#96297,#96298,#96299,#96300,
#96301,#96302,#96303,#96304,#96305,#96306,#96307,#96308,#96309,#96310,#96311,
#96312,#96313,#96314,#96315,#96316,#96317,#96318,#96319,#96320,#96321,#96322,
#96323,#96324,#96325,#96326,#96327,#96328,#96329,#96330,#96331,#96332,#96333,
#96334,#96335,#96336,#96337,#96338,#96339,#96340,#96341,#96342,#96343,#96344,
#96345,#96346,#96347,#96348,#96349,#96350,#96351,#96352,#96353,#96354,#96355,
#96356,#96357,#96358,#96359,#96360,#96361,#96362,#96363,#96364,#96365,#96366,
#96367,#96368,#96369,#96370,#96371,#96372,#96373,#96374,#96375,#96376,#96377,
#96378,#96379,#96380,#96381,#96382,#96383,#96384,#96385,#96386,#96387,#96388,
#96389,#96390,#96391,#96392,#96393,#96394,#96395,#96396,#96397,#96398,#96399,
#96400,#96401,#96402,#96403,#96404,#96405,#96406,#96407,#96408,#96409,#96410,
#96411,#96412,#96413,#96414,#96415,#96416,#96417,#96418,#96419,#96420,#96421,
#96422,#96423,#96424,#96425,#96426,#96427,#96428,#96429,#96430,#96431,#96432,
#96433,#96434,#96435,#96436,#96437,#96438,#96439,#96440,#96441,#96442,#96443,
#96444,#96445,#96446,#96447,#96448,#96449,#96450,#96451,#96452,#96453,#96454,
#96455,#96456,#96457,#96458,#96459,#96460,#96461,#96462,#96463,#96464,#96465,
#96466,#96467,#96468,#96469,#96470,#96471,#96472,#96473,#96474,#96475,#96476,
#96477,#96478,#96479,#96480,#96481,#96482,#96483,#96484,#96485,#96486,#96487,
#96488,#96489,#96490,#96491,#96492,#96493,#96494,#96495,#96496,#96497,#96498,
#96499,#96500,#96501,#96502,#96503,#96504,#96505,#96506,#96507),
 .UNSPECIFIED.,.F.,.F.,(4,2,2,2,2,2,2,2,2,2,2,2,2,2,2,2,2,2,2,2,2,2,2,2,
2,2,2,2,2,2,2,2,2,2,2,2,2,2,2,2,2,2,2,2,2,2,2,2,2,2,2,2,2,2,2,2,2,2,2,2,
2,2,2,2,2,2,2,2,2,2,2,2,2,2,2,2,2,2,2,2,2,2,2,2,2,2,2,2,2,2,2,2,2,2,2,2,
2,2,2,2,2,2,2,2,2,2,2,2,2,2,2,2,2,2,2,2,4),(-1.40849181731129,-1.39534413326025,
-1.3839435202864,-1.38166545110763,-1.38040770692253,-1.37933630327807,
-1.37798984927505,-1.37537471759749,-1.35945486214163,-1.3549530583211,
-1.33439091809116,-1.28603918699819,-1.27889054538664,-1.27598145261827,
-1.27418054699355,-1.27222510615025,-1.26955277515819,-1.26333365156747,
-1.2364027102941,-1.19587931431824,-1.17288882351002,-1.17003359567039,
-1.16865638586816,-1.16758253561546,-1.16634688497363,-1.16416985389905,
-1.15438934827788,-1.10546327810892,-1.07033832050305,-1.06604277856625,
-1.06350135239863,-1.0615605071805,-1.05948703406433,-1.05623814297163,
-1.04592691484572,-1.0293651759419,-0.996504733403481,-0.982762502489621,
-0.975913723538908,-0.975603980087717,-0.970099890012402,-0.960024116431277,
-0.957940683957954,-0.956603663469429,-0.955532937883248,-0.954268012591245,
-0.951956331220263,-0.939942367959669,-0.888190497283394,-0.858195618158027,
-0.853997984617839,-0.851485201816563,-0.849549119583362,-0.847463926274746,
-0.844161049461407,-0.833367529931291,-0.815723542794052,-0.765299615137646,
-0.764148951014091,-0.74855873040497,-0.745956883128004,-0.744613434252925,
-0.743542392477956,-0.742282718735769,-0.739995122329155,-0.728420923557461,
-0.701447117636352,-0.649842413473516,-0.642853031033282,-0.639970849521632,
-0.638175142299623,-0.636216220969492,-0.633522580024731,-0.627177323458069,
-0.599208688097817,-0.552613532096975,-0.536598391082022,-0.53397849141888,
-0.532631170900919,-0.531559912942187,-0.530303313659875,-0.52802978493932,
-0.516703247675675,-0.490716619276593,-0.437717077773332,-0.430825134330234,
-0.427959068462517,-0.426166334194717,-0.424204983883288,-0.421497624982962,
-0.415071182868322,-0.38642543851006,-0.335154364051163,-0.324142926650919,
-0.321999109401333,-0.320643665246783,-0.31957185619643,-0.318321414941718,
-0.316076127258167,-0.305228616952376,-0.281072259060738,-0.225373554692153,
-0.218721542979501,-0.215951841005866,-0.21400628797182,-0.212061424853581,
-0.210091687480759,-0.204924731766838,-0.160520234482066,-0.115647463093391,
-0.110925811268191,-0.109184560990818,-0.108159115366993,-0.1070669426203,
-0.105557060148865,-0.101976495484075,-0.0749220714811919),
 .UNSPECIFIED.);
#958=B_SPLINE_CURVE_WITH_KNOTS('',3,(#96509,#96510,#96511,#96512,#96513,
#96514,#96515,#96516,#96517,#96518,#96519,#96520,#96521,#96522,#96523,#96524,
#96525,#96526,#96527,#96528,#96529,#96530,#96531,#96532,#96533,#96534,#96535,
#96536,#96537,#96538,#96539,#96540,#96541,#96542,#96543,#96544,#96545,#96546,
#96547,#96548,#96549,#96550,#96551,#96552,#96553,#96554,#96555,#96556,#96557,
#96558,#96559,#96560,#96561,#96562,#96563,#96564,#96565,#96566,#96567,#96568,
#96569,#96570,#96571,#96572,#96573,#96574,#96575,#96576,#96577,#96578,#96579,
#96580,#96581,#96582,#96583,#96584,#96585,#96586,#96587,#96588,#96589,#96590,
#96591,#96592,#96593,#96594,#96595,#96596,#96597,#96598,#96599,#96600,#96601,
#96602,#96603,#96604,#96605,#96606,#96607,#96608,#96609,#96610,#96611,#96612,
#96613,#96614,#96615,#96616,#96617,#96618,#96619,#96620,#96621,#96622,#96623,
#96624,#96625,#96626,#96627,#96628,#96629,#96630,#96631,#96632,#96633,#96634,
#96635,#96636,#96637,#96638,#96639,#96640,#96641,#96642,#96643,#96644,#96645,
#96646,#96647,#96648,#96649,#96650,#96651,#96652,#96653,#96654,#96655,#96656,
#96657,#96658,#96659,#96660,#96661,#96662,#96663,#96664,#96665,#96666,#96667,
#96668,#96669,#96670,#96671,#96672,#96673,#96674,#96675,#96676,#96677,#96678,
#96679,#96680,#96681,#96682,#96683,#96684,#96685,#96686),.UNSPECIFIED.,
 .F.,.F.,(4,3,3,3,3,3,3,3,3,3,3,3,3,3,3,3,3,3,3,3,3,3,3,3,3,3,3,3,3,3,3,
3,3,3,3,3,3,3,3,3,3,3,3,3,3,3,3,3,3,3,3,3,3,3,3,3,3,3,3,4),(-66.3228587574741,
-66.2209269063509,-66.1189508258224,-66.0167874103627,-65.9232056974837,
-65.8198109604357,-65.7165696783208,-65.6134497129284,-65.5103951447194,
-65.4073719363617,-65.304346093689,-65.201213326911,-65.0980242355011,-64.9946522421195,
-64.9243692475218,-64.8209745104739,-64.7177332283588,-64.6146132629666,
-64.5115586947576,-64.4085354863999,-64.3055096437275,-64.2023768769495,
-64.0991877855397,-63.9958157921581,-63.9255327975599,-63.822138060512,
-63.718896778397,-63.6157768130047,-63.5127222447958,-63.4096990364379,
-63.3066731937653,-63.2035404269872,-63.1003513355775,-62.9969793421958,
-62.9266963475981,-62.8233016105502,-62.7200603284354,-62.6169403630432,
-62.5138857948343,-62.4108625864766,-62.3078367438041,-62.2047039770261,
-62.1015148856163,-61.9981428922347,-61.9278598976362,-61.8244651605881,
-61.7212238784729,-61.6181039130806,-61.5150493448717,-61.412026136514,
-61.3090002938412,-61.2058675270631,-61.1026784356533,-60.9993064422715,
-60.9290234476743,-60.8220651862385,-60.7139755891886,-60.6074364851719,
-60.4985716416054,-60.3897067980389),.UNSPECIFIED.);
#959=B_SPLINE_CURVE_WITH_KNOTS('',3,(#96687,#96688,#96689,#96690),
 .UNSPECIFIED.,.F.,.F.,(4,4),(-60.3897037700523,-60.0402339956293),
 .UNSPECIFIED.);
#960=B_SPLINE_CURVE_WITH_KNOTS('',3,(#96696,#96697,#96698,#96699,#96700,
#96701),.UNSPECIFIED.,.F.,.F.,(4,2,4),(-0.075038806717288,-0.0529910440511674,
-0.000629600917318996),.UNSPECIFIED.);
#961=B_SPLINE_CURVE_WITH_KNOTS('',3,(#96702,#96703,#96704,#96705,#96706,
#96707,#96708,#96709,#96710,#96711,#96712,#96713,#96714,#96715,#96716,#96717,
#96718,#96719,#96720,#96721,#96722,#96723,#96724,#96725,#96726,#96727,#96728,
#96729,#96730,#96731,#96732,#96733,#96734,#96735,#96736,#96737,#96738,#96739,
#96740,#96741,#96742,#96743,#96744,#96745,#96746,#96747,#96748,#96749,#96750,
#96751,#96752,#96753,#96754,#96755,#96756,#96757,#96758,#96759,#96760,#96761,
#96762,#96763,#96764,#96765,#96766,#96767,#96768,#96769,#96770,#96771,#96772,
#96773,#96774,#96775,#96776,#96777,#96778,#96779,#96780,#96781,#96782,#96783,
#96784,#96785,#96786,#96787,#96788,#96789,#96790,#96791,#96792,#96793,#96794,
#96795,#96796,#96797,#96798,#96799,#96800,#96801,#96802,#96803,#96804,#96805,
#96806,#96807,#96808,#96809,#96810,#96811,#96812,#96813,#96814,#96815,#96816,
#96817,#96818,#96819,#96820,#96821,#96822,#96823,#96824,#96825,#96826,#96827,
#96828,#96829,#96830,#96831,#96832,#96833,#96834,#96835,#96836,#96837,#96838,
#96839,#96840,#96841,#96842,#96843,#96844,#96845,#96846,#96847,#96848,#96849,
#96850,#96851,#96852,#96853,#96854,#96855,#96856,#96857,#96858,#96859,#96860,
#96861,#96862,#96863,#96864,#96865,#96866,#96867,#96868,#96869,#96870,#96871,
#96872,#96873,#96874,#96875,#96876,#96877,#96878,#96879,#96880,#96881,#96882,
#96883,#96884,#96885,#96886,#96887,#96888,#96889,#96890,#96891,#96892,#96893,
#96894,#96895,#96896,#96897,#96898,#96899,#96900,#96901,#96902,#96903,#96904,
#96905,#96906,#96907,#96908,#96909,#96910,#96911,#96912,#96913,#96914,#96915,
#96916,#96917,#96918,#96919,#96920,#96921,#96922,#96923,#96924,#96925,#96926,
#96927,#96928,#96929,#96930,#96931,#96932,#96933,#96934,#96935,#96936,#96937,
#96938,#96939,#96940,#96941,#96942,#96943,#96944,#96945,#96946,#96947,#96948,
#96949,#96950,#96951),.UNSPECIFIED.,.F.,.F.,(4,2,2,2,2,2,2,2,2,2,2,2,2,
2,2,2,2,2,2,2,2,2,2,2,2,2,2,2,2,2,2,2,2,2,2,2,2,2,2,2,2,2,2,2,2,2,2,2,2,
2,2,2,2,2,2,2,2,2,2,2,2,2,2,2,2,2,2,2,2,2,2,2,2,2,2,2,2,2,2,2,2,2,2,2,2,
2,2,2,2,2,2,2,2,2,2,2,2,2,2,2,2,2,2,2,2,2,2,2,2,2,2,2,2,2,2,2,2,2,2,2,2,
2,2,2,4),(-2.66785867798683,-2.65980139307743,-2.65544393569796,-2.65403085994829,
-2.65296354475938,-2.65193327423883,-2.65075329188821,-2.64882796290568,
-2.64276206648497,-2.64147998045497,-2.63367912055449,-2.58042654028585,
-2.56271330019522,-2.55188924146064,-2.54858214767669,-2.54649548013368,
-2.54455884793956,-2.54204651216505,-2.53785220327919,-2.50806282802426,
-2.46716795538772,-2.45178619053623,-2.44638418086373,-2.44378952291186,
-2.44168554628189,-2.44047341238879,-2.44047028729506,-2.44046714336841,
-2.44046398041027,-2.4404607982075,-2.4404575964406,-2.44045437500728,-2.44045113396158,
-2.44044787324233,-2.44044459246466,-2.44044129128748,-2.44043796991524,
-2.44043464134687,-2.4404312983739,-2.44042793429552,-2.44042454900457,
-2.44042113116944,-2.43939351501871,-2.43801460546967,-2.43515022177071,
-2.39947437974768,-2.36660902743931,-2.34389542618647,-2.33822104087803,
-2.33564591823926,-2.3337068396424,-2.33188121406708,-2.32934345565815,
-2.3227290257416,-2.26665380577393,-2.24276557413512,-2.23198914584977,
-2.22974796872575,-2.22849831188082,-2.22742625047205,-2.22606929292911,
-2.22392083108199,-2.21283818601615,-2.16155989913174,-2.13294209920106,
-2.126519122556,-2.12381216793253,-2.12185072945635,-2.12005765621856,-2.11719047436762,
-2.11029284835065,-2.05738495188888,-2.0313576970674,-2.02001968913433,
-2.01774536097607,-2.01648850666873,-2.01541714820455,-2.01406984381859,
-2.01145039637796,-1.99544564797781,-1.98996784299213,-1.97552292411418,
-1.94263073634456,-1.92606484837104,-1.91575271974157,-1.91250367583362,
-1.91043014304709,-1.90848926910961,-1.90594784570508,-1.90165243100518,
-1.86652427307357,-1.81757324781445,-1.80785368827791,-1.80568087658229,
-1.80444616302768,-1.80337219775383,-1.8019936149713,-1.79913133340986,
-1.76311285885758,-1.7303606436664,-1.70782644079248,-1.70217602943133,
-1.69960515224254,-1.69766657115448,-1.69583943065096,-1.69329638422362,
-1.68664930700714,-1.63088184758667,-1.59797879193682,-1.59443218587794,
-1.59292787761089,-1.59183643955113,-1.59080905051046,-1.58905884570364,
-1.58428012273461,-1.5471131285102,-1.49683942494867,-1.49043745040415,
-1.48773388174164,-1.48577290593268,-1.48397888354758,-1.48110719266454,
-1.47418323057818,-1.4216167136691,-1.40849181731129),.UNSPECIFIED.);
#962=B_SPLINE_CURVE_WITH_KNOTS('',3,(#96953,#96954,#96955,#96956,#96957,
#96958,#96959,#96960,#96961,#96962),.UNSPECIFIED.,.F.,.F.,(4,1,1,1,1,1,
1,4),(-60.0402339956293,-59.9301869977125,-58.9313505477506,-57.9325140977887,
-56.9336776478268,-55.934841197865,-54.9360047479031,-54.1065275196936),
 .UNSPECIFIED.);
#963=B_SPLINE_CURVE_WITH_KNOTS('',3,(#96963,#96964,#96965,#96966,#96967,
#96968,#96969,#96970,#96971,#96972,#96973,#96974,#96975,#96976,#96977,#96978,
#96979,#96980,#96981,#96982,#96983,#96984),.UNSPECIFIED.,.F.,.F.,(4,2,2,
2,2,2,2,2,2,2,4),(-2.66748285763103,-2.64324926503545,-2.63611726584707,
-2.63432648362479,-2.63311152542526,-2.63210237517397,-2.63102767404166,
-2.62964130759543,-2.62673900317765,-2.59968632690069,-2.59337489789675),
 .UNSPECIFIED.);
#964=B_SPLINE_CURVE_WITH_KNOTS('',3,(#96989,#96990,#96991,#96992,#96993,
#96994,#96995,#96996,#96997,#96998,#96999,#97000,#97001,#97002,#97003,#97004,
#97005,#97006,#97007,#97008,#97009,#97010,#97011,#97012,#97013,#97014,#97015,
#97016,#97017,#97018,#97019,#97020,#97021,#97022,#97023,#97024,#97025,#97026,
#97027,#97028,#97029,#97030,#97031,#97032,#97033,#97034,#97035,#97036,#97037,
#97038,#97039,#97040,#97041,#97042,#97043,#97044,#97045,#97046,#97047,#97048,
#97049,#97050,#97051,#97052,#97053,#97054,#97055,#97056,#97057,#97058,#97059,
#97060,#97061,#97062,#97063,#97064,#97065,#97066,#97067,#97068,#97069,#97070,
#97071,#97072,#97073,#97074,#97075,#97076,#97077,#97078,#97079,#97080,#97081,
#97082,#97083,#97084,#97085,#97086,#97087,#97088,#97089,#97090,#97091,#97092,
#97093,#97094,#97095,#97096,#97097,#97098,#97099,#97100,#97101,#97102,#97103,
#97104,#97105,#97106,#97107,#97108,#97109,#97110,#97111,#97112,#97113,#97114,
#97115,#97116,#97117,#97118,#97119,#97120,#97121,#97122,#97123,#97124,#97125,
#97126,#97127,#97128,#97129,#97130,#97131,#97132,#97133,#97134,#97135,#97136,
#97137,#97138,#97139,#97140,#97141,#97142,#97143,#97144,#97145,#97146,#97147,
#97148,#97149,#97150,#97151,#97152,#97153,#97154,#97155,#97156,#97157,#97158,
#97159,#97160,#97161,#97162,#97163,#97164,#97165,#97166,#97167,#97168,#97169,
#97170,#97171,#97172,#97173,#97174,#97175,#97176,#97177,#97178,#97179,#97180,
#97181,#97182,#97183,#97184,#97185,#97186,#97187,#97188,#97189,#97190,#97191,
#97192,#97193,#97194,#97195,#97196,#97197,#97198,#97199,#97200,#97201,#97202,
#97203,#97204,#97205,#97206,#97207,#97208,#97209,#97210,#97211,#97212,#97213,
#97214,#97215,#97216,#97217,#97218,#97219,#97220,#97221,#97222,#97223,#97224,
#97225,#97226,#97227,#97228,#97229,#97230),.UNSPECIFIED.,.F.,.F.,(4,2,2,
2,2,2,2,2,2,2,2,2,2,2,2,2,2,2,2,2,2,2,2,2,2,2,2,2,2,2,2,2,2,2,2,2,2,2,2,
2,2,2,2,2,2,2,2,2,2,2,2,2,2,2,2,2,2,2,2,2,2,2,2,2,2,2,2,2,2,2,2,2,2,2,2,
2,2,2,2,2,2,2,2,2,2,2,2,2,2,2,2,2,2,2,2,2,2,2,2,2,2,2,2,2,2,2,2,2,2,2,2,
2,2,2,2,2,2,2,2,2,4),(-1.40848019473541,-1.38239422892346,-1.36905396071534,
-1.36549889522737,-1.36335772755904,-1.36143643340249,-1.35899308762589,
-1.35511850832949,-1.33404421585164,-1.27622795910977,-1.26126705211177,
-1.25891899021377,-1.25751716473004,-1.25643775943186,-1.25523107519433,
-1.25318491262186,-1.24512732575371,-1.22994776179928,-1.19005056034978,
-1.15900595251883,-1.15478430885474,-1.15226431199618,-1.15032685172039,
-1.14824428466472,-1.14495430607332,-1.13428040366213,-1.11690862295099,
-1.06820376947828,-1.0616881803853,-1.04906566855534,-1.04682990993342,
-1.0454464620129,-1.04437201164759,-1.04314046352743,-1.04098203999855,
-1.03146950600333,-0.982315198169504,-0.947118886371042,-0.942822455217987,
-0.940280786188271,-0.938339918592029,-0.936266579679289,-0.933018228955314,
-0.922711497671774,-0.906159626264462,-0.873307589385927,-0.86038887438955,
-0.837685948899323,-0.834832345499673,-0.833455550912708,-0.832381851188896,
-0.831146178093623,-0.828968639073795,-0.819178084796704,-0.770267216652909,
-0.735149493413028,-0.730854498440486,-0.728313383490019,-0.726372768806855,
-0.724299535060604,-0.721051004586173,-0.710740799187361,-0.694180587140001,
-0.661323663265587,-0.647548901024741,-0.640781714200325,-0.639209642602496,
-0.625256611023007,-0.622954753772721,-0.621566632822581,-0.620489225944818,
-0.619275182724371,-0.61719517154778,-0.608722294385308,-0.59235999035848,
-0.550186061678572,-0.522931311232696,-0.51880379994111,-0.516311646422943,
-0.514378814354156,-0.512284527687986,-0.508940075826187,-0.497761100931318,
-0.479229583265353,-0.434842373529562,-0.413730454697519,-0.410917775636129,
-0.409549153375782,-0.408476318783945,-0.407235382109819,-0.405033425329507,
-0.394874207177727,-0.373180133958159,-0.372020402648616,-0.313853998860858,
-0.307478907457946,-0.304980419143423,-0.303165297711273,-0.301220790141232,
-0.298609755306034,-0.292735714533123,-0.268516125991691,-0.227082755051121,
-0.201866987532232,-0.198983098684127,-0.197600547825018,-0.19657105381372,
-0.19538021786063,-0.193408432882404,-0.190985475666953,-0.18607475251318,
-0.172714987700871,-0.15252651232384,-0.102928705546204,-0.0958339839794316,
-0.0929345388287951,-0.0911358677574391,-0.0891798950949667,-0.0865015004779375,
-0.0802438387687248,-0.075038806717288),.UNSPECIFIED.);
#965=B_SPLINE_CURVE_WITH_KNOTS('',3,(#97231,#97232,#97233,#97234,#97235,
#97236,#97237,#97238,#97239,#97240,#97241,#97242,#97243,#97244,#97245,#97246,
#97247,#97248,#97249,#97250,#97251,#97252,#97253,#97254,#97255,#97256,#97257,
#97258,#97259,#97260,#97261,#97262,#97263,#97264,#97265,#97266,#97267,#97268,
#97269,#97270,#97271,#97272,#97273,#97274,#97275,#97276,#97277,#97278,#97279,
#97280,#97281,#97282,#97283,#97284,#97285,#97286,#97287,#97288,#97289,#97290,
#97291,#97292,#97293,#97294,#97295,#97296,#97297,#97298,#97299,#97300,#97301,
#97302,#97303,#97304,#97305,#97306,#97307,#97308,#97309,#97310,#97311,#97312,
#97313,#97314,#97315,#97316,#97317,#97318,#97319,#97320,#97321,#97322,#97323,
#97324,#97325,#97326,#97327,#97328,#97329,#97330,#97331,#97332,#97333,#97334,
#97335,#97336,#97337,#97338,#97339,#97340,#97341,#97342,#97343,#97344,#97345,
#97346,#97347,#97348,#97349,#97350,#97351,#97352,#97353,#97354,#97355,#97356,
#97357,#97358,#97359,#97360,#97361,#97362,#97363,#97364,#97365,#97366,#97367,
#97368,#97369,#97370,#97371,#97372,#97373,#97374,#97375,#97376,#97377,#97378,
#97379,#97380,#97381,#97382,#97383,#97384,#97385,#97386,#97387,#97388,#97389,
#97390,#97391,#97392,#97393,#97394,#97395,#97396,#97397,#97398,#97399,#97400,
#97401,#97402,#97403,#97404,#97405,#97406,#97407,#97408,#97409,#97410,#97411,
#97412,#97413,#97414,#97415,#97416,#97417,#97418,#97419,#97420,#97421,#97422,
#97423,#97424,#97425,#97426,#97427,#97428,#97429,#97430,#97431,#97432,#97433,
#97434,#97435,#97436,#97437,#97438,#97439,#97440,#97441,#97442,#97443,#97444,
#97445,#97446,#97447,#97448,#97449,#97450,#97451,#97452,#97453,#97454,#97455,
#97456,#97457,#97458,#97459,#97460,#97461,#97462),.UNSPECIFIED.,.F.,.F.,
(4,2,2,2,2,2,2,2,2,2,2,2,2,2,2,2,2,2,2,2,2,2,2,2,2,2,2,2,2,2,2,2,2,2,2,
2,2,2,2,2,2,2,2,2,2,2,2,2,2,2,2,2,2,2,2,2,2,2,2,2,2,2,2,2,2,2,2,2,2,2,2,
2,2,2,2,2,2,2,2,2,2,2,2,2,2,2,2,2,2,2,2,2,2,2,2,2,2,2,2,2,2,2,2,2,2,2,2,
2,2,2,2,2,2,2,2,4),(-2.59337489789675,-2.58561238519003,-2.5736012351672,
-2.54190221097263,-2.53146041821309,-2.52819650651114,-2.5261196695812,
-2.52418002920341,-2.52164644052308,-2.51737815087784,-2.47198908962061,
-2.43802611821553,-2.42427914629956,-2.42171890202092,-2.42039483697899,
-2.41932314271042,-2.41806909731193,-2.41586843293411,-2.40685723000472,
-2.3539464386988,-2.32470989911176,-2.3182134621207,-2.31549409417234,-2.31353034358247,
-2.31173973576514,-2.30888641642316,-2.30207328760224,-2.24810944652342,
-2.2228088075181,-2.21165735957861,-2.20939377507873,-2.20813922927116,
-2.20706762767805,-2.20571719678519,-2.20308334374152,-2.18672590873896,
-2.1365525419151,-2.11849488894645,-2.10752136554714,-2.10419864685843,
-2.10210896322935,-2.10017422282583,-2.0976709568711,-2.09350624250701,
-2.06484193251605,-2.02312196497596,-2.0075113351921,-1.99929969366833,
-1.99724077921504,-1.9960313206454,-1.99495270339727,-1.99355614494871,
-1.99122585914714,-1.97668180279041,-1.97434015171541,-1.92392035721741,
-1.90628580118414,-1.89549740629227,-1.89219500059953,-1.89010985851512,
-1.88817365467598,-1.885660475484,-1.88146168600695,-1.85141120350088,-1.79974569391282,
-1.78774105761309,-1.78542990109675,-1.78416508566437,-1.78309435054852,
-1.78175718392715,-1.77967326754144,-1.76959081022052,-1.76408866920562,
-1.75666075903552,-1.74315374735036,-1.7102720985274,-1.69371845410015,
-1.68341191728806,-1.68016355512271,-1.6780901978289,-1.67614930578707,
-1.67360759552205,-1.66931110610758,-1.63409411711189,-1.58484929870086,
-1.57547164839891,-1.57332286152462,-1.57209345272159,-1.57101869294232,
-1.56963197057584,-1.56738526024835,-1.55455239771529,-1.55238635613203,
-1.50510602602108,-1.47658192153856,-1.47016996644554,-1.46746478530359,
-1.46550358715487,-1.46371001402097,-1.4608404651189,-1.45392902539541,
-1.40119799850049,-1.37504370370648,-1.36367320927299,-1.3613969336009,
-1.36013961456057,-1.35906823067263,-1.35772136595842,-1.35510415844712,
-1.33914219057051,-1.33419819696957,-1.32855219827746,-1.2815931219422,
-1.28014709804074,-1.26110786927851,-1.25973005914825),.UNSPECIFIED.);
#966=B_SPLINE_CURVE_WITH_KNOTS('',3,(#97468,#97469,#97470,#97471,#97472,
#97473,#97474,#97475,#97476,#97477,#97478,#97479,#97480,#97481,#97482,#97483),
 .UNSPECIFIED.,.F.,.F.,(4,2,2,2,2,2,2,4),(-0.0747630397369221,-0.074125929836722,
-0.0730538955052031,-0.0718062276008534,-0.0695734668952728,-0.0589294385692646,
-0.0355200016789157,-0.000629543070150967),.UNSPECIFIED.);
#967=B_SPLINE_CURVE_WITH_KNOTS('',3,(#97484,#97485,#97486,#97487,#97488,
#97489,#97490,#97491,#97492,#97493,#97494,#97495,#97496,#97497,#97498,#97499,
#97500,#97501,#97502,#97503,#97504,#97505,#97506,#97507,#97508,#97509,#97510,
#97511,#97512,#97513,#97514,#97515,#97516,#97517,#97518,#97519,#97520,#97521,
#97522,#97523,#97524,#97525,#97526,#97527,#97528,#97529,#97530,#97531,#97532,
#97533,#97534,#97535,#97536,#97537,#97538,#97539,#97540,#97541,#97542,#97543,
#97544,#97545,#97546,#97547,#97548,#97549,#97550,#97551,#97552,#97553,#97554,
#97555,#97556,#97557,#97558,#97559,#97560,#97561,#97562,#97563,#97564,#97565,
#97566,#97567,#97568,#97569,#97570,#97571,#97572,#97573,#97574,#97575,#97576,
#97577,#97578,#97579,#97580,#97581,#97582,#97583,#97584,#97585,#97586,#97587,
#97588,#97589,#97590,#97591,#97592,#97593,#97594,#97595,#97596,#97597,#97598,
#97599,#97600,#97601,#97602,#97603,#97604,#97605,#97606,#97607,#97608,#97609,
#97610,#97611,#97612,#97613,#97614,#97615,#97616,#97617,#97618,#97619,#97620,
#97621,#97622,#97623,#97624,#97625,#97626,#97627,#97628,#97629,#97630,#97631,
#97632,#97633,#97634,#97635,#97636,#97637,#97638,#97639,#97640,#97641,#97642,
#97643,#97644,#97645,#97646,#97647,#97648,#97649,#97650,#97651,#97652,#97653,
#97654,#97655,#97656,#97657,#97658,#97659,#97660,#97661,#97662,#97663,#97664,
#97665,#97666,#97667,#97668,#97669,#97670,#97671,#97672,#97673,#97674,#97675,
#97676,#97677,#97678,#97679,#97680,#97681,#97682,#97683,#97684,#97685,#97686,
#97687,#97688,#97689,#97690,#97691,#97692,#97693,#97694,#97695,#97696,#97697,
#97698,#97699,#97700,#97701,#97702,#97703,#97704,#97705,#97706,#97707),
 .UNSPECIFIED.,.F.,.F.,(4,2,2,2,2,2,2,2,2,2,2,2,2,2,2,2,2,2,2,2,2,2,2,2,
2,2,2,2,2,2,2,2,2,2,2,2,2,2,2,2,2,2,2,2,2,2,2,2,2,2,2,2,2,2,2,2,2,2,2,2,
2,2,2,2,2,2,2,2,2,2,2,2,2,2,2,2,2,2,2,2,2,2,2,2,2,2,2,2,2,2,2,2,2,2,2,2,
2,2,2,2,2,2,2,2,2,2,2,2,2,2,2,4),(-2.66783535108714,-2.64250906893,-2.63938208222713,
-2.63723600115051,-2.63543519243453,-2.63352124181565,-2.6311520769427,
-2.62751851804251,-2.61041314579988,-2.59822256861164,-2.5565501005403,
-2.54066441939936,-2.53235654636494,-2.53028999587732,-2.52907899257403,
-2.52800100808561,-2.52660787969764,-2.52428879783054,-2.51000006914887,
-2.50120107583317,-2.47962900749421,-2.44818170163269,-2.43607186156944,
-2.43058444851967,-2.42623476187509,-2.42393221098337,-2.4220195563318,
-2.41981678698706,-2.4160800392244,-2.40203629057023,-2.34395278460679,
-2.32851772707835,-2.32036856462133,-2.31831495680088,-2.3171067402988,
-2.31602794103389,-2.3146294660068,-2.31229243423733,-2.2975890856737,-2.25146107462409,
-2.22185180691862,-2.21531195362349,-2.21258551123426,-2.21062062485524,
-2.20883169361043,-2.20598689151067,-2.19922377643746,-2.14470006903296,
-2.11978692981944,-2.10873726059878,-2.10647984098072,-2.10522672175815,
-2.10415512154941,-2.10280313681509,-2.10016163887205,-2.08360356604286,
-2.03306548313488,-2.00887727263476,-2.0030074260505,-2.00039697573588,
-1.99845240207015,-1.99663686178176,-1.99413723572669,-1.98775622038017,
-1.92965504297113,-1.90706106013365,-1.89664309510086,-1.89442434029175,
-1.8931796447804,-1.89210714062645,-1.89074355824237,-1.88857313871593,
-1.87712455004244,-1.87307012438648,-1.8728248183821,-1.86595929124893,
-1.852225984038,-1.81934327750738,-1.80278750071601,-1.79248010429687,-1.78923172022595,
-1.78715840879499,-1.78521760172687,-1.78267606340333,-1.77838000061332,
-1.74318521068846,-1.69401409937404,-1.68455450257467,-1.68239993056173,
-1.68116927475662,-1.68009476271526,-1.67871012021756,-1.67581660956862,
-1.6497822965264,-1.61161487953928,-1.58258677680828,-1.5781911436166,-1.57586756012254,
-1.57395594501301,-1.57173181097133,-1.5679035370945,-1.55284212658676,
-1.50067345456839,-1.4818277802287,-1.47253189567416,-1.47038898712396,
-1.46916087139268,-1.4680858926064,-1.4666971069231,-1.46378247467635,-1.43373616217968,
-1.40848019473541),.UNSPECIFIED.);
#968=B_SPLINE_CURVE_WITH_KNOTS('',3,(#97709,#97710,#97711,#97712,#97713,
#97714,#97715,#97716,#97717,#97718,#97719,#97720,#97721,#97722,#97723,#97724,
#97725,#97726,#97727,#97728,#97729,#97730,#97731,#97732,#97733,#97734,#97735,
#97736,#97737,#97738,#97739,#97740,#97741,#97742,#97743,#97744,#97745,#97746,
#97747,#97748,#97749,#97750,#97751,#97752,#97753,#97754,#97755,#97756,#97757,
#97758,#97759,#97760,#97761,#97762,#97763,#97764,#97765,#97766,#97767,#97768,
#97769,#97770,#97771,#97772,#97773,#97774,#97775,#97776,#97777,#97778,#97779,
#97780,#97781,#97782,#97783,#97784,#97785,#97786,#97787,#97788,#97789,#97790,
#97791,#97792,#97793,#97794,#97795,#97796,#97797,#97798,#97799,#97800,#97801,
#97802,#97803,#97804,#97805,#97806,#97807,#97808,#97809,#97810,#97811,#97812,
#97813,#97814,#97815,#97816,#97817,#97818,#97819,#97820,#97821,#97822,#97823,
#97824,#97825,#97826,#97827,#97828,#97829,#97830,#97831,#97832,#97833,#97834,
#97835,#97836,#97837,#97838,#97839,#97840,#97841,#97842,#97843,#97844,#97845,
#97846,#97847,#97848,#97849,#97850,#97851,#97852,#97853,#97854,#97855,#97856,
#97857,#97858,#97859,#97860,#97861,#97862,#97863,#97864,#97865,#97866,#97867,
#97868,#97869,#97870,#97871,#97872,#97873,#97874,#97875,#97876,#97877,#97878,
#97879,#97880,#97881,#97882,#97883,#97884,#97885,#97886,#97887,#97888,#97889,
#97890,#97891,#97892,#97893,#97894,#97895,#97896,#97897,#97898,#97899,#97900,
#97901,#97902,#97903,#97904,#97905,#97906,#97907,#97908,#97909,#97910,#97911,
#97912,#97913,#97914,#97915,#97916,#97917,#97918,#97919,#97920,#97921,#97922,
#97923,#97924,#97925,#97926),.UNSPECIFIED.,.F.,.F.,(4,2,2,2,2,2,2,2,2,2,
2,2,2,2,2,2,2,2,2,2,2,2,2,2,2,2,2,2,2,2,2,2,2,2,2,2,2,2,2,2,2,2,2,2,2,2,
2,2,2,2,2,2,2,2,2,2,2,2,2,2,2,2,2,2,2,2,2,2,2,2,2,2,2,2,2,2,2,2,2,2,2,2,
2,2,2,2,2,2,2,2,2,2,2,2,2,2,2,2,2,2,2,2,2,2,2,2,2,2,4),(-1.25973005914825,
-1.25734673576451,-1.25493799364887,-1.25302024499271,-1.25085804788037,
-1.24720822119141,-1.23275560773671,-1.18236883734888,-1.15270137220804,
-1.14978688828851,-1.1483981269892,-1.1473231419446,-1.14609500024645,-1.14395198793024,
-1.13465505386342,-1.11580362506527,-1.07535049127943,-1.06307183334997,
-1.04849206650873,-1.04470610185088,-1.04249165398581,-1.04057937096035,
-1.03824369402508,-1.03379063115923,-1.0027547532014,-0.954777987487901,
-0.940188301453422,-0.937855920131238,-0.936458678044927,-0.935379884791108,
-0.934170633265356,-0.932112949431952,-0.923917837684583,-0.908352484961321,
-0.866771608499126,-0.854699776541554,-0.836944049735642,-0.833267517262526,
-0.830884743673292,-0.828969247295901,-0.82678973231593,-0.823061740997188,
-0.807614707829557,-0.756014456353178,-0.728679189755335,-0.725774778178223,
-0.724387941036871,-0.723313118750484,-0.722083677207734,-0.719934909918138,
-0.710558854482192,-0.661284061362405,-0.626051867018526,-0.621754867939458,
-0.619212998049116,-0.617272054867228,-0.615198710624219,-0.611950508975189,
-0.601645577007871,-0.58509785607852,-0.552248725360138,-0.539753922742267,
-0.516621401094841,-0.513763498712775,-0.512385837313556,-0.511312028791543,
-0.51007687077048,-0.507901770803435,-0.49814751764719,-0.449204429645168,
-0.414076923548904,-0.409780950983742,-0.407239516710465,-0.405298807344663,
-0.403225617073029,-0.399977456669936,-0.389670970747025,-0.373119152827878,
-0.340268659111501,-0.327240365109306,-0.318507978720654,-0.304211753872246,
-0.301892029381645,-0.300498637562593,-0.299420526714317,-0.298209479819172,
-0.296143057872224,-0.287838601264404,-0.271961271137324,-0.225895406465433,
-0.201639020674606,-0.1976237345401,-0.195164705357662,-0.193294628387892,
-0.19126654636763,-0.188075316889398,-0.184320141673537,-0.177183987718724,
-0.15961252712563,-0.109463964776951,-0.0924352898109446,-0.089776066101595,
-0.088420321839725,-0.087348495859116,-0.0860982883850014,-0.083854053618281,
-0.0730237950007372,-0.0489314110027095,-0.000629479462340787),
 .UNSPECIFIED.);
#969=B_SPLINE_CURVE_WITH_KNOTS('',3,(#97927,#97928,#97929,#97930,#97931,
#97932,#97933,#97934,#97935,#97936,#97937,#97938,#97939,#97940,#97941,#97942,
#97943,#97944,#97945,#97946,#97947,#97948),.UNSPECIFIED.,.F.,.F.,(4,2,2,
2,2,2,2,2,2,2,4),(-2.6678214478774,-2.66002753739846,-2.6547310404401,-2.65228763735666,
-2.65040576350708,-2.64856503657601,-2.64673861360468,-2.64419819355603,
-2.63900696606325,-2.62649661765704,-2.59340742691029),.UNSPECIFIED.);
#970=B_SPLINE_CURVE_WITH_KNOTS('',3,(#97953,#97954,#97955,#97956,#97957,
#97958,#97959,#97960,#97961,#97962,#97963,#97964,#97965,#97966,#97967,#97968,
#97969,#97970,#97971,#97972,#97973,#97974,#97975,#97976,#97977,#97978,#97979,
#97980,#97981,#97982,#97983,#97984,#97985,#97986,#97987,#97988,#97989,#97990,
#97991,#97992,#97993,#97994,#97995,#97996,#97997,#97998,#97999,#98000,#98001,
#98002,#98003,#98004,#98005,#98006,#98007,#98008,#98009,#98010,#98011,#98012,
#98013,#98014,#98015,#98016,#98017,#98018,#98019,#98020,#98021,#98022,#98023,
#98024,#98025,#98026,#98027,#98028,#98029,#98030,#98031,#98032,#98033,#98034,
#98035,#98036,#98037,#98038,#98039,#98040,#98041,#98042,#98043,#98044,#98045,
#98046,#98047,#98048,#98049,#98050,#98051,#98052,#98053,#98054,#98055,#98056,
#98057,#98058,#98059,#98060,#98061,#98062,#98063,#98064,#98065,#98066,#98067,
#98068,#98069,#98070,#98071,#98072,#98073,#98074,#98075,#98076,#98077,#98078,
#98079,#98080,#98081,#98082,#98083,#98084,#98085,#98086,#98087,#98088,#98089,
#98090,#98091,#98092,#98093,#98094,#98095,#98096,#98097,#98098,#98099,#98100,
#98101,#98102,#98103,#98104,#98105,#98106,#98107,#98108,#98109,#98110,#98111,
#98112,#98113,#98114,#98115,#98116,#98117,#98118,#98119,#98120,#98121,#98122,
#98123,#98124,#98125,#98126,#98127,#98128,#98129,#98130,#98131,#98132,#98133,
#98134,#98135,#98136,#98137,#98138,#98139,#98140,#98141,#98142,#98143,#98144,
#98145,#98146,#98147,#98148,#98149,#98150,#98151,#98152,#98153,#98154,#98155,
#98156,#98157,#98158,#98159,#98160,#98161,#98162,#98163,#98164,#98165,#98166,
#98167,#98168,#98169,#98170,#98171,#98172,#98173,#98174),.UNSPECIFIED.,
 .F.,.F.,(4,2,2,2,2,2,2,2,2,2,2,2,2,2,2,2,2,2,2,2,2,2,2,2,2,2,2,2,2,2,2,
2,2,2,2,2,2,2,2,2,2,2,2,2,2,2,2,2,2,2,2,2,2,2,2,2,2,2,2,2,2,2,2,2,2,2,2,
2,2,2,2,2,2,2,2,2,2,2,2,2,2,2,2,2,2,2,2,2,2,2,2,2,2,2,2,2,2,2,2,2,2,2,2,
2,2,2,2,2,2,2,4),(-1.40845787076926,-1.36760548623614,-1.35571294198462,
-1.35117785792175,-1.34786945228156,-1.3464069708187,-1.34532226889899,
-1.34413338184527,-1.34216743748543,-1.3357623369736,-1.33420643238553,
-1.31961991307284,-1.26057847745824,-1.24626880242789,-1.2425071213422,
-1.24029829200361,-1.23838564018709,-1.23604291757183,-1.23155599889841,
-1.19919435451072,-1.15901049115682,-1.15407864423868,-1.13812964660466,
-1.13551314136766,-1.13416643685508,-1.13309507396208,-1.13183766177518,
-1.12956090710595,-1.11818217252907,-1.09199256927698,-1.03927060553121,
-1.03235603928805,-1.02948599783301,-1.02769235386209,-1.02573127434595,
-1.02302660807084,-1.01661751513893,-0.988120778224044,-0.937199691808353,
-0.92570593998298,-0.923532784663462,-0.922168306560197,-0.921095644958398,
-0.919851398673143,-0.917634983655801,-0.907256255625866,-0.88479949620845,
-0.826425683167227,-0.820074640884895,-0.817579909948831,-0.815765546174149,
-0.813819997106104,-0.811204332633417,-0.805306067097214,-0.780904425918359,
-0.730243664865649,-0.714073288020118,-0.711447082232428,-0.710098342018559,
-0.70902691223935,-0.707771219535754,-0.705502142204713,-0.69425508762572,
-0.668580750836144,-0.615124095566524,-0.60826688100222,-0.605406389703567,
-0.603614565077583,-0.601652134216144,-0.598939470614618,-0.592482316776173,
-0.538648842451557,-0.502333043684892,-0.499481707201636,-0.498105350023912,
-0.497031682506023,-0.495795697428157,-0.493616772444554,-0.483806088750772,
-0.434911600178473,-0.39978588705918,-0.395498300221219,-0.392959320398786,
-0.391019040319279,-0.388944906261988,-0.38569233592946,-0.375347086631822,
-0.358709391730538,-0.325788065870077,-0.307647528961386,-0.2901527056505,
-0.287476521900033,-0.286117157539036,-0.285045058424708,-0.283797502071491,
-0.281565404343079,-0.270933199713164,-0.247567356259084,-0.191910477658296,
-0.184487386175552,-0.181531997981181,-0.179722854124052,-0.177893796424317,
-0.175383406597913,-0.170030959687916,-0.162914048401213,-0.145410500276712,
-0.0956238241308649,-0.0781599967756867,-0.0754850053838553,-0.0747630397369221),
 .UNSPECIFIED.);
#971=B_SPLINE_CURVE_WITH_KNOTS('',3,(#98175,#98176,#98177,#98178,#98179,
#98180,#98181,#98182,#98183,#98184,#98185,#98186,#98187,#98188,#98189,#98190,
#98191,#98192,#98193,#98194,#98195,#98196,#98197,#98198,#98199,#98200,#98201,
#98202,#98203,#98204,#98205,#98206,#98207,#98208,#98209,#98210,#98211,#98212,
#98213,#98214,#98215,#98216,#98217,#98218,#98219,#98220,#98221,#98222,#98223,
#98224,#98225,#98226,#98227,#98228,#98229,#98230,#98231,#98232,#98233,#98234,
#98235,#98236,#98237,#98238,#98239,#98240,#98241,#98242,#98243,#98244,#98245,
#98246,#98247,#98248,#98249,#98250,#98251,#98252,#98253,#98254,#98255,#98256,
#98257,#98258,#98259,#98260,#98261,#98262,#98263,#98264,#98265,#98266,#98267,
#98268,#98269,#98270,#98271,#98272,#98273,#98274,#98275,#98276,#98277,#98278,
#98279,#98280,#98281,#98282,#98283,#98284,#98285,#98286,#98287,#98288,#98289,
#98290,#98291,#98292,#98293,#98294,#98295,#98296,#98297,#98298,#98299,#98300,
#98301,#98302,#98303,#98304,#98305,#98306,#98307,#98308,#98309,#98310,#98311,
#98312,#98313,#98314,#98315,#98316,#98317,#98318,#98319,#98320,#98321,#98322,
#98323,#98324,#98325,#98326,#98327,#98328,#98329,#98330,#98331,#98332,#98333,
#98334,#98335,#98336,#98337,#98338,#98339,#98340,#98341,#98342,#98343,#98344,
#98345,#98346,#98347,#98348,#98349,#98350,#98351,#98352,#98353,#98354,#98355,
#98356,#98357,#98358,#98359,#98360,#98361,#98362,#98363,#98364,#98365,#98366,
#98367,#98368,#98369,#98370,#98371,#98372,#98373,#98374,#98375,#98376,#98377,
#98378,#98379,#98380,#98381,#98382,#98383,#98384,#98385,#98386,#98387,#98388,
#98389,#98390,#98391,#98392,#98393,#98394,#98395,#98396,#98397,#98398,#98399,
#98400,#98401,#98402,#98403,#98404,#98405,#98406,#98407,#98408,#98409,#98410,
#98411,#98412,#98413,#98414,#98415,#98416,#98417,#98418,#98419,#98420,#98421,
#98422,#98423,#98424,#98425,#98426,#98427,#98428,#98429,#98430,#98431,#98432,
#98433,#98434,#98435,#98436,#98437,#98438,#98439,#98440,#98441,#98442,#98443,
#98444),.UNSPECIFIED.,.F.,.F.,(4,2,2,2,2,2,2,2,2,2,2,2,2,2,2,2,2,2,2,2,
2,2,2,2,2,2,2,2,2,2,2,2,2,2,2,2,2,2,2,2,2,2,2,2,2,2,2,2,2,2,2,2,2,2,2,2,
2,2,2,2,2,2,2,2,2,2,2,2,2,2,2,2,2,2,2,2,2,2,2,2,2,2,2,2,2,2,2,2,2,2,2,2,
2,2,2,2,2,2,2,2,2,2,2,2,2,2,2,2,2,2,2,2,2,2,2,2,2,2,2,2,2,2,2,2,2,2,2,2,
2,2,2,2,2,2,4),(-2.59340742691029,-2.57482683816369,-2.55598428705709,-2.54668929628617,
-2.54454640880166,-2.54331827533432,-2.5422432615787,-2.54085440506306,
-2.53793953358015,-2.50824286242268,-2.45779351324169,-2.4483044705862,
-2.44369718445865,-2.43991807765489,-2.43774736955123,-2.43773167510825,
-2.43771542809484,-2.4376986083976,-2.43768119517003,-2.43766316681614,
-2.43764450094062,-2.43762517432277,-2.43760516292549,-2.43758444181548,
-2.43756298519575,-2.43754076634933,-2.43751775690632,-2.43749772062185,
-2.43747437033533,-2.43744716395983,-2.43741547348671,-2.43737857258338,
-2.43733562298907,-2.4372814105044,-2.43534068744899,-2.43279867369071,
-2.42850049441156,-2.39337894217525,-2.3444197610308,-2.33472076041937,
-2.33254960873209,-2.33131538333458,-2.33024155061225,-2.32886275572408,
-2.32599871442945,-2.29004668201088,-2.2572799032197,-2.23471839779757,
-2.22906471274651,-2.22649348217233,-2.22455509691613,-2.22272848071384,
-2.22018670929407,-2.21354621783687,-2.15773754627064,-2.13367776544556,
-2.12285518790877,-2.12061130091228,-2.11936109893463,-2.11828916558737,
-2.11693313448587,-2.11478757245249,-2.10375041867314,-2.05253448171894,
-2.02382498692971,-2.01739126118217,-2.01468258840941,-2.01272092541467,
-2.01092834882572,-2.00806348798411,-2.00117935327486,-1.94810328336587,
-1.9221968195101,-1.91088984480889,-1.9086173939238,-1.90736099249572,-1.90628966520143,
-1.90494194819707,-1.90232036973582,-1.8862782735189,-1.88098880635368,
-1.86640333575631,-1.83351148308965,-1.81694463870141,-1.80663224448225,
-1.80338329239783,-1.80130986038324,-1.79936911039311,-1.79682789202798,
-1.79253291967179,-1.75742112231489,-1.70851711837857,-1.69874599446692,
-1.69656973652486,-1.69533431009532,-1.69426052228391,-1.69288320993399,
-1.69002715620144,-1.66722999397125,-1.6116189146061,-1.59560714931515,
-1.59183766553623,-1.58964919152793,-1.58773499075694,-1.58536571962127,
-1.58173237867305,-1.56463564194741,-1.55656635629851,-1.52175568049127,
-1.49770632715769,-1.48688681590627,-1.48464320740332,-1.48339311050977,
-1.48232123638361,-1.4809652405832,-1.47830495576461,-1.46125129225894,
-1.44263945105813,-1.40968326605101,-1.39303804334902,-1.38269035032521,
-1.37943743122769,-1.37736318170756,-1.37542286917012,-1.37288395695056,
-1.36859676254284,-1.33401557331994,-1.27804985039277,-1.2737760250553,
-1.27210444939211,-1.27109242088845,-1.26999008544948,-1.26842516708966,
-1.2645126452046,-1.25985927748007),.UNSPECIFIED.);
#972=B_SPLINE_CURVE_WITH_KNOTS('',3,(#98450,#98451,#98452,#98453,#98454,
#98455,#98456,#98457,#98458,#98459,#98460,#98461,#98462,#98463,#98464,#98465,
#98466,#98467),.UNSPECIFIED.,.F.,.F.,(4,2,2,2,2,2,2,2,4),(-0.0751187452951849,
-0.0651105015072089,-0.0603738607788016,-0.0579480733093331,-0.056029062931303,
-0.0538783931757228,-0.0516516905968622,-0.0483298714381254,-0.000628983405359937),
 .UNSPECIFIED.);
#973=B_SPLINE_CURVE_WITH_KNOTS('',3,(#98468,#98469,#98470,#98471,#98472,
#98473,#98474,#98475,#98476,#98477,#98478,#98479,#98480,#98481,#98482,#98483,
#98484,#98485,#98486,#98487,#98488,#98489,#98490,#98491,#98492,#98493,#98494,
#98495,#98496,#98497,#98498,#98499,#98500,#98501,#98502,#98503,#98504,#98505,
#98506,#98507,#98508,#98509,#98510,#98511,#98512,#98513,#98514,#98515,#98516,
#98517,#98518,#98519,#98520,#98521,#98522,#98523,#98524,#98525,#98526,#98527,
#98528,#98529,#98530,#98531,#98532,#98533,#98534,#98535,#98536,#98537,#98538,
#98539,#98540,#98541,#98542,#98543,#98544,#98545,#98546,#98547,#98548,#98549,
#98550,#98551,#98552,#98553,#98554,#98555,#98556,#98557,#98558,#98559,#98560,
#98561,#98562,#98563,#98564,#98565,#98566,#98567,#98568,#98569,#98570,#98571,
#98572,#98573,#98574,#98575,#98576,#98577,#98578,#98579,#98580,#98581,#98582,
#98583,#98584,#98585,#98586,#98587,#98588,#98589,#98590,#98591,#98592,#98593,
#98594,#98595,#98596,#98597,#98598,#98599,#98600,#98601,#98602,#98603,#98604,
#98605,#98606,#98607,#98608,#98609,#98610,#98611,#98612,#98613,#98614,#98615,
#98616,#98617,#98618,#98619,#98620,#98621,#98622,#98623,#98624,#98625,#98626,
#98627,#98628,#98629,#98630,#98631,#98632,#98633,#98634,#98635,#98636,#98637,
#98638,#98639,#98640,#98641,#98642,#98643,#98644,#98645,#98646,#98647,#98648,
#98649,#98650,#98651,#98652,#98653,#98654,#98655,#98656,#98657,#98658,#98659,
#98660,#98661,#98662,#98663,#98664,#98665,#98666,#98667,#98668,#98669,#98670,
#98671,#98672,#98673,#98674,#98675,#98676,#98677,#98678,#98679,#98680,#98681,
#98682,#98683,#98684,#98685,#98686,#98687,#98688,#98689,#98690,#98691),
 .UNSPECIFIED.,.F.,.F.,(4,2,2,2,2,2,2,2,2,2,2,2,2,2,2,2,2,2,2,2,2,2,2,2,
2,2,2,2,2,2,2,2,2,2,2,2,2,2,2,2,2,2,2,2,2,2,2,2,2,2,2,2,2,2,2,2,2,2,2,2,
2,2,2,2,2,2,2,2,2,2,2,2,2,2,2,2,2,2,2,2,2,2,2,2,2,2,2,2,2,2,2,2,2,2,2,2,
2,2,2,2,2,2,2,2,2,2,2,2,2,2,2,4),(-2.66767968022051,-2.62472410100834,-2.62179024369457,
-2.62010753067188,-2.61860262187355,-2.61751100562116,-2.61648365454228,
-2.61473395702785,-2.60995915844497,-2.57250918240443,-2.55112176284539,
-2.52297042937878,-2.51633518659523,-2.51419561335918,-2.51210518020193,
-2.51017009822064,-2.50766688638814,-2.50350334361195,-2.47491290010697,
-2.44422701153071,-2.42038341354095,-2.40963328825848,-2.40740385203333,
-2.40614667163674,-2.4050751247499,-2.40372769735748,-2.40110834559491,
-2.38511092113857,-2.34084084869684,-2.3185744941839,-2.31018753941203,
-2.30409399604709,-2.30141111926008,-2.29945370777524,-2.29765499483361,
-2.29475830215823,-2.28768450447225,-2.23758434766355,-2.19964488815378,
-2.19607528994373,-2.19456697515733,-2.19347478825612,-2.19244841498421,
-2.19070363208749,-2.18596101022418,-2.146805627867,-2.09846332216771,-2.09206436586189,
-2.08936118732208,-2.08740017201908,-2.08560589113307,-2.08273330123238,
-2.07580466365126,-2.02329274066577,-1.99697702324215,-1.98556517737468,
-1.9832863475584,-1.98202838131569,-1.98095690832146,-1.97961051949116,
-1.97699596098488,-1.96109665887807,-1.96029238517123,-1.95152276698426,
-1.94394862944422,-1.91164747970902,-1.89280694214238,-1.88149571974595,
-1.87813645891381,-1.87603839440241,-1.87410579794032,-1.87161913833119,
-1.86751194760779,-1.84109148772073,-1.79881875014397,-1.78190721562362,
-1.77324496704892,-1.77114948301669,-1.76993173638218,-1.7688546328313,
-1.76747151336861,-1.76518747620935,-1.75161477006505,-1.7497906086826,
-1.70241721420444,-1.67144194092423,-1.66698993464138,-1.66465431397224,
-1.66274182562227,-1.66052685731025,-1.65673931567436,-1.64214487790029,
-1.62987934262549,-1.58946826330187,-1.57061452885678,-1.56131572211745,
-1.55917244129718,-1.55794416077477,-1.55686906942419,-1.55548018012948,
-1.55256547806248,-1.52372835638706,-1.48561706845735,-1.46809153475096,
-1.457350451559,-1.4540527827418,-1.45196837394869,-1.45003129225038,-1.44751476137409,
-1.44330550528578,-1.41283079708318,-1.40845787076926),.UNSPECIFIED.);
#974=B_SPLINE_CURVE_WITH_KNOTS('',3,(#98693,#98694,#98695,#98696,#98697,
#98698,#98699,#98700,#98701,#98702,#98703,#98704,#98705,#98706,#98707,#98708,
#98709,#98710,#98711,#98712,#98713,#98714,#98715,#98716,#98717,#98718,#98719,
#98720,#98721,#98722,#98723,#98724,#98725,#98726,#98727,#98728,#98729,#98730,
#98731,#98732,#98733,#98734,#98735,#98736,#98737,#98738,#98739,#98740,#98741,
#98742,#98743,#98744,#98745,#98746,#98747,#98748,#98749,#98750,#98751,#98752,
#98753,#98754,#98755,#98756,#98757,#98758,#98759,#98760,#98761,#98762,#98763,
#98764,#98765,#98766,#98767,#98768,#98769,#98770,#98771,#98772,#98773,#98774,
#98775,#98776,#98777,#98778,#98779,#98780,#98781,#98782,#98783,#98784,#98785,
#98786,#98787,#98788,#98789,#98790,#98791,#98792,#98793,#98794,#98795,#98796,
#98797,#98798,#98799,#98800,#98801,#98802,#98803,#98804,#98805,#98806,#98807,
#98808,#98809,#98810,#98811,#98812,#98813,#98814,#98815,#98816,#98817,#98818,
#98819,#98820,#98821,#98822,#98823,#98824,#98825,#98826,#98827,#98828,#98829,
#98830,#98831,#98832,#98833,#98834,#98835,#98836,#98837,#98838,#98839,#98840,
#98841,#98842,#98843,#98844,#98845,#98846,#98847,#98848,#98849,#98850,#98851,
#98852,#98853,#98854,#98855,#98856,#98857,#98858,#98859,#98860,#98861,#98862,
#98863,#98864,#98865,#98866,#98867,#98868,#98869,#98870,#98871,#98872,#98873,
#98874,#98875,#98876,#98877,#98878,#98879,#98880,#98881,#98882,#98883,#98884,
#98885,#98886,#98887,#98888,#98889,#98890,#98891,#98892,#98893,#98894,#98895,
#98896,#98897,#98898,#98899,#98900,#98901,#98902,#98903,#98904,#98905,#98906,
#98907,#98908,#98909,#98910,#98911,#98912,#98913,#98914,#98915,#98916,#98917,
#98918,#98919,#98920,#98921,#98922,#98923,#98924,#98925,#98926,#98927,#98928,
#98929,#98930,#98931,#98932,#98933,#98934,#98935,#98936,#98937,#98938,#98939,
#98940,#98941,#98942),.UNSPECIFIED.,.F.,.F.,(4,2,2,2,2,2,2,2,2,2,2,2,2,
2,2,2,2,2,2,2,2,2,2,2,2,2,2,2,2,2,2,2,2,2,2,2,2,2,2,2,2,2,2,2,2,2,2,2,2,
2,2,2,2,2,2,2,2,2,2,2,2,2,2,2,2,2,2,2,2,2,2,2,2,2,2,2,2,2,2,2,2,2,2,2,2,
2,2,2,2,2,2,2,2,2,2,2,2,2,2,2,2,2,2,2,2,2,2,2,2,2,2,2,2,2,2,2,2,2,2,2,2,
2,2,2,4),(-1.25985927748007,-1.2453003608062,-1.18892655397525,-1.17208144320606,
-1.16846473424463,-1.16610063855232,-1.16418684615964,-1.16199469799336,
-1.15820841068723,-1.14196185488026,-1.08448807431236,-1.07951541021613,
-1.06352987734088,-1.060911520986,-1.05956446632786,-1.05849314205298,-1.05723614299795,
-1.05496107222932,-1.04361003416923,-1.01752857920213,-0.964657620824425,
-0.957754797560903,-0.954886795420749,-0.953093601313664,-0.95113235145535,
-0.948426237280657,-0.942007982302704,-0.913433004698384,-0.862236989550861,
-0.851077062547889,-0.848923967992624,-0.847565636064483,-0.84649352601687,
-0.845245009891988,-0.843008844389658,-0.832313136909083,-0.808717538316708,
-0.752155396513283,-0.745589991140517,-0.743060124960592,-0.741236653797819,
-0.739296606699633,-0.736714622157358,-0.731002178634805,-0.708006887754293,
-0.67499115512056,-0.653966523574106,-0.639427645202852,-0.63709784681296,
-0.635701516337916,-0.63462303800303,-0.633413705604618,-0.6313549244533,
-0.623142962897156,-0.60752833142615,-0.565798520565196,-0.53711876354255,
-0.532953909722397,-0.530450790170106,-0.52851628812586,-0.526426985273519,
-0.523105135828782,-0.512136787100746,-0.494092608375872,-0.44394973431467,
-0.427599056526347,-0.424965865279674,-0.423615707203438,-0.422544286663548,
-0.421289917907758,-0.41902655374547,-0.407874729225503,-0.382567093742985,
-0.328586314515925,-0.321773694005278,-0.318920747300034,-0.317130423203263,
-0.31516702993929,-0.312448234169004,-0.305953518114173,-0.27673112699336,
-0.230070278103009,-0.215487915813216,-0.21295319667546,-0.211639178896181,
-0.210624518118271,-0.210616805287299,-0.210609243251825,-0.210601822977389,
-0.210594536107828,-0.210587374869379,-0.210580332097621,-0.210573401037422,
-0.210566575349115,-0.210559849132122,-0.210553216948067,-0.210546673528998,
-0.21054021396125,-0.210533833739875,-0.210527528431888,-0.210521294041483,
-0.210515126684568,-0.210509022608291,-0.210502978392329,-0.210496990703806,
-0.210491056335889,-0.210485172242678,-0.210479335624958,-0.2092168030889,
-0.206832087639687,-0.193334800688978,-0.157490929439518,-0.113371995598794,
-0.109091768114718,-0.106555067457512,-0.104615329130127,-0.10254060815884,
-0.0992846763182317,-0.0889080167813931,-0.0721999787376405,-0.0417595395179099,
-0.00539337765390236,-0.0019346342927621,-0.000864008595668716,-0.000629065984911949),
 .UNSPECIFIED.);
#975=B_SPLINE_CURVE_WITH_KNOTS('',3,(#98943,#98944,#98945,#98946,#98947,
#98948,#98949,#98950,#98951,#98952,#98953,#98954,#98955,#98956,#98957,#98958),
 .UNSPECIFIED.,.F.,.F.,(4,3,3,3,3,4),(-28.973780262141,-28.9662570488944,
-28.8628842312553,-28.7596459044043,-28.6565264336763,-28.6232427996483),
 .UNSPECIFIED.);
#976=B_SPLINE_CURVE_WITH_KNOTS('',3,(#98963,#98964,#98965,#98966,#98967,
#98968,#98969,#98970,#98971,#98972,#98973,#98974,#98975,#98976,#98977,#98978,
#98979,#98980,#98981,#98982,#98983,#98984,#98985,#98986,#98987,#98988,#98989,
#98990,#98991,#98992,#98993,#98994,#98995,#98996,#98997,#98998,#98999,#99000,
#99001,#99002,#99003,#99004,#99005,#99006,#99007,#99008,#99009,#99010,#99011,
#99012,#99013,#99014,#99015,#99016,#99017,#99018,#99019,#99020,#99021,#99022,
#99023,#99024,#99025,#99026,#99027,#99028,#99029,#99030,#99031,#99032,#99033,
#99034,#99035,#99036,#99037,#99038,#99039,#99040,#99041,#99042,#99043,#99044,
#99045,#99046,#99047,#99048,#99049,#99050,#99051,#99052,#99053,#99054,#99055,
#99056,#99057,#99058,#99059,#99060,#99061,#99062,#99063,#99064,#99065,#99066,
#99067,#99068,#99069,#99070,#99071,#99072,#99073,#99074,#99075,#99076,#99077,
#99078,#99079,#99080,#99081,#99082,#99083,#99084,#99085,#99086,#99087,#99088,
#99089,#99090,#99091,#99092,#99093,#99094,#99095,#99096,#99097,#99098,#99099,
#99100,#99101,#99102,#99103,#99104,#99105,#99106,#99107,#99108,#99109,#99110,
#99111,#99112,#99113,#99114,#99115,#99116,#99117,#99118,#99119,#99120,#99121,
#99122,#99123,#99124,#99125,#99126,#99127,#99128,#99129,#99130,#99131,#99132,
#99133,#99134,#99135,#99136,#99137,#99138,#99139,#99140,#99141,#99142,#99143,
#99144,#99145,#99146,#99147,#99148,#99149,#99150,#99151,#99152,#99153,#99154,
#99155,#99156,#99157,#99158,#99159,#99160,#99161,#99162,#99163,#99164,#99165,
#99166,#99167,#99168,#99169,#99170,#99171,#99172,#99173,#99174,#99175,#99176,
#99177,#99178,#99179,#99180,#99181,#99182,#99183,#99184,#99185,#99186,#99187,
#99188,#99189,#99190,#99191,#99192),.UNSPECIFIED.,.F.,.F.,(4,2,2,2,2,2,
2,2,2,2,2,2,2,2,2,2,2,2,2,2,2,2,2,2,2,2,2,2,2,2,2,2,2,2,2,2,2,2,2,2,2,2,
2,2,2,2,2,2,2,2,2,2,2,2,2,2,2,2,2,2,2,2,2,2,2,2,2,2,2,2,2,2,2,2,2,2,2,2,
2,2,2,2,2,2,2,2,2,2,2,2,2,2,2,2,2,2,2,2,2,2,2,2,2,2,2,2,2,2,2,2,2,2,2,2,
4),(-1.40850345617201,-1.36250451573646,-1.34494900943431,-1.33419481042488,
-1.33089575910889,-1.32881108876358,-1.32687418677182,-1.32431500164865,
-1.31872847952724,-1.31130510818259,-1.29270347500342,-1.24997538983778,
-1.2273474473027,-1.2244953107059,-1.22311867193607,-1.22204483400428,-1.22080870839955,
-1.2186296690159,-1.20882068857082,-1.15991605969471,-1.1247973117897,-1.1205016822107,
-1.11796017308648,-1.11601924660279,-1.11394566929914,-1.11069657869125,
-1.10038441161275,-1.0838208737984,-1.05095809007793,-1.03712981709347,
-1.03048063830151,-1.01500686837124,-1.01240980420473,-1.01106731386943,
-1.00999623450115,-1.0087355830341,-1.00644381478281,-0.99479749617328,
-0.967532404107712,-0.947347744839536,-0.912839856004122,-0.908553222099429,
-0.906014345009378,-0.904073877213896,-0.901999283978811,-0.898745452814007,
-0.888391612125599,-0.871735724992802,-0.838796771955161,-0.820073798500927,
-0.803159970223715,-0.800504776643279,-0.799149791750072,-0.798077894640733,
-0.796826831193154,-0.794579127428686,-0.783694889469947,-0.759403779996519,
-0.703900320938727,-0.697225379495664,-0.694678172334579,-0.692850075244814,
-0.69091234580841,-0.688345759397979,-0.682717600218909,-0.675223835433109,
-0.656363543322428,-0.62648896074036,-0.604932996834984,-0.590970469428296,
-0.588668080580198,-0.587279772315641,-0.586202302509577,-0.58498828096516,
-0.582908514771049,-0.574439457500337,-0.558088593267182,-0.515618639097743,
-0.488627341173812,-0.484506365326267,-0.482016079125526,-0.480083460080147,
-0.477988168978493,-0.474639431430082,-0.463420964140881,-0.444797703854754,
-0.416498823850429,-0.3794856425165,-0.376648347789939,-0.375274854288603,
-0.374201570617981,-0.37296393266865,-0.370777056715919,-0.361219425346794,
-0.312151972743189,-0.276986587383239,-0.272691408891711,-0.270150390471309,
-0.268209967617141,-0.266137053316455,-0.262889262446382,-0.252778637183708,
-0.236574052786764,-0.198328775589665,-0.16765233551806,-0.164739946623118,
-0.163351838190139,-0.162277199530957,-0.16104927574273,-0.159757267178105,
-0.155110071046882,-0.128864882825383,-0.106990878701804,-0.10555961659102,
-0.0751187452951849),.UNSPECIFIED.);
#977=B_SPLINE_CURVE_WITH_KNOTS('',3,(#99194,#99195,#99196,#99197,#99198,
#99199,#99200,#99201,#99202,#99203,#99204,#99205,#99206,#99207,#99208,#99209,
#99210,#99211,#99212,#99213,#99214,#99215,#99216,#99217,#99218,#99219,#99220,
#99221,#99222,#99223,#99224,#99225,#99226,#99227,#99228,#99229,#99230,#99231,
#99232,#99233,#99234,#99235,#99236,#99237,#99238,#99239,#99240,#99241,#99242,
#99243,#99244,#99245,#99246,#99247,#99248,#99249,#99250,#99251,#99252,#99253,
#99254,#99255,#99256,#99257,#99258,#99259,#99260,#99261,#99262,#99263,#99264,
#99265,#99266,#99267,#99268,#99269,#99270,#99271,#99272,#99273,#99274,#99275,
#99276,#99277,#99278,#99279,#99280,#99281,#99282,#99283,#99284,#99285,#99286,
#99287,#99288,#99289,#99290,#99291,#99292,#99293,#99294,#99295,#99296,#99297,
#99298,#99299,#99300,#99301,#99302,#99303,#99304,#99305,#99306,#99307,#99308,
#99309,#99310,#99311,#99312,#99313,#99314,#99315,#99316,#99317,#99318,#99319,
#99320,#99321,#99322,#99323,#99324,#99325,#99326,#99327,#99328,#99329,#99330,
#99331,#99332,#99333,#99334,#99335,#99336,#99337,#99338,#99339,#99340,#99341,
#99342,#99343,#99344,#99345,#99346,#99347,#99348,#99349,#99350,#99351,#99352,
#99353,#99354,#99355,#99356,#99357,#99358,#99359,#99360,#99361,#99362,#99363,
#99364,#99365,#99366,#99367,#99368,#99369,#99370,#99371,#99372,#99373,#99374),
 .UNSPECIFIED.,.F.,.F.,(4,3,3,3,3,3,3,3,3,3,3,3,3,3,3,3,3,3,3,3,3,3,3,3,
3,3,3,3,3,3,3,3,3,3,3,3,3,3,3,3,3,3,3,3,3,3,3,3,3,3,3,3,3,3,3,3,3,3,3,3,
4),(-28.6232427996483,-28.5202020671231,-28.4171817224122,-28.3141477780892,
-28.2110001872004,-28.1077864185769,-28.0043998212242,-27.9674205989325,
-27.8640258618991,-27.7607845797987,-27.6576646144213,-27.5546100462273,
-27.4515868378846,-27.3485609952273,-27.2454282284644,-27.1422391370698,
-27.0388671437033,-26.9685841489706,-26.8651894118465,-26.7619481296552,
-26.6588281641866,-26.5557735959015,-26.4527503874678,-26.3497245447197,
-26.2465917778669,-26.1434026863829,-26.0400306929286,-25.9697476990087,
-25.8663529620659,-25.7631116800558,-25.6599917147674,-25.5569371466617,
-25.4539139384065,-25.3508880958355,-25.2477553291568,-25.1445662378454,
-25.0411942445594,-24.9709112490469,-24.8675165120623,-24.764275230012,
-24.6611552646861,-24.5581006965446,-24.4550774882552,-24.3520516456517,
-24.2489188789435,-24.145729787604,-24.0423577942927,-23.972074799085,-23.8686800615147,
-23.7654387788756,-23.6623188129593,-23.5592642442267,-23.4562410353463,
-23.3532151921528,-23.2500824248602,-23.1468933329387,-23.0435213390553,
-22.9732383491231,-22.8444301460849,-22.71772832931,-22.6905949549614),
 .UNSPECIFIED.);
#978=B_SPLINE_CURVE_WITH_KNOTS('',3,(#99375,#99376,#99377,#99378),
 .UNSPECIFIED.,.F.,.F.,(4,4),(-22.6905949549614,-22.341147276672),
 .UNSPECIFIED.);
#979=B_SPLINE_CURVE_WITH_KNOTS('',3,(#99384,#99385,#99386,#99387,#99388,
#99389,#99390,#99391,#99392,#99393,#99394,#99395,#99396,#99397,#99398,#99399,
#99400,#99401,#99402,#99403),.UNSPECIFIED.,.F.,.F.,(4,2,2,2,2,2,2,2,2,4),
(-0.0747369786533256,-0.0746917043583635,-0.0441247850379056,-0.0412120543920209,
-0.0398238392008842,-0.0387491436130767,-0.0375211834199767,-0.0362291455859954,
-0.0342514142578872,-0.000628700708297845),.UNSPECIFIED.);
#980=B_SPLINE_CURVE_WITH_KNOTS('',3,(#99404,#99405,#99406,#99407,#99408,
#99409,#99410,#99411,#99412,#99413,#99414,#99415,#99416,#99417,#99418,#99419,
#99420,#99421,#99422,#99423,#99424,#99425,#99426,#99427,#99428,#99429,#99430,
#99431,#99432,#99433,#99434,#99435,#99436,#99437,#99438,#99439,#99440,#99441,
#99442,#99443,#99444,#99445,#99446,#99447,#99448,#99449,#99450,#99451,#99452,
#99453,#99454,#99455,#99456,#99457,#99458,#99459,#99460,#99461,#99462,#99463,
#99464,#99465,#99466,#99467,#99468,#99469,#99470,#99471,#99472,#99473,#99474,
#99475,#99476,#99477,#99478,#99479,#99480,#99481,#99482,#99483,#99484,#99485,
#99486,#99487,#99488,#99489,#99490,#99491,#99492,#99493,#99494,#99495,#99496,
#99497,#99498,#99499,#99500,#99501,#99502,#99503,#99504,#99505,#99506,#99507,
#99508,#99509,#99510,#99511,#99512,#99513,#99514,#99515,#99516,#99517,#99518,
#99519,#99520,#99521,#99522,#99523,#99524,#99525,#99526,#99527,#99528,#99529,
#99530,#99531,#99532,#99533,#99534,#99535,#99536,#99537,#99538,#99539,#99540,
#99541,#99542,#99543,#99544,#99545,#99546,#99547,#99548,#99549,#99550,#99551,
#99552,#99553,#99554,#99555,#99556,#99557,#99558,#99559,#99560,#99561,#99562,
#99563,#99564,#99565,#99566,#99567,#99568,#99569,#99570,#99571,#99572,#99573,
#99574,#99575,#99576,#99577,#99578,#99579,#99580,#99581,#99582,#99583,#99584,
#99585,#99586,#99587,#99588,#99589,#99590,#99591,#99592,#99593,#99594,#99595,
#99596,#99597,#99598,#99599,#99600,#99601,#99602,#99603,#99604,#99605,#99606,
#99607,#99608,#99609,#99610,#99611,#99612,#99613,#99614,#99615,#99616,#99617,
#99618,#99619,#99620,#99621,#99622,#99623),.UNSPECIFIED.,.F.,.F.,(4,2,2,
2,2,2,2,2,2,2,2,2,2,2,2,2,2,2,2,2,2,2,2,2,2,2,2,2,2,2,2,2,2,2,2,2,2,2,2,
2,2,2,2,2,2,2,2,2,2,2,2,2,2,2,2,2,2,2,2,2,2,2,2,2,2,2,2,2,2,2,2,2,2,2,2,
2,2,2,2,2,2,2,2,2,2,2,2,2,2,2,2,2,2,2,2,2,2,2,2,2,2,2,2,2,2,2,2,2,2,4),
(-2.66803233840665,-2.63756098231509,-2.61104504151717,-2.60487784634831,
-2.60221454463273,-2.60026071576239,-2.59845779291116,-2.5955376168873,
-2.58832279345047,-2.54292015830957,-2.52278906795612,-2.50657463302681,
-2.49817823291225,-2.49613083544029,-2.49490269536407,-2.49382769389884,
-2.4924388769836,-2.48952417197382,-2.4594875300262,-2.40817359987131,-2.39935615826286,
-2.39296017747777,-2.39025768383555,-2.38829695675368,-2.38650279568053,
-2.38363008350252,-2.37669952838482,-2.32423037013766,-2.29789168812594,
-2.28647459224803,-2.2841956462714,-2.28293774015966,-2.28186639356041,
-2.28052025914637,-2.27790647491917,-2.26202755774909,-2.25734580100041,
-2.21491157309143,-2.18434974916272,-2.17990944461745,-2.17757644393979,
-2.17566431249257,-2.17344774309271,-2.16965253765773,-2.15496801665183,
-2.1427186298469,-2.10720583685401,-2.08476940723062,-2.07439567095383,
-2.07217959453477,-2.07093541917591,-2.06986274847982,-2.06849815981428,
-2.06579801463128,-2.0476114225318,-2.02952941819104,-1.99679984642993,
-1.97430061116869,-1.96865496205343,-1.96608497612474,-1.96414654745937,
-1.96231916850218,-1.95977517649344,-1.95312195390438,-1.89741705405606,
-1.87328022634548,-1.86243622495129,-1.86019079897614,-1.85894014579244,
-1.85786807594353,-1.8565121932485,-1.85436746745846,-1.84334738178677,
-1.79204768598337,-1.76338076399131,-1.75695165432538,-1.75424351532098,
-1.75228172714543,-1.75048868410597,-1.74762231192975,-1.74073057730078,
-1.68773195233868,-1.66176214196635,-1.65043831385018,-1.64816464980308,
-1.64690786969298,-1.64583639677136,-1.64448872223772,-1.64186789011254,
-1.62584195655305,-1.62044596501797,-1.60594088498659,-1.57304501320094,
-1.55028833588863,-1.54460772337546,-1.54203121186659,-1.54009166988328,
-1.53826603501481,-1.53572894730415,-1.52912027839379,-1.472970285587,-1.44912112120558,
-1.43835460474416,-1.4361137768135,-1.43486407351235,-1.43379182328975,
-1.43243443547867,-1.42976867024961,-1.41258192057445,-1.40850345617201),
 .UNSPECIFIED.);
#981=B_SPLINE_CURVE_WITH_KNOTS('',3,(#99625,#99626,#99627,#99628,#99629,
#99630,#99631,#99632,#99633,#99634),.UNSPECIFIED.,.F.,.F.,(4,1,1,1,1,1,
1,4),(-22.341147276672,-21.9744018991612,-20.9755654491994,-19.9767289992375,
-18.9778925492756,-17.9790560993137,-16.9802196493519,-16.4074096477818),
 .UNSPECIFIED.);
#982=B_SPLINE_CURVE_WITH_KNOTS('',3,(#99635,#99636,#99637,#99638,#99639,
#99640),.UNSPECIFIED.,.F.,.F.,(4,2,4),(-2.66742168919182,-2.60891632325169,
-2.59315595175498),.UNSPECIFIED.);
#983=B_SPLINE_CURVE_WITH_KNOTS('',3,(#99645,#99646,#99647,#99648,#99649,
#99650,#99651,#99652,#99653,#99654,#99655,#99656,#99657,#99658,#99659,#99660,
#99661,#99662,#99663,#99664,#99665,#99666,#99667,#99668,#99669,#99670,#99671,
#99672,#99673,#99674,#99675,#99676,#99677,#99678,#99679,#99680,#99681,#99682,
#99683,#99684,#99685,#99686,#99687,#99688,#99689,#99690,#99691,#99692,#99693,
#99694,#99695,#99696,#99697,#99698,#99699,#99700,#99701,#99702,#99703,#99704,
#99705,#99706,#99707,#99708,#99709,#99710,#99711,#99712,#99713,#99714,#99715,
#99716,#99717,#99718,#99719,#99720,#99721,#99722,#99723,#99724,#99725,#99726,
#99727,#99728,#99729,#99730,#99731,#99732,#99733,#99734,#99735,#99736,#99737,
#99738,#99739,#99740,#99741,#99742,#99743,#99744,#99745,#99746,#99747,#99748,
#99749,#99750,#99751,#99752,#99753,#99754,#99755,#99756,#99757,#99758,#99759,
#99760,#99761,#99762,#99763,#99764,#99765,#99766,#99767,#99768,#99769,#99770,
#99771,#99772,#99773,#99774,#99775,#99776,#99777,#99778,#99779,#99780,#99781,
#99782,#99783,#99784,#99785,#99786,#99787,#99788,#99789,#99790,#99791,#99792,
#99793,#99794,#99795,#99796,#99797,#99798,#99799,#99800,#99801,#99802,#99803,
#99804,#99805,#99806,#99807,#99808,#99809,#99810,#99811,#99812,#99813,#99814,
#99815,#99816,#99817,#99818,#99819,#99820,#99821,#99822,#99823,#99824,#99825,
#99826,#99827,#99828,#99829,#99830,#99831,#99832,#99833,#99834,#99835,#99836,
#99837,#99838,#99839,#99840,#99841,#99842,#99843,#99844,#99845,#99846,#99847,
#99848,#99849,#99850,#99851,#99852,#99853,#99854,#99855,#99856,#99857,#99858,
#99859,#99860,#99861,#99862,#99863,#99864,#99865,#99866,#99867,#99868),
 .UNSPECIFIED.,.F.,.F.,(4,2,2,2,2,2,2,2,2,2,2,2,2,2,2,2,2,2,2,2,2,2,2,2,
2,2,2,2,2,2,2,2,2,2,2,2,2,2,2,2,2,2,2,2,2,2,2,2,2,2,2,2,2,2,2,2,2,2,2,2,
2,2,2,2,2,2,2,2,2,2,2,2,2,2,2,2,2,2,2,2,2,2,2,2,2,2,2,2,2,2,2,2,2,2,2,2,
2,2,2,2,2,2,2,2,2,2,2,2,2,2,2,4),(-1.40835994883514,-1.36496506558018,-1.33391364373284,
-1.31586282059911,-1.31316705999715,-1.31180334434074,-1.31073066522904,
-1.30948568806857,-1.30726626420923,-1.2968425515049,-1.27422806295316,
-1.21610121026393,-1.20971724338068,-1.20721686303649,-1.2054009159603,
-1.20345603859551,-1.20084540259578,-1.19497607013632,-1.17079842029402,
-1.12031274141491,-1.11988217351818,-1.10369440289438,-1.1010672943475,
-1.09971827769369,-1.0986467310789,-1.09739102239637,-1.0951222013546,-1.08388219691806,
-1.05823696210302,-1.0047299889714,-0.997875830436784,-0.995015684784422,
-0.993223806884562,-0.991261100244711,-0.988547655634353,-0.982086738624371,
-0.928142472106462,-0.891938229429457,-0.889083296460058,-0.887706160402034,
-0.886632335220905,-0.88539667680955,-0.883219546047789,-0.873437169264997,
-0.824513737505249,-0.789389722855819,-0.785094260725997,-0.782552881291843,
-0.780612071524827,-0.778538636076012,-0.775289803628643,-0.764978759501409,
-0.748417316710418,-0.715557434330294,-0.701818968594614,-0.694962270382339,
-0.694630896294975,-0.679575430470702,-0.677223593877109,-0.675820747720329,
-0.674741303903174,-0.673535405043201,-0.671492393166578,-0.66347021817228,
-0.648388371998441,-0.609029401102905,-0.577343038478701,-0.573108420984722,
-0.570584785065836,-0.568646917695049,-0.566566257155397,-0.563284255140809,
-0.552679768363485,-0.535463692706438,-0.488765062601624,-0.483699710436784,
-0.467678455037713,-0.465058089554265,-0.463710621449197,-0.462639295186871,
-0.461382672922729,-0.459109244683259,-0.447786119972239,-0.421813981997778,
-0.368788719256553,-0.361897881478697,-0.359031896395174,-0.357239102634568,
-0.355277598796495,-0.352569865805326,-0.346141767713424,-0.296439522833372,
-0.277531765598874,-0.271357445521186,-0.255652001523959,-0.253045247285455,
-0.251700742085052,-0.250629639458679,-0.249370802229852,-0.247132974643905,
-0.236261769431149,-0.211953870815406,-0.156483392049982,-0.149806229631321,
-0.147258804324013,-0.145430745588595,-0.143493235702129,-0.140927243534818,
-0.135301616819205,-0.116186404503192,-0.0947905862222214,-0.0747369786533256),
 .UNSPECIFIED.);
#984=B_SPLINE_CURVE_WITH_KNOTS('',3,(#99869,#99870,#99871,#99872,#99873,
#99874,#99875,#99876,#99877,#99878,#99879,#99880,#99881,#99882,#99883,#99884,
#99885,#99886,#99887,#99888,#99889,#99890,#99891,#99892,#99893,#99894,#99895,
#99896,#99897,#99898,#99899,#99900,#99901,#99902,#99903,#99904,#99905,#99906,
#99907,#99908,#99909,#99910,#99911,#99912,#99913,#99914,#99915,#99916,#99917,
#99918,#99919,#99920,#99921,#99922,#99923,#99924,#99925,#99926,#99927,#99928,
#99929,#99930,#99931,#99932,#99933,#99934,#99935,#99936,#99937,#99938,#99939,
#99940,#99941,#99942,#99943,#99944,#99945,#99946,#99947,#99948,#99949,#99950,
#99951,#99952,#99953,#99954,#99955,#99956,#99957,#99958,#99959,#99960,#99961,
#99962,#99963,#99964,#99965,#99966,#99967,#99968,#99969,#99970,#99971,#99972,
#99973,#99974,#99975,#99976,#99977,#99978,#99979,#99980,#99981,#99982,#99983,
#99984,#99985,#99986,#99987,#99988,#99989,#99990,#99991,#99992,#99993,#99994,
#99995,#99996,#99997,#99998,#99999,#100000,#100001,#100002,#100003,#100004,
#100005,#100006,#100007,#100008,#100009,#100010,#100011,#100012,#100013,
#100014,#100015,#100016,#100017,#100018,#100019,#100020,#100021,#100022,
#100023,#100024,#100025,#100026,#100027,#100028,#100029,#100030,#100031,
#100032,#100033,#100034,#100035,#100036,#100037,#100038,#100039,#100040,
#100041,#100042,#100043,#100044,#100045,#100046,#100047,#100048,#100049,
#100050,#100051,#100052,#100053,#100054,#100055,#100056,#100057,#100058,
#100059,#100060,#100061,#100062,#100063,#100064,#100065,#100066,#100067,
#100068,#100069,#100070,#100071,#100072,#100073,#100074,#100075,#100076,
#100077,#100078,#100079,#100080,#100081,#100082,#100083,#100084,#100085,
#100086,#100087,#100088,#100089,#100090,#100091,#100092,#100093,#100094,
#100095,#100096,#100097,#100098,#100099,#100100,#100101,#100102),
 .UNSPECIFIED.,.F.,.F.,(4,2,2,2,2,2,2,2,2,2,2,2,2,2,2,2,2,2,2,2,2,2,2,2,
2,2,2,2,2,2,2,2,2,2,2,2,2,2,2,2,2,2,2,2,2,2,2,2,2,2,2,2,2,2,2,2,2,2,2,2,
2,2,2,2,2,2,2,2,2,2,2,2,2,2,2,2,2,2,2,2,2,2,2,2,2,2,2,2,2,2,2,2,2,2,2,2,
2,2,2,2,2,2,2,2,2,2,2,2,2,2,2,2,2,2,2,2,4),(-2.59315595175498,-2.59007765275903,
-2.58078447923624,-2.57864198428897,-2.57741407158795,-2.57633924894897,
-2.57495063650189,-2.57203626622376,-2.54226190570917,-2.49162780586257,
-2.48229537460191,-2.47774308858225,-2.47500472226365,-2.47252035112126,
-2.47064426401568,-2.46881786361953,-2.46627671620563,-2.45963978199326,
-2.40381757790562,-2.37976765768529,-2.36894792452057,-2.3667042753065,
-2.36545415640015,-2.36438225645688,-2.36302622165248,-2.36088057815684,
-2.34984137340878,-2.29863196780722,-2.26992326006183,-2.26348974153481,
-2.26078115893801,-2.25881956202766,-2.25702704627416,-2.25416228338041,
-2.24727838555588,-2.19420739795661,-2.16829981453399,-2.15699274373935,
-2.15472035019834,-2.15346399068911,-2.15239271826015,-2.15104508986307,
-2.14842370921987,-2.13238317709358,-2.12707675461306,-2.11250768316067,
-2.07961731534741,-2.06305116899584,-2.05273924434692,-2.04949046792405,
-2.0474171553536,-2.04547652252956,-2.04293546559637,-2.03864078494573,
-2.00353525182107,-1.95465260835331,-1.94486020574292,-1.94268258638578,
-1.9414469068712,-1.94037323118513,-1.93899649901611,-1.93614315182974,
-1.9134506950524,-1.87272384866466,-1.8456806874179,-1.8394485375509,-1.83677416923669,
-1.83481856897838,-1.83301845087596,-1.8301126932048,-1.82298257636981,
-1.77422308648144,-1.735052660683,-1.7314780270815,-1.72996902053583,-1.72887685708661,
-1.72785086943613,-1.72610764747515,-1.72137451372362,-1.68180129920979,
-1.63388992385648,-1.62749311324278,-1.62479053644258,-1.62282984461181,
-1.62103578113662,-1.61816336611532,-1.61123424082424,-1.55875512132802,
-1.53242866751436,-1.52101503212502,-1.51873640125128,-1.51747861856325,
-1.51640744559843,-1.51506158295104,-1.51244823517107,-1.49656816267521,
-1.4906980547015,-1.44666701273634,-1.42810815161094,-1.41691845302898,
-1.41357286005854,-1.41147833449995,-1.40954560744237,-1.40705404760251,
-1.40292854603029,-1.37574265806748,-1.33373204506974,-1.32763511641381,
-1.30978754718718,-1.30709916290768,-1.30573723447465,-1.30466495342069,
-1.30341928442914,-1.3011958618825,-1.29070305756573,-1.26784057103001,
-1.2596092791427),.UNSPECIFIED.);
#985=B_SPLINE_CURVE_WITH_KNOTS('',3,(#100108,#100109,#100110,#100111,#100112,
#100113,#100114,#100115,#100116,#100117,#100118,#100119,#100120,#100121,
#100122,#100123,#100124,#100125,#100126,#100127,#100128,#100129,#100130,
#100131,#100132,#100133,#100134,#100135,#100136,#100137,#100138,#100139,
#100140,#100141,#100142,#100143,#100144,#100145,#100146,#100147,#100148,
#100149,#100150,#100151,#100152,#100153,#100154,#100155,#100156,#100157,
#100158,#100159,#100160,#100161,#100162,#100163,#100164,#100165,#100166,
#100167,#100168,#100169,#100170,#100171,#100172,#100173,#100174,#100175,
#100176,#100177,#100178,#100179,#100180,#100181,#100182,#100183,#100184,
#100185,#100186,#100187,#100188,#100189,#100190,#100191,#100192,#100193,
#100194,#100195,#100196,#100197,#100198,#100199,#100200,#100201,#100202,
#100203,#100204,#100205,#100206,#100207,#100208,#100209,#100210,#100211,
#100212,#100213),.UNSPECIFIED.,.F.,.F.,(4,3,3,3,3,3,3,3,3,3,3,3,3,3,3,3,
3,3,3,3,3,3,3,3,3,3,3,3,3,3,3,3,3,3,3,4),(-3.4905420523601,-3.38888724871603,
-3.2871461686745,-3.18536353037361,-3.08340260597814,-2.99650934988562,
-2.89298805351487,-2.78961775740443,-2.68636579627279,-2.58317747650148,
-2.48001897640827,-2.37685651582113,-2.27358608503739,-2.17025853571452,
-2.0667483835289,-1.99767289992375,-1.89536967835424,-1.79322051059792,
-1.69118874726443,-1.58921969074132,-1.48727797529671,-1.3853282756702,
-1.28325622478001,-1.18112117613606,-1.07878042700533,-0.998836449961875,
-0.892562662128034,-0.78099232936203,-0.675071864520977,-0.569250995903944,
-0.463501983636266,-0.357797177553288,-0.252079241114024,-0.146356223433945,
-0.0405602493167351,0.),.UNSPECIFIED.);
#986=B_SPLINE_CURVE_WITH_KNOTS('',3,(#100216,#100217,#100218,#100219,#100220,
#100221,#100222,#100223,#100224,#100225,#100226,#100227,#100228,#100229,
#100230,#100231,#100232,#100233,#100234,#100235,#100236,#100237,#100238,
#100239,#100240,#100241,#100242,#100243,#100244,#100245,#100246,#100247,
#100248,#100249,#100250,#100251,#100252,#100253,#100254,#100255,#100256,
#100257,#100258,#100259,#100260,#100261,#100262,#100263,#100264,#100265,
#100266,#100267,#100268,#100269,#100270,#100271,#100272,#100273,#100274,
#100275,#100276,#100277,#100278,#100279,#100280,#100281,#100282,#100283,
#100284,#100285,#100286,#100287,#100288,#100289,#100290,#100291,#100292,
#100293,#100294,#100295,#100296,#100297,#100298,#100299,#100300,#100301,
#100302,#100303,#100304,#100305,#100306,#100307,#100308,#100309,#100310,
#100311,#100312,#100313,#100314,#100315,#100316,#100317,#100318,#100319,
#100320,#100321,#100322,#100323,#100324,#100325,#100326,#100327,#100328,
#100329,#100330,#100331,#100332,#100333,#100334,#100335,#100336,#100337,
#100338,#100339,#100340,#100341,#100342,#100343,#100344,#100345,#100346,
#100347,#100348,#100349,#100350,#100351,#100352,#100353,#100354,#100355,
#100356,#100357,#100358,#100359,#100360,#100361,#100362,#100363,#100364,
#100365,#100366,#100367,#100368,#100369,#100370,#100371,#100372,#100373,
#100374,#100375),.UNSPECIFIED.,.F.,.F.,(4,3,3,3,3,3,3,3,3,3,3,3,3,3,3,3,
3,3,3,3,3,3,3,3,3,3,3,3,3,3,3,3,3,3,3,3,3,3,3,3,3,3,3,3,3,3,3,3,3,3,3,3,
3,4),(2.00878451797959,2.11210382153688,2.21526971314838,2.31831418782034,
2.42129345937127,2.5242416735564,2.62719293310596,2.73024899451787,2.83336205194682,
2.93665137518733,2.99650934988563,3.10008229381611,3.20350554280195,3.30681219802198,
3.4100562611044,3.51327148737704,3.61649159166828,3.71982072762219,3.82320766651887,
3.9267776968677,3.9953457998475,4.09860816546048,4.20171516905877,4.30469864795505,
4.40761543749366,4.51049977143292,4.61338583911078,4.71637840074732,4.81942682496838,
4.92265896654807,4.99418224980938,5.09760356589108,5.20087152694815,5.30401818826618,
5.40709944854827,5.51014930542219,5.61320171332603,5.71636073031365,5.81957593612848,
5.92297353214027,5.99301869977126,6.09643423322207,6.19969677808619,6.30283860095652,
6.40591538148351,6.50896112490232,6.61200979362757,6.71516567854846,6.81837808737287,
6.92177346211855,6.99185514973313,7.09672279961553,7.20139615639989,7.24304095782437),
 .UNSPECIFIED.);
#987=B_SPLINE_CURVE_WITH_KNOTS('',3,(#100381,#100382,#100383,#100384,#100385,
#100386,#100387,#100388,#100389,#100390,#100391,#100392,#100393,#100394,
#100395,#100396,#100397,#100398,#100399,#100400,#100401,#100402,#100403,
#100404,#100405,#100406),.UNSPECIFIED.,.F.,.F.,(4,2,2,2,2,2,2,2,2,2,2,2,
4),(-0.0747573277194267,-0.0739378941382004,-0.0616381618967872,-0.0559574691575537,
-0.0377855769967214,-0.0350634362630029,-0.0337175254258632,-0.032648440440134,
-0.0316335698164161,-0.0303960777140638,-0.0285521057197913,-0.0215326867205031,
-0.00065555548774641),.UNSPECIFIED.);
#988=B_SPLINE_CURVE_WITH_KNOTS('',3,(#100408,#100409,#100410,#100411,#100412,
#100413,#100414,#100415,#100416,#100417,#100418,#100419,#100420,#100421,
#100422,#100423,#100424,#100425,#100426,#100427,#100428,#100429,#100430,
#100431,#100432,#100433,#100434,#100435,#100436,#100437,#100438,#100439,
#100440,#100441,#100442,#100443,#100444,#100445,#100446,#100447,#100448,
#100449,#100450,#100451,#100452,#100453,#100454,#100455,#100456,#100457,
#100458,#100459,#100460,#100461,#100462,#100463,#100464,#100465,#100466,
#100467,#100468,#100469,#100470,#100471,#100472,#100473,#100474,#100475,
#100476,#100477,#100478,#100479,#100480,#100481,#100482,#100483,#100484,
#100485,#100486,#100487,#100488,#100489,#100490,#100491,#100492,#100493,
#100494,#100495,#100496,#100497,#100498,#100499,#100500,#100501,#100502,
#100503,#100504,#100505,#100506,#100507,#100508,#100509,#100510,#100511,
#100512,#100513,#100514,#100515,#100516,#100517,#100518,#100519,#100520,
#100521,#100522,#100523,#100524,#100525),.UNSPECIFIED.,.F.,.F.,(4,3,3,3,
3,3,3,3,3,3,3,3,3,3,3,3,3,3,3,3,3,3,3,3,3,3,3,3,3,3,3,3,3,3,3,3,3,3,3,4),
(170.955339710339,171.060905920727,171.162663399122,171.264353089028,171.366010721803,
171.467671980259,171.569433774519,171.671256094535,171.773239607341,171.799869393442,
171.903390392073,172.006760388742,172.110012049377,172.213200068173,172.316358267267,
172.419520427281,172.522790560255,172.626117812871,172.729627673424,172.798705843404,
172.901009665115,173.003159435031,173.105191801349,173.207161461353,173.309103780221,
173.411054082656,173.513126731748,173.615262377252,173.717603714352,173.797542293366,
173.903815640338,174.015386028212,174.121306049069,174.227126474861,174.332875046754,
174.43857941621,174.544296925171,174.650019520939,174.75581508523,174.796378743328),
 .UNSPECIFIED.);
#989=B_SPLINE_CURVE_WITH_KNOTS('',3,(#100529,#100530,#100531,#100532,#100533,
#100534,#100535,#100536,#100537,#100538,#100539,#100540,#100541,#100542,
#100543,#100544,#100545,#100546,#100547,#100548,#100549,#100550,#100551,
#100552,#100553,#100554,#100555,#100556,#100557,#100558,#100559,#100560,
#100561,#100562,#100563,#100564,#100565,#100566,#100567,#100568,#100569,
#100570,#100571,#100572,#100573,#100574,#100575,#100576,#100577,#100578,
#100579,#100580,#100581,#100582,#100583,#100584,#100585,#100586,#100587,
#100588,#100589,#100590,#100591,#100592,#100593,#100594,#100595,#100596,
#100597,#100598,#100599,#100600,#100601,#100602,#100603,#100604,#100605,
#100606,#100607,#100608,#100609,#100610,#100611,#100612,#100613,#100614,
#100615,#100616,#100617,#100618,#100619,#100620,#100621,#100622,#100623,
#100624,#100625,#100626,#100627,#100628,#100629,#100630,#100631,#100632,
#100633,#100634,#100635,#100636,#100637,#100638,#100639,#100640,#100641,
#100642,#100643,#100644,#100645,#100646,#100647,#100648,#100649,#100650,
#100651,#100652,#100653,#100654,#100655,#100656,#100657,#100658,#100659,
#100660,#100661,#100662,#100663,#100664,#100665,#100666,#100667,#100668,
#100669,#100670,#100671,#100672,#100673,#100674,#100675,#100676,#100677,
#100678,#100679,#100680,#100681,#100682,#100683,#100684,#100685,#100686,
#100687,#100688,#100689,#100690,#100691,#100692,#100693,#100694,#100695,
#100696,#100697),.UNSPECIFIED.,.F.,.F.,(4,3,3,3,3,3,3,3,3,3,3,3,3,3,3,3,
3,3,3,3,3,3,3,3,3,3,3,3,3,3,3,3,3,3,3,3,3,3,3,3,3,3,3,3,3,3,3,3,3,3,3,3,
3,3,3,3,4),(-172.787594225567,-172.684274861804,-172.581108909343,-172.478064373147,
-172.375085039686,-172.272136763294,-172.169185441327,-172.066129317591,
-171.963016197798,-171.859726812786,-171.799869393442,-171.696296438965,
-171.592873179124,-171.489566512639,-171.386322438044,-171.283107200028,
-171.179887083779,-171.076557935617,-170.973170984353,-170.869600941516,
-170.80103294348,-170.697770604844,-170.594663628611,-170.491680177536,
-170.388763416087,-170.285879110466,-170.182993071298,-170.080000538274,
-169.976952142771,-169.873720029761,-169.802196493519,-169.698775165844,
-169.595507193078,-169.492360519935,-169.389279247763,-169.286229378952,
-169.183176959081,-169.080017930163,-168.97680271242,-168.873405104616,
-168.803360043557,-168.69994450726,-168.59668195947,-168.493540133569,-168.390463349949,
-168.287417603378,-168.184368931446,-168.081213043256,-167.978000631122,
-167.874605253038,-167.804523593595,-167.699671753546,-167.594987925042,
-167.490464843253,-167.386036589514,-167.281667049056,-167.203857020092),
 .UNSPECIFIED.);
#990=B_SPLINE_CURVE_WITH_KNOTS('',3,(#100698,#100699,#100700,#100701,#100702,
#100703,#100704,#100705),.UNSPECIFIED.,.F.,.F.,(4,2,2,4),(-2.66736290127704,
-2.64532399614163,-2.59645533662874,-2.59317160363215),.UNSPECIFIED.);
#991=B_SPLINE_CURVE_WITH_KNOTS('',3,(#100710,#100711,#100712,#100713,#100714,
#100715,#100716,#100717,#100718,#100719,#100720,#100721,#100722,#100723,
#100724,#100725,#100726,#100727,#100728,#100729,#100730,#100731,#100732,
#100733,#100734,#100735,#100736,#100737,#100738,#100739,#100740,#100741,
#100742,#100743,#100744,#100745,#100746,#100747,#100748,#100749,#100750,
#100751,#100752,#100753,#100754,#100755,#100756,#100757,#100758,#100759,
#100760,#100761,#100762,#100763,#100764,#100765,#100766,#100767,#100768,
#100769,#100770,#100771,#100772,#100773,#100774,#100775,#100776,#100777,
#100778,#100779,#100780,#100781,#100782,#100783,#100784,#100785,#100786,
#100787,#100788,#100789,#100790,#100791,#100792,#100793,#100794,#100795,
#100796,#100797,#100798,#100799,#100800,#100801,#100802,#100803,#100804,
#100805,#100806,#100807,#100808,#100809,#100810,#100811,#100812,#100813,
#100814,#100815,#100816,#100817,#100818,#100819,#100820,#100821,#100822,
#100823,#100824,#100825,#100826,#100827,#100828,#100829,#100830,#100831,
#100832,#100833,#100834,#100835,#100836,#100837,#100838,#100839,#100840,
#100841,#100842,#100843,#100844,#100845,#100846,#100847,#100848,#100849,
#100850,#100851,#100852,#100853,#100854,#100855,#100856,#100857,#100858,
#100859,#100860,#100861,#100862,#100863,#100864,#100865,#100866,#100867,
#100868,#100869,#100870,#100871,#100872,#100873,#100874,#100875,#100876,
#100877,#100878,#100879,#100880,#100881,#100882,#100883,#100884,#100885,
#100886,#100887,#100888,#100889,#100890,#100891,#100892,#100893,#100894,
#100895,#100896,#100897,#100898,#100899,#100900,#100901,#100902,#100903,
#100904,#100905,#100906,#100907,#100908,#100909,#100910,#100911,#100912,
#100913,#100914,#100915,#100916,#100917,#100918,#100919,#100920,#100921,
#100922,#100923,#100924,#100925,#100926,#100927,#100928,#100929,#100930,
#100931,#100932,#100933,#100934,#100935),.UNSPECIFIED.,.F.,.F.,(4,2,2,2,
2,2,2,2,2,2,2,2,2,2,2,2,2,2,2,2,2,2,2,2,2,2,2,2,2,2,2,2,2,2,2,2,2,2,2,2,
2,2,2,2,2,2,2,2,2,2,2,2,2,2,2,2,2,2,2,2,2,2,2,2,2,2,2,2,2,2,2,2,2,2,2,2,
2,2,2,2,2,2,2,2,2,2,2,2,2,2,2,2,2,2,2,2,2,2,2,2,2,2,2,2,2,2,2,2,2,2,2,2,
4),(-1.4081797697387,-1.40705404714931,-1.40292854411527,-1.37574263943028,
-1.33373204743589,-1.32763514664634,-1.30978755123619,-1.3070991652891,
-1.30573723616672,-1.30466495463486,-1.30341928512133,-1.301195861737,-1.29070305468652,
-1.26784056022145,-1.21011173592253,-1.20367846621418,-1.20117010501504,
-1.19935224701617,-1.19740895594777,-1.19480674943785,-1.18898302718057,
-1.16514968570941,-1.11614973854379,-1.09779133429622,-1.09505199332823,
-1.09369780383667,-1.09262570304137,-1.09137328624521,-1.08912118833557,
-1.07817669697512,-1.05366058560861,-0.998557346910655,-0.991850158247918,
-0.989297544378724,-0.987467677688094,-0.985530001805971,-0.982966744492849,
-0.977359005991215,-0.929075125906758,-0.888723661534737,-0.884011299437307,
-0.882271324735715,-0.881246040259428,-0.880154604889832,-0.878645310963095,
-0.875062793117107,-0.870037675276166,-0.856213838582042,-0.833862609949703,
-0.787184867132219,-0.779989358286537,-0.777074355966871,-0.775273839853719,
-0.773322016017773,-0.770660377629352,-0.764492324022858,-0.737949806688716,
-0.698621228221383,-0.687287896511326,-0.673503643387962,-0.671211235544451,
-0.669826498440482,-0.668750047594006,-0.667534919431082,-0.665449594656343,
-0.656908206301732,-0.640348116914734,-0.598278238352605,-0.57109944187056,
-0.566971916353919,-0.564479092054117,-0.562545350303252,-0.560449685724274,
-0.55710216985586,-0.545904434824394,-0.527329229983804,-0.484804714632695,
-0.462028507280671,-0.459170643093303,-0.457791987418327,-0.456715722935139,
-0.455474742004388,-0.453287138242549,-0.443435079069284,-0.394232801530741,
-0.359839181976366,-0.355551477040888,-0.353009480827242,-0.351065107595321,
-0.348984818375656,-0.345718785888289,-0.335297078628961,-0.318505419793005,
-0.258883142282707,-0.249294128815231,-0.247244796286734,-0.245918179968781,
-0.244851141091832,-0.24384142056391,-0.241869026745214,-0.234451027456367,
-0.220917652702534,-0.192337636238333,-0.147271551995062,-0.143024731489448,
-0.14050666203384,-0.138580655494789,-0.136520215481735,-0.1332860526252,
-0.122977092776369,-0.106384522418824,-0.0845184776757566,-0.0747573277194267),
 .UNSPECIFIED.);
#992=B_SPLINE_CURVE_WITH_KNOTS('',3,(#100936,#100937,#100938,#100939,#100940,
#100941,#100942,#100943,#100944,#100945,#100946,#100947,#100948,#100949,
#100950,#100951,#100952,#100953,#100954,#100955,#100956,#100957,#100958,
#100959,#100960,#100961,#100962,#100963,#100964,#100965,#100966,#100967,
#100968,#100969,#100970,#100971,#100972,#100973,#100974,#100975,#100976,
#100977,#100978,#100979,#100980,#100981,#100982,#100983,#100984,#100985,
#100986,#100987,#100988,#100989,#100990,#100991,#100992,#100993,#100994,
#100995,#100996,#100997,#100998,#100999,#101000,#101001,#101002,#101003,
#101004,#101005,#101006,#101007,#101008,#101009,#101010,#101011,#101012,
#101013,#101014,#101015,#101016,#101017,#101018,#101019,#101020,#101021,
#101022,#101023,#101024,#101025,#101026,#101027,#101028,#101029,#101030,
#101031,#101032,#101033,#101034,#101035,#101036,#101037,#101038,#101039,
#101040,#101041,#101042,#101043,#101044,#101045,#101046,#101047,#101048,
#101049,#101050,#101051,#101052,#101053,#101054,#101055,#101056,#101057,
#101058,#101059,#101060,#101061,#101062,#101063,#101064,#101065,#101066,
#101067,#101068,#101069,#101070,#101071,#101072,#101073,#101074,#101075,
#101076,#101077,#101078,#101079,#101080,#101081,#101082,#101083,#101084,
#101085,#101086,#101087,#101088,#101089,#101090,#101091,#101092,#101093,
#101094,#101095,#101096,#101097,#101098,#101099,#101100,#101101,#101102,
#101103,#101104,#101105,#101106,#101107,#101108,#101109,#101110,#101111,
#101112,#101113,#101114,#101115,#101116,#101117,#101118,#101119,#101120,
#101121,#101122,#101123,#101124,#101125,#101126,#101127,#101128,#101129,
#101130,#101131,#101132,#101133,#101134,#101135,#101136,#101137,#101138,
#101139,#101140,#101141,#101142,#101143,#101144,#101145,#101146,#101147,
#101148,#101149,#101150,#101151,#101152,#101153,#101154,#101155,#101156,
#101157,#101158,#101159,#101160,#101161,#101162,#101163,#101164,#101165,
#101166,#101167,#101168,#101169,#101170,#101171,#101172,#101173,#101174,
#101175),.UNSPECIFIED.,.F.,.F.,(4,2,2,2,2,2,2,2,2,2,2,2,2,2,2,2,2,2,2,2,
2,2,2,2,2,2,2,2,2,2,2,2,2,2,2,2,2,2,2,2,2,2,2,2,2,2,2,2,2,2,2,2,2,2,2,2,
2,2,2,2,2,2,2,2,2,2,2,2,2,2,2,2,2,2,2,2,2,2,2,2,2,2,2,2,2,2,2,2,2,2,2,2,
2,2,2,2,2,2,2,2,2,2,2,2,2,2,2,2,2,2,2,2,2,2,2,2,2,2,2,4),(-2.59317160363215,
-2.58673594885869,-2.5845650297111,-2.5833317076338,-2.58225834819646,-2.58088032048256,
-2.57802034512731,-2.5419520152714,-2.50922401730088,-2.49284808246887,
-2.48605327914976,-2.48242696514828,-2.47932638804408,-2.47731985469502,
-2.47537866641607,-2.47283720339729,-2.46854251759948,-2.43358181895235,
-2.38476481586845,-2.37483908478156,-2.37265165323965,-2.37141340106578,
-2.37033969954126,-2.36896559378469,-2.3667606918179,-2.3547091910955,-2.35183965736574,
-2.34965884917676,-2.30370989443497,-2.2758044003634,-2.26946736754952,
-2.26677514184139,-2.26481648830571,-2.26302050320473,-2.26013671425176,
-2.25313750149361,-2.20171508737932,-2.1746326890419,-2.16303119512499,
-2.16074228671133,-2.15948241638636,-2.15841156517565,-2.15706880089489,
-2.15446949392708,-2.13893283302613,-2.13230550553906,-2.1184955936798,
-2.08561373455522,-2.06905687058442,-2.05874943017676,-2.05550143297457,
-2.05342846997416,-2.05148806203009,-2.04894715383983,-2.04465240459036,
-2.00951436769706,-1.9605727969908,-1.95086005968978,-1.94868809347177,
-1.94745375857685,-1.94637995106671,-1.94500141691688,-1.94213896761604,
-1.91877979985089,-1.90648241058348,-1.87361338966278,-1.85707369761816,
-1.84677342475686,-1.84352574329631,-1.84145250701174,-1.8395115070941,
-1.83696933507209,-1.83267134101501,-1.797329041018,-1.74815524971566,-1.73883781275927,
-1.73669328523529,-1.73546477758897,-1.73438985462556,-1.73300162788225,
-1.73008976366529,-1.69805880582034,-1.66514626925938,-1.64631885454103,
-1.63883435206517,-1.63321196328138,-1.63064632194556,-1.62870861843629,
-1.6268800432745,-1.62433136160931,-1.61764757677461,-1.56225455513589,
-1.53791207396448,-1.52701304662379,-1.52476438780703,-1.52351307202462,
-1.52244113574071,-1.52108632253533,-1.51843212865549,-1.50154965032546,
-1.48276192697767,-1.44979585562423,-1.43314256746031,-1.4227907804727,
-1.41953707096079,-1.41746243701401,-1.41552184894916,-1.41298269759226,
-1.40869537185761,-1.3649344835269,-1.33388337229201,-1.3158327292564,-1.31313699566266,
-1.31177329368198,-1.31070062533052,-1.30945566066131,-1.30723625909767,
-1.29681265159966,-1.27419839242439,-1.2597140489769),.UNSPECIFIED.);
#993=B_SPLINE_CURVE_WITH_KNOTS('',3,(#101181,#101182,#101183,#101184),
 .UNSPECIFIED.,.F.,.F.,(4,4),(158.039785877565,158.388969095546),
 .UNSPECIFIED.);
#994=B_SPLINE_CURVE_WITH_KNOTS('',3,(#101185,#101186,#101187,#101188,#101189,
#101190,#101191,#101192,#101193,#101194,#101195,#101196,#101197,#101198,
#101199,#101200,#101201,#101202,#101203,#101204,#101205,#101206,#101207,
#101208,#101209,#101210,#101211,#101212,#101213,#101214,#101215,#101216,
#101217,#101218,#101219,#101220,#101221,#101222,#101223,#101224,#101225,
#101226,#101227,#101228,#101229,#101230,#101231,#101232,#101233,#101234,
#101235,#101236,#101237,#101238,#101239,#101240,#101241,#101242,#101243,
#101244,#101245,#101246,#101247,#101248,#101249,#101250,#101251,#101252,
#101253,#101254,#101255,#101256,#101257,#101258,#101259,#101260,#101261,
#101262,#101263,#101264,#101265,#101266,#101267,#101268,#101269,#101270,
#101271,#101272,#101273,#101274,#101275,#101276,#101277,#101278,#101279,
#101280,#101281,#101282,#101283,#101284,#101285,#101286,#101287,#101288,
#101289,#101290,#101291,#101292,#101293,#101294,#101295,#101296,#101297,
#101298,#101299,#101300,#101301,#101302,#101303,#101304,#101305,#101306,
#101307,#101308,#101309,#101310,#101311,#101312,#101313,#101314,#101315,
#101316,#101317,#101318,#101319,#101320,#101321,#101322,#101323,#101324,
#101325,#101326,#101327,#101328,#101329,#101330,#101331,#101332,#101333,
#101334,#101335,#101336,#101337,#101338,#101339,#101340,#101341,#101342,
#101343,#101344,#101345,#101346,#101347,#101348,#101349,#101350,#101351,
#101352,#101353,#101354,#101355,#101356,#101357,#101358,#101359,#101360,
#101361,#101362,#101363,#101364,#101365,#101366,#101367,#101368,#101369,
#101370,#101371,#101372,#101373,#101374,#101375,#101376,#101377,#101378,
#101379,#101380,#101381,#101382,#101383,#101384,#101385,#101386,#101387,
#101388,#101389,#101390,#101391,#101392,#101393,#101394),.UNSPECIFIED.,
 .F.,.F.,(4,2,2,2,2,2,2,2,2,2,2,2,2,2,2,2,2,2,2,2,2,2,2,2,2,2,2,2,2,2,2,
2,2,2,2,2,2,2,2,2,2,2,2,2,2,2,2,2,2,2,2,2,2,2,2,2,2,2,2,2,2,2,2,2,2,2,2,
2,2,2,2,2,2,2,2,2,2,2,2,2,2,2,2,2,2,2,2,2,2,2,2,2,2,2,2,2,2,2,2,2,2,2,2,
2,4),(-2.66742167008063,-2.60891629962728,-2.59007761065181,-2.58078442973836,
-2.57864193350201,-2.57741402012589,-2.57633919693135,-2.57495058380529,
-2.57203621224051,-2.54225956113033,-2.49161991202839,-2.48229185293,-2.47774109911341,
-2.47500336193923,-2.47251944209562,-2.47064342803993,-2.46881688570725,
-2.46627520269848,-2.45963485678475,-2.40384585222558,-2.37977416007561,
-2.36894855197089,-2.36670454612067,-2.36545434923538,-2.36438245688096,
-2.36302652716526,-2.36088122886156,-2.34984760239113,-2.29862707678893,
-2.26992251375875,-2.26348948834143,-2.2607809886947,-2.25881940662941,
-2.25702687333504,-2.25416201476092,-2.24727753653619,-2.19421412030655,
-2.16830126967926,-2.15699285514878,-2.15472038412511,-2.15346400766958,
-2.15239273648127,-2.15104512962614,-2.14842384973225,-2.13238492277097,
-2.12706803551359,-2.11250738276455,-2.07961711069569,-2.06305108067805,
-2.05273920819065,-2.04949043734406,-2.04741712571751,-2.04547649193833,
-2.04293543109895,-2.03864073788547,-2.00353429981958,-1.9546488601183,
-1.94485976310371,-1.94268236885225,-1.9414467386515,-1.94037305564743,
-1.93899624853643,-1.93614252076347,-1.91343456440615,-1.87271784828833,
-1.8456797686759,-1.83944824396967,-1.8367739831557,-1.83481840150778,-1.83301825861359,
-1.83011236786878,-1.8229814589106,-1.77424216796041,-1.73505278561684,
-1.73147806347431,-1.72996904168253,-1.72887687551966,-1.72785089206481,
-1.72610769136682,-1.72137469754077,-1.68178582082112,-1.63388987681075,
-1.62749309848966,-1.62479052709872,-1.62282983619091,-1.62103577149068,
-1.61816334999122,-1.61123418574533,-1.55875561383704,-1.53242877602031,
-1.52101504363046,-1.51873640706946,-1.5174786230623,-1.51640744990724,
-1.51506158825751,-1.51244824645225,-1.49656843867832,-1.49069774516136,
-1.44666703398199,-1.42810816110467,-1.41691845656588,-1.41357286214017,
-1.41147833572777,-1.40954560791717,-1.4081797697387),.UNSPECIFIED.);
#995=B_SPLINE_CURVE_WITH_KNOTS('',3,(#101396,#101397,#101398,#101399,#101400,
#101401,#101402,#101403,#101404,#101405,#101406,#101407,#101408,#101409,
#101410,#101411,#101412,#101413,#101414,#101415,#101416,#101417,#101418,
#101419,#101420,#101421,#101422,#101423,#101424,#101425,#101426,#101427,
#101428,#101429,#101430,#101431,#101432,#101433,#101434,#101435,#101436,
#101437,#101438,#101439,#101440,#101441,#101442,#101443,#101444,#101445,
#101446,#101447,#101448,#101449,#101450,#101451,#101452,#101453,#101454,
#101455,#101456,#101457,#101458,#101459,#101460,#101461,#101462,#101463,
#101464,#101465,#101466,#101467,#101468,#101469,#101470,#101471,#101472,
#101473,#101474,#101475,#101476,#101477,#101478,#101479,#101480,#101481,
#101482,#101483,#101484,#101485,#101486,#101487,#101488,#101489,#101490,
#101491,#101492,#101493,#101494,#101495,#101496,#101497,#101498,#101499,
#101500,#101501,#101502,#101503,#101504,#101505,#101506,#101507,#101508,
#101509,#101510,#101511,#101512,#101513,#101514,#101515,#101516,#101517,
#101518,#101519,#101520,#101521,#101522,#101523,#101524,#101525,#101526,
#101527,#101528,#101529,#101530,#101531,#101532,#101533,#101534,#101535,
#101536,#101537,#101538,#101539,#101540,#101541,#101542,#101543,#101544,
#101545,#101546,#101547,#101548,#101549,#101550,#101551,#101552,#101553,
#101554,#101555,#101556,#101557,#101558,#101559,#101560,#101561,#101562,
#101563,#101564,#101565,#101566,#101567,#101568,#101569,#101570,#101571,
#101572,#101573,#101574,#101575,#101576,#101577,#101578,#101579,#101580,
#101581,#101582,#101583,#101584,#101585,#101586,#101587,#101588,#101589,
#101590,#101591,#101592,#101593,#101594,#101595,#101596,#101597,#101598,
#101599,#101600,#101601,#101602,#101603,#101604,#101605,#101606,#101607,
#101608,#101609,#101610,#101611,#101612,#101613,#101614,#101615),
 .UNSPECIFIED.,.F.,.F.,(4,2,2,2,2,2,2,2,2,2,2,2,2,2,2,2,2,2,2,2,2,2,2,2,
2,2,2,2,2,2,2,2,2,2,2,2,2,2,2,2,2,2,2,2,2,2,2,2,2,2,2,2,2,2,2,2,2,2,2,2,
2,2,2,2,2,2,2,2,2,2,2,2,2,2,2,2,2,2,2,2,2,2,2,2,2,2,2,2,2,2,2,2,2,2,2,2,
2,2,2,2,2,2,2,2,2,2,2,2,2,4),(-1.2597140489769,-1.21607211528067,-1.20968821294619,
-1.20718785775925,-1.20537192891124,-1.20342707102829,-1.20081646110999,
-1.19494718699638,-1.17076977582703,-1.12028459477336,-1.11985386727793,
-1.10366642251781,-1.10103934686962,-1.0996903451474,-1.09861880936702,
-1.09736311219612,-1.09509430894122,-1.08385433159205,-1.05820902126195,
-1.00470306390945,-0.997848935069586,-0.994988811669736,-0.993196950575264,
-0.991234264652791,-0.988520852931581,-0.982060034472249,-0.92811745660486,
-0.891912320049524,-0.889057454449225,-0.887680339810928,-0.886606526123829,
-0.885370875058493,-0.883193743168925,-0.873411128174183,-0.824488470402741,
-0.789364897809759,-0.78506947991398,-0.782528126301392,-0.780587336052889,
-0.778513921261863,-0.775265120777778,-0.764954174695253,-0.748392886195722,
-0.715533323037496,-0.701794094173061,-0.694939612471293,-0.69461438418154,
-0.688842051763052,-0.67901965223504,-0.676953893648946,-0.67562233210618,
-0.674551906554244,-0.673282549028711,-0.670950228963651,-0.658540221382086,
-0.602513479399798,-0.590215587091273,-0.575773210169352,-0.572000034767057,
-0.569788814639537,-0.567876739441582,-0.565538064780693,-0.561069247707397,
-0.529402403398003,-0.47805594926497,-0.467142212211925,-0.465004477830096,
-0.463650883099023,-0.462579200846446,-0.46132736876167,-0.459075726460668,
-0.4481227157292,-0.423571979107512,-0.368469533977642,-0.361757421964373,
-0.359204665749231,-0.357375232913841,-0.35543851228173,-0.352877366578463,
-0.347277710026164,-0.299799126900656,-0.280776151537551,-0.269754809606278,
-0.255489406696663,-0.253171642777262,-0.25177886671696,-0.250700886812702,
-0.249489600435585,-0.247463445738442,-0.239553872277646,-0.224727841231445,
-0.194394572833513,-0.183546222816926,-0.153290477246828,-0.149087099863418,
-0.146572705682888,-0.144636451558391,-0.142552127382758,-0.139252874556893,
-0.128491248907085,-0.0984667337296311,-0.0750459545985775,-0.0441238008826357,
-0.0412117068555677,-0.0398236153055869,-0.0387489326831677,-0.0375208947387947,
-0.0362287461449151,-0.0342507474909926,-0.000628701088768321),
 .UNSPECIFIED.);
#996=B_SPLINE_CURVE_WITH_KNOTS('',3,(#101616,#101617,#101618,#101619,#101620,
#101621,#101622,#101623,#101624,#101625,#101626,#101627,#101628,#101629,
#101630,#101631,#101632,#101633),.UNSPECIFIED.,.F.,.F.,(4,2,2,2,2,2,2,2,
4),(-2.66802706317801,-2.63755579499735,-2.6110399285369,-2.60487275085818,
-2.60220945676248,-2.60025563350888,-2.59845271585941,-2.59553254830194,
-2.59354406257328),.UNSPECIFIED.);
#997=B_SPLINE_CURVE_WITH_KNOTS('',3,(#101639,#101640,#101641,#101642,#101643,
#101644,#101645,#101646,#101647,#101648,#101649,#101650,#101651),
 .UNSPECIFIED.,.F.,.F.,(4,3,3,3,4),(151.755345484905,151.823140394205,151.951948597258,
152.078650414044,152.105783788367),.UNSPECIFIED.);
#998=B_SPLINE_CURVE_WITH_KNOTS('',3,(#101652,#101653,#101654,#101655,#101656,
#101657,#101658,#101659,#101660,#101661),.UNSPECIFIED.,.F.,.F.,(4,1,1,1,
1,1,1,4),(152.105783788367,152.821976844167,153.820813294129,154.81964974409,
155.818486194052,156.817322644014,157.816159093976,158.039785877565),
 .UNSPECIFIED.);
#999=B_SPLINE_CURVE_WITH_KNOTS('',3,(#101662,#101663,#101664,#101665,#101666,
#101667,#101668,#101669,#101670,#101671,#101672,#101673,#101674,#101675,
#101676,#101677,#101678,#101679,#101680,#101681,#101682,#101683,#101684,
#101685,#101686,#101687,#101688,#101689,#101690,#101691,#101692,#101693,
#101694,#101695,#101696,#101697,#101698,#101699,#101700,#101701,#101702,
#101703,#101704,#101705,#101706,#101707,#101708,#101709,#101710,#101711,
#101712,#101713,#101714,#101715,#101716,#101717,#101718,#101719,#101720,
#101721,#101722,#101723,#101724,#101725,#101726,#101727,#101728,#101729,
#101730,#101731,#101732,#101733,#101734,#101735,#101736,#101737,#101738,
#101739,#101740,#101741,#101742,#101743,#101744,#101745,#101746,#101747,
#101748,#101749,#101750,#101751,#101752,#101753,#101754,#101755,#101756,
#101757,#101758,#101759,#101760,#101761,#101762,#101763,#101764,#101765,
#101766,#101767,#101768,#101769,#101770,#101771,#101772,#101773,#101774,
#101775,#101776,#101777,#101778,#101779,#101780,#101781,#101782,#101783,
#101784,#101785,#101786,#101787,#101788,#101789,#101790,#101791,#101792,
#101793,#101794,#101795,#101796,#101797,#101798,#101799,#101800,#101801,
#101802,#101803,#101804,#101805,#101806,#101807,#101808,#101809,#101810,
#101811,#101812,#101813,#101814,#101815,#101816,#101817,#101818,#101819,
#101820,#101821,#101822,#101823,#101824,#101825,#101826,#101827,#101828,
#101829,#101830,#101831,#101832,#101833,#101834,#101835,#101836,#101837,
#101838,#101839,#101840,#101841,#101842,#101843,#101844,#101845,#101846,
#101847,#101848,#101849,#101850,#101851,#101852,#101853,#101854,#101855,
#101856,#101857,#101858,#101859,#101860,#101861,#101862,#101863,#101864,
#101865,#101866,#101867,#101868,#101869,#101870,#101871,#101872,#101873,
#101874,#101875,#101876,#101877,#101878,#101879,#101880,#101881,#101882,
#101883,#101884,#101885,#101886,#101887),.UNSPECIFIED.,.F.,.F.,(4,2,2,2,
2,2,2,2,2,2,2,2,2,2,2,2,2,2,2,2,2,2,2,2,2,2,2,2,2,2,2,2,2,2,2,2,2,2,2,2,
2,2,2,2,2,2,2,2,2,2,2,2,2,2,2,2,2,2,2,2,2,2,2,2,2,2,2,2,2,2,2,2,2,2,2,2,
2,2,2,2,2,2,2,2,2,2,2,2,2,2,2,2,2,2,2,2,2,2,2,2,2,2,2,2,2,2,2,2,2,2,2,2,
4),(-2.59354406257328,-2.5883177459959,-2.54291518852348,-2.52278407067703,
-2.50656977869565,-2.49817343625599,-2.49612604437296,-2.49489790920737,
-2.49382291060779,-2.49243409550616,-2.48951938763106,-2.45949266919019,
-2.40820649761714,-2.39936841407381,-2.39296073321018,-2.39025626196916,
-2.38829518038734,-2.386501439532,-2.38363102425653,-2.37671440318338,-2.32405266885479,
-2.29784933746303,-2.2864663988119,-2.2841894000465,-2.28293191795009,-2.28186053829543,
-2.28051386102173,-2.27789755233361,-2.26195311050385,-2.25752854000568,
-2.21497262544489,-2.18434770593607,-2.17990567312237,-2.17757231460419,
-2.17566016954263,-2.1734438994608,-2.16964997745239,-2.15497992752818,
-2.14272828679887,-2.10721337497845,-2.08476765647976,-2.07439129612995,
-2.07217505637237,-2.07093084721443,-2.06985818362316,-2.06849365084788,
-2.06579375923465,-2.04761477729643,-2.02952730104136,-1.99679696032674,
-1.97429645626121,-1.96865064186295,-1.96608062944405,-1.96414220066034,
-1.96231483619869,-1.95977088783293,-1.95311792005538,-1.89741077955412,
-1.87327558196273,-1.86243203046014,-1.8601866357617,-1.85893599134058,
-1.85786392366942,-1.85650803689063,-1.85436329183246,-1.84334283559094,
-1.79204287119749,-1.76337674192956,-1.75694773443749,-1.75423961683647,
-1.75227783631072,-1.75048479485884,-1.74761841346347,-1.74072659576553,
-1.68772942145559,-1.66175876004346,-1.65043472724724,-1.64816105561119,
-1.64690427580808,-1.64583280588096,-1.64448513859455,-1.64186433079932,
-1.62583873355727,-1.62044137963091,-1.60593735479828,-1.57304157782815,
-1.55028497605359,-1.54460438040687,-1.54202787592298,-1.540088338975,-1.53826270866202,
-1.53572562698701,-1.52911697206969,-1.47296714800935,-1.44911802646067,
-1.43835153256407,-1.43611071006738,-1.43486100990112,-1.43378876243328,
-1.43243137819505,-1.42976562024144,-1.4125789269329,-1.36250163812305,
-1.34494617418748,-1.33419200155471,-1.33089295855992,-1.32880829352727,
-1.32687139650913,-1.32431221801367,-1.3187257105899,-1.31130235891606,
-1.29270077583319,-1.25985604642124),.UNSPECIFIED.);
#1000=B_SPLINE_CURVE_WITH_KNOTS('',3,(#101893,#101894,#101895,#101896,#101897,
#101898,#101899,#101900,#101901,#101902,#101903,#101904,#101905,#101906),
 .UNSPECIFIED.,.F.,.F.,(4,2,2,2,2,2,4),(-0.0749180422499143,-0.0725023883060536,
-0.0418724803977279,-0.00539538322887077,-0.00193513678409589,-0.000864203141083117,
-0.000629064338207634),.UNSPECIFIED.);
#1001=B_SPLINE_CURVE_WITH_KNOTS('',3,(#101907,#101908,#101909,#101910,#101911,
#101912,#101913,#101914,#101915,#101916,#101917,#101918,#101919,#101920,
#101921,#101922,#101923,#101924,#101925,#101926,#101927,#101928,#101929,
#101930,#101931,#101932,#101933,#101934,#101935,#101936,#101937,#101938,
#101939,#101940,#101941,#101942,#101943,#101944,#101945,#101946,#101947,
#101948,#101949,#101950,#101951,#101952,#101953,#101954,#101955,#101956,
#101957,#101958,#101959,#101960,#101961,#101962,#101963,#101964,#101965,
#101966,#101967,#101968,#101969,#101970,#101971,#101972,#101973,#101974,
#101975,#101976,#101977,#101978,#101979,#101980,#101981,#101982,#101983,
#101984,#101985,#101986,#101987,#101988,#101989,#101990,#101991,#101992,
#101993,#101994,#101995,#101996,#101997,#101998,#101999,#102000,#102001,
#102002,#102003,#102004,#102005,#102006,#102007,#102008,#102009,#102010,
#102011,#102012,#102013,#102014,#102015,#102016,#102017,#102018,#102019,
#102020,#102021,#102022,#102023,#102024,#102025,#102026,#102027,#102028,
#102029,#102030,#102031,#102032,#102033,#102034,#102035,#102036,#102037,
#102038,#102039,#102040,#102041,#102042,#102043,#102044,#102045,#102046,
#102047,#102048,#102049,#102050,#102051,#102052,#102053,#102054,#102055,
#102056,#102057,#102058,#102059,#102060,#102061,#102062,#102063,#102064,
#102065,#102066,#102067,#102068,#102069,#102070,#102071,#102072,#102073,
#102074,#102075,#102076,#102077,#102078,#102079,#102080,#102081,#102082,
#102083,#102084,#102085,#102086,#102087),.UNSPECIFIED.,.F.,.F.,(4,3,3,3,
3,3,3,3,3,3,3,3,3,3,3,3,3,3,3,3,3,3,3,3,3,3,3,3,3,3,3,3,3,3,3,3,3,3,3,3,
3,3,3,3,3,3,3,3,3,3,3,3,3,3,3,3,3,3,3,3,4),(145.822598481187,145.830121694434,
145.93351643147,146.036757713573,146.139877678953,146.24293224715,146.345955455495,
146.448981298156,146.552114064923,146.655303156321,146.758675149692,146.828958144396,
146.932352881429,147.03559416353,147.138714128907,147.241768697101,147.344791905443,
147.4478177481,147.550950514863,147.654139606258,147.757511599624,147.827794594357,
147.931189331481,148.034430613672,148.13755057914,148.240605147424,148.343628355858,
148.446654198605,148.549786965458,148.652976056941,148.756348050395,148.826631044319,
148.930025781262,149.033267063273,149.136387028562,149.239441596668,149.342464804924,
149.445490647496,149.548623414175,149.651812505487,149.755184498774,149.825467494281,
149.928862231266,150.032103513317,150.135223478643,150.238278046785,150.341301255075,
150.444327097678,150.547459864387,150.650648955727,150.754020949038,150.824303944243,
150.927703487101,151.031158736827,151.134277043374,151.23732809389,151.340345927056,
151.444095816518,151.547200209519,151.651272847212,151.755345484905),
 .UNSPECIFIED.);
#1002=B_SPLINE_CURVE_WITH_KNOTS('',3,(#102089,#102090,#102091,#102092,#102093,
#102094,#102095,#102096,#102097,#102098,#102099,#102100,#102101,#102102,
#102103,#102104,#102105,#102106,#102107,#102108,#102109,#102110,#102111,
#102112,#102113,#102114,#102115,#102116,#102117,#102118,#102119,#102120,
#102121,#102122,#102123,#102124,#102125,#102126,#102127,#102128,#102129,
#102130,#102131,#102132,#102133,#102134,#102135,#102136,#102137,#102138,
#102139,#102140,#102141,#102142,#102143,#102144,#102145,#102146,#102147,
#102148,#102149,#102150,#102151,#102152,#102153,#102154,#102155,#102156,
#102157,#102158,#102159,#102160,#102161,#102162,#102163,#102164,#102165,
#102166,#102167,#102168,#102169,#102170,#102171,#102172,#102173,#102174,
#102175,#102176,#102177,#102178,#102179,#102180,#102181,#102182,#102183,
#102184,#102185,#102186,#102187,#102188,#102189,#102190,#102191,#102192,
#102193,#102194,#102195,#102196,#102197,#102198,#102199,#102200,#102201,
#102202,#102203,#102204,#102205,#102206,#102207,#102208,#102209,#102210,
#102211,#102212,#102213,#102214,#102215,#102216,#102217,#102218,#102219,
#102220,#102221,#102222,#102223,#102224,#102225,#102226,#102227,#102228,
#102229,#102230,#102231,#102232,#102233,#102234,#102235,#102236,#102237,
#102238,#102239,#102240,#102241,#102242,#102243,#102244,#102245,#102246,
#102247,#102248,#102249,#102250,#102251,#102252,#102253,#102254,#102255,
#102256,#102257,#102258,#102259,#102260,#102261,#102262,#102263,#102264,
#102265,#102266,#102267,#102268,#102269,#102270,#102271,#102272,#102273,
#102274,#102275,#102276,#102277,#102278,#102279,#102280,#102281,#102282,
#102283,#102284,#102285,#102286,#102287,#102288,#102289,#102290,#102291,
#102292,#102293,#102294,#102295,#102296,#102297,#102298,#102299,#102300,
#102301,#102302,#102303,#102304,#102305,#102306,#102307,#102308,#102309,
#102310,#102311,#102312),.UNSPECIFIED.,.F.,.F.,(4,2,2,2,2,2,2,2,2,2,2,2,
2,2,2,2,2,2,2,2,2,2,2,2,2,2,2,2,2,2,2,2,2,2,2,2,2,2,2,2,2,2,2,2,2,2,2,2,
2,2,2,2,2,2,2,2,2,2,2,2,2,2,2,2,2,2,2,2,2,2,2,2,2,2,2,2,2,2,2,2,2,2,2,2,
2,2,2,2,2,2,2,2,2,2,2,2,2,2,2,2,2,2,2,2,2,2,2,2,2,2,2,4),(-1.25985604642124,
-1.24997270655081,-1.22734490530893,-1.22449277804107,-1.22311614319518,
-1.22204230805192,-1.22080618535122,-1.21862715035613,-1.20881817752338,
-1.15991368846936,-1.12479503245296,-1.12049941387325,-1.11795791125828,
-1.11601698974665,-1.11394341775658,-1.1106943354787,-1.10038219488761,
-1.08381869971055,-1.05095599984349,-1.03712782878735,-1.03047851317781,
-1.01500486154962,-1.01240780738985,-1.01106532121958,-1.00999424463989,
-1.00873359583445,-1.0064418308268,-0.994795494656133,-0.967530279183534,
-0.947345782328875,-0.912838109771735,-0.908551488846451,-0.906012618841815,
-0.904072156114286,-0.901997567960173,-0.898743744060173,-0.888389920536443,
-0.871734055376915,-0.838795169106305,-0.820071561554565,-0.803158463282142,
-0.800503302317016,-0.799148326421416,-0.798076432464727,-0.796825368133199,
-0.794577651366278,-0.783693129837423,-0.759400920475859,-0.703899354149075,
-0.697224257985395,-0.694677030704228,-0.692848931237895,-0.690911210355583,
-0.688344654060897,-0.682716637051382,-0.675223106583611,-0.656363650866931,
-0.626425247443481,-0.604611365836883,-0.590943342810621,-0.588655218165676,
-0.587271113473261,-0.58619417280993,-0.5849776694788,-0.582886707269278,
-0.574276576288882,-0.557513645220457,-0.515491962883698,-0.488621724276845,
-0.484503802915049,-0.482014415016537,-0.480081929702114,-0.477986219744017,
-0.474635587473701,-0.463399237719763,-0.444734219807898,-0.416475451360396,
-0.379486425232132,-0.37664863960059,-0.37527504939945,-0.374201756843105,
-0.372964184162579,-0.37077760542634,-0.361224605495686,-0.312153218603028,
-0.2769866164246,-0.272691422182474,-0.270150399236703,-0.268209975686894,
-0.266137063319112,-0.262889281065477,-0.252778729953164,-0.236574307317366,
-0.198328832770132,-0.167652335690321,-0.16473994695652,-0.163351838579395,
-0.162277199954153,-0.161049276195866,-0.159757267660685,-0.155110071548611,
-0.128864883473422,-0.106990879666121,-0.105559686826295,-0.0651105010710382,
-0.0603738607572403,-0.0579480734197528,-0.0560290631069845,-0.0538783933845104,
-0.0516516908266748,-0.0483298716554019,-0.000628983746475497),
 .UNSPECIFIED.);
#1003=B_SPLINE_CURVE_WITH_KNOTS('',3,(#102313,#102314,#102315,#102316,#102317,
#102318,#102319,#102320,#102321,#102322,#102323,#102324,#102325,#102326,
#102327,#102328,#102329,#102330,#102331,#102332),.UNSPECIFIED.,.F.,.F.,
(4,2,2,2,2,2,2,2,2,4),(-2.6677002844498,-2.62474750340299,-2.62181352290306,
-2.62013078745661,-2.61862587933799,-2.61753430633498,-2.61650703011106,
-2.6147575335521,-2.60998370547245,-2.59357457362298),.UNSPECIFIED.);
#1004=B_SPLINE_CURVE_WITH_KNOTS('',3,(#102337,#102338,#102339,#102340,#102341,
#102342,#102343,#102344,#102345,#102346,#102347,#102348,#102349,#102350,
#102351,#102352,#102353,#102354,#102355,#102356,#102357,#102358,#102359,
#102360,#102361,#102362,#102363,#102364,#102365,#102366,#102367,#102368,
#102369,#102370,#102371,#102372,#102373,#102374,#102375,#102376,#102377,
#102378,#102379,#102380,#102381,#102382,#102383,#102384,#102385,#102386,
#102387,#102388,#102389,#102390,#102391,#102392,#102393,#102394,#102395,
#102396,#102397,#102398,#102399,#102400,#102401,#102402,#102403,#102404,
#102405,#102406,#102407,#102408,#102409,#102410,#102411,#102412,#102413,
#102414,#102415,#102416,#102417,#102418,#102419,#102420,#102421,#102422,
#102423,#102424,#102425,#102426,#102427,#102428,#102429,#102430,#102431,
#102432,#102433,#102434,#102435,#102436,#102437,#102438,#102439,#102440,
#102441,#102442,#102443,#102444,#102445,#102446,#102447,#102448,#102449,
#102450,#102451,#102452,#102453,#102454,#102455,#102456,#102457,#102458,
#102459,#102460,#102461,#102462,#102463,#102464,#102465,#102466,#102467,
#102468,#102469,#102470,#102471,#102472,#102473,#102474,#102475,#102476,
#102477,#102478,#102479,#102480,#102481,#102482,#102483,#102484,#102485,
#102486,#102487,#102488,#102489,#102490,#102491,#102492,#102493,#102494,
#102495,#102496,#102497,#102498,#102499,#102500,#102501,#102502,#102503,
#102504,#102505,#102506,#102507,#102508,#102509,#102510,#102511,#102512,
#102513,#102514,#102515,#102516,#102517,#102518,#102519,#102520,#102521,
#102522,#102523,#102524,#102525,#102526,#102527,#102528,#102529,#102530,
#102531,#102532,#102533,#102534,#102535,#102536,#102537,#102538,#102539,
#102540,#102541,#102542,#102543,#102544,#102545,#102546,#102547,#102548,
#102549,#102550,#102551,#102552,#102553,#102554,#102555,#102556,#102557,
#102558,#102559,#102560,#102561,#102562,#102563,#102564,#102565,#102566,
#102567,#102568,#102569,#102570,#102571,#102572,#102573,#102574,#102575,
#102576,#102577,#102578,#102579,#102580,#102581,#102582,#102583,#102584,
#102585,#102586,#102587,#102588,#102589,#102590,#102591,#102592,#102593,
#102594,#102595,#102596,#102597,#102598,#102599,#102600,#102601,#102602,
#102603,#102604,#102605,#102606,#102607,#102608,#102609,#102610,#102611,
#102612),.UNSPECIFIED.,.F.,.F.,(4,2,2,2,2,2,2,2,2,2,2,2,2,2,2,2,2,2,2,2,
2,2,2,2,2,2,2,2,2,2,2,2,2,2,2,2,2,2,2,2,2,2,2,2,2,2,2,2,2,2,2,2,2,2,2,2,
2,2,2,2,2,2,2,2,2,2,2,2,2,2,2,2,2,2,2,2,2,2,2,2,2,2,2,2,2,2,2,2,2,2,2,2,
2,2,2,2,2,2,2,2,2,2,2,2,2,2,2,2,2,2,2,2,2,2,2,2,2,2,2,2,2,2,2,2,2,2,2,2,
2,2,2,2,2,2,2,2,2,4),(-1.40847138255639,-1.3930392354306,-1.38269162152927,
-1.37943872755714,-1.37736449411351,-1.3754241966515,-1.3728853042098,-1.36859814330709,
-1.33401722799158,-1.27805194810483,-1.27377815670641,-1.27210659414637,
-1.27109457352481,-1.26999224662054,-1.26842734028213,-1.2645148479626,
-1.24530270466621,-1.18892923953642,-1.17208436580389,-1.16846769201748,
-1.16610361687919,-1.16418983950316,-1.16199770675431,-1.15821144155428,
-1.14196490929422,-1.08449072479498,-1.07951866327211,-1.06353363353854,
-1.06091531845003,-1.05956827875815,-1.0584969630881,-1.05723997029619,
-1.05496490110614,-1.04361367011582,-1.01753130893937,-0.964662362292203,
-0.957759473819122,-0.954891474404148,-0.953098290661852,-0.951137059094502,
-0.94843098289729,-0.942012878206311,-0.913438963293679,-0.862245329411575,
-0.851082848859158,-0.848929609514312,-0.84757123893153,-0.846499133412448,
-0.845250662768653,-0.843014678589856,-0.832321719669709,-0.808736040477737,
-0.752159285249997,-0.745595564561645,-0.743065980024229,-0.741242591967052,
-0.739302522367586,-0.736720317983567,-0.731006604842131,-0.708001687506784,
-0.67497997360631,-0.653842589358095,-0.639425012080224,-0.63710057987157,
-0.635705828219258,-0.634627565781027,-0.633417354671249,-0.631354592976211,
-0.623094255513504,-0.607342371482614,-0.565289505582135,-0.537102827248444,
-0.53295100083903,-0.530451711676749,-0.528517807623457,-0.526426802432169,
-0.523097188102357,-0.512056781766311,-0.493846527510116,-0.444761314335446,
-0.427658145115539,-0.42499619947284,-0.423639888499567,-0.422568039156383,
-0.421318292717594,-0.419076103659263,-0.408279038403085,-0.384309248695111,
-0.328332193337035,-0.321706535653096,-0.319167258421557,-0.317341433266562,
-0.315402965105603,-0.312830046862806,-0.307166203583433,-0.284529959069611,
-0.233320767504336,-0.231007914950522,-0.215553274769492,-0.212979023141689,
-0.211656295505932,-0.210636796956037,-0.210628818843005,-0.210621007703407,
-0.210613353319925,-0.210605846222377,-0.210598477624496,-0.210591239463591,
-0.210584124151352,-0.210577124630462,-0.210570234359993,-0.210563447155905,
-0.210556757387543,-0.210550159574956,-0.210543648645456,-0.210537219814358,
-0.210530868647234,-0.210524590888147,-0.210518382518939,-0.21051223973231,
-0.210506158877642,-0.210500136579285,-0.210494169547824,-0.210488254601243,
-0.210482388855394,-0.210476569495251,-0.209213076515601,-0.206823862893776,
-0.193227817559046,-0.156857914973535,-0.113405658750385,-0.109106791554842,
-0.106564686649097,-0.104624064738684,-0.102551548875404,-0.0993056573426866,
-0.0890165731811178,-0.0749180422499143),.UNSPECIFIED.);
#1005=B_SPLINE_CURVE_WITH_KNOTS('',3,(#102613,#102614,#102615,#102616,#102617,
#102618,#102619,#102620,#102621,#102622,#102623,#102624,#102625,#102626,
#102627,#102628,#102629,#102630,#102631,#102632,#102633,#102634,#102635,
#102636,#102637,#102638,#102639,#102640,#102641,#102642,#102643,#102644,
#102645,#102646,#102647,#102648,#102649,#102650,#102651,#102652,#102653,
#102654,#102655,#102656,#102657,#102658,#102659,#102660,#102661,#102662,
#102663,#102664,#102665,#102666,#102667,#102668,#102669,#102670,#102671,
#102672,#102673,#102674,#102675,#102676,#102677,#102678,#102679,#102680,
#102681,#102682,#102683,#102684,#102685,#102686,#102687,#102688,#102689,
#102690,#102691,#102692,#102693,#102694,#102695,#102696,#102697,#102698,
#102699,#102700,#102701,#102702,#102703,#102704,#102705,#102706,#102707,
#102708,#102709,#102710,#102711,#102712,#102713,#102714,#102715,#102716,
#102717,#102718,#102719,#102720,#102721,#102722,#102723,#102724,#102725,
#102726,#102727,#102728,#102729,#102730,#102731,#102732,#102733,#102734,
#102735,#102736,#102737,#102738,#102739,#102740,#102741,#102742,#102743,
#102744,#102745,#102746,#102747,#102748,#102749,#102750,#102751,#102752,
#102753,#102754,#102755,#102756,#102757,#102758,#102759,#102760,#102761,
#102762,#102763,#102764,#102765,#102766,#102767,#102768,#102769,#102770,
#102771,#102772,#102773,#102774,#102775,#102776,#102777,#102778,#102779,
#102780,#102781,#102782,#102783,#102784,#102785,#102786,#102787,#102788,
#102789,#102790,#102791,#102792,#102793,#102794,#102795,#102796,#102797,
#102798,#102799,#102800,#102801,#102802,#102803,#102804,#102805,#102806,
#102807,#102808,#102809,#102810,#102811,#102812,#102813,#102814,#102815,
#102816,#102817,#102818,#102819,#102820,#102821,#102822,#102823,#102824,
#102825,#102826,#102827,#102828,#102829,#102830,#102831,#102832,#102833,
#102834,#102835,#102836,#102837,#102838,#102839,#102840),.UNSPECIFIED.,
 .F.,.F.,(4,2,2,2,2,2,2,2,2,2,2,2,2,2,2,2,2,2,2,2,2,2,2,2,2,2,2,2,2,2,2,
2,2,2,2,2,2,2,2,2,2,2,2,2,2,2,2,2,2,2,2,2,2,2,2,2,2,2,2,2,2,2,2,2,2,2,2,
2,2,2,2,2,2,2,2,2,2,2,2,2,2,2,2,2,2,2,2,2,2,2,2,2,2,2,2,2,2,2,2,2,2,2,2,
2,2,2,2,2,2,2,2,2,2,4),(-2.59357457362298,-2.5725246031732,-2.55108357278968,
-2.52264233424065,-2.51626160565957,-2.51414626091878,-2.51207239908537,
-2.51013131644929,-2.50758976302121,-2.50329444958505,-2.46820949710224,
-2.41939638744359,-2.40952117414475,-2.40734679825542,-2.40610186369359,
-2.40502908379588,-2.40366506071883,-2.40096818234118,-2.38289149380774,
-2.33711789462775,-2.31735499662168,-2.30961736939984,-2.30390362642351,
-2.30128802836053,-2.29934215798713,-2.29752723212433,-2.29503131691526,
-2.28867505872206,-2.23036968426413,-2.20788111560483,-2.19749175063449,
-2.19527434870366,-2.19402972237077,-2.19295684636823,-2.19159223367025,
-2.1888927643583,-2.17074051284007,-2.12635217434615,-2.09546751996204,
-2.09101781286388,-2.08868261759104,-2.08677008134936,-2.0845546117778,
-2.08076512433499,-2.06614985948285,-2.05388708605766,-2.01348397067698,
-1.99463744705181,-1.98534080099832,-1.98319761890393,-1.98196933060854,
-1.98089419047167,-1.97950518273758,-1.97659003645882,-1.94661749989325,
-1.91158573276047,-1.89278798695755,-1.8814950007506,-1.87813765604313,
-1.87604001256748,-1.8741072788546,-1.87161971118434,-1.86750944454131,
-1.84097071500416,-1.79878882558391,-1.78190106720167,-1.77324686313445,
-1.77115200608305,-1.76993439716414,-1.76885726327654,-1.76747390897173,
-1.76518907996402,-1.75160019849135,-1.74979237495307,-1.70242001914626,
-1.67144482065021,-1.66699281031225,-1.66465718644672,-1.66274469493789,
-1.66052972235876,-1.6567421719414,-1.64214768221655,-1.62988213039964,
-1.58947099502746,-1.57061723898786,-1.56131841981834,-1.55917513564019,
-1.55794685311495,-1.55687175996042,-1.55548286826937,-1.55256816094469,
-1.52373078255813,-1.48561968446398,-1.46809409066987,-1.45735297591777,
-1.4540553000815,-1.45197088747224,-1.4500338026562,-1.44751726833858,-1.44330800783644,
-1.41283336595372,-1.36760785399605,-1.35571528989521,-1.35118019824941,
-1.34787178707464,-1.34640930316602,-1.3453245994328,-1.34413571039383,
-1.34216976275827,-1.33576465163016,-1.33420874407463,-1.31962219983047,
-1.26058066063075,-1.25976514203483),.UNSPECIFIED.);
#1006=B_SPLINE_CURVE_WITH_KNOTS('',3,(#102846,#102847,#102848,#102849,#102850,
#102851,#102852,#102853),.UNSPECIFIED.,.F.,.F.,(4,2,2,4),(-0.0748567535247674,
-0.0732687614006028,-0.0499764445815352,-0.00062947833174663),
 .UNSPECIFIED.);
#1007=B_SPLINE_CURVE_WITH_KNOTS('',3,(#102854,#102855,#102856,#102857,#102858,
#102859,#102860,#102861,#102862,#102863,#102864,#102865,#102866,#102867,
#102868,#102869,#102870,#102871,#102872,#102873,#102874,#102875,#102876,
#102877,#102878,#102879,#102880,#102881,#102882,#102883,#102884,#102885,
#102886,#102887,#102888,#102889,#102890,#102891,#102892,#102893,#102894,
#102895,#102896,#102897,#102898,#102899,#102900,#102901,#102902,#102903,
#102904,#102905,#102906,#102907,#102908,#102909,#102910,#102911,#102912,
#102913,#102914,#102915,#102916,#102917,#102918,#102919,#102920,#102921,
#102922,#102923,#102924,#102925,#102926,#102927,#102928,#102929,#102930,
#102931,#102932,#102933,#102934,#102935,#102936,#102937,#102938,#102939,
#102940,#102941,#102942,#102943,#102944,#102945,#102946,#102947,#102948,
#102949,#102950,#102951,#102952,#102953,#102954,#102955,#102956,#102957,
#102958,#102959,#102960,#102961,#102962,#102963,#102964,#102965,#102966,
#102967,#102968,#102969,#102970,#102971,#102972,#102973,#102974,#102975,
#102976,#102977,#102978,#102979,#102980,#102981,#102982,#102983,#102984,
#102985,#102986,#102987,#102988,#102989,#102990,#102991,#102992,#102993,
#102994,#102995,#102996,#102997,#102998,#102999,#103000,#103001,#103002,
#103003,#103004,#103005,#103006,#103007,#103008,#103009,#103010,#103011,
#103012,#103013,#103014,#103015,#103016,#103017,#103018,#103019,#103020,
#103021,#103022,#103023,#103024,#103025,#103026,#103027,#103028,#103029,
#103030,#103031,#103032,#103033,#103034,#103035,#103036,#103037,#103038,
#103039,#103040,#103041,#103042,#103043,#103044,#103045,#103046,#103047,
#103048,#103049,#103050,#103051,#103052,#103053,#103054,#103055,#103056,
#103057,#103058,#103059,#103060,#103061,#103062,#103063,#103064,#103065,
#103066,#103067,#103068,#103069,#103070,#103071,#103072,#103073,#103074,
#103075,#103076,#103077,#103078,#103079,#103080,#103081,#103082,#103083,
#103084,#103085,#103086,#103087,#103088,#103089,#103090,#103091,#103092,
#103093,#103094,#103095,#103096,#103097,#103098,#103099,#103100,#103101,
#103102,#103103,#103104,#103105,#103106,#103107,#103108,#103109,#103110,
#103111),.UNSPECIFIED.,.F.,.F.,(4,2,2,2,2,2,2,2,2,2,2,2,2,2,2,2,2,2,2,2,
2,2,2,2,2,2,2,2,2,2,2,2,2,2,2,2,2,2,2,2,2,2,2,2,2,2,2,2,2,2,2,2,2,2,2,2,
2,2,2,2,2,2,2,2,2,2,2,2,2,2,2,2,2,2,2,2,2,2,2,2,2,2,2,2,2,2,2,2,2,2,2,2,
2,2,2,2,2,2,2,2,2,2,2,2,2,2,2,2,2,2,2,2,2,2,2,2,2,2,2,2,2,2,2,2,2,2,2,2,
4),(-2.66781222492019,-2.66001838762793,-2.6547219431894,-2.65227856128054,
-2.65039670419209,-2.64855599431708,-2.64672958842394,-2.64418919325558,
-2.63899802022748,-2.62648778430856,-2.57481848753383,-2.55597610161522,
-2.54668119359671,-2.54453832547705,-2.5433102031511,-2.54223519917316,
-2.54084635531448,-2.53793151047647,-2.50823512364153,-2.45778623830298,
-2.44829727953654,-2.44369003448626,-2.43991096150434,-2.43774027301652,
-2.43772457867808,-2.43770833179418,-2.43769151228051,-2.43767409920081,
-2.43765607096917,-2.43763740524581,-2.43761807882281,-2.43759806759226,
-2.43757734664654,-2.43755589023898,-2.43753367159252,-2.43751066235144,
-2.43749062627382,-2.43746727622944,-2.43744007012691,-2.4374083799564,
-2.43737147940545,-2.43732853023764,-2.43727431906842,-2.43533361120814,
-2.43279161819176,-2.42849347585957,-2.39337252264298,-2.34441469832562,
-2.33471462311872,-2.33254340900183,-2.33130917572928,-2.33023535387445,
-2.32885659612426,-2.32599271201286,-2.29003732511163,-2.25727199776668,
-2.23471252911173,-2.22905913989001,-2.22648797558917,-2.22454961251538,
-2.22272299680303,-2.22018119330167,-2.21354042279847,-2.15773544341966,
-2.13367372059929,-2.12285065304746,-2.1206067486876,-2.11935654883769,
-2.11828462458865,-2.11692861431965,-2.11478310271424,-2.10374657939899,
-2.05252997599714,-2.02382110510827,-2.01738747719566,-2.01467883356504,
-2.01271718730132,-2.01092462299219,-2.00805977523021,-2.00117563801035,
-1.94810072624431,-1.92219395636758,-1.9108869405113,-1.90861449989724,
-1.90735810663759,-1.90628678781813,-1.90493908338821,-1.90231753500915,
-1.88627571696096,-1.88098515593715,-1.86640073972647,-1.83350915867338,
-1.81694245916113,-1.80663015251884,-1.80338122656909,-1.80130781087837,
-1.79936707591627,-1.79682587686432,-1.79253093632626,-1.7574192793556,
-1.70851520795402,-1.69874469197343,-1.69656848733368,-1.6953330785133,
-1.69425929790861,-1.69288198420773,-1.69002589122103,-1.66722643173411,
-1.61161804068732,-1.59560669677266,-1.59183726382131,-1.58964881155249,
-1.58773462514935,-1.58536536578613,-1.58173203162915,-1.56463510149431,
-1.55656647867173,-1.52175631463101,-1.49770679491481,-1.486887272655,-1.48464367581751,
-1.4833935873754,-1.48232172169696,-1.48096573811559,-1.47830548185271,
-1.46125216265378,-1.44264026103571,-1.40968433184212,-1.40847138255639),
 .UNSPECIFIED.);
#1008=B_SPLINE_CURVE_WITH_KNOTS('',3,(#103113,#103114,#103115,#103116,#103117,
#103118,#103119,#103120,#103121,#103122,#103123,#103124,#103125,#103126,
#103127,#103128,#103129,#103130,#103131,#103132,#103133,#103134,#103135,
#103136,#103137,#103138,#103139,#103140,#103141,#103142,#103143,#103144,
#103145,#103146,#103147,#103148,#103149,#103150,#103151,#103152,#103153,
#103154,#103155,#103156,#103157,#103158,#103159,#103160,#103161,#103162,
#103163,#103164,#103165,#103166,#103167,#103168,#103169,#103170,#103171,
#103172,#103173,#103174,#103175,#103176,#103177,#103178,#103179,#103180,
#103181,#103182,#103183,#103184,#103185,#103186,#103187,#103188,#103189,
#103190,#103191,#103192,#103193,#103194,#103195,#103196,#103197,#103198,
#103199,#103200,#103201,#103202,#103203,#103204,#103205,#103206,#103207,
#103208,#103209,#103210,#103211,#103212,#103213,#103214,#103215,#103216,
#103217,#103218,#103219,#103220,#103221,#103222,#103223,#103224,#103225,
#103226,#103227,#103228,#103229,#103230,#103231,#103232,#103233,#103234,
#103235,#103236,#103237,#103238,#103239,#103240,#103241,#103242,#103243,
#103244,#103245,#103246,#103247,#103248,#103249,#103250,#103251,#103252,
#103253,#103254,#103255,#103256,#103257,#103258,#103259,#103260,#103261,
#103262,#103263,#103264,#103265,#103266,#103267,#103268,#103269,#103270,
#103271,#103272,#103273,#103274,#103275,#103276,#103277,#103278,#103279,
#103280,#103281,#103282,#103283,#103284,#103285,#103286,#103287,#103288,
#103289,#103290,#103291,#103292,#103293,#103294,#103295,#103296,#103297,
#103298,#103299,#103300,#103301,#103302,#103303,#103304,#103305,#103306,
#103307,#103308,#103309,#103310,#103311,#103312,#103313,#103314,#103315,
#103316,#103317,#103318,#103319,#103320,#103321,#103322),.UNSPECIFIED.,
 .F.,.F.,(4,2,2,2,2,2,2,2,2,2,2,2,2,2,2,2,2,2,2,2,2,2,2,2,2,2,2,2,2,2,2,
2,2,2,2,2,2,2,2,2,2,2,2,2,2,2,2,2,2,2,2,2,2,2,2,2,2,2,2,2,2,2,2,2,2,2,2,
2,2,2,2,2,2,2,2,2,2,2,2,2,2,2,2,2,2,2,2,2,2,2,2,2,2,2,2,2,2,2,2,2,2,2,2,
2,4),(-1.25976514203483,-1.24627096371811,-1.24250927652393,-1.24030044353385,
-1.23838778851667,-1.23604506193199,-1.2315581355053,-1.19919642732524,
-1.15901287546397,-1.154080862944,-1.13813164183323,-1.13551512195141,-1.13416841297433,
-1.1330970481481,-1.13183963557149,-1.12956288498489,-1.11818426966118,
-1.09199516951617,-1.03927233402488,-1.03235781358755,-1.02948777677141,
-1.02769413151857,-1.02573304724538,-1.0230283682676,-1.01661921625226,
-0.988122027355997,-0.937199033953814,-0.92570732222101,-0.923534283368015,
-0.92216983946654,-0.921097179097549,-0.919852904953113,-0.917636368444082,
-0.907255775161229,-0.884792459204342,-0.826429150771745,-0.820076724627021,
-0.817581759295738,-0.815767332801416,-0.813821817771153,-0.811206375776999,
-0.805309368346198,-0.780917436221713,-0.730252743974468,-0.714075036808931,
-0.71144853251101,-0.710099726687497,-0.709028290787664,-0.70777264416632,
-0.705503785067525,-0.694260549833938,-0.668601107664333,-0.615122712521193,
-0.608267228794461,-0.605407019377386,-0.603615243533792,-0.601652763109141,
-0.598939841635263,-0.592481172117712,-0.538597461479476,-0.502336141671931,
-0.499483271458002,-0.498106611474066,-0.497032913624168,-0.495797126220781,
-0.493619106870349,-0.483821762615518,-0.434915951358219,-0.399786429157354,
-0.395498805114655,-0.392959812225597,-0.39101952733057,-0.388945393145167,
-0.385692833110238,-0.375347705471159,-0.358710291130442,-0.325789163427632,
-0.307660674855151,-0.290153697049808,-0.287477078436241,-0.286117619946777,
-0.285045511777135,-0.283798019624447,-0.281566221948021,-0.2709389051044,
-0.247590817162665,-0.191922910262866,-0.184490884349839,-0.181533970338131,
-0.179724538613804,-0.177895292514631,-0.175385725401274,-0.170037645275231,
-0.162927961360404,-0.145450036545872,-0.0958298182879772,-0.0781715427825538,
-0.0754897006043806,-0.0741291637744639,-0.0730570135908618,-0.0718103986139602,
-0.0695824611675837,-0.0590160995158885,-0.0358876316419884,-0.000629543614865904),
 .UNSPECIFIED.);
#1009=B_SPLINE_CURVE_WITH_KNOTS('',3,(#103323,#103324,#103325,#103326,#103327,
#103328,#103329,#103330,#103331,#103332,#103333,#103334,#103335,#103336,
#103337,#103338,#103339,#103340,#103341,#103342,#103343,#103344),
 .UNSPECIFIED.,.F.,.F.,(4,2,2,2,2,2,2,2,2,2,4),(-2.66754968025911,-2.64222557872969,
-2.63909886152637,-2.6369529653842,-2.63515231182392,-2.6332385260983,-2.63086956528686,
-2.62723631926054,-2.6101324181504,-2.59794289122828,-2.59313490574478),
 .UNSPECIFIED.);
#1010=B_SPLINE_CURVE_WITH_KNOTS('',3,(#103349,#103350,#103351,#103352,#103353,
#103354,#103355,#103356,#103357,#103358,#103359,#103360,#103361,#103362,
#103363,#103364,#103365,#103366,#103367,#103368,#103369,#103370,#103371,
#103372,#103373,#103374,#103375,#103376,#103377,#103378,#103379,#103380,
#103381,#103382,#103383,#103384,#103385,#103386,#103387,#103388,#103389,
#103390,#103391,#103392,#103393,#103394,#103395,#103396,#103397,#103398,
#103399,#103400,#103401,#103402,#103403,#103404,#103405,#103406,#103407,
#103408,#103409,#103410,#103411,#103412,#103413,#103414,#103415,#103416,
#103417,#103418,#103419,#103420,#103421,#103422,#103423,#103424,#103425,
#103426,#103427,#103428,#103429,#103430,#103431,#103432,#103433,#103434,
#103435,#103436,#103437,#103438,#103439,#103440,#103441,#103442,#103443,
#103444,#103445,#103446,#103447,#103448,#103449,#103450,#103451,#103452,
#103453,#103454,#103455,#103456,#103457,#103458,#103459,#103460,#103461,
#103462,#103463,#103464,#103465,#103466,#103467,#103468,#103469,#103470,
#103471,#103472,#103473,#103474,#103475,#103476,#103477,#103478,#103479,
#103480,#103481,#103482,#103483,#103484,#103485,#103486,#103487,#103488,
#103489,#103490,#103491,#103492,#103493,#103494,#103495,#103496,#103497,
#103498,#103499,#103500,#103501,#103502,#103503,#103504,#103505,#103506,
#103507,#103508,#103509,#103510,#103511,#103512,#103513,#103514,#103515,
#103516,#103517,#103518,#103519,#103520,#103521,#103522,#103523,#103524,
#103525,#103526,#103527,#103528,#103529,#103530,#103531,#103532,#103533,
#103534,#103535,#103536,#103537,#103538,#103539,#103540,#103541,#103542,
#103543,#103544,#103545,#103546,#103547,#103548,#103549,#103550,#103551,
#103552,#103553,#103554,#103555,#103556,#103557,#103558,#103559,#103560,
#103561,#103562,#103563,#103564,#103565,#103566,#103567,#103568,#103569,
#103570,#103571,#103572,#103573,#103574,#103575,#103576,#103577,#103578,
#103579,#103580,#103581,#103582,#103583,#103584,#103585,#103586,#103587,
#103588,#103589,#103590),.UNSPECIFIED.,.F.,.F.,(4,2,2,2,2,2,2,2,2,2,2,2,
2,2,2,2,2,2,2,2,2,2,2,2,2,2,2,2,2,2,2,2,2,2,2,2,2,2,2,2,2,2,2,2,2,2,2,2,
2,2,2,2,2,2,2,2,2,2,2,2,2,2,2,2,2,2,2,2,2,2,2,2,2,2,2,2,2,2,2,2,2,2,2,2,
2,2,2,2,2,2,2,2,2,2,2,2,2,2,2,2,2,2,2,2,2,2,2,2,2,2,2,2,2,2,2,2,2,2,2,2,
4),(-1.40835436178516,-1.40120748467684,-1.37505305271072,-1.36368250096922,
-1.36140621418413,-1.36014888904888,-1.35907749999195,-1.35773062880308,
-1.35511340876948,-1.33915136590534,-1.33420734953041,-1.32856139629404,
-1.28160143233727,-1.28015780613655,-1.26111694966373,-1.25735565670909,
-1.25494685966479,-1.25302909761683,-1.25086691763213,-1.24721719786922,
-1.2327660419842,-1.1823778016643,-1.15270966940492,-1.14979517135514,-1.14840640334139,
-1.14733141310644,-1.14610326547807,-1.14396024280758,-1.13466326363675,
-1.11581174254254,-1.07535841393395,-1.06307969665175,-1.04849987361659,
-1.0447138919679,-1.0424994337114,-1.04058714143595,-1.03825145285354,-1.03379836669918,
-1.00276226937868,-0.954784645856903,-0.940195549477655,-0.937863185595314,
-0.936465945171996,-0.935387147829541,-0.934177885721391,-0.932120170614113,
-0.923924762041621,-0.908358607240402,-0.866775225235952,-0.854638989158886,
-0.836943366883324,-0.833270679930094,-0.830889086290468,-0.82897367800387,
-0.826793330569765,-0.823061595502939,-0.807565125555238,-0.755635584891186,
-0.728680061603705,-0.725778524655203,-0.724392241475761,-0.723317470188229,
-0.722087662996888,-0.719937259692629,-0.710538472974241,-0.661283210068209,
-0.626056494999795,-0.621759540475693,-0.619217674914547,-0.617276722352837,
-0.615203355791732,-0.611955093503761,-0.601649752815576,-0.585101169720129,
-0.552251199323677,-0.539685406155158,-0.516623260530808,-0.513766768776718,
-0.512389378818381,-0.511315589921085,-0.510080237757896,-0.50790427768254,
-0.498137604845868,-0.449204626363468,-0.414080325033906,-0.409784352877915,
-0.407242910031934,-0.405302189042837,-0.403228981430708,-0.399980783576168,
-0.389674092098935,-0.373121861408414,-0.340270899400875,-0.327215628598037,
-0.318559273272307,-0.304219898924665,-0.301897168864333,-0.300502890290625,
-0.29942465718587,-0.298214103100781,-0.296149922239845,-0.287872932045477,
-0.272073958306711,-0.226218489024688,-0.201664173317549,-0.197636537294232,
-0.195173837035319,-0.193301738838713,-0.191274958300659,-0.188089451327945,
-0.184342526667239,-0.177228317181495,-0.159734752796449,-0.110014209964816,
-0.0924687521570684,-0.0897907578290559,-0.0884310004100348,-0.0873588619835297,
-0.0861115701772213,-0.0838807143168502,-0.0748567535247674),
 .UNSPECIFIED.);
#1011=B_SPLINE_CURVE_WITH_KNOTS('',3,(#103591,#103592,#103593,#103594,#103595,
#103596,#103597,#103598,#103599,#103600,#103601,#103602,#103603,#103604,
#103605,#103606,#103607,#103608,#103609,#103610,#103611,#103612,#103613,
#103614,#103615,#103616,#103617,#103618,#103619,#103620,#103621,#103622,
#103623,#103624,#103625,#103626,#103627,#103628,#103629,#103630,#103631,
#103632,#103633,#103634,#103635,#103636,#103637,#103638,#103639,#103640,
#103641,#103642,#103643,#103644,#103645,#103646,#103647,#103648,#103649,
#103650,#103651,#103652,#103653,#103654,#103655,#103656,#103657,#103658,
#103659,#103660,#103661,#103662,#103663,#103664,#103665,#103666,#103667,
#103668,#103669,#103670,#103671,#103672,#103673,#103674,#103675,#103676,
#103677,#103678,#103679,#103680,#103681,#103682,#103683,#103684,#103685,
#103686,#103687,#103688,#103689,#103690,#103691,#103692,#103693,#103694,
#103695,#103696,#103697,#103698,#103699,#103700,#103701,#103702,#103703,
#103704,#103705,#103706,#103707,#103708,#103709,#103710,#103711,#103712,
#103713,#103714,#103715,#103716,#103717,#103718,#103719,#103720,#103721,
#103722,#103723,#103724,#103725,#103726,#103727,#103728,#103729,#103730,
#103731,#103732,#103733,#103734,#103735,#103736,#103737,#103738,#103739,
#103740,#103741,#103742,#103743,#103744,#103745,#103746,#103747,#103748,
#103749,#103750,#103751,#103752,#103753,#103754,#103755,#103756,#103757,
#103758,#103759,#103760,#103761,#103762,#103763,#103764,#103765,#103766,
#103767,#103768,#103769,#103770,#103771,#103772,#103773,#103774,#103775,
#103776,#103777,#103778,#103779,#103780,#103781,#103782,#103783,#103784,
#103785,#103786,#103787,#103788,#103789,#103790,#103791,#103792,#103793,
#103794,#103795,#103796,#103797,#103798,#103799,#103800,#103801,#103802,
#103803,#103804,#103805,#103806,#103807,#103808,#103809,#103810,#103811,
#103812,#103813,#103814,#103815,#103816,#103817,#103818,#103819,#103820,
#103821,#103822,#103823,#103824,#103825,#103826,#103827,#103828,#103829,
#103830,#103831,#103832,#103833,#103834,#103835,#103836,#103837,#103838,
#103839,#103840,#103841,#103842,#103843,#103844,#103845,#103846,#103847,
#103848,#103849,#103850,#103851,#103852,#103853,#103854,#103855,#103856,
#103857,#103858,#103859,#103860,#103861,#103862,#103863,#103864,#103865,
#103866),.UNSPECIFIED.,.F.,.F.,(4,2,2,2,2,2,2,2,2,2,2,2,2,2,2,2,2,2,2,2,
2,2,2,2,2,2,2,2,2,2,2,2,2,2,2,2,2,2,2,2,2,2,2,2,2,2,2,2,2,2,2,2,2,2,2,2,
2,2,2,2,2,2,2,2,2,2,2,2,2,2,2,2,2,2,2,2,2,2,2,2,2,2,2,2,2,2,2,2,2,2,2,2,
2,2,2,2,2,2,2,2,2,2,2,2,2,2,2,2,2,2,2,2,2,2,2,2,2,2,2,2,2,2,2,2,2,2,2,2,
2,2,2,2,2,2,2,2,2,4),(-2.59313490574478,-2.55330326801384,-2.53483436151909,
-2.5310022515763,-2.52945059810669,-2.52835100895761,-2.5273363692964,-2.52565012427039,
-2.5212842676782,-2.47357798675594,-2.44429013327263,-2.43427814598053,
-2.42949034686026,-2.42559713121777,-2.42339376444406,-2.4233810955763,
-2.42336798932302,-2.42335442953436,-2.42334039932334,-2.42332587818603,
-2.42331084945732,-2.42329529574739,-2.42327919728274,-2.42326253346499,
-2.42324528285917,-2.42322742314613,-2.4232089310934,-2.42318978253747,
-2.42316995227465,-2.42314941408245,-2.42312814067539,-2.42310610361413,
-2.42308327274177,-2.4230639674276,-2.42304141425639,-2.42301506360632,
-2.42298427229399,-2.4229482878032,-2.42290622989389,-2.42285835310031,
-2.42091785871573,-2.41837621358731,-2.41407881259393,-2.37897334829359,
-2.33005825774277,-2.32031470827636,-2.31814066016904,-2.31690588134865,
-2.31583226771662,-2.31445467047015,-2.3115962759417,-2.28868622423929,
-2.24625632528545,-2.22764346886388,-2.21643091968091,-2.21308300383397,
-2.21098802371109,-2.20905555419177,-2.20656527006203,-2.20244391464848,
-2.17517766963749,-2.13299297660313,-2.11667461410578,-2.10821630695699,
-2.10613757097069,-2.10492385879532,-2.10384647192153,-2.10245800952345,
-2.10015481594809,-2.08617274881369,-2.06460740532472,-2.03153810979631,
-2.00850110350888,-2.00278363856421,-2.00020085510439,-1.99826080213208,
-1.99643776369501,-1.99390919727569,-1.98735113380447,-1.93076194716973,
-1.92829418114678,-1.90662743707945,-1.89647520864303,-1.89427366515673,
-1.89303278485856,-1.89195989220095,-1.89059104857492,-1.88840315495372,
-1.87670414775936,-1.87292085431342,-1.87268894626612,-1.86582352375722,
-1.85209117875077,-1.81921046424644,-1.80265569122254,-1.79234891954575,
-1.78910073227713,-1.78702754643769,-1.78508685692137,-1.78254547251614,
-1.77824966985943,-1.74305700781315,-1.69388887139729,-1.68442985126656,
-1.68227541001777,-1.68104482881162,-1.67997038184518,-1.67858582312859,
-1.67569248729687,-1.64965970583749,-1.61149463659113,-1.58246829861086,
-1.57807293184966,-1.57574948913394,-1.57383798981261,-1.57161399045446,
-1.56778594831757,-1.55272544856017,-1.50055993324135,-1.48171540162278,
-1.47242008047358,-1.47027730174263,-1.46904926040354,-1.46797434672869,
-1.46658564515949,-1.46367118942575,-1.43362669393912,-1.38228786957019,
-1.36894840986627,-1.36539355974845,-1.36325252177946,-1.36133134399441,
-1.35888814619682,-1.35501380153761,-1.33394078482172,-1.27612802698394,
-1.26116802669047,-1.25973369591908),.UNSPECIFIED.);
#1012=B_SPLINE_CURVE_WITH_KNOTS('',3,(#103872,#103873,#103874,#103875),
 .UNSPECIFIED.,.F.,.F.,(4,4),(120.339865682355,120.689851223097),
 .UNSPECIFIED.);
#1013=B_SPLINE_CURVE_WITH_KNOTS('',3,(#103876,#103877,#103878,#103879,#103880,
#103881,#103882,#103883,#103884,#103885,#103886,#103887,#103888,#103889,
#103890,#103891,#103892,#103893,#103894,#103895,#103896,#103897,#103898,
#103899,#103900,#103901,#103902,#103903,#103904,#103905,#103906,#103907,
#103908,#103909,#103910,#103911,#103912,#103913,#103914,#103915,#103916,
#103917,#103918,#103919,#103920,#103921,#103922,#103923,#103924,#103925,
#103926,#103927,#103928,#103929,#103930,#103931,#103932,#103933,#103934,
#103935,#103936,#103937,#103938,#103939,#103940,#103941,#103942,#103943,
#103944,#103945,#103946,#103947,#103948,#103949,#103950,#103951,#103952,
#103953,#103954,#103955,#103956,#103957,#103958,#103959,#103960,#103961,
#103962,#103963,#103964,#103965,#103966,#103967,#103968,#103969,#103970,
#103971,#103972,#103973,#103974,#103975,#103976,#103977,#103978,#103979,
#103980,#103981,#103982,#103983,#103984,#103985,#103986,#103987,#103988,
#103989,#103990,#103991,#103992,#103993,#103994,#103995,#103996,#103997,
#103998,#103999,#104000,#104001,#104002,#104003,#104004,#104005,#104006,
#104007,#104008,#104009,#104010,#104011,#104012,#104013,#104014,#104015,
#104016,#104017,#104018,#104019,#104020,#104021,#104022,#104023,#104024,
#104025,#104026,#104027,#104028,#104029,#104030,#104031,#104032,#104033,
#104034,#104035,#104036,#104037,#104038,#104039,#104040,#104041,#104042,
#104043,#104044,#104045,#104046,#104047,#104048,#104049,#104050,#104051,
#104052,#104053,#104054,#104055,#104056,#104057,#104058,#104059,#104060,
#104061,#104062,#104063,#104064,#104065,#104066,#104067,#104068,#104069,
#104070,#104071,#104072,#104073,#104074,#104075,#104076,#104077,#104078,
#104079,#104080,#104081,#104082,#104083,#104084,#104085,#104086,#104087,
#104088,#104089,#104090,#104091,#104092,#104093,#104094,#104095,#104096,
#104097,#104098,#104099,#104100,#104101),.UNSPECIFIED.,.F.,.F.,(4,2,2,2,
2,2,2,2,2,2,2,2,2,2,2,2,2,2,2,2,2,2,2,2,2,2,2,2,2,2,2,2,2,2,2,2,2,2,2,2,
2,2,2,2,2,2,2,2,2,2,2,2,2,2,2,2,2,2,2,2,2,2,2,2,2,2,2,2,2,2,2,2,2,2,2,2,
2,2,2,2,2,2,2,2,2,2,2,2,2,2,2,2,2,2,2,2,2,2,2,2,2,2,2,2,2,2,2,2,2,2,2,2,
4),(-2.66740566330074,-2.64317490644518,-2.6360437625599,-2.63425319807585,
-2.63303838589649,-2.63202935526164,-2.63095478054007,-2.62956857342768,
-2.62666658944157,-2.59961424602175,-2.58553293708982,-2.57351180775184,
-2.54173365275992,-2.53137908523418,-2.52812536151031,-2.52605092363122,
-2.5241106625936,-2.52157214574642,-2.51728635270582,-2.4742491908246,-2.4442673431881,
-2.43065638899947,-2.42319719800404,-2.42121047786026,-2.42019242067258,
-2.41912216435068,-2.41779427060571,-2.41574038253585,-2.40608495751117,
-2.35237118375876,-2.32446089926702,-2.31812322367221,-2.31543091159095,
-2.31347226465107,-2.31167633345679,-2.30879273699945,-2.30179452432377,
-2.25037547417588,-2.22330082846914,-2.21170131424476,-2.20941238508367,
-2.20815244410715,-2.20708145943003,-2.20573843689133,-2.20313844977164,
-2.18759175364158,-2.18102885537958,-2.16576374521916,-2.13787313177137,
-2.11898267497714,-2.11148113981519,-2.10584872664639,-2.10328136176684,
-2.10134352073457,-2.09951567304948,-2.09696938430387,-2.09030024854694,
-2.03477063489238,-2.01052540492794,-1.99965279600475,-1.99740583410008,
-1.9961549379745,-1.99508303698877,-1.99372785132462,-1.9910716819442,-1.97413313727524,
-1.92386907190346,-1.90627531601881,-1.89550485253889,-1.89220441116883,
-1.89011969471492,-1.88818332415432,-1.88566913169197,-1.88146689783177,
-1.85126644148712,-1.79974163337377,-1.78775102877288,-1.78544061349278,
-1.78417595451377,-1.78310520348447,-1.78176782989071,-1.77968325112593,
-1.76959123584787,-1.76409915483254,-1.75667234239292,-1.743164826707,-1.71028301970526,
-1.69372929311369,-1.6834227056449,-1.68017432770869,-1.6781009603903,-1.67616005899206,
-1.67361833651232,-1.66932182652777,-1.6341046684402,-1.58485956810295,
-1.57548192421687,-1.57333313068167,-1.57210371676431,-1.57102895166417,
-1.56964222130379,-1.56739549579956,-1.5545624869472,-1.55239653151165,
-1.50511597875543,-1.47659174138898,-1.47017975600638,-1.46747456192548,
-1.46551335433549,-1.46371977252385,-1.46085020964095,-1.45393873571281,
-1.40835436178516),.UNSPECIFIED.);
#1014=B_SPLINE_CURVE_WITH_KNOTS('',3,(#104103,#104104,#104105,#104106,#104107,
#104108,#104109,#104110,#104111,#104112,#104113,#104114,#104115,#104116,
#104117,#104118,#104119,#104120,#104121,#104122,#104123,#104124,#104125,
#104126,#104127,#104128,#104129,#104130,#104131,#104132,#104133,#104134,
#104135,#104136,#104137,#104138,#104139,#104140,#104141,#104142,#104143,
#104144,#104145,#104146,#104147,#104148,#104149,#104150,#104151,#104152,
#104153,#104154,#104155,#104156,#104157,#104158,#104159,#104160,#104161,
#104162,#104163,#104164,#104165,#104166,#104167,#104168,#104169,#104170,
#104171,#104172,#104173,#104174,#104175,#104176,#104177,#104178,#104179,
#104180,#104181,#104182,#104183,#104184,#104185,#104186,#104187,#104188,
#104189,#104190,#104191,#104192,#104193,#104194,#104195,#104196,#104197,
#104198,#104199,#104200,#104201,#104202,#104203,#104204,#104205,#104206,
#104207,#104208,#104209,#104210,#104211,#104212,#104213,#104214,#104215,
#104216,#104217,#104218,#104219,#104220,#104221,#104222,#104223,#104224,
#104225,#104226,#104227,#104228,#104229,#104230,#104231,#104232,#104233,
#104234,#104235,#104236,#104237,#104238,#104239,#104240,#104241,#104242,
#104243,#104244,#104245,#104246,#104247,#104248,#104249,#104250,#104251,
#104252,#104253,#104254,#104255,#104256,#104257,#104258,#104259,#104260,
#104261,#104262,#104263,#104264,#104265,#104266,#104267,#104268,#104269,
#104270,#104271,#104272,#104273,#104274,#104275,#104276,#104277,#104278,
#104279,#104280,#104281,#104282,#104283,#104284,#104285,#104286,#104287,
#104288,#104289,#104290,#104291,#104292,#104293,#104294,#104295,#104296,
#104297,#104298,#104299,#104300,#104301,#104302,#104303,#104304,#104305,
#104306,#104307,#104308,#104309,#104310,#104311,#104312,#104313,#104314,
#104315,#104316,#104317,#104318,#104319,#104320,#104321,#104322,#104323,
#104324,#104325,#104326),.UNSPECIFIED.,.F.,.F.,(4,2,2,2,2,2,2,2,2,2,2,2,
2,2,2,2,2,2,2,2,2,2,2,2,2,2,2,2,2,2,2,2,2,2,2,2,2,2,2,2,2,2,2,2,2,2,2,2,
2,2,2,2,2,2,2,2,2,2,2,2,2,2,2,2,2,2,2,2,2,2,2,2,2,2,2,2,2,2,2,2,2,2,2,2,
2,2,2,2,2,2,2,2,2,2,2,2,2,2,2,2,2,2,2,2,2,2,2,2,2,2,2,4),(-1.25973369591908,
-1.25882010703106,-1.25741836646077,-1.25633902654265,-1.25513241539184,
-1.25308637675045,-1.245029277895,-1.22985063334681,-1.18995584899926,-1.15891311792271,
-1.1546917298589,-1.15217188560428,-1.1502345426746,-1.14815210177199,-1.14486232251316,
-1.13418906717786,-1.11681833999807,-1.06811645470584,-1.06160140353263,
-1.04897950432908,-1.04674387314019,-1.04536050660888,-1.04428612108112,
-1.04305464910848,-1.04089636336231,-1.03138450553894,-0.982233088275675,
-0.947038879444556,-0.942742708123222,-0.940201192925525,-0.938260442868806,
-0.936187229586887,-0.932939075835942,-0.922632970759417,-0.906082106209736,
-0.87323206225543,-0.860314571933824,-0.837612583026447,-0.834759141645184,
-0.833382428324641,-0.832308793433493,-0.831073196598608,-0.828895795913767,
-0.819105929104722,-0.770197943800586,-0.735082318584062,-0.730787583347391,
-0.728246622193727,-0.726306125035958,-0.724233016917092,-0.720984683435521,
-0.710675104521929,-0.694115899984244,-0.661260969463728,-0.647487449350561,
-0.640719713392962,-0.639092290674091,-0.625191559062593,-0.62289233454933,
-0.62150503156868,-0.620427782873463,-0.619213382334404,-0.617131555436607,
-0.608634898562339,-0.592203006413606,-0.550103306052869,-0.522875939161712,
-0.518749332543588,-0.516257521915162,-0.51432483506572,-0.512230585132612,
-0.508885930337426,-0.497703828023856,-0.479164576426568,-0.43498853085022,
-0.41369061059898,-0.410873471058813,-0.409504015921035,-0.408431166335568,
-0.407190937311453,-0.404991997310929,-0.394877399544114,-0.373335899106141,
-0.363128768521085,-0.314935732240373,-0.307784427807797,-0.304875456329372,
-0.30307499276735,-0.301120321420233,-0.298449562819577,-0.292236469553449,
-0.26534659046944,-0.226490563733547,-0.201853293048104,-0.198976728268952,
-0.197595613296098,-0.19656687565604,-0.195375402799059,-0.193400822351896,
-0.190973660742924,-0.186051016465701,-0.172643559365281,-0.151527626500562,
-0.102990334553856,-0.0958517578786078,-0.0929449766948306,-0.0911449588602478,
-0.0891900531518719,-0.0865176815474027,-0.0802949449086537,-0.0533261439010829,
-0.000629601453589488),.UNSPECIFIED.);
#1015=B_SPLINE_CURVE_WITH_KNOTS('',3,(#104327,#104328,#104329,#104330,#104331,
#104332,#104333,#104334,#104335,#104336,#104337,#104338,#104339,#104340,
#104341,#104342,#104343,#104344,#104345,#104346,#104347,#104348,#104349,
#104350),.UNSPECIFIED.,.F.,.F.,(4,2,2,2,2,2,2,2,2,2,2,4),(-2.66819246569389,
-2.66013468457772,-2.65577695930745,-2.65436379664703,-2.65329641581407,
-2.6522660819304,-2.651086027011,-2.6491605796328,-2.64309431029485,-2.64181214569972,
-2.63401080610002,-2.59392646598523),.UNSPECIFIED.);
#1016=B_SPLINE_CURVE_WITH_KNOTS('',3,(#104356,#104357,#104358,#104359,#104360,
#104361,#104362,#104363,#104364,#104365,#104366,#104367,#104368),
 .UNSPECIFIED.,.F.,.F.,(4,3,3,3,4),(114.057240443604,114.163813834894,114.270250535392,
114.376547448128,114.406671945289),.UNSPECIFIED.);
#1017=B_SPLINE_CURVE_WITH_KNOTS('',3,(#104369,#104370,#104371,#104372,#104373,
#104374,#104375,#104376,#104377,#104378),.UNSPECIFIED.,.F.,.F.,(4,1,1,1,
1,1,1,4),(114.406674973168,114.866191745616,115.865028195577,116.863864645539,
117.862701095501,118.861537545463,119.860373995425,120.339865682355),
 .UNSPECIFIED.);
#1018=B_SPLINE_CURVE_WITH_KNOTS('',3,(#104379,#104380,#104381,#104382,#104383,
#104384,#104385,#104386,#104387,#104388,#104389,#104390,#104391,#104392,
#104393,#104394,#104395,#104396,#104397,#104398,#104399,#104400,#104401,
#104402,#104403,#104404,#104405,#104406,#104407,#104408,#104409,#104410,
#104411,#104412,#104413,#104414,#104415,#104416,#104417,#104418,#104419,
#104420,#104421,#104422,#104423,#104424,#104425,#104426,#104427,#104428,
#104429,#104430,#104431,#104432,#104433,#104434,#104435,#104436,#104437,
#104438,#104439,#104440,#104441,#104442,#104443,#104444,#104445,#104446,
#104447,#104448,#104449,#104450,#104451,#104452,#104453,#104454,#104455,
#104456,#104457,#104458,#104459,#104460,#104461,#104462,#104463,#104464,
#104465,#104466,#104467,#104468,#104469,#104470,#104471,#104472,#104473,
#104474,#104475,#104476,#104477,#104478,#104479,#104480,#104481,#104482,
#104483,#104484,#104485,#104486,#104487,#104488,#104489,#104490,#104491,
#104492,#104493,#104494,#104495,#104496,#104497,#104498,#104499,#104500,
#104501,#104502,#104503,#104504,#104505,#104506,#104507,#104508,#104509,
#104510,#104511,#104512,#104513,#104514,#104515,#104516,#104517,#104518,
#104519,#104520,#104521,#104522,#104523,#104524,#104525,#104526,#104527,
#104528,#104529,#104530,#104531,#104532,#104533,#104534,#104535,#104536,
#104537,#104538,#104539,#104540,#104541,#104542,#104543,#104544,#104545,
#104546,#104547,#104548,#104549,#104550,#104551,#104552,#104553,#104554,
#104555,#104556,#104557,#104558,#104559,#104560,#104561,#104562,#104563,
#104564,#104565,#104566,#104567,#104568,#104569,#104570,#104571,#104572,
#104573,#104574,#104575,#104576,#104577,#104578,#104579,#104580,#104581,
#104582,#104583,#104584,#104585,#104586,#104587,#104588,#104589,#104590,
#104591,#104592,#104593,#104594,#104595,#104596,#104597,#104598,#104599,
#104600,#104601,#104602,#104603,#104604,#104605,#104606,#104607,#104608,
#104609,#104610,#104611,#104612,#104613,#104614,#104615,#104616,#104617,
#104618,#104619,#104620,#104621,#104622,#104623,#104624,#104625,#104626,
#104627,#104628,#104629,#104630,#104631,#104632,#104633,#104634,#104635,
#104636,#104637,#104638,#104639,#104640,#104641,#104642,#104643,#104644),
 .UNSPECIFIED.,.F.,.F.,(4,2,2,2,2,2,2,2,2,2,2,2,2,2,2,2,2,2,2,2,2,2,2,2,
2,2,2,2,2,2,2,2,2,2,2,2,2,2,2,2,2,2,2,2,2,2,2,2,2,2,2,2,2,2,2,2,2,2,2,2,
2,2,2,2,2,2,2,2,2,2,2,2,2,2,2,2,2,2,2,2,2,2,2,2,2,2,2,2,2,2,2,2,2,2,2,2,
2,2,2,2,2,2,2,2,2,2,2,2,2,2,2,2,2,2,2,2,2,2,2,2,2,2,2,2,2,2,2,2,2,2,2,2,
4),(-2.59392646598523,-2.58066502555958,-2.56300901345937,-2.5522099013361,
-2.54890542051214,-2.54681924632914,-2.54488227583739,-2.54236837323655,
-2.5381689719236,-2.50879236248568,-2.46759283265409,-2.45213649756508,
-2.44671689522576,-2.44411614220636,-2.44200814993706,-2.44079506757119,
-2.44079195659206,-2.44078882665356,-2.44078567760298,-2.44078250933715,
-2.44077932176747,-2.44077611469552,-2.44077288804981,-2.44076964168511,
-2.44076637548386,-2.44076308927576,-2.4407597829211,-2.44075645626122,
-2.44075312209097,-2.44074977343357,-2.44074640360696,-2.44074301250016,
-2.44073958889878,-2.43971148371076,-2.43833172623461,-2.43546361523069,
-2.39998403574502,-2.36704576945719,-2.34422233712747,-2.3385327789589,
-2.33595465332513,-2.33401488516542,-2.33218976179598,-2.32965454379678,
-2.32305751480103,-2.2667982738266,-2.24302124160745,-2.23227440562075,
-2.23003480513183,-2.22878538166568,-2.22771312142934,-2.22635539967584,
-2.22420476539108,-2.21309029939523,-2.1618232717555,-2.13321419439624,
-2.12679182067121,-2.12408473194876,-2.12212305523122,-2.12032966709056,
-2.11746177027316,-2.11056132915635,-2.05766974361515,-2.03162195559925,
-2.02027804318085,-2.01800314045304,-2.0167460504074,-2.01567454060791,
-2.01432710904692,-2.01170759989892,-1.99570618493379,-1.99020645925097,
-1.97577391529199,-1.94287710523563,-1.92630900304767,-1.91599546283168,
-1.91274595649969,-1.91067212434943,-1.90873096721912,-1.90618916869418,
-1.90189311034052,-1.86675840593335,-1.81779579351645,-1.80808008488306,
-1.80590731934123,-1.80467250585235,-1.80359837273467,-1.8022194686122,
-1.79935615455937,-1.76334935722691,-1.73058682285606,-1.70804069402824,
-1.7023882896687,-1.69981682302094,-1.69787792662867,-1.69605058389674,
-1.69350740843637,-1.68686090440254,-1.63107000103531,-1.59817517576441,
-1.59462811060725,-1.59312359316423,-1.59203199788474,-1.59100445649406,
-1.58925398277654,-1.58447447185232,-1.54730070324189,-1.49702116171413,
-1.49061825743434,-1.48791429555067,-1.48595303431212,-1.48415875065031,
-1.48128664121933,-1.47436166830793,-1.421787532311,-1.39551110069199,-1.38410882121919,
-1.38183041999204,-1.38057249260765,-1.3795009329836,-1.37815428305887,
-1.37553877115204,-1.35961660813774,-1.35511411290143,-1.33454900263241,
-1.28619023022274,-1.27904054767369,-1.27613103133974,-1.27432986351377,
-1.27237413797995,-1.26970141794458,-1.26348138904713,-1.26001305103131),
 .UNSPECIFIED.);
#1019=B_SPLINE_CURVE_WITH_KNOTS('',3,(#104650,#104651,#104652,#104653,#104654,
#104655,#104656,#104657,#104658,#104659,#104660,#104661,#104662,#104663,
#104664,#104665,#104666,#104667,#104668,#104669),.UNSPECIFIED.,.F.,.F.,
(4,2,2,2,2,2,2,2,2,4),(-0.0747504621130409,-0.0610229394801576,-0.0562870045128616,
-0.054543581138797,-0.0535177052337252,-0.0524257925231619,-0.0509174394464196,
-0.0492296206923426,-0.0462824100167693,-0.000629119177008705),
 .UNSPECIFIED.);
#1020=B_SPLINE_CURVE_WITH_KNOTS('',3,(#104670,#104671,#104672,#104673,#104674,
#104675,#104676,#104677,#104678,#104679,#104680,#104681,#104682,#104683,
#104684,#104685,#104686,#104687,#104688,#104689,#104690,#104691,#104692,
#104693,#104694,#104695,#104696,#104697,#104698,#104699,#104700,#104701,
#104702,#104703,#104704,#104705,#104706,#104707,#104708,#104709,#104710,
#104711,#104712,#104713,#104714,#104715,#104716,#104717,#104718,#104719,
#104720,#104721,#104722,#104723,#104724,#104725,#104726,#104727,#104728,
#104729,#104730,#104731,#104732,#104733,#104734,#104735,#104736,#104737,
#104738,#104739,#104740,#104741,#104742,#104743,#104744,#104745,#104746,
#104747,#104748,#104749,#104750,#104751,#104752,#104753,#104754,#104755,
#104756,#104757,#104758,#104759,#104760,#104761,#104762,#104763,#104764,
#104765,#104766,#104767,#104768,#104769,#104770,#104771,#104772,#104773,
#104774,#104775,#104776,#104777,#104778,#104779,#104780,#104781,#104782,
#104783,#104784,#104785,#104786,#104787,#104788,#104789,#104790,#104791,
#104792,#104793,#104794,#104795,#104796,#104797,#104798,#104799,#104800,
#104801,#104802,#104803,#104804,#104805,#104806,#104807,#104808,#104809,
#104810,#104811,#104812,#104813,#104814,#104815,#104816,#104817,#104818,
#104819,#104820,#104821,#104822,#104823,#104824,#104825,#104826,#104827,
#104828,#104829,#104830,#104831,#104832,#104833,#104834,#104835,#104836,
#104837,#104838,#104839,#104840,#104841,#104842,#104843,#104844,#104845,
#104846,#104847,#104848,#104849,#104850),.UNSPECIFIED.,.F.,.F.,(4,3,3,3,
3,3,3,3,3,3,3,3,3,3,3,3,3,3,3,3,3,3,3,3,3,3,3,3,3,3,3,3,3,3,3,3,3,3,3,3,
3,3,3,3,3,3,3,3,3,3,3,3,3,3,3,3,3,3,3,3,4),(108.12348663811,108.225421296431,
108.327291076165,108.429131491865,108.530978014042,108.632930880403,108.734945943836,
108.837130903885,108.873173045844,108.976567782892,109.079809065007,109.1829290304,
109.285983598609,109.389006806967,109.492032649639,109.595165416417,109.698354507827,
109.801726501209,109.872009495806,109.975404232854,110.078645514969,110.181765480362,
110.28482004857,110.387843256928,110.490869099601,110.594001866379,110.697190957789,
110.800562951171,110.870845945768,110.974240682816,111.077481964931,111.180601930323,
111.283656498532,111.38667970689,111.489705549562,111.59283831634,111.69602740775,
111.799399401132,111.86968239573,111.973077132778,112.076318414893,112.179438380285,
112.282492948494,112.385516156852,112.488541999524,112.591674766303,112.694863857712,
112.798235851094,112.868518845692,112.97191358274,113.075154864855,113.178274830248,
113.281329398457,113.384352606815,113.487378449487,113.590511216265,113.693700307675,
113.797072301057,113.867355295654,113.974272639368,114.057240443604),
 .UNSPECIFIED.);
#1021=B_SPLINE_CURVE_WITH_KNOTS('',3,(#104852,#104853,#104854,#104855,#104856,
#104857,#104858,#104859,#104860,#104861,#104862,#104863,#104864,#104865,
#104866,#104867,#104868,#104869,#104870,#104871,#104872,#104873,#104874,
#104875,#104876,#104877,#104878,#104879,#104880,#104881,#104882,#104883,
#104884,#104885,#104886,#104887,#104888,#104889,#104890,#104891,#104892,
#104893,#104894,#104895,#104896,#104897,#104898,#104899,#104900,#104901,
#104902,#104903,#104904,#104905,#104906,#104907,#104908,#104909,#104910,
#104911,#104912,#104913,#104914,#104915,#104916,#104917,#104918,#104919,
#104920,#104921,#104922,#104923,#104924,#104925,#104926,#104927,#104928,
#104929,#104930,#104931,#104932,#104933,#104934,#104935,#104936,#104937,
#104938,#104939,#104940,#104941,#104942,#104943,#104944,#104945,#104946,
#104947,#104948,#104949,#104950,#104951,#104952,#104953,#104954,#104955,
#104956,#104957,#104958,#104959,#104960,#104961,#104962,#104963,#104964,
#104965,#104966,#104967,#104968,#104969,#104970,#104971,#104972,#104973,
#104974,#104975,#104976,#104977,#104978,#104979,#104980,#104981,#104982,
#104983,#104984,#104985,#104986,#104987,#104988,#104989,#104990,#104991,
#104992,#104993,#104994,#104995,#104996,#104997,#104998,#104999,#105000,
#105001,#105002,#105003,#105004,#105005,#105006,#105007,#105008,#105009,
#105010,#105011,#105012,#105013,#105014,#105015,#105016,#105017,#105018,
#105019,#105020,#105021,#105022,#105023,#105024,#105025,#105026,#105027,
#105028,#105029,#105030,#105031,#105032,#105033,#105034,#105035,#105036,
#105037,#105038,#105039,#105040,#105041,#105042,#105043,#105044,#105045,
#105046,#105047,#105048,#105049,#105050,#105051,#105052,#105053,#105054,
#105055,#105056,#105057,#105058,#105059,#105060,#105061,#105062,#105063,
#105064,#105065,#105066,#105067),.UNSPECIFIED.,.F.,.F.,(4,2,2,2,2,2,2,2,
2,2,2,2,2,2,2,2,2,2,2,2,2,2,2,2,2,2,2,2,2,2,2,2,2,2,2,2,2,2,2,2,2,2,2,2,
2,2,2,2,2,2,2,2,2,2,2,2,2,2,2,2,2,2,2,2,2,2,2,2,2,2,2,2,2,2,2,2,2,2,2,2,
2,2,2,2,2,2,2,2,2,2,2,2,2,2,2,2,2,2,2,2,2,2,2,2,2,2,2,4),(-1.26001305103131,
-1.236546528138,-1.19601723368554,-1.17302338979252,-1.17016774612471,-1.1687903357867,
-1.16771632918863,-1.1664804986667,-1.16430315072426,-1.15452122247037,
-1.10558802777883,-1.0704579529701,-1.06616178556445,-1.06361998936534,
-1.06167886157342,-1.05960508658686,-1.05635572252675,-1.0460429935662,
-1.02947884433227,-0.996613617850608,-0.982869511029417,-0.976019436372951,
-0.97570881818813,-0.970189105870943,-0.960125838630565,-0.958043063190949,
-0.956706143309467,-0.955635277538568,-0.954369928227707,-0.952056799877416,
-0.940020236017337,-0.888050633906243,-0.858275267555108,-0.854081820408176,
-0.851570075538851,-0.849633932071001,-0.847547823011974,-0.844241681169512,
-0.8334212373689,-0.815716956570843,-0.765142043162348,-0.748688316661077,
-0.746050663149659,-0.744699388111575,-0.74362769297481,-0.742373709538034,
-0.740112823948655,-0.729008814736019,-0.703888241194228,-0.649614579223858,
-0.642824912843948,-0.639975427925457,-0.638185470213055,-0.636221016593174,
-0.633498051885379,-0.626980395416872,-0.597568275097048,-0.547613731328803,
-0.536213183438616,-0.534045464982643,-0.532682628984102,-0.531610088504744,
-0.530364645439957,-0.528142810196855,-0.517678996270604,-0.494920901946999,
-0.437029625182237,-0.430618952160738,-0.428114251199299,-0.426297280064509,
-0.424353285136179,-0.421747270802334,-0.41590291347179,-0.391914313035495,
-0.342043705642979,-0.32466688567579,-0.321994678619817,-0.320636069225288,
-0.31956391413444,-0.318315545180878,-0.316080138974597,-0.305397394370176,
-0.28184949767725,-0.225205284497385,-0.218651621412212,-0.215899096865799,
-0.21395697617716,-0.212008337317596,-0.21003265608343,-0.204809495390636,
-0.197989211077535,-0.181524624333188,-0.14874670231778,-0.112915186594562,
-0.110056468619816,-0.108678728269664,-0.107605005720207,-0.106370113057628,
-0.104195878191195,-0.094452065454749,-0.0455058292351705,-0.0267279147051765,
-0.018764008653592,-0.00802108915905755,-0.00466632909900502,-0.00258130056107843,
-0.00128118359696819,-0.000628940766197544),.UNSPECIFIED.);
#1022=B_SPLINE_CURVE_WITH_KNOTS('',3,(#105068,#105069,#105070,#105071,#105072,
#105073,#105074,#105075,#105076,#105077,#105078,#105079,#105080),
 .UNSPECIFIED.,.F.,.F.,(4,3,3,3,4),(-104.372003947921,-104.263735348745,
-104.155311094227,-104.046631225742,-104.02252548323),.UNSPECIFIED.);
#1023=B_SPLINE_CURVE_WITH_KNOTS('',3,(#105085,#105086,#105087,#105088,#105089,
#105090,#105091,#105092,#105093,#105094,#105095,#105096,#105097,#105098,
#105099,#105100,#105101,#105102,#105103,#105104,#105105,#105106,#105107,
#105108,#105109,#105110,#105111,#105112,#105113,#105114,#105115,#105116,
#105117,#105118,#105119,#105120,#105121,#105122,#105123,#105124,#105125,
#105126,#105127,#105128,#105129,#105130,#105131,#105132,#105133,#105134,
#105135,#105136,#105137,#105138,#105139,#105140,#105141,#105142,#105143,
#105144,#105145,#105146,#105147,#105148,#105149,#105150,#105151,#105152,
#105153,#105154,#105155,#105156,#105157,#105158,#105159,#105160,#105161,
#105162,#105163,#105164,#105165,#105166,#105167,#105168,#105169,#105170,
#105171,#105172,#105173,#105174,#105175,#105176,#105177,#105178,#105179,
#105180,#105181,#105182,#105183,#105184,#105185,#105186,#105187,#105188,
#105189,#105190,#105191,#105192,#105193,#105194,#105195,#105196,#105197,
#105198,#105199,#105200,#105201,#105202,#105203,#105204,#105205,#105206,
#105207,#105208,#105209,#105210,#105211,#105212,#105213,#105214,#105215,
#105216,#105217,#105218,#105219,#105220,#105221,#105222,#105223,#105224,
#105225,#105226,#105227,#105228,#105229,#105230,#105231,#105232,#105233,
#105234,#105235,#105236,#105237,#105238,#105239,#105240,#105241,#105242,
#105243,#105244,#105245,#105246,#105247,#105248,#105249,#105250,#105251,
#105252,#105253,#105254,#105255,#105256,#105257,#105258,#105259,#105260,
#105261,#105262,#105263,#105264,#105265,#105266,#105267,#105268,#105269,
#105270,#105271,#105272,#105273,#105274,#105275,#105276,#105277,#105278,
#105279,#105280,#105281,#105282,#105283,#105284,#105285,#105286,#105287,
#105288,#105289,#105290,#105291,#105292,#105293,#105294,#105295,#105296,
#105297,#105298,#105299,#105300,#105301,#105302,#105303,#105304),
 .UNSPECIFIED.,.F.,.F.,(4,2,2,2,2,2,2,2,2,2,2,2,2,2,2,2,2,2,2,2,2,2,2,2,
2,2,2,2,2,2,2,2,2,2,2,2,2,2,2,2,2,2,2,2,2,2,2,2,2,2,2,2,2,2,2,2,2,2,2,2,
2,2,2,2,2,2,2,2,2,2,2,2,2,2,2,2,2,2,2,2,2,2,2,2,2,2,2,2,2,2,2,2,2,2,2,2,
2,2,2,2,2,2,2,2,2,2,2,2,2,4),(-1.40835486065175,-1.37307255299345,-1.33396207864897,
-1.33297748426174,-1.32826979514078,-1.32653032040276,-1.32550499424266,
-1.32441216338815,-1.32290008987306,-1.31930843874777,-1.28016662750195,
-1.231343669678,-1.22421240551894,-1.22130614945658,-1.21950571100321,-1.21754975931901,
-1.21487489659208,-1.20864151528037,-1.18159595652532,-1.14086971316094,
-1.11820870358814,-1.11535575851077,-1.11397896091013,-1.11290510797361,
-1.11166908812003,-1.1094905298683,-1.09968861468525,-1.05077804374086,
-1.01565733058686,-1.0113616749969,-1.00882015837761,-1.00687923071736,
-1.00480565656637,-1.00155658010668,-0.991244535586352,-0.974681268546033,
-0.941818709324578,-0.928012119514121,-0.921312903073065,-0.90586503211797,
-0.903497117398427,-0.902089535649802,-0.901009379508387,-0.899805930223189,
-0.89777412752424,-0.889883895692131,-0.875166680607255,-0.846103611921341,
-0.803698157867828,-0.799404688363424,-0.796863862447183,-0.79492311507512,
-0.792849396808795,-0.78959939123828,-0.779278464535908,-0.762695283424875,
-0.72981705058985,-0.714520484150677,-0.709793773457523,-0.693941561266164,
-0.691328748893703,-0.689982891873249,-0.688911647907598,-0.687653730774862,
-0.685374419137727,-0.673948877877966,-0.647572472915313,-0.595122291163116,
-0.58818879175417,-0.585315747503484,-0.583521640547718,-0.581561188059488,
-0.578859459016999,-0.572467089056242,-0.526046822988734,-0.484947942418818,
-0.480263095535808,-0.478527315143957,-0.477502864635007,-0.476409860217495,
-0.474895738211797,-0.471290870983224,-0.432949505047567,-0.383317401821813,
-0.376221669184502,-0.373321738335967,-0.371522744055547,-0.36956640256799,
-0.366887471566432,-0.360806609691591,-0.352445821237174,-0.301551441055394,
-0.270313241009477,-0.267401273969782,-0.266013097090093,-0.264938281360049,
-0.263710016435639,-0.26156604738355,-0.252414963132737,-0.203666416644472,
-0.167704289861289,-0.162982355971044,-0.160559557536596,-0.158640676069439,
-0.156487802200587,-0.154258046820985,-0.146612093912555,-0.121083043579651,
-0.100337615416932,-0.0747504621130409),.UNSPECIFIED.);
#1024=B_SPLINE_CURVE_WITH_KNOTS('',3,(#105306,#105307,#105308,#105309,#105310,
#105311,#105312,#105313,#105314,#105315,#105316,#105317,#105318,#105319,
#105320,#105321,#105322,#105323,#105324,#105325,#105326,#105327,#105328,
#105329,#105330,#105331,#105332,#105333,#105334,#105335,#105336,#105337,
#105338,#105339,#105340,#105341,#105342,#105343,#105344,#105345,#105346,
#105347,#105348,#105349,#105350,#105351,#105352,#105353,#105354,#105355,
#105356,#105357,#105358,#105359,#105360,#105361,#105362,#105363,#105364,
#105365,#105366,#105367,#105368,#105369,#105370,#105371,#105372,#105373,
#105374,#105375,#105376,#105377,#105378,#105379,#105380,#105381,#105382,
#105383,#105384,#105385,#105386,#105387,#105388,#105389,#105390,#105391,
#105392,#105393,#105394,#105395,#105396,#105397,#105398,#105399,#105400,
#105401,#105402,#105403,#105404,#105405,#105406,#105407,#105408,#105409,
#105410,#105411,#105412,#105413,#105414,#105415,#105416,#105417,#105418,
#105419,#105420,#105421,#105422,#105423,#105424,#105425,#105426,#105427,
#105428,#105429,#105430,#105431,#105432,#105433,#105434,#105435,#105436,
#105437,#105438,#105439,#105440,#105441,#105442,#105443,#105444,#105445,
#105446,#105447,#105448,#105449,#105450,#105451,#105452,#105453,#105454,
#105455,#105456,#105457,#105458,#105459,#105460,#105461,#105462,#105463,
#105464,#105465,#105466,#105467,#105468,#105469,#105470,#105471,#105472,
#105473,#105474,#105475,#105476,#105477,#105478,#105479,#105480,#105481,
#105482,#105483,#105484,#105485,#105486),.UNSPECIFIED.,.F.,.F.,(4,3,3,3,
3,3,3,3,3,3,3,3,3,3,3,3,3,3,3,3,3,3,3,3,3,3,3,3,3,3,3,3,3,3,3,3,3,3,3,3,
3,3,3,3,3,3,3,3,3,3,3,3,3,3,3,3,3,3,3,3,4),(-104.02252548323,-103.91351434008,
-103.878990796035,-103.775596058987,-103.672354776872,-103.569234811479,
-103.46618024327,-103.363157034913,-103.26013119224,-103.156998425462,-103.053809334052,
-102.95043734067,-102.880154346073,-102.776759609025,-102.67351832691,-102.570398361518,
-102.467343793309,-102.364320584951,-102.261294742278,-102.1581619755,-102.05497288409,
-101.951600890709,-101.881317896111,-101.777923159063,-101.674681876948,
-101.571561911556,-101.468507343347,-101.365484134989,-101.262458292316,
-101.159325525538,-101.056136434129,-100.952764440747,-100.882481446149,
-100.779086709101,-100.675845426986,-100.572725461594,-100.469670893385,
-100.366647685027,-100.263621842355,-100.160489075577,-100.057299984167,
-99.9539279907855,-99.8836449961874,-99.7802502591395,-99.6770089770246,
-99.5738890116323,-99.4708344434234,-99.3678112350657,-99.2647853923932,
-99.1616526256152,-99.0584635342055,-98.9550915408238,-98.8848085462255,
-98.7829332776307,-98.681193284401,-98.5795525376358,-98.4779751499171,
-98.3763829554481,-98.2747883682232,-98.173080529173,-98.088818832803),
 .UNSPECIFIED.);
#1025=B_SPLINE_CURVE_WITH_KNOTS('',3,(#105487,#105488,#105489,#105490,#105491),
 .UNSPECIFIED.,.F.,.F.,(4,1,4),(-98.0888186411165,-97.8859720962637,-97.7379483482805),
 .UNSPECIFIED.);
#1026=B_SPLINE_CURVE_WITH_KNOTS('',3,(#105497,#105498,#105499,#105500,#105501,
#105502,#105503,#105504,#105505,#105506,#105507,#105508,#105509,#105510,
#105511,#105512,#105513,#105514,#105515,#105516,#105517,#105518),
 .UNSPECIFIED.,.F.,.F.,(4,2,2,2,2,2,2,2,2,2,4),(-0.0750516936837853,-0.0634020284095776,
-0.0604358780118531,-0.0436144741885916,-0.039999552682271,-0.0376361154365763,
-0.0357225173379457,-0.0339209980332159,-0.0317709111716201,-0.028634281768215,
-0.00062847532083142),.UNSPECIFIED.);
#1027=B_SPLINE_CURVE_WITH_KNOTS('',3,(#105519,#105520,#105521,#105522,#105523,
#105524,#105525,#105526,#105527,#105528,#105529,#105530,#105531,#105532,
#105533,#105534,#105535,#105536,#105537,#105538,#105539,#105540,#105541,
#105542,#105543,#105544,#105545,#105546,#105547,#105548,#105549,#105550,
#105551,#105552,#105553,#105554,#105555,#105556,#105557,#105558,#105559,
#105560,#105561,#105562,#105563,#105564,#105565,#105566,#105567,#105568,
#105569,#105570,#105571,#105572,#105573,#105574,#105575,#105576,#105577,
#105578,#105579,#105580,#105581,#105582,#105583,#105584,#105585,#105586,
#105587,#105588,#105589,#105590,#105591,#105592,#105593,#105594,#105595,
#105596,#105597,#105598,#105599,#105600,#105601,#105602,#105603,#105604,
#105605,#105606,#105607,#105608,#105609,#105610,#105611,#105612,#105613,
#105614,#105615,#105616,#105617,#105618,#105619,#105620,#105621,#105622,
#105623,#105624,#105625,#105626,#105627,#105628,#105629,#105630,#105631,
#105632,#105633,#105634,#105635,#105636,#105637,#105638,#105639,#105640,
#105641,#105642,#105643,#105644,#105645,#105646,#105647,#105648,#105649,
#105650,#105651,#105652,#105653,#105654,#105655,#105656,#105657,#105658,
#105659,#105660,#105661,#105662,#105663,#105664,#105665,#105666,#105667,
#105668,#105669,#105670,#105671,#105672,#105673,#105674,#105675,#105676,
#105677,#105678,#105679,#105680,#105681,#105682,#105683,#105684,#105685,
#105686,#105687,#105688,#105689,#105690,#105691,#105692,#105693,#105694,
#105695,#105696,#105697,#105698,#105699,#105700,#105701,#105702,#105703,
#105704,#105705,#105706,#105707,#105708,#105709,#105710,#105711,#105712,
#105713,#105714,#105715,#105716,#105717,#105718,#105719,#105720,#105721,
#105722,#105723,#105724,#105725,#105726,#105727,#105728,#105729,#105730,
#105731,#105732,#105733,#105734,#105735,#105736),.UNSPECIFIED.,.F.,.F.,
(4,2,2,2,2,2,2,2,2,2,2,2,2,2,2,2,2,2,2,2,2,2,2,2,2,2,2,2,2,2,2,2,2,2,2,
2,2,2,2,2,2,2,2,2,2,2,2,2,2,2,2,2,2,2,2,2,2,2,2,2,2,2,2,2,2,2,2,2,2,2,2,
2,2,2,2,2,2,2,2,2,2,2,2,2,2,2,2,2,2,2,2,2,2,2,2,2,2,2,2,2,2,2,2,2,2,2,2,
2,4),(-2.66765111215731,-2.62407445969734,-2.60409385631716,-2.60009969993428,
-2.59852161183882,-2.59741658343656,-2.59640713873932,-2.59474984029436,
-2.59056385451666,-2.54053209371147,-2.51638356999891,-2.50455767987239,
-2.49657807409339,-2.49363506596365,-2.49184383953861,-2.48990306162119,
-2.48736308345081,-2.48307306618434,-2.44794206582757,-2.39901908258442,
-2.38926017550042,-2.38708452483878,-2.38584911720301,-2.38477513702998,
-2.38339730507794,-2.38053923481449,-2.35767518797266,-2.31214656554528,
-2.29549076408549,-2.28513772404252,-2.28188377473653,-2.27980902410011,
-2.27786835206758,-2.27532912684878,-2.27104175607711,-2.23592408342776,
-2.18705567479819,-2.17723123233823,-2.17505109491602,-2.17381469258006,
-2.17274084029038,-2.1713644687973,-2.16851388094193,-2.13210984678009,
-2.07830554016108,-2.07184821374121,-2.06913522816466,-2.06717247666518,
-2.06538030292746,-2.06251912043925,-2.05565952917868,-2.00224248325543,
-1.97655925428298,-1.96530844930874,-1.96303890217495,-1.96178297358227,
-1.96071136080605,-1.9593624071158,-1.95673583757679,-1.94056643275142,
-1.93131628638674,-1.89233774568212,-1.86585604079635,-1.85969287225457,
-1.85703013956307,-1.85507628727629,-1.85327303306179,-1.8503516278065,
-1.84313034462125,-1.79864231564355,-1.78473362850401,-1.76327602592312,
-1.75318370090961,-1.75098566897263,-1.74974535124647,-1.74867204967684,
-1.74730152130014,-1.74510870590138,-1.73333923482992,-1.72962683247937,
-1.72236557804097,-1.67901009360733,-1.66042268654731,-1.64921987837732,
-1.64587221629192,-1.6437768023276,-1.64184353018162,-1.63935164944882,
-1.63522643606853,-1.60809056910824,-1.56616637828247,-1.54954737000885,
-1.5409847878197,-1.53889723711027,-1.53768129815543,-1.53660390598313,
-1.53521798115663,-1.53292427491676,-1.51915033083512,-1.50784478798864,
-1.46844818216272,-1.44187538096531,-1.43570086894304,-1.43303616072426,
-1.43108195985373,-1.42927915700106,-1.42636021023468,-1.419153546198,-1.40835486065175),
 .UNSPECIFIED.);
#1028=B_SPLINE_CURVE_WITH_KNOTS('',3,(#105738,#105739,#105740,#105741,#105742,
#105743,#105744,#105745,#105746,#105747),.UNSPECIFIED.,.F.,.F.,(4,1,1,1,
1,1,1,4),(-97.7379483482805,-96.8871356463018,-95.8882991963399,-94.889462746378,
-93.8906262964161,-92.8917898464543,-91.8929533964924,-91.8056333339369),
 .UNSPECIFIED.);
#1029=B_SPLINE_CURVE_WITH_KNOTS('',3,(#105748,#105749,#105750,#105751,#105752,
#105753,#105754,#105755),.UNSPECIFIED.,.F.,.F.,(4,2,2,4),(-2.66796196902112,
-2.61567753669294,-2.59732738807453,-2.59351319560632),.UNSPECIFIED.);
#1030=B_SPLINE_CURVE_WITH_KNOTS('',3,(#105760,#105761,#105762,#105763,#105764,
#105765,#105766,#105767,#105768,#105769,#105770,#105771,#105772,#105773,
#105774,#105775,#105776,#105777,#105778,#105779,#105780,#105781,#105782,
#105783,#105784,#105785,#105786,#105787,#105788,#105789,#105790,#105791,
#105792,#105793,#105794,#105795,#105796,#105797,#105798,#105799,#105800,
#105801,#105802,#105803,#105804,#105805,#105806,#105807,#105808,#105809,
#105810,#105811,#105812,#105813,#105814,#105815,#105816,#105817,#105818,
#105819,#105820,#105821,#105822,#105823,#105824,#105825,#105826,#105827,
#105828,#105829,#105830,#105831,#105832,#105833,#105834,#105835,#105836,
#105837,#105838,#105839,#105840,#105841,#105842,#105843,#105844,#105845,
#105846,#105847,#105848,#105849,#105850,#105851,#105852,#105853,#105854,
#105855,#105856,#105857,#105858,#105859,#105860,#105861,#105862,#105863,
#105864,#105865,#105866,#105867,#105868,#105869,#105870,#105871,#105872,
#105873,#105874,#105875,#105876,#105877,#105878,#105879,#105880,#105881,
#105882,#105883,#105884,#105885,#105886,#105887,#105888,#105889,#105890,
#105891,#105892,#105893,#105894,#105895,#105896,#105897,#105898,#105899,
#105900,#105901,#105902,#105903,#105904,#105905,#105906,#105907,#105908,
#105909,#105910,#105911,#105912,#105913,#105914,#105915,#105916,#105917,
#105918,#105919,#105920,#105921,#105922,#105923,#105924,#105925,#105926,
#105927,#105928,#105929,#105930,#105931,#105932,#105933,#105934,#105935,
#105936,#105937,#105938,#105939,#105940,#105941,#105942,#105943,#105944,
#105945,#105946,#105947,#105948,#105949,#105950,#105951,#105952,#105953,
#105954,#105955,#105956,#105957,#105958,#105959,#105960,#105961,#105962,
#105963,#105964,#105965,#105966,#105967,#105968,#105969,#105970,#105971,
#105972,#105973,#105974,#105975),.UNSPECIFIED.,.F.,.F.,(4,2,2,2,2,2,2,2,
2,2,2,2,2,2,2,2,2,2,2,2,2,2,2,2,2,2,2,2,2,2,2,2,2,2,2,2,2,2,2,2,2,2,2,2,
2,2,2,2,2,2,2,2,2,2,2,2,2,2,2,2,2,2,2,2,2,2,2,2,2,2,2,2,2,2,2,2,2,2,2,2,
2,2,2,2,2,2,2,2,2,2,2,2,2,2,2,2,2,2,2,2,2,2,2,2,2,2,2,4),(-1.40856975518855,
-1.37753587866969,-1.33437708927627,-1.31573942604955,-1.31200670593019,
-1.30960679601331,-1.30769002652343,-1.30552247328272,-1.30184787503229,
-1.28708495689693,-1.25915990071243,-1.20936296122167,-1.20516000691329,
-1.20350003174228,-1.20249023890662,-1.20138599617114,-1.19981100945422,
-1.19583510293771,-1.17602243210622,-1.14710962007291,-1.10479066552403,
-1.10049554998527,-1.09795430887023,-1.09601356625899,-1.09394016522393,
-1.09069130869549,-1.08037952948746,-1.06381627701968,-1.03095548478581,
-1.01703050932108,-1.01060171826353,-0.995018249780802,-0.992416681650823,
-0.991073289507136,-0.990002246656862,-0.988742517785766,-0.986454683199814,
-0.974876354420389,-0.94788591706954,-0.896303999186155,-0.889313147946355,
-0.886430715237282,-0.884634956267085,-0.882676062091122,-0.879982610669475,
-0.873638510385787,-0.845679555567062,-0.799181399229366,-0.78306901187068,
-0.780442219249276,-0.779093411635139,-0.778022051023146,-0.776766581434501,
-0.774498267217136,-0.763262292897871,-0.737629700058277,-0.684119355716797,
-0.677267312166131,-0.674407802274688,-0.672616250976325,-0.670653844248833,
-0.667940707904399,-0.661480017710091,-0.607515332483881,-0.571349700551674,
-0.568494221403407,-0.56711711175029,-0.566043443635467,-0.564808120067418,
-0.562631946360587,-0.552859947082846,-0.503937170129568,-0.468830136471749,
-0.464527892189037,-0.461984761505626,-0.460043915174238,-0.457971700664554,
-0.454727409177611,-0.444452873120169,-0.427971021338313,-0.371279173650671,
-0.358728321248603,-0.356496629706004,-0.355114537874551,-0.354040395715363,
-0.352808363303963,-0.350647107763793,-0.341090377556351,-0.291984792241839,
-0.256812528772424,-0.252513924435505,-0.249971864513634,-0.248031213376732,
-0.246240564164274,-0.243303252798097,-0.235329252280526,-0.223526490989541,
-0.190999838568903,-0.150078388071853,-0.14538763422155,-0.143651112007467,
-0.142626619777758,-0.141533907642915,-0.140020740693023,-0.136420690088568,
-0.098526352753562,-0.0757357784074703,-0.0750516936837853),
 .UNSPECIFIED.);
#1031=B_SPLINE_CURVE_WITH_KNOTS('',3,(#105976,#105977,#105978,#105979,#105980,
#105981,#105982,#105983,#105984,#105985,#105986,#105987,#105988,#105989,
#105990,#105991,#105992,#105993,#105994,#105995,#105996,#105997,#105998,
#105999,#106000,#106001,#106002,#106003,#106004,#106005,#106006,#106007,
#106008,#106009,#106010,#106011,#106012,#106013,#106014,#106015,#106016,
#106017,#106018,#106019,#106020,#106021,#106022,#106023,#106024,#106025,
#106026,#106027,#106028,#106029,#106030,#106031,#106032,#106033,#106034,
#106035,#106036,#106037,#106038,#106039,#106040,#106041,#106042,#106043,
#106044,#106045,#106046,#106047,#106048,#106049,#106050,#106051,#106052,
#106053,#106054,#106055,#106056,#106057,#106058,#106059,#106060,#106061,
#106062,#106063,#106064,#106065,#106066,#106067,#106068,#106069,#106070,
#106071,#106072,#106073,#106074,#106075,#106076,#106077,#106078,#106079,
#106080,#106081,#106082,#106083,#106084,#106085,#106086,#106087,#106088,
#106089,#106090,#106091,#106092,#106093,#106094,#106095,#106096,#106097,
#106098,#106099,#106100,#106101,#106102,#106103,#106104,#106105,#106106,
#106107,#106108,#106109,#106110,#106111,#106112,#106113,#106114,#106115,
#106116,#106117,#106118,#106119,#106120,#106121,#106122,#106123,#106124,
#106125,#106126,#106127,#106128,#106129,#106130,#106131,#106132,#106133,
#106134,#106135,#106136,#106137,#106138,#106139,#106140,#106141,#106142,
#106143,#106144,#106145,#106146,#106147,#106148,#106149,#106150,#106151,
#106152,#106153,#106154,#106155,#106156,#106157,#106158,#106159,#106160,
#106161,#106162,#106163,#106164,#106165,#106166,#106167,#106168,#106169,
#106170,#106171,#106172,#106173,#106174,#106175,#106176,#106177,#106178,
#106179,#106180,#106181,#106182,#106183,#106184,#106185,#106186,#106187,
#106188,#106189,#106190,#106191,#106192,#106193,#106194,#106195,#106196,
#106197,#106198,#106199,#106200,#106201,#106202,#106203,#106204,#106205,
#106206,#106207,#106208,#106209,#106210,#106211,#106212,#106213,#106214,
#106215,#106216,#106217,#106218,#106219,#106220,#106221,#106222,#106223,
#106224,#106225,#106226,#106227,#106228,#106229,#106230,#106231,#106232,
#106233,#106234,#106235,#106236,#106237,#106238,#106239,#106240,#106241,
#106242,#106243,#106244,#106245,#106246,#106247),.UNSPECIFIED.,.F.,.F.,
(4,2,2,2,2,2,2,2,2,2,2,2,2,2,2,2,2,2,2,2,2,2,2,2,2,2,2,2,2,2,2,2,2,2,2,
2,2,2,2,2,2,2,2,2,2,2,2,2,2,2,2,2,2,2,2,2,2,2,2,2,2,2,2,2,2,2,2,2,2,2,2,
2,2,2,2,2,2,2,2,2,2,2,2,2,2,2,2,2,2,2,2,2,2,2,2,2,2,2,2,2,2,2,2,2,2,2,2,
2,2,2,2,2,2,2,2,2,2,2,2,2,2,2,2,2,2,2,2,2,2,2,2,2,2,2,2,4),(-2.59351319560632,
-2.58622729647481,-2.5828910286521,-2.58079840780792,-2.57886475756614,
-2.57636824993871,-2.57222640200302,-2.54442188896087,-2.50218668673736,
-2.4863039129939,-2.48078587998544,-2.47815169115976,-2.47603980137504,
-2.47481721054413,-2.47481365550069,-2.47481008690544,-2.47480650437782,
-2.47480290789427,-2.47479903883037,-2.47479510242231,-2.47479109722825,
-2.47478702163512,-2.47478287417935,-2.47477865356258,-2.47477435809535,
-2.4747699860217,-2.47476553576133,-2.47476100560858,-2.4747563936866,-2.4747516982887,
-2.47474691755708,-2.47474204951989,-2.47371676215764,-2.47234226881227,
-2.46950023768353,-2.43258570407835,-2.4009737629099,-2.38440863396358,
-2.37409713727002,-2.37084837729661,-2.36877504609808,-2.36683437516808,
-2.36429323824179,-2.3599983540294,-2.32488069726845,-2.27595609337913,
-2.26621225986546,-2.26403793530591,-2.2628029665682,-2.26172916672737,
-2.26035130298056,-2.25749226052489,-2.23432220255429,-2.19389543829676,
-2.16701319175459,-2.16080089954351,-2.15812995821089,-2.15617495824058,
-2.15437405952378,-2.15146407834257,-2.1443087833654,-2.09623415175186,
-2.05641757161317,-2.05283996628691,-2.05133047028622,-2.05023825258886,
-2.04921250722231,-2.04747019668775,-2.04274245790632,-2.00254661427086,
-1.95409223359277,-1.94848361985468,-1.94592066735513,-1.94398352098303,
-1.94215438428467,-1.93960316766758,-1.93290199156341,-1.87770481430317,
-1.8532397838111,-1.84230846741542,-1.8400580009635,-1.83880635261458,-1.83773454389397,
-1.8363804186677,-1.83424114104554,-1.82330530234437,-1.81870714839375,
-1.81437645424526,-1.76781417873323,-1.74938219701642,-1.73824679811172,
-1.73490673030146,-1.73281325542241,-1.73087985742359,-1.72838513436213,
-1.72424941044737,-1.69667985670387,-1.65436520346332,-1.63836283839693,
-1.63001370185051,-1.62794354536582,-1.6267316103303,-1.6256536018176,-1.62426148703803,
-1.62194627929144,-1.60773046460698,-1.60656384512424,-1.60507075355574,
-1.59761470273349,-1.58581497489413,-1.55294923960831,-1.53641432631062,
-1.52611631511088,-1.52286896909941,-1.52079585850479,-1.51885491497281,
-1.51631272961663,-1.51201452299214,-1.47665305033896,-1.42748800017924,
-1.41817192492958,-1.4160275905967,-1.41479917716189,-1.41372427645148,
-1.41233603847899,-1.40942413232278,-1.37758912981916,-1.33442733211732,
-1.31578836957074,-1.31205538917346,-1.30965531190433,-1.30773840874649,
-1.3055707043418,-1.3018958498089,-1.28713190177762,-1.26001648429561),
 .UNSPECIFIED.);
#1032=B_SPLINE_CURVE_WITH_KNOTS('',3,(#106253,#106254,#106255,#106256,#106257),
 .UNSPECIFIED.,.F.,.F.,(4,1,4),(82.6397395452727,82.9034253468356,82.9907454093913),
 .UNSPECIFIED.);
#1033=B_SPLINE_CURVE_WITH_KNOTS('',3,(#106258,#106259,#106260,#106261,#106262,
#106263,#106264,#106265,#106266,#106267,#106268,#106269,#106270,#106271,
#106272,#106273,#106274,#106275,#106276,#106277,#106278,#106279,#106280,
#106281,#106282,#106283,#106284,#106285,#106286,#106287,#106288,#106289,
#106290,#106291,#106292,#106293,#106294,#106295,#106296,#106297,#106298,
#106299,#106300,#106301,#106302,#106303,#106304,#106305,#106306,#106307,
#106308,#106309,#106310,#106311,#106312,#106313,#106314,#106315,#106316,
#106317,#106318,#106319,#106320,#106321,#106322,#106323,#106324,#106325,
#106326,#106327,#106328,#106329,#106330,#106331,#106332,#106333,#106334,
#106335,#106336,#106337,#106338,#106339,#106340,#106341,#106342,#106343,
#106344,#106345,#106346,#106347,#106348,#106349,#106350,#106351,#106352,
#106353,#106354,#106355,#106356,#106357,#106358,#106359,#106360,#106361,
#106362,#106363,#106364,#106365,#106366,#106367,#106368,#106369,#106370,
#106371,#106372,#106373,#106374,#106375,#106376,#106377,#106378,#106379,
#106380,#106381,#106382,#106383,#106384,#106385,#106386,#106387,#106388,
#106389,#106390,#106391,#106392,#106393,#106394,#106395,#106396,#106397,
#106398,#106399,#106400,#106401,#106402,#106403,#106404,#106405,#106406,
#106407,#106408,#106409,#106410,#106411,#106412,#106413,#106414,#106415,
#106416,#106417,#106418,#106419,#106420,#106421,#106422,#106423,#106424,
#106425,#106426,#106427,#106428,#106429,#106430,#106431,#106432,#106433,
#106434,#106435,#106436,#106437,#106438,#106439,#106440,#106441,#106442,
#106443,#106444,#106445,#106446,#106447,#106448,#106449,#106450,#106451,
#106452,#106453,#106454,#106455,#106456,#106457,#106458,#106459,#106460,
#106461,#106462,#106463,#106464,#106465,#106466,#106467,#106468,#106469,
#106470,#106471,#106472,#106473,#106474,#106475,#106476,#106477,#106478,
#106479,#106480,#106481,#106482,#106483,#106484,#106485,#106486,#106487,
#106488,#106489,#106490,#106491,#106492,#106493,#106494,#106495,#106496,
#106497,#106498,#106499,#106500,#106501,#106502,#106503,#106504,#106505,
#106506,#106507,#106508,#106509,#106510,#106511,#106512,#106513,#106514,
#106515,#106516,#106517),.UNSPECIFIED.,.F.,.F.,(4,2,2,2,2,2,2,2,2,2,2,2,
2,2,2,2,2,2,2,2,2,2,2,2,2,2,2,2,2,2,2,2,2,2,2,2,2,2,2,2,2,2,2,2,2,2,2,2,
2,2,2,2,2,2,2,2,2,2,2,2,2,2,2,2,2,2,2,2,2,2,2,2,2,2,2,2,2,2,2,2,2,2,2,2,
2,2,2,2,2,2,2,2,2,2,2,2,2,2,2,2,2,2,2,2,2,2,2,2,2,2,2,2,2,2,2,2,2,2,2,2,
2,2,2,2,2,2,2,2,2,4),(-2.66770269248702,-2.61543390608651,-2.59708901872597,
-2.58599213567297,-2.58265684473502,-2.58056483944361,-2.57863175991318,
-2.57613599181597,-2.57199537664879,-2.54419949573402,-2.50197655657685,
-2.4860982783431,-2.48058182905784,-2.47794840215327,-2.4758371254069,-2.47461489290665,
-2.47461133859609,-2.47460777046125,-2.47460418859721,-2.47460059284622,
-2.47459672452964,-2.47459278871543,-2.47458878423225,-2.4745847095446,
-2.47458056293282,-2.47457634316857,-2.47457204866205,-2.47456767749543,
-2.47456322803027,-2.47455869878193,-2.47455408788495,-2.47454939350027,
-2.47454461377057,-2.47453974666965,-2.47351462281696,-2.47214035031746,
-2.46929879256742,-2.43238860783665,-2.40078017653839,-2.38421945468437,
-2.37391039286149,-2.3706622359411,-2.36858925018365,-2.36664887490175,
-2.36410808514931,-2.35981369817105,-2.32468817729439,-2.27572965952275,
-2.26603636731641,-2.26386575406602,-2.26263172004954,-2.26155798021014,
-2.26017920818975,-2.25731488151531,-2.23382126683387,-2.22170969805593,
-2.18883046149072,-2.17227566196906,-2.16196909941451,-2.15872109813416,
-2.156648059864,-2.15470752876087,-2.15216638105854,-2.14787104409181,-2.11269116772034,
-2.06356069282311,-2.05406347989256,-2.05190645283678,-2.050675361251,-2.04960109425711,
-2.04821758978073,-2.0453293297153,-2.01983024614342,-1.97758286427438,
-1.95424053602413,-1.94848220349302,-1.94589190605637,-1.94395059511402,
-1.94212956853807,-1.9396088721162,-1.93309992710885,-1.87606425095122,
-1.85280178606955,-1.84219712827799,-1.83996667070711,-1.83871942591645,
-1.83764722297716,-1.83628724094131,-1.83412863148369,-1.82287775300273,
-1.81679515807037,-1.76734752482176,-1.74916993396683,-1.73814465114353,
-1.7348165485156,-1.73272580971532,-1.73079168593352,-1.7282914589008,-1.72413668097178,
-1.69583626693606,-1.65387892702485,-1.63817238209544,-1.62992715167251,
-1.62786559807225,-1.62665562651006,-1.62557726257417,-1.62418195649302,
-1.6218557050497,-1.607472541764,-1.60648225523406,-1.60500252507759,-1.59754601795155,
-1.58574720429294,-1.55288376098251,-1.53635000124923,-1.52605270838614,
-1.52280558884335,-1.52073262281562,-1.51879181462613,-1.51624980652628,
-1.51195189957472,-1.47659289017339,-1.42743126908458,-1.41811584365443,
-1.41597165886288,-1.41474333108927,-1.4136685053321,-1.41228036416027,
-1.40936866104105,-1.40856975518855),.UNSPECIFIED.);
#1034=B_SPLINE_CURVE_WITH_KNOTS('',3,(#106519,#106520,#106521,#106522,#106523,
#106524,#106525,#106526,#106527,#106528,#106529,#106530,#106531,#106532,
#106533,#106534,#106535,#106536,#106537,#106538,#106539,#106540,#106541,
#106542,#106543,#106544,#106545,#106546,#106547,#106548,#106549,#106550,
#106551,#106552,#106553,#106554,#106555,#106556,#106557,#106558,#106559,
#106560,#106561,#106562,#106563,#106564,#106565,#106566,#106567,#106568,
#106569,#106570,#106571,#106572,#106573,#106574,#106575,#106576,#106577,
#106578,#106579,#106580,#106581,#106582,#106583,#106584,#106585,#106586,
#106587,#106588,#106589,#106590,#106591,#106592,#106593,#106594,#106595,
#106596,#106597,#106598,#106599,#106600,#106601,#106602,#106603,#106604,
#106605,#106606,#106607,#106608,#106609,#106610,#106611,#106612,#106613,
#106614,#106615,#106616,#106617,#106618,#106619,#106620,#106621,#106622,
#106623,#106624,#106625,#106626,#106627,#106628,#106629,#106630,#106631,
#106632,#106633,#106634,#106635,#106636,#106637,#106638,#106639,#106640,
#106641,#106642,#106643,#106644,#106645,#106646,#106647,#106648,#106649,
#106650,#106651,#106652,#106653,#106654,#106655,#106656,#106657,#106658,
#106659,#106660,#106661,#106662,#106663,#106664,#106665,#106666,#106667,
#106668,#106669,#106670,#106671,#106672,#106673,#106674,#106675,#106676,
#106677,#106678,#106679,#106680,#106681,#106682,#106683,#106684,#106685,
#106686,#106687,#106688,#106689,#106690,#106691,#106692,#106693,#106694,
#106695,#106696,#106697,#106698,#106699,#106700,#106701,#106702,#106703,
#106704,#106705,#106706,#106707,#106708,#106709,#106710,#106711,#106712,
#106713,#106714,#106715,#106716,#106717,#106718,#106719,#106720,#106721,
#106722,#106723,#106724,#106725,#106726,#106727,#106728,#106729,#106730,
#106731,#106732,#106733,#106734,#106735,#106736,#106737,#106738,#106739,
#106740,#106741,#106742,#106743,#106744,#106745,#106746,#106747,#106748,
#106749,#106750,#106751,#106752,#106753,#106754,#106755,#106756,#106757,
#106758,#106759,#106760,#106761,#106762,#106763,#106764,#106765,#106766,
#106767,#106768,#106769,#106770,#106771,#106772,#106773,#106774,#106775,
#106776,#106777,#106778,#106779,#106780,#106781,#106782),.UNSPECIFIED.,
 .F.,.F.,(4,2,2,2,2,2,2,2,2,2,2,2,2,2,2,2,2,2,2,2,2,2,2,2,2,2,2,2,2,2,2,
2,2,2,2,2,2,2,2,2,2,2,2,2,2,2,2,2,2,2,2,2,2,2,2,2,2,2,2,2,2,2,2,2,2,2,2,
2,2,2,2,2,2,2,2,2,2,2,2,2,2,2,2,2,2,2,2,2,2,2,2,2,2,2,2,2,2,2,2,2,2,2,2,
2,2,2,2,2,2,2,2,2,2,2,2,2,2,2,2,2,2,2,2,2,2,2,2,2,2,2,2,4),(-1.26001648429561,
-1.25920489695078,-1.20940448836762,-1.20520124082162,-1.20354114986599,
-1.20253128660603,-1.20142696686747,-1.19985187033462,-1.19587568666747,
-1.17606163521429,-1.1471468068602,-1.10482490162242,-1.10052948659098,
-1.09798806826835,-1.09604719031824,-1.09397364468755,-1.0907245615764,
-1.08041206308618,-1.06384765514126,-1.03098457123331,-1.01705856606983,
-1.0106294555596,-0.995044836916912,-0.992443084660772,-0.991099598250274,
-0.990028480673695,-0.988768664410134,-0.986480672386839,-0.974901573923448,
-0.947909407086809,-0.896323680640296,-0.889332355187557,-0.886449723671537,
-0.884653839874391,-0.88269480875693,-0.880001167632593,-0.873656613949112,
-0.845695618422445,-0.799193315313246,-0.783080691472976,-0.780453790669127,
-0.779104905126549,-0.778033470879843,-0.776777901415799,-0.774509372324553,
-0.763271636052209,-0.737633451839069,-0.684124892294134,-0.67727192457901,
-0.674412141771313,-0.672620452228583,-0.670657920468287,-0.667944659801545,
-0.661483904869319,-0.607528601539598,-0.571346076407321,-0.568490853645776,
-0.567113737401025,-0.566040002926676,-0.564804533874532,-0.562627938470995,
-0.552851307085002,-0.503928450894076,-0.468823462713982,-0.464101471570169,
-0.46167862601721,-0.459759698495756,-0.457606763773942,-0.453997974824864,
-0.440035486926255,-0.389255795890994,-0.359425299829533,-0.356511190805702,
-0.355122608814479,-0.35404776287155,-0.35281978042695,-0.350677046768013,
-0.341381333426028,-0.322532398642188,-0.285802998947758,-0.256623995330623,
-0.252442931410543,-0.249934948227704,-0.247999556502226,-0.247958738862809,
-0.247923852040322,-0.247894029820711,-0.24786853301023,-0.247846730883511,
-0.247828085306439,-0.247805395030296,-0.247783497486897,-0.247762362612493,
-0.247741961719488,-0.247722267322392,-0.247703253072053,-0.247684893668127,
-0.247667164828339,-0.247650043226398,-0.247633506438837,-0.247617532879141,
-0.247602101991462,-0.247587193913733,-0.247572792895465,-0.247558879109898,
-0.247545433492083,-0.247532439218449,-0.247519880067256,-0.245316875653341,
-0.24143011281927,-0.236650002340525,-0.226661648557354,-0.197489855218114,
-0.149610976621307,-0.145275678286585,-0.143594266582085,-0.142580467621698,
-0.141479947671423,-0.13992389071989,-0.136065402572038,-0.117353448275053,
-0.0757357782033879,-0.0634020279927224,-0.0604358932045252,-0.0436144758865441,
-0.0399995534467219,-0.0376361158920789,-0.0357225177441432,-0.0339209984432892,
-0.0317709117344062,-0.0286342827363197,-0.000628475142166855),
 .UNSPECIFIED.);
#1035=B_SPLINE_CURVE_WITH_KNOTS('',3,(#106783,#106784,#106785,#106786,#106787,
#106788,#106789,#106790,#106791,#106792,#106793,#106794,#106795,#106796,
#106797,#106798,#106799,#106800),.UNSPECIFIED.,.F.,.F.,(4,2,2,2,2,2,2,2,
4),(-2.66758135155173,-2.62400468004738,-2.60402406129045,-2.60002990222267,
-2.59845181316381,-2.59734678412026,-2.5963373388615,-2.59468003953891,
-2.59343214472076),.UNSPECIFIED.);
#1036=B_SPLINE_CURVE_WITH_KNOTS('',3,(#106806,#106807,#106808,#106809,#106810,
#106811,#106812,#106813,#106814,#106815,#106816,#106817,#106818),
 .UNSPECIFIED.,.F.,.F.,(4,3,3,3,4),(76.3573195230834,76.458908846057,76.5605128417353,
76.6622238573892,76.7075599105292),.UNSPECIFIED.);
#1037=B_SPLINE_CURVE_WITH_KNOTS('',3,(#106819,#106820,#106821,#106822,#106823,
#106824,#106825,#106826,#106827,#106828),.UNSPECIFIED.,.F.,.F.,(4,1,1,1,
1,1,1,4),(76.7075601022117,76.9104066470643,77.9092430970262,78.9080795469881,
79.9069159969499,80.9057524469118,81.9045888968737,82.6397395452727),
 .UNSPECIFIED.);
#1038=B_SPLINE_CURVE_WITH_KNOTS('',3,(#106829,#106830,#106831,#106832,#106833,
#106834,#106835,#106836,#106837,#106838,#106839,#106840,#106841,#106842,
#106843,#106844,#106845,#106846,#106847,#106848,#106849,#106850,#106851,
#106852,#106853,#106854,#106855,#106856,#106857,#106858,#106859,#106860,
#106861,#106862,#106863,#106864,#106865,#106866,#106867,#106868,#106869,
#106870,#106871,#106872,#106873,#106874,#106875,#106876,#106877,#106878,
#106879,#106880,#106881,#106882,#106883,#106884,#106885,#106886,#106887,
#106888,#106889,#106890,#106891,#106892,#106893,#106894,#106895,#106896,
#106897,#106898,#106899,#106900,#106901,#106902,#106903,#106904,#106905,
#106906,#106907,#106908,#106909,#106910,#106911,#106912,#106913,#106914,
#106915,#106916,#106917,#106918,#106919,#106920,#106921,#106922,#106923,
#106924,#106925,#106926,#106927,#106928,#106929,#106930,#106931,#106932,
#106933,#106934,#106935,#106936,#106937,#106938,#106939,#106940,#106941,
#106942,#106943,#106944,#106945,#106946,#106947,#106948,#106949,#106950,
#106951,#106952,#106953,#106954,#106955,#106956,#106957,#106958,#106959,
#106960,#106961,#106962,#106963,#106964,#106965,#106966,#106967,#106968,
#106969,#106970,#106971,#106972,#106973,#106974,#106975,#106976,#106977,
#106978,#106979,#106980,#106981,#106982,#106983,#106984,#106985,#106986,
#106987,#106988,#106989,#106990,#106991,#106992,#106993,#106994,#106995,
#106996,#106997,#106998,#106999,#107000,#107001,#107002,#107003,#107004,
#107005,#107006,#107007,#107008,#107009,#107010,#107011,#107012,#107013,
#107014,#107015,#107016,#107017,#107018,#107019,#107020,#107021,#107022,
#107023,#107024,#107025,#107026,#107027,#107028,#107029,#107030,#107031,
#107032,#107033,#107034,#107035,#107036,#107037,#107038,#107039,#107040,
#107041,#107042,#107043,#107044,#107045,#107046,#107047,#107048,#107049,
#107050,#107051,#107052,#107053,#107054,#107055,#107056,#107057,#107058,
#107059,#107060),.UNSPECIFIED.,.F.,.F.,(4,2,2,2,2,2,2,2,2,2,2,2,2,2,2,2,
2,2,2,2,2,2,2,2,2,2,2,2,2,2,2,2,2,2,2,2,2,2,2,2,2,2,2,2,2,2,2,2,2,2,2,2,
2,2,2,2,2,2,2,2,2,2,2,2,2,2,2,2,2,2,2,2,2,2,2,2,2,2,2,2,2,2,2,2,2,2,2,2,
2,2,2,2,2,2,2,2,2,2,2,2,2,2,2,2,2,2,2,2,2,2,2,2,2,2,2,4),(-2.59343214472076,
-2.59049405177952,-2.54046226013771,-2.51631371553413,-2.50448782487539,
-2.49650821776788,-2.49356520789235,-2.4917739804419,-2.48983320130117,
-2.48729322097717,-2.48300319883559,-2.44787191663159,-2.39894810145459,
-2.38919014010936,-2.38701455334178,-2.38577915932073,-2.38470517646818,
-2.3833273220989,-2.38046913999823,-2.35760068662714,-2.31207027802872,
-2.29541852548593,-2.28506731090479,-2.28181356940159,-2.27973886362835,
-2.27779817210041,-2.27525883283369,-2.27097107139423,-2.23581092895971,
-2.18681243869875,-2.17714169331629,-2.17497209228785,-2.17373800617207,
-2.17266381785388,-2.17128394195642,-2.16906025241394,-2.15666860288048,
-2.14992522387111,-2.10271279728319,-2.08431872950774,-2.07319905836646,
-2.06986026397319,-2.06776681331326,-2.06583291058881,-2.06333679777569,
-2.05919716850347,-2.03150304958646,-1.98921351003062,-1.97327362885962,
-1.96494579070437,-1.96287710524162,-1.9616653542782,-1.96058704774786,
-1.95919394894811,-1.95687585020999,-1.94261282142306,-1.93155606646583,
-1.93131882217436,-1.89233827786464,-1.86585616222138,-1.85969294270398,
-1.8570302012477,-1.85507634752613,-1.85327309549817,-1.85035170163565,
-1.84313048537446,-1.79862196300042,-1.78473430111998,-1.76327618979293,
-1.75318371597878,-1.75098567421837,-1.74974535432619,-1.74867205301748,
-1.74730152774724,-1.74510872263625,-1.73333941156873,-1.72962683785969,
-1.72236557018538,-1.67901009148259,-1.66042268433315,-1.64921987609181,
-1.64587221396772,-1.64377679997451,-1.64184352779864,-1.63935164702255,
-1.63522643355997,-1.60809056486313,-1.56616637408107,-1.54954736726303,
-1.54098478554423,-1.53889723485167,-1.53768129588908,-1.53660390369748,
-1.5352179788294,-1.53292427248687,-1.51915032676092,-1.50784479204249,
-1.46844818147014,-1.44187537907986,-1.43570086687288,-1.43303615859763,
-1.43108195769395,-1.42927915481719,-1.4263602080251,-1.41915354398586,
-1.37307254950704,-1.33396207651879,-1.33297747694236,-1.32826979179497,
-1.32653031764444,-1.3255049915898,-1.32441216064219,-1.32290008666066,
-1.31930843287669,-1.28016623845279,-1.25968440003088),.UNSPECIFIED.);
#1039=B_SPLINE_CURVE_WITH_KNOTS('',3,(#107066,#107067,#107068,#107069,#107070,
#107071,#107072,#107073,#107074,#107075,#107076,#107077,#107078,#107079,
#107080,#107081),.UNSPECIFIED.,.F.,.F.,(4,2,2,2,2,2,2,4),(-0.0749582685536123,
-0.0267279126156495,-0.0187640072134933,-0.00802108894736205,-0.00466632906678189,
-0.00258130059291907,-0.00128118361729658,-0.000628940948285152),
 .UNSPECIFIED.);
#1040=B_SPLINE_CURVE_WITH_KNOTS('',3,(#107082,#107083,#107084,#107085,#107086,
#107087,#107088,#107089,#107090,#107091,#107092,#107093,#107094,#107095,
#107096,#107097,#107098,#107099,#107100,#107101,#107102,#107103,#107104,
#107105,#107106,#107107,#107108,#107109,#107110,#107111,#107112,#107113,
#107114,#107115,#107116,#107117,#107118,#107119,#107120,#107121,#107122,
#107123,#107124,#107125,#107126,#107127,#107128,#107129,#107130,#107131,
#107132,#107133,#107134,#107135,#107136,#107137,#107138,#107139,#107140,
#107141,#107142,#107143,#107144,#107145,#107146,#107147,#107148,#107149,
#107150,#107151,#107152,#107153,#107154,#107155,#107156,#107157,#107158,
#107159,#107160,#107161,#107162,#107163,#107164,#107165,#107166,#107167,
#107168,#107169,#107170,#107171,#107172,#107173,#107174,#107175,#107176,
#107177,#107178,#107179,#107180,#107181,#107182,#107183,#107184,#107185,
#107186,#107187,#107188,#107189,#107190,#107191,#107192,#107193,#107194,
#107195,#107196,#107197,#107198,#107199,#107200,#107201,#107202,#107203,
#107204,#107205,#107206,#107207,#107208,#107209,#107210,#107211,#107212,
#107213,#107214,#107215,#107216,#107217,#107218,#107219,#107220,#107221,
#107222,#107223,#107224,#107225,#107226,#107227,#107228,#107229,#107230,
#107231,#107232,#107233,#107234,#107235,#107236,#107237,#107238,#107239,
#107240,#107241,#107242,#107243,#107244,#107245,#107246,#107247,#107248,
#107249,#107250,#107251,#107252,#107253,#107254,#107255,#107256,#107257,
#107258,#107259,#107260,#107261,#107262),.UNSPECIFIED.,.F.,.F.,(4,3,3,3,
3,3,3,3,3,3,3,3,3,3,3,3,3,3,3,3,3,3,3,3,3,3,3,3,3,3,3,3,3,3,3,3,3,3,3,3,
3,3,3,3,3,3,3,3,3,3,3,3,3,3,3,3,3,3,3,3,4),(70.4243747954073,70.5325790413764,
70.6410991164255,70.7497863837844,70.8587740112828,70.9173879472931,71.0207826843409,
71.1240239664559,71.227143931848,71.3301985000568,71.4332217084145,71.5362475510868,
71.6393803178647,71.7425694092745,71.845941402656,71.9162243972549,72.0196191343028,
72.1228604164179,72.2259803818101,72.3290349500191,72.4320581583768,72.5350840010493,
72.6382167678274,72.7414058592372,72.8447778526189,72.9150608472168,73.0184555842648,
73.1216968663798,73.2248168317722,73.3278713999811,73.4308946083389,73.5339204510115,
73.6370532177896,73.7402423091995,73.8436143025812,73.9138972971787,74.0172920342266,
74.1205333163416,74.2236532817338,74.3267078499427,74.4297310583004,74.5327569009728,
74.6358896677508,74.7390787591606,74.8424507525422,74.9127337471406,75.0161284841885,
75.1193697663035,75.2224897316958,75.3255442999047,75.4285675082625,75.5315933509351,
75.6347261177132,75.7379152091229,75.8412872025046,75.9115701971024,76.0134810050321,
76.1152211478687,76.2168630906174,76.3184433457363,76.3573195230834),
 .UNSPECIFIED.);
#1041=B_SPLINE_CURVE_WITH_KNOTS('',3,(#107264,#107265,#107266,#107267,#107268,
#107269,#107270,#107271,#107272,#107273,#107274,#107275,#107276,#107277,
#107278,#107279,#107280,#107281,#107282,#107283,#107284,#107285,#107286,
#107287,#107288,#107289,#107290,#107291,#107292,#107293,#107294,#107295,
#107296,#107297,#107298,#107299,#107300,#107301,#107302,#107303,#107304,
#107305,#107306,#107307,#107308,#107309,#107310,#107311,#107312,#107313,
#107314,#107315,#107316,#107317,#107318,#107319,#107320,#107321,#107322,
#107323,#107324,#107325,#107326,#107327,#107328,#107329,#107330,#107331,
#107332,#107333,#107334,#107335,#107336,#107337,#107338,#107339,#107340,
#107341,#107342,#107343,#107344,#107345,#107346,#107347,#107348,#107349,
#107350,#107351,#107352,#107353,#107354,#107355,#107356,#107357,#107358,
#107359,#107360,#107361,#107362,#107363,#107364,#107365,#107366,#107367,
#107368,#107369,#107370,#107371,#107372,#107373,#107374,#107375,#107376,
#107377,#107378,#107379,#107380,#107381,#107382,#107383,#107384,#107385,
#107386,#107387,#107388,#107389,#107390,#107391,#107392,#107393,#107394,
#107395,#107396,#107397,#107398,#107399,#107400,#107401,#107402,#107403,
#107404,#107405,#107406,#107407,#107408,#107409,#107410,#107411,#107412,
#107413,#107414,#107415,#107416,#107417,#107418,#107419,#107420,#107421,
#107422,#107423,#107424,#107425,#107426,#107427,#107428,#107429,#107430,
#107431,#107432,#107433,#107434,#107435,#107436,#107437,#107438,#107439,
#107440,#107441,#107442,#107443,#107444,#107445,#107446,#107447,#107448,
#107449,#107450,#107451,#107452,#107453,#107454,#107455,#107456,#107457,
#107458,#107459,#107460,#107461,#107462,#107463,#107464,#107465,#107466,
#107467,#107468,#107469,#107470,#107471,#107472,#107473,#107474,#107475,
#107476,#107477,#107478,#107479),.UNSPECIFIED.,.F.,.F.,(4,2,2,2,2,2,2,2,
2,2,2,2,2,2,2,2,2,2,2,2,2,2,2,2,2,2,2,2,2,2,2,2,2,2,2,2,2,2,2,2,2,2,2,2,
2,2,2,2,2,2,2,2,2,2,2,2,2,2,2,2,2,2,2,2,2,2,2,2,2,2,2,2,2,2,2,2,2,2,2,2,
2,2,2,2,2,2,2,2,2,2,2,2,2,2,2,2,2,2,2,2,2,2,2,2,2,2,2,4),(-1.25968440003088,
-1.23134369063143,-1.22421241025332,-1.22130615144709,-1.21950571246795,
-1.21754976113992,-1.21487490057086,-1.20864153191671,-1.18159607626975,
-1.14087004519534,-1.11820871474527,-1.11535576177377,-1.11397896260965,
-1.11290510951051,-1.11166909066276,-1.10949053703989,-1.09968869014144,
-1.05077806094501,-1.01565732978857,-1.01136167391632,-1.00882015719558,
-1.00687922949478,-1.0048056553366,-1.00155657894078,-0.991244535246914,
-0.974681270103429,-0.94181871242264,-0.928012268689017,-0.921312713500247,
-0.905865018602465,-0.903497110758078,-0.902089531001489,-0.901009375125651,
-0.89980592473939,-0.897774117147262,-0.889883828855659,-0.875166458977492,
-0.84610353321798,-0.803698159063138,-0.799404688454027,-0.79686386219703,
-0.794923114745073,-0.792849396568352,-0.789599391503073,-0.779278469475279,
-0.762695298773928,-0.729817074534332,-0.71452118017559,-0.709793775253745,
-0.693941560887125,-0.691328748436845,-0.689982891387343,-0.688911647404452,
-0.687653730257804,-0.685374418609237,-0.673948877567028,-0.647572473611019,
-0.59512229067345,-0.588188791336395,-0.585315747071719,-0.583521640093746,
-0.581561187570464,-0.578859458459984,-0.572467088243047,-0.526046748643198,
-0.48494794489779,-0.480263095853582,-0.47852731511801,-0.477502864531078,
-0.47640986013649,-0.474895738335049,-0.47129087238757,-0.432949642134656,
-0.383317392119324,-0.376221666139646,-0.373321736379029,-0.371522742279671,
-0.369566400597489,-0.366887468622537,-0.360806601280349,-0.352445803405556,
-0.301551400708137,-0.270313240735481,-0.267401273607805,-0.266013096698057,
-0.264938280950742,-0.263710016013293,-0.26156604694954,-0.252414962827848,
-0.203666416271385,-0.167704289663162,-0.162982355730755,-0.160559557266441,
-0.158640675771371,-0.156487801866807,-0.15425804644873,-0.146612093359325,
-0.121083043180849,-0.100337614942073,-0.0610229393878702,-0.0562870044016026,
-0.0545435810105591,-0.0535177050911518,-0.0524257923617553,-0.0509174392522457,
-0.0492296204587821,-0.0462824097053656,-0.000629118990308949),
 .UNSPECIFIED.);
#1042=B_SPLINE_CURVE_WITH_KNOTS('',3,(#107480,#107481,#107482,#107483,#107484,
#107485,#107486,#107487,#107488,#107489,#107490,#107491,#107492),
 .UNSPECIFIED.,.F.,.F.,(4,3,3,3,4),(-66.6728921052185,-66.5709585796848,
-66.469095014769,-66.367250944913,-66.322858845468),.UNSPECIFIED.);
#1043=B_SPLINE_CURVE_WITH_KNOTS('',3,(#107497,#107498,#107499,#107500,#107501,
#107502,#107503,#107504,#107505,#107506,#107507,#107508,#107509,#107510,
#107511,#107512,#107513,#107514,#107515,#107516,#107517,#107518,#107519,
#107520,#107521,#107522,#107523,#107524,#107525,#107526,#107527,#107528,
#107529,#107530,#107531,#107532,#107533,#107534,#107535,#107536,#107537,
#107538,#107539,#107540,#107541,#107542,#107543,#107544,#107545,#107546,
#107547,#107548,#107549,#107550,#107551,#107552,#107553,#107554,#107555,
#107556,#107557,#107558,#107559,#107560,#107561,#107562,#107563,#107564,
#107565,#107566,#107567,#107568,#107569,#107570,#107571,#107572,#107573,
#107574,#107575,#107576,#107577,#107578,#107579,#107580,#107581,#107582,
#107583,#107584,#107585,#107586,#107587,#107588,#107589,#107590,#107591,
#107592,#107593,#107594,#107595,#107596,#107597,#107598,#107599,#107600,
#107601,#107602,#107603,#107604,#107605,#107606,#107607,#107608,#107609,
#107610,#107611,#107612,#107613,#107614,#107615,#107616,#107617,#107618,
#107619,#107620,#107621,#107622,#107623,#107624,#107625,#107626,#107627,
#107628,#107629,#107630,#107631,#107632,#107633,#107634,#107635,#107636,
#107637,#107638,#107639,#107640,#107641,#107642,#107643,#107644,#107645,
#107646,#107647,#107648,#107649,#107650,#107651,#107652,#107653,#107654,
#107655,#107656,#107657,#107658,#107659,#107660,#107661,#107662,#107663,
#107664,#107665,#107666,#107667,#107668,#107669,#107670,#107671,#107672,
#107673,#107674,#107675,#107676,#107677,#107678,#107679,#107680,#107681,
#107682,#107683,#107684,#107685,#107686,#107687,#107688,#107689,#107690,
#107691,#107692,#107693,#107694,#107695,#107696,#107697,#107698,#107699,
#107700,#107701,#107702,#107703,#107704,#107705,#107706,#107707,#107708,
#107709,#107710,#107711,#107712,#107713,#107714,#107715,#107716,#107717,
#107718,#107719,#107720,#107721,#107722,#107723,#107724,#107725,#107726,
#107727,#107728,#107729,#107730,#107731,#107732),.UNSPECIFIED.,.F.,.F.,
(4,2,2,2,2,2,2,2,2,2,2,2,2,2,2,2,2,2,2,2,2,2,2,2,2,2,2,2,2,2,2,2,2,2,2,
2,2,2,2,2,2,2,2,2,2,2,2,2,2,2,2,2,2,2,2,2,2,2,2,2,2,2,2,2,2,2,2,2,2,2,2,
2,2,2,2,2,2,2,2,2,2,2,2,2,2,2,2,2,2,2,2,2,2,2,2,2,2,2,2,2,2,2,2,2,2,2,2,
2,2,2,2,2,2,2,2,2,2,4),(-1.40860274249303,-1.39545372053415,-1.38405191255192,
-1.38177360603223,-1.38051573100286,-1.37944421601724,-1.37809762224227,
-1.37548221954635,-1.35956072507084,-1.35505839864631,-1.3344941572798,
-1.28613739827495,-1.27898801345227,-1.27607861829502,-1.27427752549132,
-1.27232188142241,-1.26964927272706,-1.26342950298786,-1.23649576466275,
-1.19596815909722,-1.1729752699172,-1.17011974512723,-1.16874239215002,
-1.16766843028723,-1.16643265125198,-1.16425539405046,-1.15447387394157,
-1.10554271681862,-1.07041410358646,-1.06611811509309,-1.06357642475794,
-1.06163537781953,-1.05956168921858,-1.05631246052951,-1.04600016133745,
-1.02943670254059,-0.996572845154755,-0.982829375741294,-0.975979431163806,
-0.975668394635018,-0.970141227948445,-0.960085624833772,-0.958003434641783,
-0.956666723725821,-0.955595910672606,-0.954330489411165,-0.952016880235014,
-0.939969961362546,-0.887892504752826,-0.85823648297296,-0.854045172676218,
-0.851534106912541,-0.849598134439495,-0.847511861535831,-0.844204716305503,
-0.833374313120382,-0.815647041064647,-0.765033835011717,-0.748652933501051,
-0.746018229818602,-0.744667621415628,-0.743596013538634,-0.742341621977587,
-0.740078712913451,-0.728939064684917,-0.703681073476061,-0.64961305370415,
-0.642806060412559,-0.639953770356868,-0.638163360840862,-0.636199471538239,
-0.633479246418707,-0.626977553308289,-0.597700080219243,-0.557147289503821,
-0.552470286680263,-0.536615849012431,-0.534003013797779,-0.532657161058179,
-0.531585928963038,-0.530328035593527,-0.52804879206617,-0.516624112560615,
-0.490250909400853,-0.437796774641233,-0.430863984088467,-0.427991076922987,
-0.426197009858696,-0.424236564324825,-0.421534777893735,-0.415141956993546,
-0.368529713838952,-0.327635551524136,-0.322942373867071,-0.321205340293311,
-0.32018065208492,-0.319087820765109,-0.317574635505883,-0.313975218995091,
-0.276193354998924,-0.225953709927059,-0.21889336642317,-0.216053366803244,
-0.21408580476914,-0.212152641387071,-0.210202118920216,-0.205222354907001,
-0.167242607375536,-0.126440833166427,-0.112446926052252,-0.110143000891382,
-0.108754236261121,-0.107676702942697,-0.106462936107806,-0.104384338263129,
-0.0959299608814828,-0.0796216983056657,-0.0749582685536123),
 .UNSPECIFIED.);
#1044=B_SPLINE_CURVE_WITH_KNOTS('',3,(#107734,#107735,#107736,#107737,#107738,
#107739,#107740,#107741,#107742,#107743,#107744,#107745,#107746,#107747,
#107748,#107749,#107750,#107751,#107752,#107753,#107754,#107755,#107756,
#107757,#107758,#107759,#107760,#107761,#107762,#107763,#107764,#107765,
#107766,#107767,#107768,#107769,#107770,#107771,#107772,#107773,#107774,
#107775,#107776,#107777,#107778,#107779,#107780,#107781,#107782,#107783,
#107784,#107785,#107786,#107787,#107788,#107789,#107790,#107791,#107792,
#107793,#107794,#107795,#107796,#107797,#107798,#107799,#107800,#107801,
#107802,#107803,#107804,#107805,#107806,#107807,#107808,#107809,#107810,
#107811,#107812,#107813,#107814,#107815,#107816,#107817,#107818,#107819,
#107820,#107821,#107822,#107823,#107824,#107825,#107826,#107827,#107828,
#107829,#107830,#107831,#107832,#107833,#107834,#107835,#107836,#107837,
#107838,#107839,#107840,#107841,#107842,#107843,#107844,#107845,#107846,
#107847,#107848,#107849,#107850,#107851,#107852,#107853,#107854,#107855,
#107856,#107857,#107858,#107859,#107860,#107861,#107862,#107863,#107864,
#107865,#107866,#107867,#107868,#107869,#107870,#107871,#107872,#107873,
#107874,#107875,#107876,#107877,#107878,#107879,#107880,#107881,#107882,
#107883,#107884,#107885,#107886,#107887,#107888,#107889,#107890,#107891,
#107892,#107893,#107894,#107895,#107896,#107897,#107898,#107899,#107900,
#107901,#107902,#107903,#107904,#107905,#107906,#107907,#107908,#107909,
#107910,#107911),.UNSPECIFIED.,.F.,.F.,(4,3,3,3,3,3,3,3,3,3,3,3,3,3,3,3,
3,3,3,3,3,3,3,3,3,3,3,3,3,3,3,3,3,3,3,3,3,3,3,3,3,3,3,3,3,3,3,3,3,3,3,3,
3,3,3,3,3,3,3,4),(-66.322858845468,-66.2209269943692,-66.1189509138928,
-66.0167874984565,-65.9232056974837,-65.8198109604357,-65.7165696783207,
-65.6134497129284,-65.5103951447195,-65.4073719363617,-65.3043460936892,
-65.201213326911,-65.0980242355013,-64.9946522421195,-64.9243692475218,
-64.8209745104739,-64.7177332283589,-64.6146132629666,-64.5115586947577,
-64.4085354864,-64.3055096437274,-64.2023768769493,-64.0991877855396,-63.9958157921579,
-63.9255327975599,-63.822138060512,-63.718896778397,-63.6157768130047,-63.5127222447958,
-63.4096990364381,-63.3066731937654,-63.2035404269873,-63.1003513355775,
-62.9969793421958,-62.9266963475981,-62.8233016105501,-62.7200603284354,
-62.6169403630431,-62.5138857948342,-62.4108625864764,-62.3078367438042,
-62.2047039770261,-62.1015148856164,-61.9981428922348,-61.9278598976362,
-61.8244651605882,-61.7212238784728,-61.6181039130805,-61.5150493448716,
-61.4120261365139,-61.3090002938414,-61.2058675270632,-61.1026784356534,
-60.9993064422717,-60.9290234476743,-60.8220651862384,-60.7139755891885,
-60.6074364851718,-60.4985716416054,-60.3897067980389),.UNSPECIFIED.);
#1045=B_SPLINE_CURVE_WITH_KNOTS('',3,(#107912,#107913,#107914,#107915),
 .UNSPECIFIED.,.F.,.F.,(4,4),(-60.389703770172,-60.0402340848269),
 .UNSPECIFIED.);
#1046=B_SPLINE_CURVE_WITH_KNOTS('',3,(#107921,#107922,#107923,#107924,#107925,
#107926),.UNSPECIFIED.,.F.,.F.,(4,2,4),(-0.075040891899263,-0.0536888394344463,
-0.000629601840572249),.UNSPECIFIED.);
#1047=B_SPLINE_CURVE_WITH_KNOTS('',3,(#107927,#107928,#107929,#107930,#107931,
#107932,#107933,#107934,#107935,#107936,#107937,#107938,#107939,#107940,
#107941,#107942,#107943,#107944,#107945,#107946,#107947,#107948,#107949,
#107950,#107951,#107952,#107953,#107954,#107955,#107956,#107957,#107958,
#107959,#107960,#107961,#107962,#107963,#107964,#107965,#107966,#107967,
#107968,#107969,#107970,#107971,#107972,#107973,#107974,#107975,#107976,
#107977,#107978,#107979,#107980,#107981,#107982,#107983,#107984,#107985,
#107986,#107987,#107988,#107989,#107990,#107991,#107992,#107993,#107994,
#107995,#107996,#107997,#107998,#107999,#108000,#108001,#108002,#108003,
#108004,#108005,#108006,#108007,#108008,#108009,#108010,#108011,#108012,
#108013,#108014,#108015,#108016,#108017,#108018,#108019,#108020,#108021,
#108022,#108023,#108024,#108025,#108026,#108027,#108028,#108029,#108030,
#108031,#108032,#108033,#108034,#108035,#108036,#108037,#108038,#108039,
#108040,#108041,#108042,#108043,#108044,#108045,#108046,#108047,#108048,
#108049,#108050,#108051,#108052,#108053,#108054,#108055,#108056,#108057,
#108058,#108059,#108060,#108061,#108062,#108063,#108064,#108065,#108066,
#108067,#108068,#108069,#108070,#108071,#108072,#108073,#108074,#108075,
#108076,#108077,#108078,#108079,#108080,#108081,#108082,#108083,#108084,
#108085,#108086,#108087,#108088,#108089,#108090,#108091,#108092,#108093,
#108094,#108095,#108096,#108097,#108098,#108099,#108100,#108101,#108102,
#108103,#108104,#108105,#108106,#108107,#108108,#108109,#108110,#108111,
#108112,#108113,#108114,#108115,#108116,#108117,#108118,#108119,#108120,
#108121,#108122,#108123,#108124,#108125,#108126,#108127,#108128,#108129,
#108130,#108131,#108132,#108133,#108134,#108135,#108136,#108137,#108138,
#108139,#108140,#108141,#108142,#108143,#108144,#108145,#108146,#108147,
#108148,#108149,#108150,#108151,#108152,#108153,#108154,#108155,#108156,
#108157,#108158,#108159,#108160,#108161,#108162,#108163,#108164,#108165,
#108166,#108167,#108168,#108169,#108170,#108171,#108172,#108173,#108174,
#108175,#108176,#108177,#108178),.UNSPECIFIED.,.F.,.F.,(4,2,2,2,2,2,2,2,
2,2,2,2,2,2,2,2,2,2,2,2,2,2,2,2,2,2,2,2,2,2,2,2,2,2,2,2,2,2,2,2,2,2,2,2,
2,2,2,2,2,2,2,2,2,2,2,2,2,2,2,2,2,2,2,2,2,2,2,2,2,2,2,2,2,2,2,2,2,2,2,2,
2,2,2,2,2,2,2,2,2,2,2,2,2,2,2,2,2,2,2,2,2,2,2,2,2,2,2,2,2,2,2,2,2,2,2,2,
2,2,2,2,2,2,2,2,2,4),(-2.66807656983836,-2.66001931216341,-2.65566187021585,
-2.65424879941531,-2.65318148796654,-2.65215122106027,-2.65097124285194,
-2.64904592064653,-2.64298004572499,-2.64169796462927,-2.63389713220412,
-2.58067129022967,-2.56294088045462,-2.55210929912035,-2.54880138677269,
-2.54671454326925,-2.5447779822075,-2.54226607056276,-2.53807319770196,
-2.50861277988315,-2.46747060755929,-2.45202922886731,-2.44661324534596,
-2.44401378375114,-2.44190666294874,-2.44069382405631,-2.44069071036685,
-2.44068757765006,-2.4406844262157,-2.44068125547413,-2.44067806521928,
-2.44067485554611,-2.44067162617671,-2.44066837713124,-2.44066510804369,
-2.440661818944,-2.44065850972164,-2.44065518013926,-2.44065184303295,-2.44064849146409,
-2.4406451186021,-2.44064172430211,-2.4406382977067,-2.43961003975432,-2.43822996682275,
-2.43536006662262,-2.40000187929051,-2.36702700814441,-2.34413886403262,
-2.33844071610385,-2.33586108299189,-2.33392114450774,-2.33209656636895,
-2.32956323339432,-2.32297765799664,-2.26661514864444,-2.24290774166351,
-2.23218005588033,-2.22994169397189,-2.22869257256167,-2.22762033104054,
-2.22626232395855,-2.22411065702757,-2.21297838061014,-2.16172584551341,
-2.13312487315829,-2.12670359206788,-2.12399675560698,-2.1220351859839,
-2.1202418436328,-2.11737390656077,-2.11047278086461,-2.05759631778182,
-2.03154060316174,-2.02019487474647,-2.01791993584475,-2.01666286978899,
-2.01559140711415,-2.01424406876241,-2.01162484057531,-1.99562716149847,
-1.99011655002598,-1.97569213356159,-1.94279678023562,-1.92622947076308,
-1.91591640674569,-1.91266704127572,-1.91059329681986,-1.90865222022573,
-1.90611052492405,-1.9018146360312,-1.86668065146954,-1.81771775944691,
-1.80800519245818,-1.80583270591349,-1.80459798537159,-1.80352389101702,
-1.80214498157591,-1.79928146642341,-1.76328492711041,-1.73052088549797,
-1.70797122228241,-1.70231844785027,-1.69974697700491,-1.69780814426694,
-1.69598091063723,-1.69343796585279,-1.68679253526116,-1.63099604229814,
-1.59810930967717,-1.59456242182821,-1.59305797213324,-1.59196642319294,
-1.59093892317369,-1.58918851509386,-1.5844091556551,-1.547236227462,-1.496959549346,
-1.49055691298743,-1.4878530639403,-1.48589188443366,-1.4840976754684,-1.48122568543685,
-1.47430099954898,-1.42172907120572,-1.40860274249303),.UNSPECIFIED.);
#1048=B_SPLINE_CURVE_WITH_KNOTS('',3,(#108180,#108181,#108182,#108183,#108184,
#108185,#108186,#108187,#108188,#108189),.UNSPECIFIED.,.F.,.F.,(4,1,1,1,
1,1,1,4),(-60.0402340848269,-59.9301869977125,-58.9313505477506,-57.9325140977887,
-56.9336776478268,-55.934841197865,-54.9360047479031,-54.1065275202913),
 .UNSPECIFIED.);
#1049=B_SPLINE_CURVE_WITH_KNOTS('',3,(#108190,#108191,#108192,#108193,#108194,
#108195,#108196,#108197,#108198,#108199,#108200,#108201,#108202,#108203,
#108204,#108205,#108206,#108207,#108208,#108209,#108210,#108211),
 .UNSPECIFIED.,.F.,.F.,(4,2,2,2,2,2,2,2,2,2,4),(-2.66761363830502,-2.64338362104628,
-2.63625165986871,-2.63446074350259,-2.63324577351584,-2.63223669094568,
-2.63116210710082,-2.62977606482891,-2.62687504598501,-2.59995451275591,
-2.59351250887444),.UNSPECIFIED.);
#1050=B_SPLINE_CURVE_WITH_KNOTS('',3,(#108216,#108217,#108218,#108219,#108220,
#108221,#108222,#108223,#108224,#108225,#108226,#108227,#108228,#108229,
#108230,#108231,#108232,#108233,#108234,#108235,#108236,#108237,#108238,
#108239,#108240,#108241,#108242,#108243,#108244,#108245,#108246,#108247,
#108248,#108249,#108250,#108251,#108252,#108253,#108254,#108255,#108256,
#108257,#108258,#108259,#108260,#108261,#108262,#108263,#108264,#108265,
#108266,#108267,#108268,#108269,#108270,#108271,#108272,#108273,#108274,
#108275,#108276,#108277,#108278,#108279,#108280,#108281,#108282,#108283,
#108284,#108285,#108286,#108287,#108288,#108289,#108290,#108291,#108292,
#108293,#108294,#108295,#108296,#108297,#108298,#108299,#108300,#108301,
#108302,#108303,#108304,#108305,#108306,#108307,#108308,#108309,#108310,
#108311,#108312,#108313,#108314,#108315,#108316,#108317,#108318,#108319,
#108320,#108321,#108322,#108323,#108324,#108325,#108326,#108327,#108328,
#108329,#108330,#108331,#108332,#108333,#108334,#108335,#108336,#108337,
#108338,#108339,#108340,#108341,#108342,#108343,#108344,#108345,#108346,
#108347,#108348,#108349,#108350,#108351,#108352,#108353,#108354,#108355,
#108356,#108357,#108358,#108359,#108360,#108361,#108362,#108363,#108364,
#108365,#108366,#108367,#108368,#108369,#108370,#108371,#108372,#108373,
#108374,#108375,#108376,#108377,#108378,#108379,#108380,#108381,#108382,
#108383,#108384,#108385,#108386,#108387,#108388,#108389,#108390,#108391,
#108392,#108393,#108394,#108395,#108396,#108397,#108398,#108399,#108400,
#108401,#108402,#108403,#108404,#108405,#108406,#108407,#108408,#108409,
#108410,#108411,#108412,#108413,#108414,#108415,#108416,#108417,#108418,
#108419,#108420,#108421,#108422,#108423,#108424,#108425,#108426,#108427,
#108428,#108429,#108430,#108431,#108432,#108433,#108434,#108435,#108436,
#108437,#108438,#108439,#108440,#108441,#108442,#108443,#108444,#108445,
#108446,#108447,#108448,#108449,#108450,#108451,#108452,#108453,#108454,
#108455,#108456,#108457),.UNSPECIFIED.,.F.,.F.,(4,2,2,2,2,2,2,2,2,2,2,2,
2,2,2,2,2,2,2,2,2,2,2,2,2,2,2,2,2,2,2,2,2,2,2,2,2,2,2,2,2,2,2,2,2,2,2,2,
2,2,2,2,2,2,2,2,2,2,2,2,2,2,2,2,2,2,2,2,2,2,2,2,2,2,2,2,2,2,2,2,2,2,2,2,
2,2,2,2,2,2,2,2,2,2,2,2,2,2,2,2,2,2,2,2,2,2,2,2,2,2,2,2,2,2,2,2,2,2,2,2,
4),(-1.4083648719342,-1.38228065803757,-1.36894127842204,-1.36538644960133,
-1.36324542445129,-1.36132425816373,-1.35888107498145,-1.35500675348651,
-1.33393386252568,-1.27612144912632,-1.26116153864079,-1.25881363304285,
-1.25741190086447,-1.25633256740672,-1.25512596347766,-1.25307993708088,
-1.24502288644303,-1.22984433276336,-1.1899497876185,-1.15890724031151,
-1.15468587745723,-1.15216604826746,-1.15022871693044,-1.14814628849906,
-1.14485652896388,-1.13418333782302,-1.11681271534813,-1.06811113144221,
-1.0615961970822,-1.04897429092784,-1.04673866878302,-1.04535530922547,
-1.04428092999729,-1.04304946623855,-1.0408911972377,-1.03137945064811,
-0.982228280512713,-0.947034266730386,-0.942738120907567,-0.940196620859603,
-0.938255882409529,-0.936182681563432,-0.932934547373618,-0.922628505026184,
-0.906077741869524,-0.873227896211311,-0.860310720820461,-0.837608632169213,
-0.834755202051013,-0.833378495829121,-0.832304867256694,-0.831069278578373,
-0.828891894387172,-0.81910213692217,-0.770194401526692,-0.735078970921858,
-0.730784261169856,-0.728243315161181,-0.726302829608377,-0.724229733925277,
-0.720981420008596,-0.710671903867421,-0.694112800822422,-0.661258068670178,
-0.647484848121893,-0.64071664199297,-0.639061302700117,-0.625189382805616,
-0.622889893585463,-0.621502516926235,-0.620425264313628,-0.619210919235713,
-0.617129322019864,-0.608635437510486,-0.592211559054857,-0.550103913138771,
-0.522873976770003,-0.518747325349785,-0.516255509253578,-0.514322830978031,
-0.512228603140846,-0.508884011407604,-0.497702379996471,-0.479164179919319,
-0.434965958872584,-0.413688344646884,-0.410871718878125,-0.409502370161695,
-0.408429535609674,-0.407189246296834,-0.40499001083307,-0.394870774261701,
-0.373313283791549,-0.363916869376676,-0.31488853818834,-0.307769058459617,
-0.304865435229307,-0.303065968954601,-0.301110552577836,-0.298435483067391,
-0.29219732858794,-0.265103892615965,-0.225442438814623,-0.201826409179347,
-0.198964970216695,-0.197586822993611,-0.19655964682314,-0.195366835491709,
-0.1933863944972,-0.190950416575893,-0.186002759025304,-0.172495020457729,
-0.150027583419131,-0.10305833797812,-0.095871369505978,-0.0929564727872435,
-0.0911549606563658,-0.0892012124947926,-0.086535416674339,-0.0803506587845703,
-0.075040891899263),.UNSPECIFIED.);
#1051=B_SPLINE_CURVE_WITH_KNOTS('',3,(#108458,#108459,#108460,#108461,#108462,
#108463,#108464,#108465,#108466,#108467,#108468,#108469,#108470,#108471,
#108472,#108473,#108474,#108475,#108476,#108477,#108478,#108479,#108480,
#108481,#108482,#108483,#108484,#108485,#108486,#108487,#108488,#108489,
#108490,#108491,#108492,#108493,#108494,#108495,#108496,#108497,#108498,
#108499,#108500,#108501,#108502,#108503,#108504,#108505,#108506,#108507,
#108508,#108509,#108510,#108511,#108512,#108513,#108514,#108515,#108516,
#108517,#108518,#108519,#108520,#108521,#108522,#108523,#108524,#108525,
#108526,#108527,#108528,#108529,#108530,#108531,#108532,#108533,#108534,
#108535,#108536,#108537,#108538,#108539,#108540,#108541,#108542,#108543,
#108544,#108545,#108546,#108547,#108548,#108549,#108550,#108551,#108552,
#108553,#108554,#108555,#108556,#108557,#108558,#108559,#108560,#108561,
#108562,#108563,#108564,#108565,#108566,#108567,#108568,#108569,#108570,
#108571,#108572,#108573,#108574,#108575,#108576,#108577,#108578,#108579,
#108580,#108581,#108582,#108583,#108584,#108585,#108586,#108587,#108588,
#108589,#108590,#108591,#108592,#108593,#108594,#108595,#108596,#108597,
#108598,#108599,#108600,#108601,#108602,#108603,#108604,#108605,#108606,
#108607,#108608,#108609,#108610,#108611,#108612,#108613,#108614,#108615,
#108616,#108617,#108618,#108619,#108620,#108621,#108622,#108623,#108624,
#108625,#108626,#108627,#108628,#108629,#108630,#108631,#108632,#108633,
#108634,#108635,#108636,#108637,#108638,#108639,#108640,#108641,#108642,
#108643,#108644,#108645,#108646,#108647,#108648,#108649,#108650,#108651,
#108652,#108653,#108654,#108655,#108656,#108657,#108658,#108659,#108660,
#108661,#108662,#108663,#108664,#108665,#108666,#108667,#108668,#108669,
#108670,#108671,#108672,#108673,#108674,#108675,#108676,#108677,#108678,
#108679,#108680,#108681,#108682,#108683,#108684,#108685),.UNSPECIFIED.,
 .F.,.F.,(4,2,2,2,2,2,2,2,2,2,2,2,2,2,2,2,2,2,2,2,2,2,2,2,2,2,2,2,2,2,2,
2,2,2,2,2,2,2,2,2,2,2,2,2,2,2,2,2,2,2,2,2,2,2,2,2,2,2,2,2,2,2,2,2,2,2,2,
2,2,2,2,2,2,2,2,2,2,2,2,2,2,2,2,2,2,2,2,2,2,2,2,2,2,2,2,2,2,2,2,2,2,2,2,
2,2,2,2,2,2,2,2,2,2,4),(-2.59351250887444,-2.58627132755899,-2.57475056578942,
-2.54617420876759,-2.5322760739487,-2.52867254583601,-2.5265206756222,-2.52460139815959,
-2.52217635843806,-2.51744459412592,-2.4800073394474,-2.42965592482369,
-2.42318153346149,-2.42129005227563,-2.42027907783809,-2.41920580512948,
-2.41783413989595,-2.41563725140815,-2.40380161873765,-2.34640696934181,
-2.32984084338238,-2.31952895204551,-2.31628018793202,-2.31420688296764,
-2.31226625687532,-2.30972520792143,-2.30543053797334,-2.27032333094732,
-2.22142962689166,-2.21165056862751,-2.20947386375746,-2.20823838682896,
-2.20716468515013,-2.20578765320441,-2.20293276527677,-2.16673537944714,
-2.13404718358941,-2.11160908086825,-2.10597201544872,-2.10340378344222,
-2.10146579932734,-2.09963819310631,-2.09709284592049,-2.09042983160154,
-2.03483734684125,-2.01063326760602,-1.99977167645199,-1.99752536847757,
-1.99627460970123,-1.99520268683062,-1.99384729454306,-1.99119018487353,
-1.97422692051994,-1.92398177534601,-1.90639237712722,-1.89562381061545,
-1.89232356372019,-1.89023888066884,-1.88830247942656,-1.8857881596038,
-1.88158552044819,-1.85136840109467,-1.79985871250863,-1.7878695760094,
-1.78555922765983,-1.78429457785566,-1.78322381824376,-1.78188641330958,
-1.77980174823529,-1.76970861435776,-1.76421760799779,-1.75679086914864,
-1.74328321183606,-1.71040117781003,-1.69384733664869,-1.6835406779019,
-1.68029227752141,-1.67821889588199,-1.67627798108125,-1.67373624105447,
-1.66943970141705,-1.63422230022242,-1.58497685489194,-1.57559915198036,
-1.5734503440178,-1.57222092170071,-1.57114614916315,-1.56975940908192,
-1.56751266758141,-1.55467956074227,-1.55251360106794,-1.50523272241264,
-1.47670828858993,-1.47029625899942,-1.46759104624969,-1.46562982511807,
-1.46383623091739,-1.46096664820263,-1.45405512645051,-1.4013235146106,
-1.37516890081238,-1.36379827027713,-1.36152196775808,-1.36026463393816,
-1.35919323748336,-1.3578463569948,-1.35522911889583,-1.33926696600732,
-1.33432291560366,-1.32867693141128,-1.28171657000092,-1.28027319717024,
-1.26123204158777,-1.25985393253769),.UNSPECIFIED.);
#1052=B_SPLINE_CURVE_WITH_KNOTS('',3,(#108691,#108692,#108693,#108694,#108695,
#108696,#108697,#108698,#108699,#108700,#108701,#108702,#108703,#108704,
#108705,#108706),.UNSPECIFIED.,.F.,.F.,(4,2,2,2,2,2,2,4),(-0.0747637516645625,
-0.0741311798278147,-0.0730589563255482,-0.0718129938420133,-0.069588043911114,
-0.0590694513428154,-0.0361125965627976,-0.000629543915810415),
 .UNSPECIFIED.);
#1053=B_SPLINE_CURVE_WITH_KNOTS('',3,(#108707,#108708,#108709,#108710,#108711,
#108712,#108713,#108714,#108715,#108716,#108717,#108718,#108719,#108720,
#108721,#108722,#108723,#108724,#108725,#108726,#108727,#108728,#108729,
#108730,#108731,#108732,#108733,#108734,#108735,#108736,#108737,#108738,
#108739,#108740,#108741,#108742,#108743,#108744,#108745,#108746,#108747,
#108748,#108749,#108750,#108751,#108752,#108753,#108754,#108755,#108756,
#108757,#108758,#108759,#108760,#108761,#108762,#108763,#108764,#108765,
#108766,#108767,#108768,#108769,#108770,#108771,#108772,#108773,#108774,
#108775,#108776,#108777,#108778,#108779,#108780,#108781,#108782,#108783,
#108784,#108785,#108786,#108787,#108788,#108789,#108790,#108791,#108792,
#108793,#108794,#108795,#108796,#108797,#108798,#108799,#108800,#108801,
#108802,#108803,#108804,#108805,#108806,#108807,#108808,#108809,#108810,
#108811,#108812,#108813,#108814,#108815,#108816,#108817,#108818,#108819,
#108820,#108821,#108822,#108823,#108824,#108825,#108826,#108827,#108828,
#108829,#108830,#108831,#108832,#108833,#108834,#108835,#108836,#108837,
#108838,#108839,#108840,#108841,#108842,#108843,#108844,#108845,#108846,
#108847,#108848,#108849,#108850,#108851,#108852,#108853,#108854,#108855,
#108856,#108857,#108858,#108859,#108860,#108861,#108862,#108863,#108864,
#108865,#108866,#108867,#108868,#108869,#108870,#108871,#108872,#108873,
#108874,#108875,#108876,#108877,#108878,#108879,#108880,#108881,#108882,
#108883,#108884,#108885,#108886,#108887,#108888,#108889,#108890,#108891,
#108892,#108893,#108894,#108895,#108896,#108897,#108898,#108899,#108900,
#108901,#108902,#108903,#108904,#108905,#108906,#108907,#108908,#108909,
#108910,#108911,#108912,#108913,#108914,#108915,#108916,#108917,#108918,
#108919,#108920,#108921,#108922,#108923,#108924,#108925,#108926,#108927,
#108928,#108929,#108930),.UNSPECIFIED.,.F.,.F.,(4,2,2,2,2,2,2,2,2,2,2,2,
2,2,2,2,2,2,2,2,2,2,2,2,2,2,2,2,2,2,2,2,2,2,2,2,2,2,2,2,2,2,2,2,2,2,2,2,
2,2,2,2,2,2,2,2,2,2,2,2,2,2,2,2,2,2,2,2,2,2,2,2,2,2,2,2,2,2,2,2,2,2,2,2,
2,2,2,2,2,2,2,2,2,2,2,2,2,2,2,2,2,2,2,2,2,2,2,2,2,2,2,4),(-2.66759551301063,
-2.64226750593368,-2.63914030665614,-2.63699407964818,-2.63519314844083,
-2.63327906761791,-2.63090974149732,-2.62727593515308,-2.61016939536854,
-2.59797798888022,-2.56928353171966,-2.54370956853474,-2.5324883834596,
-2.53022107940407,-2.52896588673696,-2.52789459429043,-2.52654565169851,
-2.52391794688924,-2.50779178616906,-2.50379742664539,-2.45804564367148,
-2.43957118040182,-2.43218401642221,-2.42665861840623,-2.42412186227216,
-2.42229832814302,-2.4204978465425,-2.41758902621197,-2.41043901546901,
-2.36229640204076,-2.32255563283699,-2.31897892562159,-2.31746972719541,
-2.3163776943593,-2.31535209834435,-2.31360998963901,-2.30888249688065,
-2.26870167715171,-2.22139730934245,-2.21500291564738,-2.21230110696522,
-2.21034088207934,-2.20854718415339,-2.20567522142932,-2.19874651514277,
-2.14629595725478,-2.11995998655112,-2.10854480352007,-2.10626638520139,
-2.10500878977185,-2.10393771956789,-2.10259194741275,-2.09997891037995,
-2.08410713777049,-2.07939135327073,-2.06407848434781,-2.03118220844407,
-2.01460696166349,-2.00429114530251,-2.00104207632652,-1.99896880056252,
-1.99702835894149,-1.99448777821134,-1.99019440755108,-1.9551640810914,
-1.90649186167509,-1.89645175727684,-1.89425760298284,-1.89301834784435,
-1.89194525309181,-1.890574062135,-1.88837840748431,-1.87655871576081,-1.87290461442835,
-1.87267890003012,-1.8658133562767,-1.85208116146166,-1.81920064391645,
-1.80264597048692,-1.79233926071727,-1.78909109291391,-1.78701791948844,
-1.78507724158568,-1.78253587237868,-1.77824009539095,-1.74304764195883,
-1.69387979804871,-1.68442083645631,-1.68226640823787,-1.68103583442675,
-1.67996139388663,-1.67857684341219,-1.6756835246681,-1.6496508754464,-1.61148605333721,
-1.58245989248429,-1.57806455212859,-1.57574112333995,-1.57382963546072,
-1.57160564939747,-1.56777763010058,-1.5527172196965,-1.50055201496992,
-1.48170759679173,-1.47241233146421,-1.47026956557208,-1.46904153158635,
-1.4679666243447,-1.46657793108343,-1.46366349277898,-1.43361917560424,
-1.4083648719342),.UNSPECIFIED.);
#1054=B_SPLINE_CURVE_WITH_KNOTS('',3,(#108932,#108933,#108934,#108935,#108936,
#108937,#108938,#108939,#108940,#108941,#108942,#108943,#108944,#108945,
#108946,#108947,#108948,#108949,#108950,#108951,#108952,#108953,#108954,
#108955,#108956,#108957,#108958,#108959,#108960,#108961,#108962,#108963,
#108964,#108965,#108966,#108967,#108968,#108969,#108970,#108971,#108972,
#108973,#108974,#108975,#108976,#108977,#108978,#108979,#108980,#108981,
#108982,#108983,#108984,#108985,#108986,#108987,#108988,#108989,#108990,
#108991,#108992,#108993,#108994,#108995,#108996,#108997,#108998,#108999,
#109000,#109001,#109002,#109003,#109004,#109005,#109006,#109007,#109008,
#109009,#109010,#109011,#109012,#109013,#109014,#109015,#109016,#109017,
#109018,#109019,#109020,#109021,#109022,#109023,#109024,#109025,#109026,
#109027,#109028,#109029,#109030,#109031,#109032,#109033,#109034,#109035,
#109036,#109037,#109038,#109039,#109040,#109041,#109042,#109043,#109044,
#109045,#109046,#109047,#109048,#109049,#109050,#109051,#109052,#109053,
#109054,#109055,#109056,#109057,#109058,#109059,#109060,#109061,#109062,
#109063,#109064,#109065,#109066,#109067,#109068,#109069,#109070,#109071,
#109072,#109073,#109074,#109075,#109076,#109077,#109078,#109079,#109080,
#109081,#109082,#109083,#109084,#109085,#109086,#109087,#109088,#109089,
#109090,#109091,#109092,#109093,#109094,#109095,#109096,#109097,#109098,
#109099,#109100,#109101,#109102,#109103,#109104,#109105,#109106,#109107,
#109108,#109109,#109110,#109111,#109112,#109113,#109114,#109115,#109116,
#109117,#109118,#109119,#109120,#109121,#109122,#109123,#109124,#109125,
#109126,#109127,#109128,#109129,#109130,#109131,#109132,#109133,#109134,
#109135,#109136,#109137,#109138,#109139,#109140,#109141),.UNSPECIFIED.,
 .F.,.F.,(4,2,2,2,2,2,2,2,2,2,2,2,2,2,2,2,2,2,2,2,2,2,2,2,2,2,2,2,2,2,2,
2,2,2,2,2,2,2,2,2,2,2,2,2,2,2,2,2,2,2,2,2,2,2,2,2,2,2,2,2,2,2,2,2,2,2,2,
2,2,2,2,2,2,2,2,2,2,2,2,2,2,2,2,2,2,2,2,2,2,2,2,2,2,2,2,2,2,2,2,2,2,2,2,
2,4),(-1.25985393253769,-1.25747070720351,-1.25506188878625,-1.25314411303961,
-1.25098192113377,-1.24733218977863,-1.23288110106248,-1.1824923785715,
-1.15282398413172,-1.14990946594436,-1.14852068833715,-1.14744569067698,
-1.14621753456537,-1.14407449709132,-1.13477745367465,-1.11592580221188,
-1.07547219421632,-1.06319339210751,-1.04861346996789,-1.04482746231387,
-1.0426129887951,-1.04070068330876,-1.03836497855085,-1.03391186143486,
-1.00287554189128,-0.954897516395568,-0.940308393613797,-0.937976016854732,
-0.936578767727052,-0.935499963058658,-0.934290692063161,-0.932232960337385,
-0.924037466166763,-0.908471121932689,-0.866887193211196,-0.83798284483716,
-0.833811357428992,-0.831306000739872,-0.829370800318638,-0.827281764971649,
-0.823962535307346,-0.813022830397436,-0.795046075348513,-0.744623015337069,
-0.728417150603735,-0.725789275347843,-0.724440079623504,-0.723368498715762,
-0.722112872809143,-0.719844534118631,-0.70861366263376,-0.683004469102693,
-0.629442223705916,-0.622592174645762,-0.619732650444161,-0.617940844231113,
-0.615977959971502,-0.613263798639319,-0.606798928859718,-0.552723562412723,
-0.516660360537288,-0.513800649203694,-0.512422547116781,-0.51134859757237,
-0.510113505817779,-0.507939068487506,-0.498196788353505,-0.449237575063062,
-0.414102805498129,-0.409806352309035,-0.407264642758628,-0.405323728394954,
-0.403250324181468,-0.400001839122923,-0.389694411770858,-0.373141166049173,
-0.340287485000375,-0.327284836256106,-0.304664024465874,-0.301812373959264,
-0.30043594147997,-0.299362251126977,-0.298126280334976,-0.295947477759373,
-0.286138962867638,-0.237241698828617,-0.202131567173052,-0.197834504628224,
-0.195292756173294,-0.193351997241082,-0.191344263162471,-0.188242470093938,
-0.184615851054495,-0.177819649992327,-0.161438223436073,-0.128729467479277,
-0.0927003709452161,-0.0898402865255275,-0.0884622746523991,-0.0873885221057937,
-0.086153799858813,-0.0839803544989066,-0.0742481400092202,-0.0252918468826534,
-0.000629465204745831),.UNSPECIFIED.);
#1055=B_SPLINE_CURVE_WITH_KNOTS('',3,(#109142,#109143,#109144,#109145,#109146,
#109147,#109148,#109149,#109150,#109151,#109152,#109153,#109154,#109155,
#109156,#109157,#109158,#109159,#109160,#109161,#109162,#109163),
 .UNSPECIFIED.,.F.,.F.,(4,2,2,2,2,2,2,2,2,2,4),(-2.66786964950218,-2.66007560444753,
-2.65477901912715,-2.65233557188793,-2.65045366453286,-2.64861290556403,
-2.64678645097458,-2.644245988198,-2.63905467741707,-2.62654410744952,-2.59345435029626),
 .UNSPECIFIED.);
#1056=B_SPLINE_CURVE_WITH_KNOTS('',3,(#109168,#109169,#109170,#109171,#109172,
#109173,#109174,#109175,#109176,#109177,#109178,#109179,#109180,#109181,
#109182,#109183,#109184,#109185,#109186,#109187,#109188,#109189,#109190,
#109191,#109192,#109193,#109194,#109195,#109196,#109197,#109198,#109199,
#109200,#109201,#109202,#109203,#109204,#109205,#109206,#109207,#109208,
#109209,#109210,#109211,#109212,#109213,#109214,#109215,#109216,#109217,
#109218,#109219,#109220,#109221,#109222,#109223,#109224,#109225,#109226,
#109227,#109228,#109229,#109230,#109231,#109232,#109233,#109234,#109235,
#109236,#109237,#109238,#109239,#109240,#109241,#109242,#109243,#109244,
#109245,#109246,#109247,#109248,#109249,#109250,#109251,#109252,#109253,
#109254,#109255,#109256,#109257,#109258,#109259,#109260,#109261,#109262,
#109263,#109264,#109265,#109266,#109267,#109268,#109269,#109270,#109271,
#109272,#109273,#109274,#109275,#109276,#109277,#109278,#109279,#109280,
#109281,#109282,#109283,#109284,#109285,#109286,#109287,#109288,#109289,
#109290,#109291,#109292,#109293,#109294,#109295,#109296,#109297,#109298,
#109299,#109300,#109301,#109302,#109303,#109304,#109305,#109306,#109307,
#109308,#109309,#109310,#109311,#109312,#109313,#109314,#109315,#109316,
#109317,#109318,#109319,#109320,#109321,#109322,#109323,#109324,#109325,
#109326,#109327,#109328,#109329,#109330,#109331,#109332,#109333,#109334,
#109335,#109336,#109337,#109338,#109339,#109340,#109341,#109342,#109343,
#109344,#109345,#109346,#109347,#109348,#109349,#109350,#109351,#109352,
#109353,#109354,#109355,#109356,#109357,#109358,#109359,#109360,#109361,
#109362,#109363,#109364,#109365,#109366,#109367,#109368,#109369,#109370,
#109371,#109372,#109373,#109374,#109375,#109376,#109377,#109378,#109379,
#109380,#109381,#109382,#109383,#109384,#109385,#109386,#109387,#109388,
#109389),.UNSPECIFIED.,.F.,.F.,(4,2,2,2,2,2,2,2,2,2,2,2,2,2,2,2,2,2,2,2,
2,2,2,2,2,2,2,2,2,2,2,2,2,2,2,2,2,2,2,2,2,2,2,2,2,2,2,2,2,2,2,2,2,2,2,2,
2,2,2,2,2,2,2,2,2,2,2,2,2,2,2,2,2,2,2,2,2,2,2,2,2,2,2,2,2,2,2,2,2,2,2,2,
2,2,2,2,2,2,2,2,2,2,2,2,2,2,2,2,2,2,4),(-1.40846183573222,-1.36760935404396,
-1.35571677711112,-1.35118168056498,-1.34787326581396,-1.34641078032389,
-1.34532607541812,-1.34413718509467,-1.34217123533643,-1.3357661173238,
-1.33421020789535,-1.31962364758894,-1.26058204198727,-1.2462723306543,
-1.24251063948406,-1.24030180412614,-1.23838914703816,-1.23604641789166,
-1.23155948648072,-1.19919773828322,-1.15901433858493,-1.15408223932826,
-1.13813289937514,-1.13551637136099,-1.13416965978534,-1.13309829372798,
-1.13184088067692,-1.12956413170179,-1.11818557546823,-1.09199672936701,
-1.03927343228281,-1.03235893398958,-1.02948889894336,-1.02769525263767,
-1.02573416548043,-1.02302947935368,-1.01662029543279,-0.988122866940365,
-0.937198879267705,-0.925708217044988,-0.923535237783938,-0.922170811223976,
-0.921098151255365,-0.919853862467044,-0.917637262802063,-0.907255704932003,
-0.884789000923542,-0.826431098724289,-0.820077957807639,-0.817582871117166,
-0.815768411894293,-0.813822913967139,-0.811207586020978,-0.805311225420001,
-0.780924288888288,-0.730257961845517,-0.714076099833773,-0.711449426175511,
-0.710100583030828,-0.709029143525843,-0.707773522827226,-0.705504786963308,
-0.694263711462023,-0.668612691125667,-0.615121987936699,-0.608267484558596,
-0.605407434595423,-0.603615686178932,-0.601653177388932,-0.598940109306859,
-0.592480579174513,-0.538568124541575,-0.502338026817227,-0.499484232452788,
-0.498107390003983,-0.497033673778689,-0.4957980052161,-0.493620530506494,
-0.48383119987943,-0.434918575917131,-0.399786768537606,-0.395499121893788,
-0.392960120996656,-0.391019833082001,-0.388945698678438,-0.385693144596759,
-0.375348089202393,-0.358710841954113,-0.325789830865112,-0.307668578930956,
-0.290154298854215,-0.287477419144722,-0.286117904090707,-0.285045790411848,
-0.283798336677043,-0.281566718793299,-0.270942331211855,-0.247604880567332,
-0.191930349490594,-0.184492974251068,-0.181535148185156,-0.179725544233453,
-0.177896185303057,-0.175387108746966,-0.17004163193405,-0.162936255911303,
-0.1454735968787,-0.0959607259706829,-0.0781787445690996,-0.0754926276015686,
-0.0747637516645625),.UNSPECIFIED.);
#1057=B_SPLINE_CURVE_WITH_KNOTS('',3,(#109390,#109391,#109392,#109393,#109394,
#109395,#109396,#109397,#109398,#109399,#109400,#109401,#109402,#109403,
#109404,#109405,#109406,#109407,#109408,#109409,#109410,#109411,#109412,
#109413,#109414,#109415,#109416,#109417,#109418,#109419,#109420,#109421,
#109422,#109423,#109424,#109425,#109426,#109427,#109428,#109429,#109430,
#109431,#109432,#109433,#109434,#109435,#109436,#109437,#109438,#109439,
#109440,#109441,#109442,#109443,#109444,#109445,#109446,#109447,#109448,
#109449,#109450,#109451,#109452,#109453,#109454,#109455,#109456,#109457,
#109458,#109459,#109460,#109461,#109462,#109463,#109464,#109465,#109466,
#109467,#109468,#109469,#109470,#109471,#109472,#109473,#109474,#109475,
#109476,#109477,#109478,#109479,#109480,#109481,#109482,#109483,#109484,
#109485,#109486,#109487,#109488,#109489,#109490,#109491,#109492,#109493,
#109494,#109495,#109496,#109497,#109498,#109499,#109500,#109501,#109502,
#109503,#109504,#109505,#109506,#109507,#109508,#109509,#109510,#109511,
#109512,#109513,#109514,#109515,#109516,#109517,#109518,#109519,#109520,
#109521,#109522,#109523,#109524,#109525,#109526,#109527,#109528,#109529,
#109530,#109531,#109532,#109533,#109534,#109535,#109536,#109537,#109538,
#109539,#109540,#109541,#109542,#109543,#109544,#109545,#109546,#109547,
#109548,#109549,#109550,#109551,#109552,#109553,#109554,#109555,#109556,
#109557,#109558,#109559,#109560,#109561,#109562,#109563,#109564,#109565,
#109566,#109567,#109568,#109569,#109570,#109571,#109572,#109573,#109574,
#109575,#109576,#109577,#109578,#109579,#109580,#109581,#109582,#109583,
#109584,#109585,#109586,#109587,#109588,#109589,#109590,#109591,#109592,
#109593,#109594,#109595,#109596,#109597,#109598,#109599,#109600,#109601,
#109602,#109603,#109604,#109605,#109606,#109607,#109608,#109609,#109610,
#109611,#109612,#109613,#109614,#109615,#109616,#109617,#109618,#109619,
#109620,#109621,#109622,#109623,#109624,#109625,#109626,#109627,#109628,
#109629,#109630,#109631,#109632,#109633,#109634,#109635,#109636,#109637,
#109638,#109639,#109640,#109641,#109642,#109643,#109644,#109645,#109646,
#109647,#109648,#109649,#109650,#109651,#109652,#109653,#109654,#109655,
#109656,#109657,#109658,#109659),.UNSPECIFIED.,.F.,.F.,(4,2,2,2,2,2,2,2,
2,2,2,2,2,2,2,2,2,2,2,2,2,2,2,2,2,2,2,2,2,2,2,2,2,2,2,2,2,2,2,2,2,2,2,2,
2,2,2,2,2,2,2,2,2,2,2,2,2,2,2,2,2,2,2,2,2,2,2,2,2,2,2,2,2,2,2,2,2,2,2,2,
2,2,2,2,2,2,2,2,2,2,2,2,2,2,2,2,2,2,2,2,2,2,2,2,2,2,2,2,2,2,2,2,2,2,2,2,
2,2,2,2,2,2,2,2,2,2,2,2,2,2,2,2,2,2,4),(-2.59345435029626,-2.57487343302133,
-2.55603054349818,-2.54673538719394,-2.54459246186581,-2.54336430675748,
-2.54228927408724,-2.54090039316212,-2.53798547053879,-2.50828829265839,
-2.45783806134818,-2.448348849042,-2.44374148092713,-2.43996230701688,-2.43779156057653,
-2.43777586588201,-2.4377596186006,-2.43774279865574,-2.43772538517487,
-2.43770735653761,-2.4376886903526,-2.43766936342921,-2.43764935173658,
-2.43762863030754,-2.43760717336548,-2.43758495418478,-2.43756194437979,
-2.4375419078355,-2.43751855724927,-2.43749135053028,-2.43745965963862,
-2.43742275825009,-2.43737980810024,-2.43732559577303,-2.43538484296361,
-2.4328427911657,-2.42854454965186,-2.39342281925613,-2.34446396997995,
-2.33476354132117,-2.33259226802617,-2.33135800420501,-2.33028415775527,
-2.32890537102029,-2.32604143566114,-2.29008480882023,-2.25731885641484,
-2.23475907357195,-2.2291055815852,-2.22653436290148,-2.22459595571837,
-2.22276929615355,-2.22022742796077,-2.21358646657787,-2.15778055934402,
-2.13371804059057,-2.12289465798696,-2.12065069774379,-2.11940046807973,
-2.1183285190827,-2.1169724785515,-2.11482692102098,-2.103790203029,-2.05257229344681,
-2.02386280264726,-2.01742903107829,-2.01472032560763,-2.01275863406502,
-2.01096602804043,-2.0081011128712,-2.0012168098453,-1.94814075254518,-1.92223332524728,
-1.91092603288176,-1.9086535387874,-1.90739711624071,-1.90632577261868,
-1.9049780372029,-1.9023564291846,-1.88631425680576,-1.88102344571043,-1.86643879725074,
-1.83354645597647,-1.81697937446422,-1.80666682974584,-1.8034178286264,
-1.80134436492348,-1.79940358499364,-1.79686232702021,-1.79256728680515,
-1.75745480157287,-1.70854954716936,-1.69877886429716,-1.69660261330852,
-1.69536717676263,-1.6942933711541,-1.69291602419614,-1.69005985817146,
-1.6672595939259,-1.61165016670609,-1.59563848503265,-1.59186896715905,
-1.58968046471779,-1.58776623391067,-1.58539691891518,-1.5817634981857,
-1.564666135491,-1.5565973928003,-1.52178644924782,-1.49773633287172,-1.48691654931937,
-1.48467289985831,-1.48342278231305,-1.48235089181459,-1.48099487700528,
-1.47833455998944,-1.46128086936533,-1.44266851361881,-1.4097118208564,
-1.39306633846209,-1.38271848467888,-1.37946551532565,-1.37739123382153,
-1.3754508914063,-1.37291194014815,-1.3686246799394,-1.33404296401158,-1.27807638839781,
-1.27380249806267,-1.27213089678816,-1.27111885272133,-1.27001650027444,
-1.26845155766493,-1.26453897460501,-1.25988555695749),.UNSPECIFIED.);
#1058=B_SPLINE_CURVE_WITH_KNOTS('',3,(#109665,#109666,#109667,#109668,#109669,
#109670,#109671,#109672,#109673,#109674,#109675,#109676,#109677,#109678,
#109679,#109680,#109681,#109682),.UNSPECIFIED.,.F.,.F.,(4,2,2,2,2,2,2,2,
4),(-0.0751187269598587,-0.0651105008529126,-0.0603738607500047,-0.057948073480137,
-0.0560290632015776,-0.0538783934967688,-0.0516516909504345,-0.0483298717746776,
-0.000628983924256894),.UNSPECIFIED.);
#1059=B_SPLINE_CURVE_WITH_KNOTS('',3,(#109683,#109684,#109685,#109686,#109687,
#109688,#109689,#109690,#109691,#109692,#109693,#109694,#109695,#109696,
#109697,#109698,#109699,#109700,#109701,#109702,#109703,#109704,#109705,
#109706,#109707,#109708,#109709,#109710,#109711,#109712,#109713,#109714,
#109715,#109716,#109717,#109718,#109719,#109720,#109721,#109722,#109723,
#109724,#109725,#109726,#109727,#109728,#109729,#109730,#109731,#109732,
#109733,#109734,#109735,#109736,#109737,#109738,#109739,#109740,#109741,
#109742,#109743,#109744,#109745,#109746,#109747,#109748,#109749,#109750,
#109751,#109752,#109753,#109754,#109755,#109756,#109757,#109758,#109759,
#109760,#109761,#109762,#109763,#109764,#109765,#109766,#109767,#109768,
#109769,#109770,#109771,#109772,#109773,#109774,#109775,#109776,#109777,
#109778,#109779,#109780,#109781,#109782,#109783,#109784,#109785,#109786,
#109787,#109788,#109789,#109790,#109791,#109792,#109793,#109794,#109795,
#109796,#109797,#109798,#109799,#109800,#109801,#109802,#109803,#109804,
#109805,#109806,#109807,#109808,#109809,#109810,#109811,#109812,#109813,
#109814,#109815,#109816,#109817,#109818,#109819,#109820,#109821,#109822,
#109823,#109824,#109825,#109826,#109827,#109828,#109829,#109830,#109831,
#109832,#109833,#109834,#109835,#109836,#109837,#109838,#109839,#109840,
#109841,#109842,#109843,#109844,#109845,#109846,#109847,#109848,#109849,
#109850,#109851,#109852,#109853,#109854,#109855,#109856,#109857,#109858,
#109859,#109860,#109861,#109862,#109863,#109864,#109865,#109866,#109867,
#109868,#109869,#109870,#109871,#109872,#109873,#109874,#109875,#109876,
#109877,#109878,#109879,#109880,#109881,#109882,#109883,#109884,#109885,
#109886,#109887,#109888,#109889,#109890,#109891,#109892,#109893,#109894,
#109895,#109896,#109897,#109898,#109899,#109900,#109901,#109902,#109903,
#109904,#109905,#109906,#109907,#109908,#109909,#109910),.UNSPECIFIED.,
 .F.,.F.,(4,2,2,2,2,2,2,2,2,2,2,2,2,2,2,2,2,2,2,2,2,2,2,2,2,2,2,2,2,2,2,
2,2,2,2,2,2,2,2,2,2,2,2,2,2,2,2,2,2,2,2,2,2,2,2,2,2,2,2,2,2,2,2,2,2,2,2,
2,2,2,2,2,2,2,2,2,2,2,2,2,2,2,2,2,2,2,2,2,2,2,2,2,2,2,2,2,2,2,2,2,2,2,2,
2,2,2,2,2,2,2,2,2,2,4),(-2.66766695993853,-2.62471357151963,-2.62177987548942,
-2.62009725320902,-2.61859242480639,-2.61750086530987,-2.61647356640042,
-2.61472395506007,-2.60994937627041,-2.57250172672594,-2.55111738233075,
-2.52297782877626,-2.51633382567163,-2.51419350871687,-2.51210259779417,
-2.51016781385845,-2.50766602902802,-2.50350712852976,-2.47508598865391,
-2.44452441819042,-2.42045245241616,-2.40964062699257,-2.40740758394692,
-2.4061496438327,-2.40507822136512,-2.40373193197073,-2.40111767193013,
-2.38522589855565,-2.38061496893986,-2.332214992904,-2.3156705597439,-2.30540677793349,
-2.30223450532698,-2.30013654154442,-2.29820421266851,-2.29571814072694,
-2.29161244469763,-2.26523392152814,-2.21006137226532,-2.19772551770827,
-2.1953966964881,-2.19412793620628,-2.19305724478535,-2.19172438264602,
-2.18965484953988,-2.17978309477761,-2.17405469228903,-2.16659958338089,
-2.16525949738652,-2.12103637417534,-2.09759236277211,-2.09181977710513,
-2.08922645996908,-2.08728424122182,-2.08546334837626,-2.08294440099943,
-2.07644869911415,-2.01926568033057,-2.01353564816784,-1.99465320548339,
-1.98534514768651,-1.98320113692008,-1.98197266386553,-1.98089755124883,
-1.97950882881032,-1.97659516278302,-1.94769410723579,-1.91155771415965,
-1.89277977092843,-1.88149522970752,-1.87813877271382,-1.87604132388002,
-1.87410852573285,-1.8716205354189,-1.86750883815242,-1.84091458245761,
-1.79877356684269,-1.78189820759751,-1.77324820062156,-1.77115367064405,
-1.76993613341275,-1.7688589834256,-1.76747550605699,-1.76519026255414,
-1.75159291516044,-1.74979364095306,-1.70242181693978,-1.6714466509955,
-1.66699463761633,-1.66465901159815,-1.66274651804397,-1.66053154277795,
-1.65674398699093,-1.64214946712625,-1.62988390412784,-1.58947273110877,
-1.5706189598816,-1.56132013229282,-1.5591768459171,-1.55794856209121,-1.55687346777172,
-1.55548457454187,-1.55256986386833,-1.52373234564028,-1.48562133855473,
-1.46809570978883,-1.4573545763476,-1.45405689616496,-1.45197248113065,
-1.45003539428428,-1.44751885764649,-1.44330959396303,-1.41283498024576,
-1.40846183573222),.UNSPECIFIED.);
#1060=B_SPLINE_CURVE_WITH_KNOTS('',3,(#109912,#109913,#109914,#109915,#109916,
#109917,#109918,#109919,#109920,#109921,#109922,#109923,#109924,#109925,
#109926,#109927,#109928,#109929,#109930,#109931,#109932,#109933,#109934,
#109935,#109936,#109937,#109938,#109939,#109940,#109941,#109942,#109943,
#109944,#109945,#109946,#109947,#109948,#109949,#109950,#109951,#109952,
#109953,#109954,#109955,#109956,#109957,#109958,#109959,#109960,#109961,
#109962,#109963,#109964,#109965,#109966,#109967,#109968,#109969,#109970,
#109971,#109972,#109973,#109974,#109975,#109976,#109977,#109978,#109979,
#109980,#109981,#109982,#109983,#109984,#109985,#109986,#109987,#109988,
#109989,#109990,#109991,#109992,#109993,#109994,#109995,#109996,#109997,
#109998,#109999,#110000,#110001,#110002,#110003,#110004,#110005,#110006,
#110007,#110008,#110009,#110010,#110011,#110012,#110013,#110014,#110015,
#110016,#110017,#110018,#110019,#110020,#110021,#110022,#110023,#110024,
#110025,#110026,#110027,#110028,#110029,#110030,#110031,#110032,#110033,
#110034,#110035,#110036,#110037,#110038,#110039,#110040,#110041,#110042,
#110043,#110044,#110045,#110046,#110047,#110048,#110049,#110050,#110051,
#110052,#110053,#110054,#110055,#110056,#110057,#110058,#110059,#110060,
#110061,#110062,#110063,#110064,#110065,#110066,#110067,#110068,#110069,
#110070,#110071,#110072,#110073,#110074,#110075,#110076,#110077,#110078,
#110079,#110080,#110081,#110082,#110083,#110084,#110085,#110086,#110087,
#110088,#110089,#110090,#110091,#110092,#110093,#110094,#110095,#110096,
#110097,#110098,#110099,#110100,#110101,#110102,#110103,#110104,#110105,
#110106,#110107,#110108,#110109,#110110,#110111,#110112,#110113,#110114,
#110115,#110116,#110117,#110118,#110119,#110120,#110121,#110122,#110123,
#110124,#110125,#110126,#110127,#110128,#110129,#110130,#110131,#110132,
#110133,#110134,#110135,#110136,#110137,#110138,#110139,#110140,#110141,
#110142,#110143,#110144,#110145,#110146,#110147,#110148,#110149,#110150,
#110151,#110152,#110153,#110154,#110155,#110156,#110157,#110158,#110159,
#110160,#110161,#110162,#110163,#110164,#110165,#110166,#110167),
 .UNSPECIFIED.,.F.,.F.,(4,2,2,2,2,2,2,2,2,2,2,2,2,2,2,2,2,2,2,2,2,2,2,2,
2,2,2,2,2,2,2,2,2,2,2,2,2,2,2,2,2,2,2,2,2,2,2,2,2,2,2,2,2,2,2,2,2,2,2,2,
2,2,2,2,2,2,2,2,2,2,2,2,2,2,2,2,2,2,2,2,2,2,2,2,2,2,2,2,2,2,2,2,2,2,2,2,
2,2,2,2,2,2,2,2,2,2,2,2,2,2,2,2,2,2,2,2,2,2,2,2,2,2,2,2,2,2,2,4),(-1.25988555695749,
-1.24532638527379,-1.18895160322942,-1.17210635115282,-1.16848959436862,
-1.16612546470395,-1.16421164300566,-1.1620194592878,-1.15823310554555,
-1.14198618534886,-1.08451057375482,-1.07953846025835,-1.06355310283422,
-1.06093472943854,-1.0595876590446,-1.05851631858572,-1.05725929627782,
-1.05498417256997,-1.04363264697203,-1.01754955677824,-0.964679565391793,
-0.957776503627436,-0.954908435567873,-0.953115209880324,-0.951153933219339,
-0.948447796236104,-0.942029554150818,-0.913455071828924,-0.862260476417587,
-0.851097438988294,-0.848944131514223,-0.847585723903216,-0.846513593116859,
-0.845265097591007,-0.843029080127315,-0.832336174459459,-0.808751048046474,
-0.752171282267619,-0.745607594149311,-0.743077980625541,-0.741254558118842,
-0.739314439323958,-0.736732147990228,-0.73101815388237,-0.708011594626844,
-0.674988410250267,-0.653838201291532,-0.6394335828407,-0.637109688979565,
-0.635715078715253,-0.634636814177033,-0.633426476253124,-0.631363222198257,
-0.623097286303419,-0.607329663075481,-0.565247540525825,-0.537107798038922,
-0.532957134485539,-0.53045815685201,-0.528524264249283,-0.526433043031681,
-0.523102592125976,-0.512054873399786,-0.493827900162138,-0.444883046408736,
-0.427669885066384,-0.425003850105975,-0.423646647400107,-0.422574708937565,
-0.421325565883563,-0.419086221032513,-0.408336392100513,-0.384541072611784,
-0.328294934455361,-0.32169691908426,-0.319161979739908,-0.317337273738358,
-0.315398148959251,-0.312821212149841,-0.307135635914288,-0.284338654622944,
-0.233331782369013,-0.231142533946231,-0.215562932255187,-0.212983041122076,
-0.211659059758323,-0.210638858375426,-0.210630841871536,-0.21062299470742,
-0.210615306447954,-0.210607767556776,-0.210600369080208,-0.21059310271116,
-0.210585960810013,-0.210578936212478,-0.210572022261058,-0.210565212726491,
-0.210558501849934,-0.210551884105566,-0.210545354392377,-0.21053890772416,
-0.210532539685671,-0.210526245983347,-0.210520022512278,-0.210513865397359,
-0.21050777101508,-0.210501735916263,-0.210495756758664,-0.21048983061208,
-0.210483954282331,-0.210478124871857,-0.209215188219218,-0.206828581169588,
-0.193289889053911,-0.157226498309435,-0.113379973391436,-0.109095331437991,
-0.106557349953289,-0.104617402728217,-0.102543206822558,-0.099289665684863,
-0.0889339236456346,-0.0722722792900259,-0.041786616349719,-0.00539386482498733,
-0.00193475652062522,-0.000864055931841007,-0.000629064156325977),
 .UNSPECIFIED.);
#1061=B_SPLINE_CURVE_WITH_KNOTS('',3,(#110168,#110169,#110170,#110171,#110172,
#110173,#110174,#110175,#110176,#110177,#110178,#110179,#110180,#110181,
#110182,#110183),.UNSPECIFIED.,.F.,.F.,(4,3,3,3,3,4),(-28.973780262141,
-28.9662570488944,-28.8628842312382,-28.7596459043713,-28.6565264336345,
-28.6232428877577),.UNSPECIFIED.);
#1062=B_SPLINE_CURVE_WITH_KNOTS('',3,(#110188,#110189,#110190,#110191,#110192,
#110193,#110194,#110195,#110196,#110197,#110198,#110199,#110200,#110201,
#110202,#110203,#110204,#110205,#110206,#110207,#110208,#110209,#110210,
#110211,#110212,#110213,#110214,#110215,#110216,#110217,#110218,#110219,
#110220,#110221,#110222,#110223,#110224,#110225,#110226,#110227,#110228,
#110229,#110230,#110231,#110232,#110233,#110234,#110235,#110236,#110237,
#110238,#110239,#110240,#110241,#110242,#110243,#110244,#110245,#110246,
#110247,#110248,#110249,#110250,#110251,#110252,#110253,#110254,#110255,
#110256,#110257,#110258,#110259,#110260,#110261,#110262,#110263,#110264,
#110265,#110266,#110267,#110268,#110269,#110270,#110271,#110272,#110273,
#110274,#110275,#110276,#110277,#110278,#110279,#110280,#110281,#110282,
#110283,#110284,#110285,#110286,#110287,#110288,#110289,#110290,#110291,
#110292,#110293,#110294,#110295,#110296,#110297,#110298,#110299,#110300,
#110301,#110302,#110303,#110304,#110305,#110306,#110307,#110308,#110309,
#110310,#110311,#110312,#110313,#110314,#110315,#110316,#110317,#110318,
#110319,#110320,#110321,#110322,#110323,#110324,#110325,#110326,#110327,
#110328,#110329,#110330,#110331,#110332,#110333,#110334,#110335,#110336,
#110337,#110338,#110339,#110340,#110341,#110342,#110343,#110344,#110345,
#110346,#110347,#110348,#110349,#110350,#110351,#110352,#110353,#110354,
#110355,#110356,#110357,#110358,#110359,#110360,#110361,#110362,#110363,
#110364,#110365,#110366,#110367,#110368,#110369,#110370,#110371,#110372,
#110373,#110374,#110375,#110376,#110377,#110378,#110379,#110380,#110381,
#110382,#110383,#110384,#110385,#110386,#110387,#110388,#110389,#110390,
#110391,#110392,#110393,#110394,#110395,#110396,#110397,#110398,#110399,
#110400,#110401,#110402,#110403,#110404,#110405,#110406,#110407,#110408,
#110409,#110410,#110411,#110412,#110413,#110414,#110415,#110416,#110417),
 .UNSPECIFIED.,.F.,.F.,(4,2,2,2,2,2,2,2,2,2,2,2,2,2,2,2,2,2,2,2,2,2,2,2,
2,2,2,2,2,2,2,2,2,2,2,2,2,2,2,2,2,2,2,2,2,2,2,2,2,2,2,2,2,2,2,2,2,2,2,2,
2,2,2,2,2,2,2,2,2,2,2,2,2,2,2,2,2,2,2,2,2,2,2,2,2,2,2,2,2,2,2,2,2,2,2,2,
2,2,2,2,2,2,2,2,2,2,2,2,2,2,2,2,2,2,4),(-1.40849963608456,-1.36250086534813,
-1.34494541177015,-1.33419124570262,-1.33089220484147,-1.32880754118493,
-1.32687064546567,-1.32431146871617,-1.31872496522311,-1.31130161884544,
-1.29270004945226,-1.24997196002806,-1.22734421722922,-1.22449209291687,
-1.22311545919613,-1.22204162478914,-1.22080550277749,-1.21862646861658,
-1.20881749322397,-1.15991304437755,-1.12479441280277,-1.12049879708814,
-1.11795729616835,-1.11601637595224,-1.1139428053469,-1.11069372524074,
-1.10038159156822,-1.08381810755195,-1.05095542944343,-1.03712730217916,
-1.0304779110454,-1.015004310628,-1.01240725994416,-1.01106477504636,-1.009993699204,
-1.00873305094366,-1.00644128609784,-0.994794933060641,-0.967529635336812,
-0.94734520946427,-0.91283762636,-0.908551009330935,-0.906012141320413,
-0.904071679935995,-0.901997093043025,-0.898743270755462,-0.888389449269371,
-0.871733584457522,-0.83879471098802,-0.820070761551213,-0.803158031315011,
-0.800502885531302,-0.799147913410304,-0.798076020379622,-0.796824954757866,
-0.794577229742132,-0.783692553638892,-0.759399756619677,-0.703899136882833,
-0.697223955902817,-0.6946767164775,-0.692848614562407,-0.690910896837158,
-0.688344354483421,-0.682716407593117,-0.675222993875717,-0.656363960129019,
-0.626392479024081,-0.604467361698181,-0.590931231729453,-0.58864953436849,
-0.587267326295838,-0.586190619468233,-0.584972979309737,-0.582876886936892,
-0.574201278309242,-0.55724515214131,-0.515316336921049,-0.488613915676676,
-0.484500237825154,-0.482012098258073,-0.480079798313352,-0.477983504499995,
-0.47463023154339,-0.463368913111905,-0.444645514487062,-0.416442756046856,
-0.379487469877617,-0.376649028657838,-0.375275309310357,-0.374202004849005,
-0.372964519233759,-0.370778337042213,-0.361231512847888,-0.312154875908352,
-0.276986654722135,-0.272691439467162,-0.270150410452519,-0.268209985932634,
-0.266137076081078,-0.262889305186038,-0.252778852228058,-0.236574643820261,
-0.198328907679375,-0.167652335660903,-0.164739947093335,-0.163351838761409,
-0.162277200155732,-0.161049276403844,-0.159757267870224,-0.155110071595339,
-0.128864883766184,-0.10699088015377,-0.105559722238614,-0.0751187269598587),
 .UNSPECIFIED.);
#1063=B_SPLINE_CURVE_WITH_KNOTS('',3,(#110419,#110420,#110421,#110422,#110423,
#110424,#110425,#110426,#110427,#110428,#110429,#110430,#110431,#110432,
#110433,#110434,#110435,#110436,#110437,#110438,#110439,#110440,#110441,
#110442,#110443,#110444,#110445,#110446,#110447,#110448,#110449,#110450,
#110451,#110452,#110453,#110454,#110455,#110456,#110457,#110458,#110459,
#110460,#110461,#110462,#110463,#110464,#110465,#110466,#110467,#110468,
#110469,#110470,#110471,#110472,#110473,#110474,#110475,#110476,#110477,
#110478,#110479,#110480,#110481,#110482,#110483,#110484,#110485,#110486,
#110487,#110488,#110489,#110490,#110491,#110492,#110493,#110494,#110495,
#110496,#110497,#110498,#110499,#110500,#110501,#110502,#110503,#110504,
#110505,#110506,#110507,#110508,#110509,#110510,#110511,#110512,#110513,
#110514,#110515,#110516,#110517,#110518,#110519,#110520,#110521,#110522,
#110523,#110524,#110525,#110526,#110527,#110528,#110529,#110530,#110531,
#110532,#110533,#110534,#110535,#110536,#110537,#110538,#110539,#110540,
#110541,#110542,#110543,#110544,#110545,#110546,#110547,#110548,#110549,
#110550,#110551,#110552,#110553,#110554,#110555,#110556,#110557,#110558,
#110559,#110560,#110561,#110562,#110563,#110564,#110565,#110566,#110567,
#110568,#110569,#110570,#110571,#110572,#110573,#110574,#110575,#110576,
#110577,#110578,#110579,#110580,#110581,#110582,#110583,#110584,#110585,
#110586,#110587,#110588,#110589,#110590,#110591,#110592,#110593,#110594,
#110595,#110596,#110597,#110598,#110599),.UNSPECIFIED.,.F.,.F.,(4,3,3,3,
3,3,3,3,3,3,3,3,3,3,3,3,3,3,3,3,3,3,3,3,3,3,3,3,3,3,3,3,3,3,3,3,3,3,3,3,
3,3,3,3,3,3,3,3,3,3,3,3,3,3,3,3,3,3,3,3,4),(-28.6232428877577,-28.5202021552005,
-28.4171818104866,-28.3141478661896,-28.2110002753443,-28.1077865067903,
-28.0043999094814,-27.9674205989325,-27.8640258618989,-27.7607845797986,
-27.6576646144211,-27.554610046227,-27.4515868378843,-27.3485609952268,
-27.2454282284638,-27.142239137069,-27.0388671437024,-26.9685841489706,
-26.8651894118469,-26.761948129656,-26.6588281641879,-26.5557735959032,
-26.4527503874699,-26.3497245447222,-26.2465917778698,-26.1434026863862,
-26.0400306929323,-25.9697476990087,-25.8663529620654,-25.7631116800547,
-25.6599917147658,-25.5569371466596,-25.4539139384038,-25.3508880958323,
-25.2477553291532,-25.1445662378413,-25.0411942445548,-24.9709112490468,
-24.8675165120618,-24.7642752300111,-24.6611552646847,-24.5581006965428,
-24.4550774882529,-24.352051645649,-24.2489188789403,-24.1457297876004,
-24.0423577942887,-23.972074799085,-23.8686800615172,-23.7654387788806,
-23.6623188129668,-23.5592642442367,-23.4562410353589,-23.353215192168,
-23.2500824248778,-23.1468933329587,-23.0435213390778,-22.9732383491231,
-22.8444301460683,-22.7177283292801,-22.6905949549614),.UNSPECIFIED.);
#1064=B_SPLINE_CURVE_WITH_KNOTS('',3,(#110600,#110601,#110602,#110603),
 .UNSPECIFIED.,.F.,.F.,(4,4),(-22.6905949549614,-22.3411473650526),
 .UNSPECIFIED.);
#1065=B_SPLINE_CURVE_WITH_KNOTS('',3,(#110609,#110610,#110611,#110612,#110613,
#110614,#110615,#110616,#110617,#110618,#110619,#110620,#110621,#110622,
#110623,#110624,#110625,#110626),.UNSPECIFIED.,.F.,.F.,(4,2,2,2,2,2,2,2,
4),(-0.0747374496497559,-0.0441237844182805,-0.0412117011286783,-0.0398236116774997,
-0.0387489292896549,-0.0375208900578933,-0.0362287396242862,-0.0342507365147655,
-0.000628701287238877),.UNSPECIFIED.);
#1066=B_SPLINE_CURVE_WITH_KNOTS('',3,(#110627,#110628,#110629,#110630,#110631,
#110632,#110633,#110634,#110635,#110636,#110637,#110638,#110639,#110640,
#110641,#110642,#110643,#110644,#110645,#110646,#110647,#110648,#110649,
#110650,#110651,#110652,#110653,#110654,#110655,#110656,#110657,#110658,
#110659,#110660,#110661,#110662,#110663,#110664,#110665,#110666,#110667,
#110668,#110669,#110670,#110671,#110672,#110673,#110674,#110675,#110676,
#110677,#110678,#110679,#110680,#110681,#110682,#110683,#110684,#110685,
#110686,#110687,#110688,#110689,#110690,#110691,#110692,#110693,#110694,
#110695,#110696,#110697,#110698,#110699,#110700,#110701,#110702,#110703,
#110704,#110705,#110706,#110707,#110708,#110709,#110710,#110711,#110712,
#110713,#110714,#110715,#110716,#110717,#110718,#110719,#110720,#110721,
#110722,#110723,#110724,#110725,#110726,#110727,#110728,#110729,#110730,
#110731,#110732,#110733,#110734,#110735,#110736,#110737,#110738,#110739,
#110740,#110741,#110742,#110743,#110744,#110745,#110746,#110747,#110748,
#110749,#110750,#110751,#110752,#110753,#110754,#110755,#110756,#110757,
#110758,#110759,#110760,#110761,#110762,#110763,#110764,#110765,#110766,
#110767,#110768,#110769,#110770,#110771,#110772,#110773,#110774,#110775,
#110776,#110777,#110778,#110779,#110780,#110781,#110782,#110783,#110784,
#110785,#110786,#110787,#110788,#110789,#110790,#110791,#110792,#110793,
#110794,#110795,#110796,#110797,#110798,#110799,#110800,#110801,#110802,
#110803,#110804,#110805,#110806,#110807,#110808,#110809,#110810,#110811,
#110812,#110813,#110814,#110815,#110816,#110817,#110818,#110819,#110820,
#110821,#110822,#110823,#110824,#110825,#110826,#110827,#110828,#110829,
#110830,#110831,#110832,#110833,#110834,#110835,#110836,#110837,#110838,
#110839,#110840,#110841,#110842,#110843,#110844,#110845,#110846),
 .UNSPECIFIED.,.F.,.F.,(4,2,2,2,2,2,2,2,2,2,2,2,2,2,2,2,2,2,2,2,2,2,2,2,
2,2,2,2,2,2,2,2,2,2,2,2,2,2,2,2,2,2,2,2,2,2,2,2,2,2,2,2,2,2,2,2,2,2,2,2,
2,2,2,2,2,2,2,2,2,2,2,2,2,2,2,2,2,2,2,2,2,2,2,2,2,2,2,2,2,2,2,2,2,2,2,2,
2,2,2,2,2,2,2,2,2,2,2,2,2,4),(-2.66802542164946,-2.63755417114925,-2.61103832252004,
-2.60487114890265,-2.60220785653925,-2.60025403454764,-2.59845111805707,
-2.59553095236573,-2.58831615461444,-2.54291362715924,-2.52278252471317,
-2.50656823983998,-2.49817190163438,-2.49612451106828,-2.49489637664954,
-2.4938213787511,-2.4924325646186,-2.48951785900045,-2.45949080718715,-2.4082036857542,
-2.39936634425664,-2.3929590848947,-2.39025468606481,-2.38829361857624,
-2.38649986413826,-2.38362936940678,-2.37671225829577,-2.32405732039061,
-2.29784926700888,-2.28646513786489,-2.28418807232359,-2.2829305762518,
-2.28185919856569,-2.28051254141557,-2.27789632360918,-2.26195362471783,
-2.25752409833991,-2.21497018184428,-2.18434635016617,-2.17990434965435,
-2.1775709988326,-2.17565885536641,-2.17344258182554,-2.1696486409106,-2.15497835789923,
-2.14272676364302,-2.10721191288641,-2.0847663655952,-2.07439005645545,
-2.07217382100489,-2.0709296132986,-2.0698569503543,-2.06849241762192,-2.06579252371313,
-2.04761342823916,-2.02952741803248,-1.99679663800888,-1.97429543162791,
-1.96864952379694,-1.96607949520937,-1.9641410649718,-1.96231370703854,
-1.95976978044937,-1.95311694568588,-1.89740855395777,-1.87327422033005,
-1.86243090428267,-1.86018552488489,-1.85893488430517,-1.85786281704301,
-1.85650692708351,-1.85436217006904,-1.84334150555545,-1.79204137555043,
-1.76337564037632,-1.7569466818527,-1.75423857360005,-1.75227679575202,
-1.75048375393106,-1.74761736581653,-1.74072550021672,-1.68772904682384,
-1.66175792437525,-1.65043377730957,-1.64816010019916,-1.64690331971634,
-1.64583185063414,-1.64448418622504,-1.64186338936202,-1.62583795685175,
-1.62043989082364,-1.60593640459328,-1.573040655047,-1.55028407741119,-1.54460348675651,
-1.54202698421215,-1.54008744859317,-1.53826181943444,-1.53572473920949,
-1.52911608717087,-1.47296631352672,-1.44911719837533,-1.43835070904764,
-1.43610988788624,-1.43486018851902,-1.43378794177061,-1.43243055848784,
-1.4297648025452,-1.41257812712104,-1.40849963608456),.UNSPECIFIED.);
#1067=B_SPLINE_CURVE_WITH_KNOTS('',3,(#110848,#110849,#110850,#110851,#110852,
#110853,#110854,#110855,#110856,#110857),.UNSPECIFIED.,.F.,.F.,(4,1,1,1,
1,1,1,4),(-22.3411473650526,-21.9744018991612,-20.9755654491994,-19.9767289992375,
-18.9778925492756,-17.9790560993137,-16.9802196493519,-16.4074096477818),
 .UNSPECIFIED.);
#1068=B_SPLINE_CURVE_WITH_KNOTS('',3,(#110858,#110859,#110860,#110861,#110862,
#110863),.UNSPECIFIED.,.F.,.F.,(4,2,4),(-2.66742166919024,-2.60891629842673,
-2.59315592110003),.UNSPECIFIED.);
#1069=B_SPLINE_CURVE_WITH_KNOTS('',3,(#110868,#110869,#110870,#110871,#110872,
#110873,#110874,#110875,#110876,#110877,#110878,#110879,#110880,#110881,
#110882,#110883,#110884,#110885,#110886,#110887,#110888,#110889,#110890,
#110891,#110892,#110893,#110894,#110895,#110896,#110897,#110898,#110899,
#110900,#110901,#110902,#110903,#110904,#110905,#110906,#110907,#110908,
#110909,#110910,#110911,#110912,#110913,#110914,#110915,#110916,#110917,
#110918,#110919,#110920,#110921,#110922,#110923,#110924,#110925,#110926,
#110927,#110928,#110929,#110930,#110931,#110932,#110933,#110934,#110935,
#110936,#110937,#110938,#110939,#110940,#110941,#110942,#110943,#110944,
#110945,#110946,#110947,#110948,#110949,#110950,#110951,#110952,#110953,
#110954,#110955,#110956,#110957,#110958,#110959,#110960,#110961,#110962,
#110963,#110964,#110965,#110966,#110967,#110968,#110969,#110970,#110971,
#110972,#110973,#110974,#110975,#110976,#110977,#110978,#110979,#110980,
#110981,#110982,#110983,#110984,#110985,#110986,#110987,#110988,#110989,
#110990,#110991,#110992,#110993,#110994,#110995,#110996,#110997,#110998,
#110999,#111000,#111001,#111002,#111003,#111004,#111005,#111006,#111007,
#111008,#111009,#111010,#111011,#111012,#111013,#111014,#111015,#111016,
#111017,#111018,#111019,#111020,#111021,#111022,#111023,#111024,#111025,
#111026,#111027,#111028,#111029,#111030,#111031,#111032,#111033,#111034,
#111035,#111036,#111037,#111038,#111039,#111040,#111041,#111042,#111043,
#111044,#111045,#111046,#111047,#111048,#111049,#111050,#111051,#111052,
#111053,#111054,#111055,#111056,#111057,#111058,#111059,#111060,#111061,
#111062,#111063,#111064,#111065,#111066,#111067,#111068,#111069,#111070,
#111071,#111072,#111073,#111074,#111075,#111076,#111077,#111078,#111079,
#111080,#111081,#111082,#111083,#111084,#111085,#111086,#111087,#111088,
#111089,#111090,#111091),.UNSPECIFIED.,.F.,.F.,(4,2,2,2,2,2,2,2,2,2,2,2,
2,2,2,2,2,2,2,2,2,2,2,2,2,2,2,2,2,2,2,2,2,2,2,2,2,2,2,2,2,2,2,2,2,2,2,2,
2,2,2,2,2,2,2,2,2,2,2,2,2,2,2,2,2,2,2,2,2,2,2,2,2,2,2,2,2,2,2,2,2,2,2,2,
2,2,2,2,2,2,2,2,2,2,2,2,2,2,2,2,2,2,2,2,2,2,2,2,2,2,2,4),(-1.40825517075566,
-1.36486070561898,-1.33380956985227,-1.31575891231249,-1.31306317661106,
-1.31169947357094,-1.31062680438786,-1.30938183875461,-1.30716243548391,
-1.29673882022339,-1.27412454479273,-1.21599821858833,-1.20961431155974,
-1.20711395446872,-1.20529802421571,-1.20335316480793,-1.20074255280682,
-1.19487327385787,-1.17069584189302,-1.12021061713001,-1.11977980004809,
-1.10359243152392,-1.10096535738956,-1.09961635537938,-1.09854481881298,
-1.09728912007681,-1.0950203123576,-1.08378027973149,-1.05813476867367,
-1.00462903004577,-0.997774874658043,-0.994914745537326,-0.993122882415104,
-0.991160195526036,-0.988446784775229,-0.981985979620462,-0.928043982984161,
-0.891838135733603,-0.888983288922922,-0.887606177339344,-0.88653236320879,
-0.885296708443276,-0.883119562402402,-0.873336757335368,-0.824414215182172,
-0.789290664026276,-0.784995243414214,-0.782453888004092,-0.780513096273503,
-0.778439679793219,-0.775190876441804,-0.764879919409157,-0.748318611586668,
-0.715459017225508,-0.701719286163376,-0.694865970527898,-0.694544051345743,
-0.68882747734314,-0.678952475356014,-0.676883015550683,-0.675550313355996,
-0.674479832973003,-0.673211423550649,-0.670883507061314,-0.65855923581904,
-0.603512539575028,-0.576984973962758,-0.572875855777599,-0.570389091677128,
-0.568457036580506,-0.566360183106348,-0.563004217864846,-0.551716844864075,
-0.532932223090572,-0.497974924995506,-0.467987713472837,-0.465074023301411,
-0.463685608444667,-0.462610877514032,-0.461383010982414,-0.459240440159017,
-0.449944824800894,-0.431095093403466,-0.387250853073146,-0.364754422847273,
-0.360810609394575,-0.358346530092496,-0.356423149017978,-0.354294224281466,
-0.350793180911979,-0.338041041544176,-0.315661048082141,-0.265630907114065,
-0.255111362957835,-0.252998938797095,-0.251653126764957,-0.250582034471614,
-0.24932442991037,-0.247091844486272,-0.236304903717156,-0.212308631438729,
-0.186250529351654,-0.153387327652072,-0.149130333772282,-0.146600315032072,
-0.144661579838321,-0.142583928024751,-0.139314981065769,-0.128824707791949,
-0.0985425252177895,-0.0750520070855559,-0.0747374496497559),
 .UNSPECIFIED.);
#1070=B_SPLINE_CURVE_WITH_KNOTS('',3,(#111092,#111093,#111094,#111095,#111096,
#111097,#111098,#111099,#111100,#111101,#111102,#111103,#111104,#111105,
#111106,#111107,#111108,#111109,#111110,#111111,#111112,#111113,#111114,
#111115,#111116,#111117,#111118,#111119,#111120,#111121,#111122,#111123,
#111124,#111125,#111126,#111127,#111128,#111129,#111130,#111131,#111132,
#111133,#111134,#111135,#111136,#111137,#111138,#111139,#111140,#111141,
#111142,#111143,#111144,#111145,#111146,#111147,#111148,#111149,#111150,
#111151,#111152,#111153,#111154,#111155,#111156,#111157,#111158,#111159,
#111160,#111161,#111162,#111163,#111164,#111165,#111166,#111167,#111168,
#111169,#111170,#111171,#111172,#111173,#111174,#111175,#111176,#111177,
#111178,#111179,#111180,#111181,#111182,#111183,#111184,#111185,#111186,
#111187,#111188,#111189,#111190,#111191,#111192,#111193,#111194,#111195,
#111196,#111197,#111198,#111199,#111200,#111201,#111202,#111203,#111204,
#111205,#111206,#111207,#111208,#111209,#111210,#111211,#111212,#111213,
#111214,#111215,#111216,#111217,#111218,#111219,#111220,#111221,#111222,
#111223,#111224,#111225,#111226,#111227,#111228,#111229,#111230,#111231,
#111232,#111233,#111234,#111235,#111236,#111237,#111238,#111239,#111240,
#111241,#111242,#111243,#111244,#111245,#111246,#111247,#111248,#111249,
#111250,#111251,#111252,#111253,#111254,#111255,#111256,#111257,#111258,
#111259,#111260,#111261,#111262,#111263,#111264,#111265,#111266,#111267,
#111268,#111269,#111270,#111271,#111272,#111273,#111274,#111275,#111276,
#111277,#111278,#111279,#111280,#111281,#111282,#111283,#111284,#111285,
#111286,#111287,#111288,#111289,#111290,#111291,#111292,#111293,#111294,
#111295,#111296,#111297,#111298,#111299,#111300,#111301,#111302,#111303,
#111304,#111305,#111306,#111307,#111308,#111309,#111310,#111311,#111312,
#111313,#111314,#111315,#111316,#111317,#111318,#111319,#111320,#111321,
#111322,#111323,#111324,#111325),.UNSPECIFIED.,.F.,.F.,(4,2,2,2,2,2,2,2,
2,2,2,2,2,2,2,2,2,2,2,2,2,2,2,2,2,2,2,2,2,2,2,2,2,2,2,2,2,2,2,2,2,2,2,2,
2,2,2,2,2,2,2,2,2,2,2,2,2,2,2,2,2,2,2,2,2,2,2,2,2,2,2,2,2,2,2,2,2,2,2,2,
2,2,2,2,2,2,2,2,2,2,2,2,2,2,2,2,2,2,2,2,2,2,2,2,2,2,2,2,2,2,2,2,2,2,2,2,
4),(-2.59315592110003,-2.59007760746276,-2.58078442575993,-2.57864192938728,
-2.57741401594,-2.57633919268755,-2.57495057949168,-2.57203620779358,-2.54225933787784,
-2.49161915788067,-2.48229151674428,-2.47774090940545,-2.47500323237432,
-2.47251935567029,-2.47064334858746,-2.46881679266551,-2.46627505840282,
-2.45963438585243,-2.40384856483129,-2.37977478395088,-2.36894861241379,
-2.36670457236547,-2.36545436799998,-2.3643824763686,-2.36302655672008,
-2.3608812914899,-2.3498481993763,-2.29862656964715,-2.26992243674973,-2.26348946250616,
-2.26078097146617,-2.25881939093963,-2.25702685582208,-2.25416198731251,
-2.24727744883033,-2.19421481901948,-2.16830142125363,-2.1569928671498,
-2.15472038807679,-2.15346400985927,-2.15239273879776,-2.15104513417737,
-2.14842386474133,-2.1323851049409,-2.127067161605,-2.11250735298119,-2.07961709049668,
-2.06305107213864,-2.05273920487412,-2.04949043458139,-2.04741712304519,
-2.0454764891654,-2.04293542792708,-2.03864073343987,-2.00353420408067,
-1.95464848169311,-1.94485971866109,-1.94268234715487,-1.94144672193535,
-1.94037303818875,-1.93899622349874,-1.93614245724537,-1.91343293577874,
-1.87271723892081,-1.84567967566739,-1.83944821448597,-1.83677396459371,
-1.83481838483426,-1.83301823941712,-1.83011233514104,-1.82298134565623,
-1.77424411226903,-1.73505279865021,-1.73147806748382,-1.72996904413746,
-1.72887687769649,-1.72785089466849,-1.72610769613703,-1.72137471656642,
-1.68178411444338,-1.63388987192041,-1.62749309716374,-1.62479052636968,
-1.62282983556348,-1.62103577072735,-1.61816334851162,-1.6112341799604,
-1.55875566853387,-1.53242878829024,-1.52101504518211,-1.518736407992,-1.51747862383898,
-1.51640745066291,-1.51506158912328,-1.51244824797811,-1.4965684694718,
-1.49069771123085,-1.4466670366256,-1.4281081624543,-1.41691845725991,-1.41357286267423,
-1.41147833616775,-1.40954560827383,-1.40705404740345,-1.4029285442078,
-1.37574263767364,-1.33373204800133,-1.32763515029272,-1.30978755198806,
-1.30709916585634,-1.30573723665793,-1.30466495507299,-1.30341928550094,
-1.3011958620241,-1.29070305466864,-1.26784055931316,-1.25960929803069),
 .UNSPECIFIED.);
#1071=B_SPLINE_CURVE_WITH_KNOTS('',3,(#111331,#111332,#111333,#111334,#111335,
#111336,#111337,#111338,#111339,#111340,#111341,#111342,#111343,#111344,
#111345,#111346,#111347,#111348,#111349,#111350,#111351,#111352,#111353,
#111354,#111355,#111356,#111357,#111358,#111359,#111360,#111361,#111362,
#111363,#111364,#111365,#111366,#111367,#111368,#111369,#111370,#111371,
#111372,#111373,#111374,#111375,#111376,#111377,#111378,#111379,#111380,
#111381,#111382,#111383,#111384,#111385,#111386,#111387,#111388,#111389,
#111390,#111391,#111392,#111393,#111394,#111395,#111396,#111397,#111398,
#111399,#111400,#111401,#111402,#111403,#111404,#111405,#111406,#111407,
#111408,#111409,#111410,#111411,#111412,#111413,#111414,#111415,#111416,
#111417,#111418,#111419,#111420,#111421,#111422,#111423,#111424,#111425,
#111426,#111427,#111428,#111429,#111430,#111431,#111432,#111433,#111434,
#111435,#111436),.UNSPECIFIED.,.F.,.F.,(4,3,3,3,3,3,3,3,3,3,3,3,3,3,3,3,
3,3,3,3,3,3,3,3,3,3,3,3,3,3,3,3,3,3,3,4),(-3.49054215479303,-3.38888735076487,
-3.28714626812733,-3.1853636260202,-3.08340269581344,-2.99650934988562,
-2.89298838415396,-2.78961842057155,-2.68636679313983,-2.58317880759896,
-2.48002064176422,-2.37685851496102,-2.27358841489215,-2.17026119505921,
-2.0667513667292,-1.99767289992375,-1.89536901188922,-1.79321917542624,
-1.69118674247088,-1.58921701577402,-1.48727463022104,-1.38532426116751,
-1.28325154596753,-1.18111583450429,-1.07877443242786,-0.998836449961874,
-0.892563151715311,-0.780992757750897,-0.67507278596415,-0.569252409114429,
-0.463503885892151,-0.35779956469349,-0.252082102978442,-0.14635955384072,
-0.0405640348441946,0.),.UNSPECIFIED.);
#1072=B_SPLINE_CURVE_WITH_KNOTS('',3,(#111439,#111440,#111441,#111442,#111443,
#111444,#111445,#111446,#111447,#111448,#111449,#111450,#111451,#111452,
#111453,#111454,#111455,#111456,#111457,#111458,#111459,#111460,#111461,
#111462,#111463,#111464,#111465,#111466,#111467,#111468,#111469,#111470,
#111471,#111472,#111473,#111474,#111475,#111476,#111477,#111478,#111479,
#111480,#111481,#111482,#111483,#111484,#111485,#111486,#111487,#111488,
#111489,#111490,#111491,#111492,#111493,#111494,#111495,#111496,#111497,
#111498,#111499,#111500,#111501,#111502,#111503,#111504,#111505,#111506,
#111507,#111508,#111509,#111510,#111511,#111512,#111513,#111514,#111515,
#111516,#111517,#111518,#111519,#111520,#111521,#111522,#111523,#111524,
#111525,#111526,#111527,#111528,#111529,#111530,#111531,#111532,#111533,
#111534,#111535,#111536,#111537,#111538,#111539,#111540,#111541,#111542,
#111543,#111544,#111545,#111546,#111547,#111548,#111549,#111550,#111551,
#111552,#111553,#111554,#111555,#111556,#111557,#111558,#111559,#111560,
#111561,#111562,#111563,#111564,#111565,#111566,#111567,#111568,#111569,
#111570,#111571,#111572,#111573,#111574,#111575,#111576,#111577,#111578,
#111579,#111580,#111581,#111582,#111583,#111584,#111585,#111586,#111587,
#111588,#111589,#111590,#111591,#111592,#111593,#111594,#111595,#111596,
#111597,#111598),.UNSPECIFIED.,.F.,.F.,(4,3,3,3,3,3,3,3,3,3,3,3,3,3,3,3,
3,3,3,3,3,3,3,3,3,3,3,3,3,3,3,3,3,3,3,3,3,3,3,3,3,3,3,3,3,3,3,3,3,3,3,3,
3,4),(2.00878451764821,2.1121039127969,2.21526989698106,2.31831446525083,
2.42129383098608,2.52424213980843,2.62719349431524,2.73024965054137,2.83336280284649,
2.93665222006088,2.99650934988562,3.10008230986107,3.20350557536155,3.30681224772107,
3.41005632831867,3.51327157245742,3.61649169494131,3.71982084946884,3.82320780718046,
3.92677785652894,3.9953457998475,4.09860812441836,4.20171508638263,4.30469852295221,
4.40761526975679,4.51049956061297,4.61338558491661,4.71637810302106,4.81942648355174,
4.92265858166651,4.99418224980938,5.09760358352984,5.20087156240149,5.30401824170998,
5.40709952008126,5.51014939511656,5.61320182122765,5.71636085636681,5.81957608032992,
5.92297369428319,5.99301869977126,6.09643423755246,6.19969678686738,6.30283861434794,
6.40591539958103,6.50896114779528,6.61200982139887,6.71516571129326,6.81837812515211,
6.92177350497573,6.99185514973313,7.09672279125044,7.20139613948791,7.24304105038295),
 .UNSPECIFIED.);
#1073=B_SPLINE_CURVE_WITH_KNOTS('',3,(#111601,#111602,#111603,#111604,#111605,
#111606,#111607,#111608,#111609,#111610,#111611,#111612,#111613),
 .UNSPECIFIED.,.F.,.F.,(4,3,3,3,4),(7.24304105038295,7.3475229962934,7.45192126808273,
7.55626822218831,7.5925217232362),.UNSPECIFIED.);
#1074=B_SPLINE_CURVE_WITH_KNOTS('',3,(#111614,#111615,#111616,#111617,#111618,
#111619,#111620,#111621,#111622,#111623,#111624,#111625,#111626,#111627,
#111628,#111629,#111630,#111631,#111632,#111633,#111634,#111635,#111636,
#111637,#111638,#111639,#111640,#111641,#111642,#111643,#111644,#111645,
#111646,#111647,#111648,#111649,#111650,#111651,#111652,#111653,#111654,
#111655,#111656,#111657,#111658,#111659,#111660,#111661,#111662,#111663,
#111664,#111665,#111666,#111667,#111668,#111669,#111670,#111671,#111672,
#111673,#111674,#111675,#111676,#111677,#111678,#111679,#111680,#111681,
#111682,#111683,#111684,#111685,#111686,#111687,#111688,#111689,#111690,
#111691,#111692,#111693,#111694,#111695,#111696,#111697,#111698,#111699,
#111700,#111701,#111702,#111703,#111704,#111705,#111706,#111707,#111708,
#111709,#111710,#111711,#111712,#111713,#111714,#111715,#111716,#111717,
#111718,#111719,#111720,#111721,#111722,#111723,#111724,#111725,#111726,
#111727,#111728,#111729,#111730,#111731,#111732,#111733,#111734,#111735,
#111736,#111737,#111738,#111739,#111740,#111741,#111742,#111743,#111744,
#111745,#111746,#111747,#111748,#111749,#111750,#111751,#111752,#111753,
#111754,#111755,#111756,#111757,#111758,#111759,#111760,#111761,#111762,
#111763,#111764,#111765,#111766,#111767,#111768,#111769,#111770,#111771,
#111772,#111773,#111774,#111775,#111776,#111777,#111778,#111779,#111780,
#111781,#111782,#111783,#111784,#111785,#111786,#111787,#111788,#111789,
#111790,#111791,#111792,#111793,#111794,#111795,#111796,#111797,#111798,
#111799,#111800,#111801,#111802,#111803,#111804,#111805,#111806,#111807,
#111808,#111809,#111810,#111811,#111812,#111813,#111814,#111815,#111816,
#111817,#111818,#111819,#111820,#111821,#111822,#111823,#111824,#111825,
#111826,#111827,#111828,#111829,#111830,#111831,#111832,#111833,#111834,
#111835,#111836,#111837),.UNSPECIFIED.,.F.,.F.,(4,2,2,2,2,2,2,2,2,2,2,2,
2,2,2,2,2,2,2,2,2,2,2,2,2,2,2,2,2,2,2,2,2,2,2,2,2,2,2,2,2,2,2,2,2,2,2,2,
2,2,2,2,2,2,2,2,2,2,2,2,2,2,2,2,2,2,2,2,2,2,2,2,2,2,2,2,2,2,2,2,2,2,2,2,
2,2,2,2,2,2,2,2,2,2,2,2,2,2,2,2,2,2,2,2,2,2,2,2,2,2,2,4),(-2.66727271147711,
-2.64514416123945,-2.59598682591251,-2.58660188532894,-2.58445439068241,
-2.58322622212268,-2.58215204826259,-2.58076604165038,-2.57786525834857,
-2.55097420357146,-2.51353771549261,-2.49429289537454,-2.48669443218254,
-2.48276636104382,-2.47945649826737,-2.47740192605286,-2.47547608342467,
-2.47299780604071,-2.46900881820271,-2.44540125182709,-2.39836981398955,
-2.38274909190571,-2.37453345221375,-2.37247353224399,-2.3712634653851,
-2.37018463046746,-2.36878790365098,-2.36645716905911,-2.35190421798962,
-2.34958113653479,-2.30363635510011,-2.27573127058486,-2.26939428504012,
-2.26670206614296,-2.26474341268377,-2.2629474242732,-2.26006362258563,
-2.2530643410738,-2.20164290380157,-2.174559750452,-2.16295806679369,-2.16066914658454,
-2.15940927313382,-2.15833842129164,-2.15699565879203,-2.15439636277061,
-2.13885999261317,-2.13223205772158,-2.11842240488002,-2.08554052236304,
-2.06898364824746,-2.0586762010965,-2.05542820156501,-2.05335523703073,
-2.05141482761761,-2.04887391745638,-2.04457916477255,-2.00944108908087,
-1.96049945514058,-1.95078674134142,-1.94861477560486,-1.94738044024498,
-1.94630663183684,-1.94492809590307,-1.94206564076842,-1.918706272745,-1.9064090561897,
-1.87354001080172,-1.85700030741615,-1.84670002718578,-1.84345234324541,
-1.84137910534026,-1.8394381038791,-1.83689592979739,-1.83259793217183,
-1.79725558910473,-1.74808177107833,-1.73876433087334,-1.73661980194068,
-1.73539129338086,-1.7343163695614,-1.73292814162882,-1.73001627459185,
-1.69798300408521,-1.66507278295209,-1.64624531853499,-1.6387608006613,
-1.6331384018191,-1.63057275744381,-1.62863505227293,-1.62680647601108,
-1.62425779356639,-1.61757401128421,-1.56218086420771,-1.53783841722789,
-1.52693939559833,-1.52469073589719,-1.52343941933517,-1.52236748220644,
-1.52101266770936,-1.51835847063183,-1.50147594892666,-1.482688240376,-1.44972214359721,
-1.43306884299333,-1.42271704818392,-1.41946333617731,-1.41738870063118,
-1.41544811106488,-1.41290895773657,-1.40862162865882,-1.40825517075566),
 .UNSPECIFIED.);
#1075=B_SPLINE_CURVE_WITH_KNOTS('',3,(#111839,#111840,#111841,#111842,#111843,
#111844,#111845,#111846,#111847,#111848,#111849,#111850,#111851,#111852,
#111853,#111854,#111855,#111856,#111857,#111858,#111859,#111860,#111861,
#111862,#111863,#111864,#111865,#111866,#111867,#111868,#111869,#111870,
#111871,#111872,#111873,#111874,#111875,#111876,#111877,#111878,#111879,
#111880,#111881,#111882,#111883,#111884,#111885,#111886,#111887,#111888,
#111889,#111890,#111891,#111892,#111893,#111894,#111895,#111896,#111897,
#111898,#111899,#111900,#111901,#111902,#111903,#111904,#111905,#111906,
#111907,#111908,#111909,#111910,#111911,#111912,#111913,#111914,#111915,
#111916,#111917,#111918,#111919,#111920,#111921,#111922,#111923,#111924,
#111925,#111926,#111927,#111928,#111929,#111930,#111931,#111932,#111933,
#111934,#111935,#111936,#111937,#111938,#111939,#111940,#111941,#111942,
#111943,#111944,#111945,#111946,#111947,#111948,#111949,#111950,#111951,
#111952,#111953,#111954,#111955,#111956,#111957,#111958,#111959,#111960,
#111961,#111962,#111963,#111964,#111965,#111966,#111967,#111968,#111969,
#111970,#111971,#111972,#111973,#111974,#111975,#111976,#111977,#111978,
#111979,#111980,#111981,#111982,#111983,#111984,#111985,#111986,#111987,
#111988,#111989,#111990,#111991,#111992,#111993,#111994,#111995,#111996,
#111997,#111998,#111999,#112000,#112001,#112002,#112003,#112004,#112005,
#112006,#112007,#112008,#112009,#112010,#112011,#112012,#112013,#112014,
#112015,#112016,#112017,#112018,#112019,#112020,#112021,#112022,#112023,
#112024,#112025,#112026,#112027,#112028,#112029,#112030,#112031,#112032,
#112033,#112034,#112035,#112036,#112037,#112038,#112039,#112040,#112041,
#112042,#112043,#112044,#112045,#112046,#112047,#112048,#112049,#112050,
#112051,#112052,#112053,#112054,#112055,#112056,#112057,#112058,#112059,
#112060),.UNSPECIFIED.,.F.,.F.,(4,2,2,2,2,2,2,2,2,2,2,2,2,2,2,2,2,2,2,2,
2,2,2,2,2,2,2,2,2,2,2,2,2,2,2,2,2,2,2,2,2,2,2,2,2,2,2,2,2,2,2,2,2,2,2,2,
2,2,2,2,2,2,2,2,2,2,2,2,2,2,2,2,2,2,2,2,2,2,2,2,2,2,2,2,2,2,2,2,2,2,2,2,
2,2,2,2,2,2,2,2,2,2,2,2,2,2,2,2,2,2,4),(-1.25960929803069,-1.21011174059313,
-1.20367847070001,-1.20117010943763,-1.19935225139578,-1.19740896028293,
-1.19480675371619,-1.18898303134276,-1.16514968953682,-1.11614974413865,
-1.09779133614114,-1.09505199506547,-1.09369780555932,-1.09262570481289,
-1.091373288173,-1.0891211906243,-1.07817670271,-1.0536606039483,-0.998557337097207,
-0.99185015018964,-0.989297536679468,-0.987467670152941,-0.985529994360003,
-0.982966737023876,-0.977358997910008,-0.929075022523474,-0.888723650897612,
-0.884011293331561,-0.882271319328065,-0.881246034995388,-0.880154599411069,
-0.878645304763367,-0.875062783457867,-0.87003765954688,-0.856213798932361,
-0.833862851050275,-0.787184857092799,-0.779989353322992,-0.77707435160675,
-0.775273835415769,-0.773322011139474,-0.770660371509933,-0.764492312114575,
-0.737949751057634,-0.698620981785537,-0.687287703556983,-0.673503625815556,
-0.671211226208082,-0.669826491416476,-0.668750040710085,-0.667534910834848,
-0.665449578878858,-0.656908102706735,-0.640347757197037,-0.598278136195905,
-0.57109945539481,-0.566971932881447,-0.564479109437179,-0.562545367777876,
-0.560449702725794,-0.557102184858802,-0.545904431502816,-0.527329184645362,
-0.484805743872738,-0.462028553407037,-0.459170664799327,-0.457792004451033,
-0.456715739894236,-0.45547476300475,-0.453287175566931,-0.443435343816671,
-0.394232923641606,-0.359839149025425,-0.355551442270918,-0.353009445992766,
-0.35106507330854,-0.348984785261022,-0.345718755854318,-0.335297069174024,
-0.318505453670392,-0.258883112535898,-0.249294109526251,-0.247244777885605,
-0.245918161908627,-0.244851122932402,-0.24384140172536,-0.241869006075161,
-0.234450995222338,-0.220917592501162,-0.192337588586147,-0.147271549613432,
-0.143024726566531,-0.140506655582846,-0.138580647851886,-0.136520206534398,
-0.133286041550045,-0.122977073904068,-0.106384488990819,-0.0845184569141308,
-0.0739378345267708,-0.0616381299481483,-0.0559579040156458,-0.0377855980021243,
-0.0350634423940383,-0.0337175280400151,-0.0326484421208826,-0.0316335711034375,
-0.030396079803991,-0.0285521106333106,-0.021532695795065,-0.00065555409686486),
 .UNSPECIFIED.);
#1076=B_SPLINE_CURVE_WITH_KNOTS('',3,(#112061,#112062,#112063,#112064,#112065,
#112066,#112067,#112068,#112069,#112070,#112071,#112072,#112073),
 .UNSPECIFIED.,.F.,.F.,(4,3,3,3,4),(-3.84103903298818,-3.73916989819696,
-3.63740764530368,-3.53571860707482,-3.49054215479303),.UNSPECIFIED.);
#1077=B_SPLINE_CURVE_WITH_KNOTS('',3,(#112076,#112077,#112078,#112079,#112080,
#112081,#112082,#112083,#112084,#112085,#112086,#112087,#112088),
 .UNSPECIFIED.,.F.,.F.,(4,3,3,3,4),(7.24304095782437,7.34752291252988,7.45192119316322,
7.55626815616017,7.5925217232362),.UNSPECIFIED.);
#1078=B_SPLINE_CURVE_WITH_KNOTS('',3,(#112089,#112090,#112091,#112092,#112093,
#112094,#112095,#112096,#112097,#112098,#112099,#112100,#112101,#112102,
#112103,#112104,#112105,#112106,#112107,#112108,#112109,#112110,#112111,
#112112,#112113,#112114,#112115,#112116,#112117,#112118,#112119,#112120,
#112121,#112122,#112123,#112124,#112125,#112126,#112127,#112128,#112129,
#112130,#112131,#112132,#112133,#112134,#112135,#112136,#112137,#112138,
#112139,#112140,#112141,#112142,#112143,#112144,#112145,#112146,#112147,
#112148,#112149,#112150,#112151,#112152,#112153,#112154,#112155,#112156,
#112157,#112158,#112159,#112160,#112161,#112162,#112163,#112164,#112165,
#112166,#112167,#112168,#112169,#112170,#112171,#112172,#112173,#112174,
#112175,#112176,#112177,#112178,#112179,#112180,#112181,#112182,#112183,
#112184,#112185,#112186,#112187,#112188,#112189,#112190,#112191,#112192,
#112193,#112194,#112195,#112196,#112197,#112198,#112199,#112200,#112201,
#112202,#112203,#112204,#112205,#112206,#112207,#112208,#112209,#112210,
#112211,#112212,#112213,#112214,#112215,#112216,#112217,#112218,#112219,
#112220,#112221,#112222,#112223,#112224,#112225,#112226,#112227,#112228,
#112229,#112230,#112231,#112232,#112233,#112234,#112235,#112236,#112237,
#112238,#112239,#112240,#112241,#112242,#112243,#112244,#112245,#112246,
#112247,#112248,#112249,#112250,#112251,#112252,#112253,#112254,#112255,
#112256,#112257,#112258,#112259,#112260,#112261,#112262,#112263,#112264,
#112265,#112266,#112267,#112268,#112269,#112270,#112271,#112272,#112273,
#112274,#112275,#112276,#112277,#112278,#112279,#112280,#112281,#112282,
#112283,#112284,#112285,#112286,#112287,#112288,#112289,#112290,#112291,
#112292,#112293,#112294,#112295,#112296,#112297,#112298,#112299,#112300,
#112301,#112302,#112303,#112304,#112305,#112306,#112307,#112308,#112309,
#112310,#112311,#112312,#112313,#112314),.UNSPECIFIED.,.F.,.F.,(4,2,2,2,
2,2,2,2,2,2,2,2,2,2,2,2,2,2,2,2,2,2,2,2,2,2,2,2,2,2,2,2,2,2,2,2,2,2,2,2,
2,2,2,2,2,2,2,2,2,2,2,2,2,2,2,2,2,2,2,2,2,2,2,2,2,2,2,2,2,2,2,2,2,2,2,2,
2,2,2,2,2,2,2,2,2,2,2,2,2,2,2,2,2,2,2,2,2,2,2,2,2,2,2,2,2,2,2,2,2,2,2,2,
4),(-2.66738008698545,-2.62224783784958,-2.59781807626665,-2.58689866123443,
-2.58465077822854,-2.58340061958436,-2.58232936394948,-2.5809754340121,
-2.57823682703122,-2.55989579598849,-2.54256186398593,-2.50963546001051,
-2.49302151413064,-2.48615785461855,-2.48250535135525,-2.47938648970499,
-2.47737576448748,-2.47543621773921,-2.47290497400306,-2.46864554443795,
-2.43625798350028,-2.38684716722421,-2.3750771819673,-2.37277788668897,
-2.371515230832,-2.37044400533806,-2.36910315768299,-2.36700741861124,-2.3567449683609,
-2.35162580739283,-2.34970817795153,-2.30375081737001,-2.27584422957403,
-2.26950703470382,-2.26681476519162,-2.26485608899408,-2.26306008949113,
-2.26017629141725,-2.25317712794255,-2.20175227992819,-2.1746709946617,
-2.16306972535565,-2.16078081288259,-2.1595209339716,-2.1584500716418,-2.15710728856331,
-2.1545079310582,-2.13897054293179,-2.13234428594965,-2.11853372607665,
-2.08565153311177,-2.06909449796636,-2.05878695179806,-2.05553892165284,
-2.05346593771655,-2.05152551023676,-2.04898457655228,-2.04468978440395,
-2.00955141633932,-1.96060940061397,-1.950896509287,-1.94872451732727,-1.94749016914898,
-1.94641635098428,-1.94503780430775,-1.9421753328758,-1.91881626262359,
-1.9065184180079,-1.87364906551616,-1.85710920486868,-1.84680882756439,
-1.84356111345625,-1.84148785639893,-1.83954683708113,-1.83700463971943,
-1.8327066029785,-1.79736397701867,-1.74818967157994,-1.73887213386421,
-1.73672758436278,-1.73549906432215,-1.73442413061742,-1.73303589015582,
-1.73012399776097,-1.69809709466842,-1.66517975028743,-1.64635221385029,
-1.63886765464738,-1.63324522036375,-1.63067955529907,-1.62874183265477,
-1.62691323854142,-1.62436452902093,-1.61768066234483,-1.56228724285179,
-1.53794441598955,-1.52704525222948,-1.52479656921338,-1.5235452405122,
-1.52247329349964,-1.52111846716453,-1.5184642488387,-1.50158165907637,
-1.48279369110174,-1.44982728879555,-1.43317383267406,-1.42282194145276,
-1.41956819924802,-1.41749354447039,-1.41555293693074,-1.41301376010656,
-1.40872639140123,-1.40835994883514),.UNSPECIFIED.);
#1079=B_SPLINE_CURVE_WITH_KNOTS('',3,(#112316,#112317,#112318,#112319,#112320,
#112321,#112322,#112323,#112324,#112325,#112326,#112327,#112328,#112329,
#112330,#112331,#112332,#112333,#112334,#112335,#112336,#112337,#112338,
#112339,#112340,#112341,#112342,#112343,#112344,#112345,#112346,#112347,
#112348,#112349,#112350,#112351,#112352,#112353,#112354,#112355,#112356,
#112357,#112358,#112359,#112360,#112361,#112362,#112363,#112364,#112365,
#112366,#112367,#112368,#112369,#112370,#112371,#112372,#112373,#112374,
#112375,#112376,#112377,#112378,#112379,#112380,#112381,#112382,#112383,
#112384,#112385,#112386,#112387,#112388,#112389,#112390,#112391,#112392,
#112393,#112394,#112395,#112396,#112397,#112398,#112399,#112400,#112401,
#112402,#112403,#112404,#112405,#112406,#112407,#112408,#112409,#112410,
#112411,#112412,#112413,#112414,#112415,#112416,#112417,#112418,#112419,
#112420,#112421,#112422,#112423,#112424,#112425,#112426,#112427,#112428,
#112429,#112430,#112431,#112432,#112433,#112434,#112435,#112436,#112437,
#112438,#112439,#112440,#112441,#112442,#112443,#112444,#112445,#112446,
#112447,#112448,#112449,#112450,#112451,#112452,#112453,#112454,#112455,
#112456,#112457,#112458,#112459,#112460,#112461,#112462,#112463,#112464,
#112465,#112466,#112467,#112468,#112469,#112470,#112471,#112472,#112473,
#112474,#112475,#112476,#112477,#112478,#112479,#112480,#112481,#112482,
#112483,#112484,#112485,#112486,#112487,#112488,#112489,#112490,#112491,
#112492,#112493,#112494,#112495,#112496,#112497,#112498,#112499,#112500,
#112501,#112502,#112503,#112504,#112505,#112506,#112507,#112508,#112509,
#112510,#112511,#112512,#112513,#112514,#112515,#112516,#112517,#112518,
#112519,#112520,#112521,#112522,#112523,#112524,#112525,#112526,#112527,
#112528,#112529,#112530,#112531,#112532,#112533,#112534,#112535,#112536,
#112537),.UNSPECIFIED.,.F.,.F.,(4,2,2,2,2,2,2,2,2,2,2,2,2,2,2,2,2,2,2,2,
2,2,2,2,2,2,2,2,2,2,2,2,2,2,2,2,2,2,2,2,2,2,2,2,2,2,2,2,2,2,2,2,2,2,2,2,
2,2,2,2,2,2,2,2,2,2,2,2,2,2,2,2,2,2,2,2,2,2,2,2,2,2,2,2,2,2,2,2,2,2,2,2,
2,2,2,2,2,2,2,2,2,2,2,2,2,2,2,2,2,2,4),(-1.2596092791427,-1.21011169664944,
-1.20367842859327,-1.20117006796674,-1.19935221036289,-1.19740891969948,
-1.19480671370743,-1.1889829925253,-1.16514965425979,-1.11614969218952,
-1.09779132074701,-1.09505198071949,-1.09369779134588,-1.09262569009982,
-1.09137327188847,-1.0891211707322,-1.07817664855281,-1.05366042450533,
-0.998557438618785,-0.991850234273926,-0.989297617185117,-0.987467749012962,
-0.985530072311542,-0.982966815170316,-0.977359082047891,-0.929076048470101,
-0.888723759846889,-0.884011357367577,-0.882271376440202,-0.881246090678849,
-0.880154657239091,-0.878645369768322,-0.87506288280695,-0.870037819142832,
-0.856214195879545,-0.833860460614285,-0.787184959555151,-0.779989405419897,
-0.777074397744445,-0.775273882355138,-0.77332206248597,-0.770660435232421,
-0.764492433475752,-0.737950307557521,-0.698623437672005,-0.68728966454219,
-0.673503806106148,-0.671211322848425,-0.669826564557874,-0.668750112408046,
-0.667534999889146,-0.665449740786321,-0.656909155741711,-0.640351409192942,
-0.598279168069409,-0.571099321214126,-0.566971768417946,-0.564478936343208,
-0.562545193753715,-0.560449533462879,-0.557102035727017,-0.545904467008763,
-0.527329643544558,-0.484795377006182,-0.462028090530099,-0.459170447779128,
-0.457791834481783,-0.456715570669755,-0.455474553101724,-0.453286801311886,
-0.443432679424966,-0.394231696149154,-0.359839482001392,-0.355551793568,
-0.353009797948434,-0.351065419758364,-0.348985119919028,-0.345719059516173,
-0.335297165786895,-0.318505114312126,-0.258883412648892,-0.249294304900512,
-0.247244964361322,-0.24591834496186,-0.244851306982384,-0.243841592595941,
-0.241869215319139,-0.23445132044746,-0.220918198218288,-0.192338068365553,
-0.147271574269591,-0.143024776704226,-0.140506721051313,-0.138580725286331,
-0.136520297076973,-0.133286153483837,-0.122977264284867,-0.106384825868077,
-0.0845186660431512,-0.0739384345445597,-0.0616384513993995,-0.0559535320440041,
-0.0377853867776285,-0.0350633807398456,-0.0337175017363041,-0.0326484251826848,
-0.0316335581109729,-0.030396058734142,-0.0285520611649711,-0.0215326044775512,
-0.00065556807277999),.UNSPECIFIED.);
#1080=B_SPLINE_CURVE_WITH_KNOTS('',3,(#112538,#112539,#112540,#112541,#112542,
#112543,#112544,#112545,#112546,#112547,#112548,#112549,#112550),
 .UNSPECIFIED.,.F.,.F.,(4,3,3,3,4),(-3.8410390329882,-3.7391698932069,-3.63740763660875,
-3.53571859652656,-3.4905420523601),.UNSPECIFIED.);
#1081=B_SPLINE_CURVE_WITH_KNOTS('',3,(#112553,#112554,#112555,#112556,#112557,
#112558,#112559,#112560,#112561,#112562,#112563,#112564,#112565),
 .UNSPECIFIED.,.F.,.F.,(4,3,3,3,4),(7.2430409600995,7.34752291120672,7.45192118821202,
7.55626814755434,7.5925217232362),.UNSPECIFIED.);
#1082=B_SPLINE_CURVE_WITH_KNOTS('',3,(#112566,#112567,#112568,#112569,#112570,
#112571,#112572,#112573,#112574,#112575,#112576,#112577,#112578,#112579,
#112580,#112581,#112582,#112583,#112584,#112585,#112586,#112587,#112588,
#112589,#112590,#112591,#112592,#112593,#112594,#112595,#112596,#112597,
#112598,#112599,#112600,#112601,#112602,#112603,#112604,#112605,#112606,
#112607,#112608,#112609,#112610,#112611,#112612,#112613,#112614,#112615,
#112616,#112617,#112618,#112619,#112620,#112621,#112622,#112623,#112624,
#112625,#112626,#112627,#112628,#112629,#112630,#112631,#112632,#112633,
#112634,#112635,#112636,#112637,#112638,#112639,#112640,#112641,#112642,
#112643,#112644,#112645,#112646,#112647,#112648,#112649,#112650,#112651,
#112652,#112653,#112654,#112655,#112656,#112657,#112658,#112659,#112660,
#112661,#112662,#112663,#112664,#112665,#112666,#112667,#112668,#112669,
#112670,#112671,#112672,#112673,#112674,#112675,#112676,#112677,#112678,
#112679,#112680,#112681,#112682,#112683,#112684,#112685,#112686,#112687,
#112688,#112689,#112690,#112691,#112692,#112693,#112694,#112695,#112696,
#112697,#112698,#112699,#112700,#112701,#112702,#112703,#112704,#112705,
#112706,#112707,#112708,#112709,#112710,#112711,#112712,#112713,#112714,
#112715,#112716,#112717,#112718,#112719,#112720,#112721,#112722,#112723,
#112724,#112725,#112726,#112727,#112728,#112729,#112730,#112731,#112732,
#112733,#112734,#112735,#112736,#112737,#112738,#112739,#112740,#112741,
#112742,#112743,#112744,#112745,#112746,#112747,#112748,#112749,#112750,
#112751,#112752,#112753,#112754,#112755,#112756,#112757,#112758,#112759,
#112760,#112761,#112762,#112763,#112764,#112765,#112766,#112767,#112768,
#112769,#112770,#112771,#112772,#112773,#112774,#112775,#112776,#112777,
#112778,#112779,#112780,#112781,#112782,#112783,#112784,#112785,#112786,
#112787,#112788,#112789,#112790,#112791),.UNSPECIFIED.,.F.,.F.,(4,2,2,2,
2,2,2,2,2,2,2,2,2,2,2,2,2,2,2,2,2,2,2,2,2,2,2,2,2,2,2,2,2,2,2,2,2,2,2,2,
2,2,2,2,2,2,2,2,2,2,2,2,2,2,2,2,2,2,2,2,2,2,2,2,2,2,2,2,2,2,2,2,2,2,2,2,
2,2,2,2,2,2,2,2,2,2,2,2,2,2,2,2,2,2,2,2,2,2,2,2,2,2,2,2,2,2,2,2,2,2,2,2,
4),(-2.66730687879803,-2.64516059795848,-2.59597250440395,-2.58663388874494,
-2.5844897853591,-2.58326240108112,-2.58218815896832,-2.58080107566422,
-2.57789455211048,-2.55020246391889,-2.51345475354417,-2.49429362638936,
-2.48671793935886,-2.48279836081912,-2.47949437709281,-2.47744121871936,
-2.47560711525565,-2.47317516578146,-2.46933881710637,-2.44888830435509,
-2.3998575173308,-2.3832044732505,-2.37463043778995,-2.37254157870367,-2.37132511676415,
-2.3702477505218,-2.368862206611,-2.36656943007814,-2.35280908560213,-2.35171480594859,
-2.34963344277311,-2.30368328812431,-2.27577856566349,-2.26944174036203,
-2.26674961218141,-2.26479103304299,-2.26299511854612,-2.26011144819991,
-2.2531125500284,-2.20169140113042,-2.17461056513675,-2.16300964613649,
-2.16072083305361,-2.15946101282519,-2.15839020276534,-2.15704748826761,
-2.15444827237636,-2.13891199681551,-2.13228535013131,-2.1184757802571,
-2.08559518754418,-2.0690389600921,-2.05873191624902,-2.05548404415292,
-2.05341116103188,-2.05147082788239,-2.04893001766635,-2.04463543408901,
-2.00949876012414,-1.96055909398235,-1.95084670976453,-1.94867482579937,
-1.94744053815821,-1.94636677209731,-1.94498829159577,-1.94212595516369,
-1.91876781382108,-1.90647077296417,-1.87360301875142,-1.8570639634473,
-1.84676408733396,-1.84351653107586,-1.84144337474289,-1.83950244969533,
-1.83696037575888,-1.83266254759222,-1.79732162117904,-1.7481497180924,
-1.73883263765423,-1.73668819264555,-1.73545973234315,-1.7343848508444,
-1.7329966777096,-1.73008492616404,-1.69805682769749,-1.66514389826425,
-1.64631723445147,-1.63883302738929,-1.63321085945028,-1.63064531779105,
-1.62870768911201,-1.62687918423403,-1.62433059999678,-1.6176470674001,
-1.5622562402909,-1.53791466010126,-1.52701604297646,-1.52476747025897,
-1.52351620259121,-1.52244430765029,-1.52108954685869,-1.51843545613556,
-1.50155365029971,-1.48276663059011,-1.44980183034579,-1.43314918401495,
-1.42279779605753,-1.41954421199193,-1.41746965803777,-1.41552914480069,
-1.41299009135711,-1.40870293095995,-1.40833650609706),.UNSPECIFIED.);
#1083=B_SPLINE_CURVE_WITH_KNOTS('',3,(#112793,#112794,#112795,#112796,#112797,
#112798,#112799,#112800,#112801,#112802,#112803,#112804,#112805,#112806,
#112807,#112808,#112809,#112810,#112811,#112812,#112813,#112814,#112815,
#112816,#112817,#112818,#112819,#112820,#112821,#112822,#112823,#112824,
#112825,#112826,#112827,#112828,#112829,#112830,#112831,#112832,#112833,
#112834,#112835,#112836,#112837,#112838,#112839,#112840,#112841,#112842,
#112843,#112844,#112845,#112846,#112847,#112848,#112849,#112850,#112851,
#112852,#112853,#112854,#112855,#112856,#112857,#112858,#112859,#112860,
#112861,#112862,#112863,#112864,#112865,#112866,#112867,#112868,#112869,
#112870,#112871,#112872,#112873,#112874,#112875,#112876,#112877,#112878,
#112879,#112880,#112881,#112882,#112883,#112884,#112885,#112886,#112887,
#112888,#112889,#112890,#112891,#112892,#112893,#112894,#112895,#112896,
#112897,#112898,#112899,#112900,#112901,#112902,#112903,#112904,#112905,
#112906,#112907,#112908,#112909,#112910,#112911,#112912,#112913,#112914,
#112915,#112916,#112917,#112918,#112919,#112920,#112921,#112922,#112923,
#112924,#112925,#112926,#112927,#112928,#112929,#112930,#112931,#112932,
#112933,#112934,#112935,#112936,#112937,#112938,#112939,#112940,#112941,
#112942,#112943,#112944,#112945,#112946,#112947,#112948,#112949,#112950,
#112951,#112952,#112953,#112954,#112955,#112956,#112957,#112958,#112959,
#112960,#112961,#112962,#112963,#112964,#112965,#112966,#112967,#112968,
#112969,#112970,#112971,#112972,#112973,#112974,#112975,#112976,#112977,
#112978,#112979,#112980,#112981,#112982,#112983,#112984,#112985,#112986,
#112987,#112988,#112989,#112990,#112991,#112992,#112993,#112994,#112995,
#112996,#112997,#112998,#112999,#113000,#113001,#113002,#113003,#113004,
#113005,#113006,#113007,#113008,#113009,#113010,#113011,#113012,#113013,
#113014),.UNSPECIFIED.,.F.,.F.,(4,2,2,2,2,2,2,2,2,2,2,2,2,2,2,2,2,2,2,2,
2,2,2,2,2,2,2,2,2,2,2,2,2,2,2,2,2,2,2,2,2,2,2,2,2,2,2,2,2,2,2,2,2,2,2,2,
2,2,2,2,2,2,2,2,2,2,2,2,2,2,2,2,2,2,2,2,2,2,2,2,2,2,2,2,2,2,2,2,2,2,2,2,
2,2,2,2,2,2,2,2,2,2,2,2,2,2,2,2,2,2,4),(-1.25960927882884,-1.21011169532823,
-1.20367842731546,-1.20117006670425,-1.19935220911066,-1.19740891845822,
-1.1948067124806,-1.18898299132885,-1.16514965315903,-1.11614969077259,
-1.09779132013028,-1.09505198012728,-1.09369779075751,-1.09262568950179,
-1.09137327125847,-1.08912117002723,-1.07817664712381,-1.05366042041119,
-0.998557440635837,-0.991850235923305,-0.989297618760896,-0.987467750555575,
-0.985530073836942,-0.982966816703447,-0.977359083717694,-0.929076070422091,
-0.888723762183214,-0.884011358744775,-0.882271377671097,-0.881246091880497,
-0.880154658488213,-0.878645371172887,-0.875062884953175,-0.870037822588928,
-0.85621420444147,-0.833860409293135,-0.787184961841286,-0.77998940663088,
-0.777074398830036,-0.775273883459694,-0.773322063687082,-0.770660436701997,
-0.764492436189761,-0.737950319646653,-0.698623490627323,-0.687289707791117,
-0.673503810242227,-0.671211325147951,-0.669826566341357,-0.668750114159319,
-0.667535002020493,-0.665449744515916,-0.656909179027754,-0.64035148951231,
-0.598279190791866,-0.571099318538436,-0.56697176508342,-0.564478932820849,
-0.562545190211058,-0.560449530023899,-0.557102032726576,-0.545904468030332,
-0.527329653789821,-0.484795151298745,-0.462028080676498,-0.45917044328081,
-0.457791831008699,-0.456715567213456,-0.455474548760424,-0.45328679339357,
-0.44343262163769,-0.394231669735219,-0.359839489357513,-0.355551801319755,
-0.353009805714651,-0.351065427406005,-0.348985127312124,-0.345719066239315,
-0.335297168033496,-0.318505107132256,-0.258883419254725,-0.249294309271303,
-0.247244968541648,-0.245918349068586,-0.24485131111036,-0.243841596870197,
-0.241869219986305,-0.234451327593885,-0.220918211360422,-0.192338078805669,
-0.147271574900182,-0.143024777879832,-0.140506722555446,-0.138580727046731,
-0.136520299117926,-0.133286155983296,-0.122977268470218,-0.106384833205498,
-0.0845186705986564,-0.0739384475260423,-0.0616384583542045,-0.0559534378375188,
-0.03778538222746,-0.0350633794114932,-0.0337175011687427,-0.0326484248162633,
-0.0316335578296692,-0.0303960582785997,-0.028552060096841,-0.0215326025070754,
-0.000655568373725938),.UNSPECIFIED.);
#1084=B_SPLINE_CURVE_WITH_KNOTS('',3,(#113015,#113016,#113017,#113018,#113019,
#113020,#113021,#113022,#113023,#113024,#113025,#113026,#113027),
 .UNSPECIFIED.,.F.,.F.,(4,3,3,3,4),(-3.84103903298819,-3.73916989309881,
-3.63740763642035,-3.53571859629846,-3.4905420525369),.UNSPECIFIED.);
#1085=B_SPLINE_CURVE_WITH_KNOTS('',3,(#113030,#113031,#113032,#113033,#113034,
#113035,#113036,#113037,#113038,#113039,#113040,#113041,#113042),
 .UNSPECIFIED.,.F.,.F.,(4,3,3,3,4),(7.24304101724442,7.34752294213327,7.45192119271409,
7.5562681254478,7.5925217232362),.UNSPECIFIED.);
#1086=B_SPLINE_CURVE_WITH_KNOTS('',3,(#113043,#113044,#113045,#113046,#113047,
#113048,#113049,#113050,#113051,#113052,#113053,#113054,#113055,#113056,
#113057,#113058,#113059,#113060,#113061,#113062,#113063,#113064,#113065,
#113066,#113067,#113068,#113069,#113070,#113071,#113072,#113073,#113074,
#113075,#113076,#113077,#113078,#113079,#113080,#113081,#113082,#113083,
#113084,#113085,#113086,#113087,#113088,#113089,#113090,#113091,#113092,
#113093,#113094,#113095,#113096,#113097,#113098,#113099,#113100,#113101,
#113102,#113103,#113104,#113105,#113106,#113107,#113108,#113109,#113110,
#113111,#113112,#113113,#113114,#113115,#113116,#113117,#113118,#113119,
#113120,#113121,#113122,#113123,#113124,#113125,#113126,#113127,#113128,
#113129,#113130,#113131,#113132,#113133,#113134,#113135,#113136,#113137,
#113138,#113139,#113140,#113141,#113142,#113143,#113144,#113145,#113146,
#113147,#113148,#113149,#113150,#113151,#113152,#113153,#113154,#113155,
#113156,#113157,#113158,#113159,#113160,#113161,#113162,#113163,#113164,
#113165,#113166,#113167,#113168,#113169,#113170,#113171,#113172,#113173,
#113174,#113175,#113176,#113177,#113178,#113179,#113180,#113181,#113182,
#113183,#113184,#113185,#113186,#113187,#113188,#113189,#113190,#113191,
#113192,#113193,#113194,#113195,#113196,#113197,#113198,#113199,#113200,
#113201,#113202,#113203,#113204,#113205,#113206,#113207,#113208,#113209,
#113210,#113211,#113212,#113213,#113214,#113215,#113216,#113217,#113218,
#113219,#113220,#113221,#113222,#113223,#113224,#113225,#113226,#113227,
#113228,#113229,#113230,#113231,#113232,#113233,#113234,#113235,#113236,
#113237,#113238,#113239,#113240,#113241,#113242,#113243,#113244,#113245,
#113246,#113247,#113248,#113249,#113250,#113251,#113252,#113253,#113254,
#113255,#113256,#113257,#113258),.UNSPECIFIED.,.F.,.F.,(4,2,2,2,2,2,2,2,
2,2,2,2,2,2,2,2,2,2,2,2,2,2,2,2,2,2,2,2,2,2,2,2,2,2,2,2,2,2,2,2,2,2,2,2,
2,2,2,2,2,2,2,2,2,2,2,2,2,2,2,2,2,2,2,2,2,2,2,2,2,2,2,2,2,2,2,2,2,2,2,2,
2,2,2,2,2,2,2,2,2,2,2,2,2,2,2,2,2,2,2,2,2,2,2,2,2,2,2,4),(-2.66731151661852,
-2.64527185279398,-2.59640216442595,-2.58668066625757,-2.58450952792302,
-2.58327612034247,-2.5822027106984,-2.58082465065772,-2.57796472130922,
-2.54188915064359,-2.50916127755015,-2.49278663887684,-2.48599210724353,
-2.48236584360222,-2.47926527249087,-2.47725867411702,-2.47531737148135,
-2.47277568511123,-2.46848045684978,-2.43348606520522,-2.38457210454266,
-2.37475884470456,-2.37257893914507,-2.37134230128741,-2.37026831322801,
-2.36889163335558,-2.36603913620571,-2.32973367110866,-2.27586869803088,
-2.26941107622515,-2.26669839730375,-2.26473602260654,-2.26294429953827,
-2.26008406699031,-2.25322794818502,-2.19978060101934,-2.17412315671989,
-2.16288001130005,-2.16061141503366,-2.15935593733485,-2.15828470191138,
-2.15693621006764,-2.1543104172533,-2.13814252822413,-2.09165928558698,
-2.06369635954698,-2.05735261406887,-2.0546594631257,-2.05270084790813,
-2.05090539161289,-2.04802353856523,-2.04103459607239,-1.9894622732371,
-1.96249380035042,-1.95092069309849,-1.94863343629199,-1.94737395496668,
-1.94630298714801,-1.94495955402626,-1.94235776759311,-1.92677008376512,
-1.92028688316622,-1.9063874221587,-1.87350459214437,-1.85694733158858,
-1.84663922694345,-1.84339073145481,-1.84131737338695,-1.83937653898136,
-1.8368349871214,-1.83253894587197,-1.7973408108906,-1.74809994649225,-1.73871504219033,
-1.73656572820817,-1.73533619628985,-1.734261494231,-1.73287502528677,-1.72997202728907,
-1.69791050362839,-1.66501814149649,-1.6461912354045,-1.63870697009884,
-1.63308477158178,-1.63051922950906,-1.62858160605694,-1.62675311019602,
-1.6242045451054,-1.61752110285484,-1.56212974443479,-1.53778871066859,
-1.52689025439241,-1.52464169684738,-1.52339043512033,-1.5223185437245,
-1.52096378545313,-1.51830969384103,-1.50142768119834,-1.48264098203071,
-1.44967629550916,-1.43302371015258,-1.42267235932078,-1.41941878660761,
-1.41734423982245,-1.41540373324461,-1.41286468844989,-1.40857754252068,
-1.40821110954925),.UNSPECIFIED.);
#1087=B_SPLINE_CURVE_WITH_KNOTS('',3,(#113260,#113261,#113262,#113263,#113264,
#113265,#113266,#113267,#113268,#113269,#113270,#113271,#113272,#113273,
#113274,#113275,#113276,#113277,#113278,#113279,#113280,#113281,#113282,
#113283,#113284,#113285,#113286,#113287,#113288,#113289,#113290,#113291,
#113292,#113293,#113294,#113295,#113296,#113297,#113298,#113299,#113300,
#113301,#113302,#113303,#113304,#113305,#113306,#113307,#113308,#113309,
#113310,#113311,#113312,#113313,#113314,#113315,#113316,#113317,#113318,
#113319,#113320,#113321,#113322,#113323,#113324,#113325,#113326,#113327,
#113328,#113329,#113330,#113331,#113332,#113333,#113334,#113335,#113336,
#113337,#113338,#113339,#113340,#113341,#113342,#113343,#113344,#113345,
#113346,#113347,#113348,#113349,#113350,#113351,#113352,#113353,#113354,
#113355,#113356,#113357,#113358,#113359,#113360,#113361,#113362,#113363,
#113364,#113365,#113366,#113367,#113368,#113369,#113370,#113371,#113372,
#113373,#113374,#113375,#113376,#113377,#113378,#113379,#113380,#113381,
#113382,#113383,#113384,#113385,#113386,#113387,#113388,#113389,#113390,
#113391,#113392,#113393,#113394,#113395,#113396,#113397,#113398,#113399,
#113400,#113401,#113402,#113403,#113404,#113405,#113406,#113407,#113408,
#113409,#113410,#113411,#113412,#113413,#113414,#113415,#113416,#113417,
#113418,#113419,#113420,#113421,#113422,#113423,#113424,#113425,#113426,
#113427,#113428,#113429,#113430,#113431,#113432,#113433,#113434,#113435,
#113436,#113437,#113438,#113439,#113440,#113441,#113442,#113443,#113444,
#113445,#113446,#113447,#113448,#113449,#113450,#113451,#113452,#113453,
#113454,#113455,#113456,#113457,#113458,#113459,#113460,#113461,#113462,
#113463,#113464,#113465,#113466,#113467,#113468,#113469,#113470,#113471,
#113472,#113473,#113474,#113475,#113476,#113477,#113478,#113479,#113480,
#113481),.UNSPECIFIED.,.F.,.F.,(4,2,2,2,2,2,2,2,2,2,2,2,2,2,2,2,2,2,2,2,
2,2,2,2,2,2,2,2,2,2,2,2,2,2,2,2,2,2,2,2,2,2,2,2,2,2,2,2,2,2,2,2,2,2,2,2,
2,2,2,2,2,2,2,2,2,2,2,2,2,2,2,2,2,2,2,2,2,2,2,2,2,2,2,2,2,2,2,2,2,2,2,2,
2,2,2,2,2,2,2,2,2,2,2,2,2,2,2,2,2,2,4),(-1.25960928830829,-1.2101117100023,
-1.20367844137046,-1.20117008054523,-1.199352222804,-1.19740893200012,-1.19480672582928,
-1.18898300427882,-1.1651496649384,-1.11614970833641,-1.09779132516482,
-1.09505198479947,-1.09369779538215,-1.09262569429207,-1.091373276574,-1.08912117655308,
-1.07817666520136,-1.05366048074937,-0.998557406439847,-0.991850207608283,
-0.989297591648701,-0.987467723994383,-0.985530047576476,-0.982966790367328,
-0.977359055330417,-0.929075722515686,-0.888723725139279,-0.88401133694563,
-0.882271358220582,-0.881246072913938,-0.8801546388005,-0.878645349061097,
-0.875062851212622,-0.870037768440905,-0.856214069864457,-0.833861217404663,
-0.787184926908894,-0.779989388727153,-0.777074382950992,-0.77527386731896,
-0.773322046068984,-0.770660414921931,-0.764492394996883,-0.737950131824738,
-0.698622662555807,-0.687289036438417,-0.673503748242721,-0.671211291792618,
-0.669826541041902,-0.668750089367687,-0.66753497130969,-0.665449688919358,
-0.656908818831688,-0.640350240953428,-0.598278838009361,-0.571099362543136,
-0.566971819389208,-0.564478990064701,-0.562545247774404,-0.560449585972271,
-0.557102081837438,-0.545904454396437,-0.527329496232905,-0.484798680915965,
-0.462028237451359,-0.459170516350986,-0.457791888052064,-0.456715623980624,
-0.45547461932324,-0.453286919802481,-0.443433527039587,-0.394232083469812,
-0.359839378033064,-0.355551683815739,-0.35300968797315,-0.351065311500599,
-0.348985015352746,-0.34571896466666,-0.335297135909555,-0.31850522127589,
-0.258883319425073,-0.24929424390937,-0.247244906115271,-0.245918287774539,
-0.244851249483811,-0.243841532970202,-0.241869149982625,-0.234451219181236,
-0.220918010117147,-0.192337919011177,-0.147271566506105,-0.143024761003124,
-0.140506700568832,-0.138580701068639,-0.136520268764679,-0.133286118483809,
-0.122977204712598,-0.106384720379404,-0.084518600633027,-0.0739382468765593,
-0.0616383509458848,-0.0559548978942787,-0.0377854527850606,-0.0350634000144293,
-0.0337175099674206,-0.0326484304901323,-0.0316335621886587,-0.0303960653396582,
-0.0285520766491967,-0.0215326330435678,-0.000655563710816865),
 .UNSPECIFIED.);
#1088=B_SPLINE_CURVE_WITH_KNOTS('',3,(#113482,#113483,#113484,#113485,#113486,
#113487,#113488,#113489,#113490,#113491,#113492,#113493,#113494),
 .UNSPECIFIED.,.F.,.F.,(4,3,3,3,4),(-3.84103903298818,-3.73916989476587,
-3.63740763932563,-3.5357185998273,-3.49054210138362),.UNSPECIFIED.);
#1089=B_SPLINE_CURVE_WITH_KNOTS('',3,(#113497,#113498,#113499,#113500,#113501,
#113502,#113503,#113504,#113505,#113506,#113507,#113508,#113509,#113510,
#113511,#113512,#113513,#113514,#113515,#113516,#113517,#113518,#113519,
#113520,#113521,#113522,#113523,#113524,#113525,#113526,#113527,#113528,
#113529,#113530,#113531,#113532,#113533,#113534,#113535,#113536,#113537,
#113538,#113539,#113540,#113541,#113542,#113543,#113544,#113545,#113546,
#113547,#113548,#113549,#113550,#113551,#113552,#113553,#113554,#113555,
#113556,#113557,#113558,#113559,#113560,#113561,#113562,#113563,#113564,
#113565,#113566,#113567,#113568,#113569,#113570,#113571,#113572,#113573,
#113574,#113575,#113576,#113577,#113578,#113579,#113580,#113581,#113582,
#113583,#113584,#113585,#113586,#113587,#113588,#113589,#113590,#113591,
#113592,#113593,#113594,#113595,#113596,#113597,#113598,#113599,#113600,
#113601,#113602,#113603,#113604,#113605,#113606,#113607,#113608,#113609,
#113610,#113611,#113612,#113613,#113614,#113615,#113616,#113617,#113618,
#113619,#113620,#113621,#113622,#113623,#113624,#113625,#113626,#113627,
#113628,#113629,#113630,#113631,#113632,#113633,#113634,#113635,#113636,
#113637,#113638,#113639,#113640,#113641,#113642,#113643,#113644,#113645,
#113646,#113647,#113648,#113649,#113650,#113651,#113652,#113653,#113654,
#113655,#113656,#113657,#113658,#113659,#113660,#113661,#113662,#113663,
#113664,#113665,#113666,#113667,#113668,#113669,#113670,#113671,#113672,
#113673,#113674,#113675,#113676,#113677,#113678,#113679,#113680,#113681,
#113682,#113683,#113684,#113685,#113686,#113687,#113688,#113689,#113690,
#113691,#113692,#113693,#113694,#113695,#113696,#113697,#113698,#113699,
#113700,#113701,#113702,#113703,#113704,#113705,#113706,#113707),
 .UNSPECIFIED.,.F.,.F.,(4,3,3,3,3,3,3,3,3,3,3,3,3,3,3,3,3,3,3,3,3,3,3,3,
3,3,3,3,3,3,3,3,3,3,3,3,3,3,3,3,3,3,3,3,3,3,3,3,3,3,3,3,3,3,3,3,3,3,3,3,
3,3,3,3,3,3,3,3,3,3,4),(7.94826257357117,8.03933917600296,8.13040880367845,
8.22150057347938,8.28490746193705,8.37600652726715,8.46708731777336,8.55817079881158,
8.64924995373853,8.74034821484711,8.77225495969805,8.86358513560277,8.9548986330717,
9.04621476194116,9.1375258664909,9.22885308111593,9.25960245745905,9.35004385837792,
9.44046482582385,9.53089150074111,9.62131715354628,9.7117720080883,9.74694995522006,
9.83977478998513,9.93258815792015,10.025393459506,10.1181816912061,10.2109546401573,
10.2342974529811,10.3226295283866,10.410939313145,10.4992670123095,10.5876031247876,
10.6759967918602,10.7216449507421,10.8173001765085,10.9152232445072,11.0108032234786,
11.1098978359908,11.2089924485031,11.2974448715171,11.3858946564481,11.4743908456245,
11.562911632656,11.6515132694445,11.6963399462641,11.7845989400825,11.872784715549,
11.9609169884106,12.0496817325825,12.1377840060822,12.22589474066,12.31403174787,
12.403282546349,12.4915728517076,12.5813038967469,12.6710349417861,12.7563671078331,
12.8415835245525,12.9267079378408,13.011763973049,13.0967844578901,13.1817894416759,
13.2668001713248,13.3518378971159,13.4369760189292,13.5221713946028,13.6075027101629,
13.6457299373081,13.775760012771,13.8747245557601),.UNSPECIFIED.);
#1090=B_SPLINE_CURVE_WITH_KNOTS('',3,(#113708,#113709,#113710,#113711,#113712,
#113713,#113714,#113715,#113716,#113717,#113718,#113719,#113720,#113721,
#113722,#113723),.UNSPECIFIED.,.F.,.F.,(4,3,3,3,3,4),(13.8747245559395,
13.9640191448913,14.0502852614935,14.1364993985763,14.2226809109192,14.2319029117468),
 .UNSPECIFIED.);
#1091=B_SPLINE_CURVE_WITH_KNOTS('',3,(#113725,#113726,#113727,#113728,#113729,
#113730,#113731,#113732,#113733,#113734,#113735,#113736,#113737),
 .UNSPECIFIED.,.F.,.F.,(4,3,3,3,4),(-10.49477808198,-10.4064650448213,-10.3181276030325,
-10.2342974529811,-10.1382057107015),.UNSPECIFIED.);
#1092=B_SPLINE_CURVE_WITH_KNOTS('',3,(#113738,#113739,#113740,#113741,#113742,
#113743,#113744,#113745,#113746,#113747,#113748,#113749,#113750,#113751,
#113752,#113753,#113754,#113755,#113756,#113757,#113758,#113759,#113760,
#113761,#113762,#113763,#113764,#113765,#113766,#113767,#113768,#113769,
#113770,#113771,#113772,#113773,#113774,#113775,#113776,#113777,#113778,
#113779,#113780,#113781,#113782,#113783,#113784,#113785,#113786,#113787,
#113788,#113789),.UNSPECIFIED.,.F.,.F.,(4,2,2,2,2,2,2,2,2,2,2,2,2,2,2,2,
2,2,2,2,2,2,2,2,2,4),(1.80129261558726,1.89085724581047,1.95815067052896,
2.04087191045445,2.16781420139301,2.30159864887717,2.38018379042639,2.50753373614498,
2.58026236347961,2.72352021082451,2.80830108353013,2.89228193268548,3.05888345033062,
3.13851550682636,3.22568042995156,3.3096718361238,3.47401737896509,3.55360256241736,
3.69279581467806,3.77292072282912,3.8403007617186,3.92420528255271,4.09335994867267,
4.20858348747028,4.27205568576047,4.33574044619876),.UNSPECIFIED.);
#1093=B_SPLINE_CURVE_WITH_KNOTS('',3,(#113791,#113792,#113793,#113794,#113795,
#113796,#113797,#113798,#113799,#113800,#113801,#113802,#113803,#113804,
#113805,#113806,#113807,#113808,#113809,#113810,#113811,#113812,#113813,
#113814,#113815,#113816,#113817,#113818,#113819,#113820,#113821,#113822,
#113823,#113824,#113825,#113826,#113827,#113828,#113829,#113830,#113831,
#113832,#113833,#113834,#113835,#113836,#113837,#113838,#113839,#113840,
#113841,#113842,#113843,#113844),.UNSPECIFIED.,.F.,.F.,(4,2,2,2,2,2,2,2,
2,2,2,2,2,2,2,2,2,2,2,2,2,2,2,2,2,2,4),(-2.84070125419267,-2.78020516982207,
-2.65435179246817,-2.57659131794918,-2.4969909063458,-2.32946562003716,
-2.24549752924312,-2.17252648783871,-2.05532984848559,-1.97398064924123,
-1.85252487658554,-1.68460873253962,-1.51626211229805,-1.442685683892,-1.30223160143275,
-1.22322244978935,-1.10078998236665,-1.03027786474523,-0.859932808523249,
-0.777908083368037,-0.656316970603006,-0.575106553635839,-0.460076680830133,
-0.393722373564878,-0.309798675310045,-0.154355410284551,-0.153225104208862),
 .UNSPECIFIED.);
#1094=B_SPLINE_CURVE_WITH_KNOTS('',3,(#113846,#113847,#113848,#113849,#113850,
#113851,#113852,#113853,#113854,#113855,#113856,#113857,#113858,#113859,
#113860,#113861,#113862,#113863,#113864,#113865,#113866,#113867,#113868,
#113869,#113870,#113871,#113872,#113873,#113874,#113875,#113876,#113877,
#113878,#113879,#113880,#113881,#113882,#113883,#113884,#113885,#113886,
#113887,#113888,#113889,#113890,#113891,#113892,#113893,#113894,#113895,
#113896,#113897,#113898,#113899,#113900,#113901,#113902,#113903,#113904,
#113905,#113906,#113907,#113908,#113909,#113910,#113911,#113912,#113913,
#113914,#113915,#113916,#113917,#113918,#113919,#113920,#113921,#113922,
#113923,#113924,#113925,#113926,#113927,#113928,#113929,#113930,#113931,
#113932,#113933,#113934,#113935,#113936,#113937,#113938,#113939,#113940,
#113941,#113942,#113943,#113944,#113945,#113946,#113947,#113948,#113949,
#113950,#113951,#113952,#113953,#113954,#113955,#113956,#113957,#113958,
#113959,#113960,#113961,#113962,#113963,#113964,#113965,#113966,#113967,
#113968,#113969,#113970,#113971,#113972,#113973,#113974,#113975,#113976,
#113977,#113978,#113979,#113980,#113981,#113982,#113983,#113984,#113985,
#113986,#113987,#113988,#113989,#113990,#113991,#113992,#113993,#113994,
#113995,#113996,#113997,#113998,#113999,#114000,#114001,#114002,#114003,
#114004,#114005,#114006,#114007,#114008,#114009,#114010,#114011,#114012,
#114013,#114014,#114015,#114016,#114017,#114018,#114019,#114020,#114021,
#114022,#114023,#114024,#114025,#114026,#114027,#114028,#114029,#114030,
#114031,#114032,#114033,#114034,#114035,#114036,#114037,#114038,#114039,
#114040,#114041,#114042,#114043,#114044,#114045,#114046,#114047,#114048,
#114049,#114050,#114051,#114052,#114053,#114054,#114055,#114056,#114057,
#114058,#114059),.UNSPECIFIED.,.F.,.F.,(4,3,3,3,3,3,3,3,3,3,3,3,3,3,3,3,
3,3,3,3,3,3,3,3,3,3,3,3,3,3,3,3,3,3,3,3,3,3,3,3,3,3,3,3,3,3,3,3,3,3,3,3,
3,3,3,3,3,3,3,3,3,3,3,3,3,3,3,3,3,3,3,4),(20.5146317045532,20.6057411498849,
20.6968511934372,20.7879526845016,20.879076798166,20.9559424037231,21.0470612888528,
21.1381622720158,21.2292662857086,21.3203661134592,21.4114850765015,21.4432899014841,
21.5344090066244,21.6255102040649,21.7166144214506,21.8077144461872,21.8988335947371,
21.9306373992451,22.0217552957911,22.1128552867068,22.2039583127407,22.2950571581876,
22.3861751549738,22.4179848970061,22.5091059022033,22.6002090058036,22.6913151191521,
22.7824170287616,22.8735380301917,22.9053323947671,22.9964483174135,23.0875463337701,
23.1786474040368,23.2697443099321,23.3608604070626,23.3926798925281,23.4838001385027,
23.5749024646883,23.6660077819953,23.7571088869989,23.8482290782052,23.8800273902891,
23.9711543330786,24.0622634337937,24.1533755706366,24.2444835024034,24.3356104731702,
24.3673748880501,24.4584575658978,24.5495221768875,24.6405899421199,24.7316536918334,
24.82273712851,24.8547223858111,24.9459385829945,25.037137248471,25.1283384958124,
25.2195350261609,25.3107491009262,25.3420698835722,25.4329784991865,25.5238689926783,
25.6147642806767,25.7056569563173,25.7965727963716,25.8294173813332,25.9210352148413,
26.0126339675887,26.1042287090123,26.1958136721735,26.2874053890112,26.3167648790942),
 .UNSPECIFIED.);
#1095=B_SPLINE_CURVE_WITH_KNOTS('',3,(#114063,#114064,#114065,#114066,#114067,
#114068,#114069,#114070),.UNSPECIFIED.,.F.,.F.,(4,1,1,1,1,4),(17.9342415705864,
18.8587793842596,19.8576158342214,20.8564522841833,21.8552887341452,21.9911485751286),
 .UNSPECIFIED.);
#1096=B_SPLINE_CURVE_WITH_KNOTS('',3,(#114071,#114072,#114073,#114074,#114075,
#114076),.UNSPECIFIED.,.F.,.F.,(4,1,1,4),(21.9911485751286,22.854125184107,
23.8529616340689,24.2176478004184),.UNSPECIFIED.);
#1097=B_SPLINE_CURVE_WITH_KNOTS('',3,(#114078,#114079,#114080,#114081,#114082,
#114083,#114084,#114085,#114086,#114087,#114088,#114089,#114090,#114091,
#114092,#114093,#114094,#114095,#114096,#114097,#114098,#114099,#114100,
#114101,#114102,#114103,#114104,#114105,#114106,#114107,#114108,#114109,
#114110,#114111,#114112,#114113,#114114,#114115,#114116,#114117,#114118,
#114119,#114120,#114121,#114122,#114123,#114124,#114125,#114126,#114127,
#114128,#114129,#114130,#114131,#114132,#114133,#114134,#114135,#114136,
#114137,#114138,#114139,#114140,#114141,#114142,#114143,#114144,#114145,
#114146,#114147),.UNSPECIFIED.,.F.,.F.,(4,3,3,3,3,3,3,3,3,3,3,3,3,3,3,3,
3,3,3,3,3,3,3,4),(21.9911487995909,22.0999040367044,22.2090425458686,22.3187160667875,
22.3893184515875,22.487921335874,22.5863839114419,22.6866052852054,22.7848896824335,
22.883141107753,22.9813890373117,23.0830805033711,23.1814697140479,23.2848123077986,
23.3881549015493,23.4916866771327,23.5901227234309,23.6884632070921,23.7867377206608,
23.8849757858551,23.9832411509404,24.0815224781616,24.1798939405651,24.2164091062169),
 .UNSPECIFIED.);
#1098=B_SPLINE_CURVE_WITH_KNOTS('',3,(#114148,#114149,#114150,#114151,#114152,
#114153,#114154,#114155),.UNSPECIFIED.,.F.,.F.,(4,1,1,1,1,4),(17.9335273147171,
18.39397265174,19.3928091017018,20.3916455516637,21.3904820016256,21.9911485751286),
 .UNSPECIFIED.);
#1099=B_SPLINE_CURVE_WITH_KNOTS('',3,(#114158,#114159,#114160,#114161,#114162,
#114163,#114164,#114165),.UNSPECIFIED.,.F.,.F.,(4,1,1,1,1,4),(17.9342415897067,
18.8587793842596,19.8576158342214,20.8564522841833,21.8552887341452,21.9911485751286),
 .UNSPECIFIED.);
#1100=B_SPLINE_CURVE_WITH_KNOTS('',3,(#114166,#114167,#114168,#114169,#114170,
#114171),.UNSPECIFIED.,.F.,.F.,(4,1,1,4),(21.9911485751286,22.854125184107,
23.8529616340689,24.2176478214031),.UNSPECIFIED.);
#1101=B_SPLINE_CURVE_WITH_KNOTS('',3,(#114173,#114174,#114175,#114176,#114177,
#114178,#114179,#114180,#114181,#114182,#114183,#114184,#114185,#114186,
#114187,#114188,#114189,#114190,#114191,#114192,#114193,#114194,#114195,
#114196,#114197,#114198,#114199,#114200,#114201,#114202,#114203,#114204,
#114205,#114206,#114207,#114208,#114209,#114210,#114211,#114212,#114213,
#114214,#114215,#114216,#114217,#114218,#114219,#114220,#114221,#114222,
#114223,#114224,#114225,#114226,#114227,#114228,#114229,#114230,#114231,
#114232,#114233,#114234,#114235,#114236,#114237,#114238,#114239,#114240,
#114241,#114242),.UNSPECIFIED.,.F.,.F.,(4,3,3,3,3,3,3,3,3,3,3,3,3,3,3,3,
3,3,3,3,3,3,3,4),(21.9911487995816,22.0999040743052,22.2090426220591,22.3187161819304,
22.3893184515875,22.487921325434,22.5863838904609,22.6866052668469,22.7848896533628,
22.8831410679294,22.9813889867089,23.083080465419,23.1814696653607,23.284812283455,
23.3881549015493,23.4916866796568,23.5901227238994,23.6884632054536,23.7867377168667,
23.8849757798596,23.983241142689,24.081522467619,24.1798939277032,24.2164091264089),
 .UNSPECIFIED.);
#1102=B_SPLINE_CURVE_WITH_KNOTS('',3,(#114243,#114244,#114245,#114246,#114247,
#114248,#114249,#114250),.UNSPECIFIED.,.F.,.F.,(4,1,1,1,1,4),(17.9335273553052,
18.39397265174,19.3928091017018,20.3916455516637,21.3904820016256,21.9911485751286),
 .UNSPECIFIED.);
#1103=B_SPLINE_CURVE_WITH_KNOTS('',3,(#114253,#114254,#114255,#114256,#114257,
#114258,#114259,#114260),.UNSPECIFIED.,.F.,.F.,(4,1,1,1,1,4),(17.9342415884722,
18.8587793842595,19.8576158342214,20.8564522841833,21.8552887341452,21.9911485751286),
 .UNSPECIFIED.);
#1104=B_SPLINE_CURVE_WITH_KNOTS('',3,(#114261,#114262,#114263,#114264,#114265,
#114266),.UNSPECIFIED.,.F.,.F.,(4,1,1,4),(21.9911485751286,22.854125184107,
23.8529616340689,24.2176478200484),.UNSPECIFIED.);
#1105=B_SPLINE_CURVE_WITH_KNOTS('',3,(#114268,#114269,#114270,#114271,#114272,
#114273,#114274,#114275,#114276,#114277,#114278,#114279,#114280,#114281,
#114282,#114283,#114284,#114285,#114286,#114287,#114288,#114289,#114290,
#114291,#114292,#114293,#114294,#114295,#114296,#114297,#114298,#114299,
#114300,#114301,#114302,#114303,#114304,#114305,#114306,#114307,#114308,
#114309,#114310,#114311,#114312,#114313,#114314,#114315,#114316,#114317,
#114318,#114319,#114320,#114321,#114322,#114323,#114324,#114325,#114326,
#114327,#114328,#114329,#114330,#114331,#114332,#114333,#114334,#114335,
#114336,#114337),.UNSPECIFIED.,.F.,.F.,(4,3,3,3,3,3,3,3,3,3,3,3,3,3,3,3,
3,3,3,3,3,3,3,4),(21.9911487995803,22.0999040794723,22.2090426325292,22.3187161977535,
22.3893184515875,22.4879213239996,22.5863838875782,22.6866052643246,22.7848896493685,
22.8831410624578,22.9813889797561,23.0830804602044,23.1814696586711,23.2848122801102,
23.3881549015493,23.4916866794652,23.5901227234261,23.6884632046911,23.7867377158082,
23.8849757784984,23.9832411410165,24.0815224656302,24.179893925392,24.2164091248765),
 .UNSPECIFIED.);
#1106=B_SPLINE_CURVE_WITH_KNOTS('',3,(#114338,#114339,#114340,#114341,#114342,
#114343,#114344,#114345),.UNSPECIFIED.,.F.,.F.,(4,1,1,1,1,4),(17.9335273566036,
18.39397265174,19.3928091017018,20.3916455516637,21.3904820016256,21.9911485751286),
 .UNSPECIFIED.);
#1107=B_SPLINE_CURVE_WITH_KNOTS('',3,(#114348,#114349,#114350,#114351,#114352,
#114353,#114354,#114355),.UNSPECIFIED.,.F.,.F.,(4,1,1,1,1,4),(17.9342415312022,
18.8587793842595,19.8576158342214,20.8564522841833,21.8552887341452,21.9911485751286),
 .UNSPECIFIED.);
#1108=B_SPLINE_CURVE_WITH_KNOTS('',3,(#114356,#114357,#114358,#114359,#114360,
#114361),.UNSPECIFIED.,.F.,.F.,(4,1,1,4),(21.9911485751286,22.854125184107,
23.8529616340689,24.2176477571914),.UNSPECIFIED.);
#1109=B_SPLINE_CURVE_WITH_KNOTS('',3,(#114363,#114364,#114365,#114366,#114367,
#114368,#114369,#114370,#114371,#114372,#114373,#114374,#114375,#114376,
#114377,#114378,#114379,#114380,#114381,#114382,#114383,#114384,#114385,
#114386,#114387,#114388,#114389,#114390,#114391,#114392,#114393,#114394,
#114395,#114396,#114397,#114398,#114399,#114400,#114401,#114402,#114403,
#114404,#114405,#114406,#114407,#114408,#114409,#114410,#114411,#114412,
#114413,#114414,#114415,#114416,#114417,#114418,#114419,#114420,#114421,
#114422,#114423,#114424,#114425,#114426,#114427,#114428,#114429,#114430,
#114431,#114432),.UNSPECIFIED.,.F.,.F.,(4,3,3,3,3,3,3,3,3,3,3,3,3,3,3,3,
3,3,3,3,3,3,3,4),(21.9911487995834,22.0999040669592,22.2090426071739,22.318716159435,
22.3893184515875,22.4879213274736,22.5863838945597,22.6866052704334,22.7848896590419,
22.8831410757092,22.9813889965944,23.0830804728331,23.181469674872,23.2848122882107,
23.3881549015493,23.4916866715276,23.5901227161827,23.6884631981554,23.7867377099928,
23.884975773415,23.9832411366681,24.081522462026,24.1798939225121,24.2164090613759),
 .UNSPECIFIED.);
#1110=B_SPLINE_CURVE_WITH_KNOTS('',3,(#114433,#114434,#114435,#114436,#114437,
#114438,#114439,#114440),.UNSPECIFIED.,.F.,.F.,(4,1,1,1,1,4),(17.9335272866486,
18.39397265174,19.3928091017018,20.3916455516637,21.3904820016256,21.9911485751286),
 .UNSPECIFIED.);
#1111=B_SPLINE_CURVE_WITH_KNOTS('',3,(#114443,#114444,#114445,#114446,#114447,
#114448,#114449,#114450,#114451,#114452,#114453,#114454),.UNSPECIFIED.,
 .F.,.F.,(4,1,1,1,1,1,1,1,1,4),(17.9329414843961,18.1884603353201,18.6758078330811,
19.1631553308421,19.6505028286031,20.1378503263641,20.6251978241251,21.1125453218861,
21.5998928196471,21.991148557883),.UNSPECIFIED.);
#1112=B_SPLINE_CURVE_WITH_KNOTS('',3,(#114455,#114456,#114457,#114458,#114459,
#114460,#114461,#114462,#114463,#114464,#114465,#114466,#114467,#114468,
#114469,#114470,#114471,#114472,#114473,#114474,#114475,#114476,#114477,
#114478,#114479,#114480,#114481,#114482,#114483,#114484,#114485,#114486,
#114487,#114488,#114489,#114490,#114491,#114492,#114493,#114494,#114495,
#114496,#114497,#114498,#114499,#114500,#114501,#114502,#114503,#114504,
#114505,#114506,#114507,#114508,#114509,#114510,#114511,#114512,#114513,
#114514,#114515,#114516,#114517,#114518,#114519,#114520,#114521,#114522,
#114523,#114524,#114525,#114526,#114527,#114528,#114529,#114530,#114531,
#114532,#114533,#114534,#114535,#114536),.UNSPECIFIED.,.F.,.F.,(4,3,3,3,
3,3,3,3,3,3,3,3,3,3,3,3,3,3,3,3,3,3,3,3,3,3,3,4),(21.9911485751285,22.0872403174081,
22.1717077643695,22.2561544844513,22.3406177643316,22.4250871456575,22.5096125640496,
22.5745878151691,22.6660514455681,22.7575040081467,22.8489019715955,22.9402390467649,
23.0314631630385,23.0619353129301,23.1465167513392,23.2310954406081,23.3157173860693,
23.4003602647289,23.4850816883211,23.5492828106911,23.633669288197,23.7179929955514,
23.8022695765466,23.8865146391538,23.970761703403,24.0550059922274,24.139296875598,
24.2156473321997),.UNSPECIFIED.);
#1113=B_SPLINE_CURVE_WITH_KNOTS('',3,(#114538,#114539,#114540,#114541,#114542,
#114543,#114544,#114545,#114546,#114547,#114548,#114549,#114550,#114551,
#114552,#114553,#114554,#114555,#114556,#114557,#114558,#114559,#114560,
#114561,#114562,#114563,#114564,#114565,#114566,#114567,#114568,#114569,
#114570,#114571,#114572,#114573,#114574,#114575,#114576,#114577,#114578,
#114579,#114580,#114581,#114582,#114583,#114584,#114585,#114586,#114587,
#114588,#114589,#114590,#114591,#114592,#114593,#114594,#114595,#114596,
#114597,#114598,#114599,#114600,#114601,#114602,#114603,#114604,#114605,
#114606,#114607,#114608,#114609,#114610,#114611,#114612,#114613,#114614,
#114615,#114616,#114617,#114618,#114619,#114620,#114621,#114622),
 .UNSPECIFIED.,.F.,.F.,(4,3,3,3,3,3,3,3,3,3,3,3,3,3,3,3,3,3,3,3,3,3,3,3,
3,3,3,3,4),(21.9911485753162,22.0800609495919,22.168999417996,22.1971692907241,
22.2842691742849,22.3713525460866,22.4584393273926,22.5455216572055,22.6326240181457,
22.6845167884851,22.7716275763734,22.8587214790213,22.9458181342347,23.0329099438452,
23.120021097721,23.1718642862461,23.2591953323291,23.3465109695105,23.4338293669418,
23.5211423678883,23.60847190326,23.6592117840071,23.7456953098164,23.832159927636,
23.9186299638456,24.005097953844,24.0915948443439,24.1465592817681,24.2161266164728),
 .UNSPECIFIED.);
#1114=B_SPLINE_CURVE_WITH_KNOTS('',3,(#114623,#114624,#114625,#114626,#114627,
#114628,#114629,#114630,#114631,#114632,#114633,#114634,#114635,#114636,
#114637,#114638,#114639,#114640,#114641,#114642,#114643,#114644,#114645,
#114646,#114647,#114648,#114649,#114650,#114651,#114652,#114653,#114654,
#114655,#114656,#114657,#114658,#114659,#114660,#114661,#114662,#114663,
#114664,#114665,#114666,#114667,#114668,#114669,#114670,#114671,#114672,
#114673,#114674,#114675,#114676,#114677,#114678,#114679,#114680,#114681,
#114682,#114683,#114684,#114685,#114686,#114687,#114688,#114689,#114690,
#114691,#114692,#114693,#114694,#114695,#114696,#114697,#114698,#114699,
#114700,#114701,#114702,#114703,#114704,#114705,#114706,#114707,#114708,
#114709,#114710,#114711,#114712,#114713,#114714,#114715,#114716,#114717,
#114718,#114719,#114720,#114721,#114722,#114723,#114724,#114725,#114726,
#114727,#114728,#114729,#114730,#114731,#114732,#114733,#114734,#114735,
#114736,#114737,#114738,#114739,#114740,#114741,#114742,#114743,#114744,
#114745,#114746,#114747,#114748,#114749,#114750,#114751,#114752,#114753,
#114754,#114755,#114756,#114757,#114758,#114759,#114760,#114761,#114762,
#114763,#114764,#114765,#114766,#114767,#114768,#114769,#114770,#114771,
#114772,#114773,#114774,#114775,#114776),.UNSPECIFIED.,.F.,.F.,(4,3,3,3,
3,3,3,3,3,3,3,3,3,3,3,3,3,3,3,3,3,3,3,3,3,3,3,3,3,3,3,3,3,3,3,3,3,3,3,3,
3,3,3,3,3,3,3,3,3,3,3,4),(17.9329528346437,18.0243119531418,18.1114270891671,
18.1985409744401,18.2856718326635,18.298389308636,18.3855180493059,18.4726302285909,
18.559745465589,18.6468559845724,18.7339858790278,18.785736806397,18.8728666485425,
18.959979950145,19.0470963297829,19.1342080001734,19.2213390494988,19.273084304158,
19.3602139689286,19.4473270846037,19.534443267337,19.6215547350878,19.7086855747234,
19.760431801919,19.8475621199502,19.9346758967653,20.0217927459667,20.1089048815892,
20.1960363853822,20.24777929968,20.3349058916832,20.4220159234169,20.5091290354302,
20.5962374473094,20.6833652806739,20.735126797441,20.8222649721476,20.9093866302891,
20.9965113211569,21.0836312571589,21.1707704295162,21.222474295202,21.3095858862927,
21.3966808826214,21.4837790530665,21.5708726121089,21.6579858588927,21.709821792963,
21.797454164746,21.8850673211435,21.9726698643262,21.9911485751285),
 .UNSPECIFIED.);
#1115=B_SPLINE_CURVE_WITH_KNOTS('',3,(#114779,#114780,#114781,#114782,#114783,
#114784,#114785,#114786,#114787,#114788,#114789,#114790),.UNSPECIFIED.,
 .F.,.F.,(4,1,1,1,1,1,1,1,1,4),(17.9329414836179,18.1884603353201,18.6758078330811,
19.1631553308421,19.6505028286031,20.1378503263641,20.6251978241251,21.1125453218861,
21.5998928196471,21.9911485578925),.UNSPECIFIED.);
#1116=B_SPLINE_CURVE_WITH_KNOTS('',3,(#114791,#114792,#114793,#114794,#114795,
#114796,#114797,#114798,#114799,#114800,#114801,#114802,#114803,#114804,
#114805,#114806,#114807,#114808,#114809,#114810,#114811,#114812,#114813,
#114814,#114815,#114816,#114817,#114818,#114819,#114820,#114821,#114822,
#114823,#114824,#114825,#114826,#114827,#114828,#114829,#114830,#114831,
#114832,#114833,#114834,#114835,#114836,#114837,#114838,#114839,#114840,
#114841,#114842,#114843,#114844,#114845,#114846,#114847,#114848,#114849,
#114850,#114851,#114852,#114853,#114854,#114855,#114856,#114857,#114858,
#114859,#114860,#114861,#114862,#114863,#114864,#114865,#114866,#114867,
#114868,#114869,#114870,#114871,#114872),.UNSPECIFIED.,.F.,.F.,(4,3,3,3,
3,3,3,3,3,3,3,3,3,3,3,3,3,3,3,3,3,3,3,3,3,3,3,4),(21.9911485751285,22.0872403174081,
22.1717043008718,22.256147550065,22.3406073668107,22.425073290183,22.5095952809818,
22.5745878151691,22.6660564577372,22.7575140633748,22.8489170049659,22.9402589752051,
23.0314877939314,23.0619353129301,23.1465147382964,23.2310914061767,23.3157113292587,
23.4003521854755,23.4850716002667,23.5492828106911,23.6336693594472,23.7179931343229,
23.8022697790428,23.8865149015084,23.9707620193541,24.0550063583272,24.1392972858986,
24.2156474862923),.UNSPECIFIED.);
#1117=B_SPLINE_CURVE_WITH_KNOTS('',3,(#114874,#114875,#114876,#114877,#114878,
#114879,#114880,#114881,#114882,#114883,#114884,#114885,#114886,#114887,
#114888,#114889,#114890,#114891,#114892,#114893,#114894,#114895,#114896,
#114897,#114898,#114899,#114900,#114901,#114902,#114903,#114904,#114905,
#114906,#114907,#114908,#114909,#114910,#114911,#114912,#114913,#114914,
#114915,#114916,#114917,#114918,#114919,#114920,#114921,#114922,#114923,
#114924,#114925,#114926,#114927,#114928,#114929,#114930,#114931,#114932,
#114933,#114934,#114935,#114936,#114937,#114938,#114939,#114940,#114941,
#114942,#114943,#114944,#114945,#114946,#114947,#114948,#114949,#114950,
#114951,#114952,#114953,#114954,#114955,#114956,#114957,#114958),
 .UNSPECIFIED.,.F.,.F.,(4,3,3,3,3,3,3,3,3,3,3,3,3,3,3,3,3,3,3,3,3,3,3,3,
3,3,3,3,4),(21.9911485753162,22.0800610136685,22.1689995435299,22.1971692907241,
22.2842690753762,22.3713523483423,22.4584390318698,22.5455212647318,22.6326235308353,
22.6845167884851,22.7716274880237,22.8587213011356,22.9458178659101,23.0329095847879,
23.1200206482753,23.1718642862461,23.2591959782146,23.3465122652369,23.4338313118415,
23.5211449598873,23.6084751333609,23.6592117840071,23.745693612034,23.8321565252023,
23.9186248608383,24.0050911555493,24.0915863725887,24.1465592817681,24.2161265625725),
 .UNSPECIFIED.);
#1118=B_SPLINE_CURVE_WITH_KNOTS('',3,(#114959,#114960,#114961,#114962,#114963,
#114964,#114965,#114966,#114967,#114968,#114969,#114970,#114971,#114972,
#114973,#114974,#114975,#114976,#114977,#114978,#114979,#114980,#114981,
#114982,#114983,#114984,#114985,#114986,#114987,#114988,#114989,#114990,
#114991,#114992,#114993,#114994,#114995,#114996,#114997,#114998,#114999,
#115000,#115001,#115002,#115003,#115004,#115005,#115006,#115007,#115008,
#115009,#115010,#115011,#115012,#115013,#115014,#115015,#115016,#115017,
#115018,#115019,#115020,#115021,#115022,#115023,#115024,#115025,#115026,
#115027,#115028,#115029,#115030,#115031,#115032,#115033,#115034,#115035,
#115036,#115037,#115038,#115039,#115040,#115041,#115042,#115043,#115044,
#115045,#115046,#115047,#115048,#115049,#115050,#115051,#115052,#115053,
#115054,#115055,#115056,#115057,#115058,#115059,#115060,#115061,#115062,
#115063,#115064,#115065,#115066,#115067,#115068,#115069,#115070,#115071,
#115072,#115073,#115074,#115075,#115076,#115077,#115078,#115079,#115080,
#115081,#115082,#115083,#115084,#115085,#115086,#115087,#115088,#115089,
#115090,#115091,#115092,#115093,#115094,#115095,#115096,#115097,#115098,
#115099,#115100,#115101,#115102,#115103,#115104,#115105,#115106,#115107,
#115108,#115109,#115110,#115111,#115112),.UNSPECIFIED.,.F.,.F.,(4,3,3,3,
3,3,3,3,3,3,3,3,3,3,3,3,3,3,3,3,3,3,3,3,3,3,3,3,3,3,3,3,3,3,3,3,3,3,3,3,
3,3,3,3,3,3,3,3,3,3,3,4),(17.932952833811,18.0243119525172,18.1114270941441,
18.1985409850432,18.2856718488903,18.298389308636,18.3855180458292,18.4726302215735,
18.5597454549696,18.6468559703248,18.7339858611432,18.785736806397,18.8728666494913,
18.9599799520757,19.0470963327356,19.1342080041683,19.2213390545579,19.273084304158,
19.3602139685927,19.4473270839117,19.5344432662626,19.6215547336169,19.7086855728379,
19.7604318019191,19.8475621241585,19.9346759052151,20.0217927586668,20.1089048985344,
20.1960364065272,20.2477792996801,20.334905875275,20.4220158905206,20.5091289860856,
20.5962373815785,20.6833651987953,20.7351267974411,20.8222650135847,20.9093867133256,
20.9965114456318,21.0836314228818,21.1707706358326,21.2224742952021,21.3095858066139,
21.396680723011,21.4837788139183,21.570872293834,21.6579854628139,21.7098217929631,
21.7974543214401,21.8850676348139,21.972670334226,21.9911485751285),
 .UNSPECIFIED.);
#1119=B_SPLINE_CURVE_WITH_KNOTS('',3,(#115247,#115248,#115249,#115250,#115251,
#115252,#115253,#115254,#115255,#115256,#115257,#115258,#115259,#115260,
#115261,#115262,#115263,#115264,#115265,#115266,#115267,#115268,#115269,
#115270,#115271,#115272,#115273,#115274,#115275,#115276,#115277,#115278,
#115279,#115280,#115281,#115282,#115283,#115284,#115285,#115286,#115287,
#115288,#115289,#115290,#115291,#115292,#115293,#115294,#115295,#115296,
#115297,#115298,#115299,#115300,#115301,#115302,#115303,#115304,#115305,
#115306,#115307,#115308,#115309,#115310,#115311,#115312,#115313,#115314,
#115315,#115316,#115317,#115318,#115319,#115320,#115321,#115322,#115323,
#115324,#115325,#115326,#115327,#115328,#115329,#115330,#115331,#115332,
#115333,#115334),.UNSPECIFIED.,.F.,.F.,(4,3,3,3,3,3,3,3,3,3,3,3,3,3,3,3,
3,3,3,3,3,3,3,3,3,3,3,3,3,4),(0.,0.0223800438562072,0.0455571551273786,
0.0675550647019532,0.0773342777042101,0.0821512753707187,0.0865889152558688,
0.110577888018856,0.135008177241417,0.157206748761003,0.165672870216831,
0.170323072593406,0.173915834948667,0.198993095015585,0.224022472738064,
0.248522734273473,0.258554636060882,0.264135020452961,0.288903377496841,
0.314991214965926,0.34107905243501,0.351267090483404,0.355315312120404,
0.381664714548266,0.403487578295303,0.410694478291004,0.416463279199868,
0.443066534667852,0.469275862304387,0.472065636590521),.UNSPECIFIED.);
#1120=B_SPLINE_CURVE_WITH_KNOTS('',3,(#115335,#115336,#115337,#115338,#115339,
#115340,#115341,#115342,#115343,#115344,#115345,#115346,#115347,#115348,
#115349,#115350,#115351,#115352,#115353,#115354,#115355,#115356,#115357,
#115358,#115359,#115360,#115361,#115362,#115363,#115364,#115365,#115366,
#115367,#115368,#115369,#115370,#115371,#115372,#115373,#115374,#115375,
#115376,#115377,#115378,#115379,#115380,#115381,#115382,#115383,#115384,
#115385,#115386,#115387,#115388,#115389,#115390,#115391,#115392,#115393,
#115394,#115395,#115396,#115397,#115398,#115399,#115400,#115401,#115402,
#115403,#115404,#115405,#115406,#115407,#115408,#115409,#115410,#115411,
#115412,#115413,#115414,#115415,#115416,#115417,#115418,#115419,#115420,
#115421,#115422),.UNSPECIFIED.,.F.,.F.,(4,3,3,3,3,3,3,3,3,3,3,3,3,3,3,3,
3,3,3,3,3,3,3,3,3,3,3,3,3,4),(0.,0.0260517790363223,0.0527225331664048,
0.0776790837678674,0.0889727987852075,0.0959464344588869,0.100845925000849,
0.126855201330769,0.152534130320941,0.176212520341607,0.186122361847472,
0.192547946339425,0.196620306261614,0.221672219573634,0.246724132885653,
0.272050620367204,0.282513655994357,0.286631738476199,0.311154772354935,
0.33576599459967,0.360166888444423,0.370324933502905,0.375577979330509,
0.399326638864468,0.417608625696714,0.42311115157445,0.427811305959952,
0.450556505121142,0.47164802816755,0.474022601254833),.UNSPECIFIED.);
#1121=B_SPLINE_CURVE_WITH_KNOTS('',3,(#115423,#115424,#115425,#115426,#115427,
#115428,#115429,#115430,#115431,#115432,#115433,#115434,#115435,#115436,
#115437,#115438,#115439,#115440,#115441,#115442,#115443,#115444,#115445,
#115446,#115447,#115448,#115449,#115450,#115451,#115452,#115453,#115454,
#115455,#115456,#115457,#115458,#115459,#115460,#115461,#115462,#115463,
#115464,#115465,#115466,#115467,#115468,#115469,#115470,#115471,#115472,
#115473,#115474,#115475,#115476,#115477,#115478,#115479,#115480,#115481,
#115482,#115483,#115484,#115485,#115486,#115487,#115488,#115489,#115490,
#115491,#115492,#115493,#115494,#115495,#115496,#115497,#115498,#115499,
#115500,#115501,#115502,#115503,#115504,#115505,#115506,#115507,#115508,
#115509,#115510),.UNSPECIFIED.,.F.,.F.,(4,3,3,3,3,3,3,3,3,3,3,3,3,3,3,3,
3,3,3,3,3,3,3,3,3,3,3,3,3,4),(0.,0.0223800372151316,0.0455571433117667,
0.0675550536686484,0.0773342673604862,0.0821512524289193,0.0865889078224679,
0.110577875996278,0.135008164712988,0.157206738276085,0.165672856963219,
0.170323012283074,0.173915733667268,0.198992994974291,0.224022472738052,
0.248477225379953,0.258554635842646,0.264135020504929,0.288903381765904,
0.314991218209838,0.341079054653772,0.351267092682162,0.355315313446979,
0.38166471636314,0.403487580067799,0.410694485847216,0.41646327764549,0.443066533245085,
0.469275862304372,0.472065636984189),.UNSPECIFIED.);
#1122=B_SPLINE_CURVE_WITH_KNOTS('',3,(#115511,#115512,#115513,#115514,#115515,
#115516,#115517,#115518,#115519,#115520,#115521,#115522,#115523,#115524,
#115525,#115526,#115527,#115528,#115529,#115530,#115531,#115532,#115533,
#115534,#115535,#115536,#115537,#115538,#115539,#115540,#115541,#115542,
#115543,#115544,#115545,#115546,#115547,#115548,#115549,#115550,#115551,
#115552,#115553,#115554,#115555,#115556,#115557,#115558,#115559,#115560,
#115561,#115562,#115563,#115564,#115565,#115566,#115567,#115568,#115569,
#115570,#115571,#115572,#115573,#115574,#115575,#115576,#115577,#115578,
#115579,#115580,#115581,#115582,#115583,#115584,#115585,#115586,#115587,
#115588,#115589,#115590,#115591,#115592,#115593,#115594,#115595,#115596,
#115597,#115598),.UNSPECIFIED.,.F.,.F.,(4,3,3,3,3,3,3,3,3,3,3,3,3,3,3,3,
3,3,3,3,3,3,3,3,3,3,3,3,3,4),(0.,0.026051796848667,0.0527225544334848,0.0776790985121134,
0.088972803707389,0.0959464341599202,0.100845925569268,0.126855201703197,
0.152534124110727,0.176212516457141,0.186122361672799,0.192547951517572,
0.196620308043645,0.221672220464654,0.246724132885662,0.272050621021719,
0.282513655344617,0.286631737801889,0.311154771378495,0.335765992433512,
0.360166881962943,0.370324927588301,0.375577975882316,0.399326629362454,
0.417608623757103,0.423111147264353,0.427811294162416,0.4505564811234,0.471648028167544,
0.474022601254839),.UNSPECIFIED.);
#1123=B_SPLINE_CURVE_WITH_KNOTS('',3,(#115599,#115600,#115601,#115602,#115603,
#115604,#115605,#115606,#115607,#115608,#115609,#115610,#115611,#115612,
#115613,#115614,#115615,#115616,#115617,#115618,#115619,#115620,#115621,
#115622,#115623,#115624,#115625,#115626,#115627,#115628,#115629,#115630,
#115631,#115632,#115633,#115634,#115635,#115636,#115637,#115638,#115639,
#115640,#115641,#115642,#115643,#115644,#115645,#115646,#115647,#115648,
#115649,#115650,#115651,#115652,#115653,#115654,#115655,#115656,#115657,
#115658,#115659,#115660,#115661,#115662,#115663,#115664,#115665,#115666,
#115667,#115668,#115669,#115670,#115671,#115672,#115673,#115674,#115675,
#115676,#115677,#115678,#115679,#115680,#115681,#115682,#115683,#115684,
#115685,#115686),.UNSPECIFIED.,.F.,.F.,(4,3,3,3,3,3,3,3,3,3,3,3,3,3,3,3,
3,3,3,3,3,3,3,3,3,3,3,3,3,4),(0.,0.0226012852117639,0.0452025704235279,
0.067555058212843,0.0773342716206684,0.0821512618789957,0.0865889109720383,
0.110761871811172,0.134934832650306,0.157206742672241,0.165672862519276,
0.17032303759631,0.173915776335193,0.198993037124028,0.224022472738049,
0.24847722404691,0.258554635931002,0.264135020402494,0.289777625640233,
0.315428339653183,0.341079053666132,0.351267091758101,0.355315312641973,
0.381664715351709,0.403487579124147,0.410694481959163,0.416463278906866,
0.443066534477177,0.469275862304408,0.472065636821688),.UNSPECIFIED.);
#1124=B_SPLINE_CURVE_WITH_KNOTS('',3,(#115687,#115688,#115689,#115690,#115691,
#115692,#115693,#115694,#115695,#115696,#115697,#115698,#115699,#115700,
#115701,#115702,#115703,#115704,#115705,#115706,#115707,#115708,#115709,
#115710,#115711,#115712,#115713,#115714,#115715,#115716,#115717,#115718,
#115719,#115720,#115721,#115722,#115723,#115724,#115725,#115726,#115727,
#115728,#115729,#115730,#115731,#115732,#115733,#115734,#115735,#115736,
#115737,#115738,#115739,#115740,#115741,#115742,#115743,#115744,#115745,
#115746,#115747,#115748,#115749,#115750,#115751,#115752,#115753,#115754,
#115755,#115756,#115757,#115758,#115759,#115760,#115761,#115762,#115763,
#115764,#115765,#115766,#115767,#115768,#115769,#115770,#115771,#115772,
#115773,#115774),.UNSPECIFIED.,.F.,.F.,(4,3,3,3,3,3,3,3,3,3,3,3,3,3,3,3,
3,3,3,3,3,3,3,3,3,3,3,3,3,4),(0.,0.0259306190073998,0.0526009583628531,
0.0776790988226147,0.0889728038113335,0.0959464341623167,0.100845925575729,
0.126856858203816,0.152713971434144,0.177949842661195,0.186122361669415,
0.192547951595364,0.196620308076219,0.221672220480934,0.24672413288565,
0.272050621046898,0.282513655340624,0.286631737980665,0.311197491830502,
0.335883934797747,0.360158613793621,0.3703249274938,0.375577975829039,0.399326629202052,
0.41760862372711,0.423111147116857,0.427811294064984,0.450556480771393,
0.471648028167486,0.47402260125479),.UNSPECIFIED.);
#1125=B_SPLINE_CURVE_WITH_KNOTS('',3,(#115775,#115776,#115777,#115778,#115779,
#115780,#115781,#115782,#115783,#115784,#115785,#115786,#115787,#115788,
#115789,#115790,#115791,#115792,#115793,#115794,#115795,#115796,#115797,
#115798,#115799,#115800,#115801,#115802,#115803,#115804,#115805,#115806,
#115807,#115808,#115809,#115810,#115811,#115812,#115813,#115814,#115815,
#115816,#115817,#115818,#115819,#115820,#115821,#115822,#115823,#115824,
#115825,#115826,#115827,#115828,#115829,#115830,#115831,#115832,#115833,
#115834,#115835,#115836,#115837,#115838,#115839,#115840,#115841,#115842,
#115843,#115844,#115845,#115846,#115847,#115848,#115849,#115850,#115851,
#115852,#115853,#115854,#115855,#115856,#115857,#115858,#115859,#115860,
#115861,#115862),.UNSPECIFIED.,.F.,.F.,(4,3,3,3,3,3,3,3,3,3,3,3,3,3,3,3,
3,3,3,3,3,3,3,3,3,3,3,3,3,4),(0.,0.0223800600970211,0.0455571838797127,
0.0675550913477831,0.0773343026846742,0.0821513307715598,0.086588933128813,
0.110761903794659,0.134934874460505,0.159278641767769,0.165672902158484,
0.170323218744956,0.173916080012127,0.198993337115258,0.224022472738042,
0.248522726826221,0.25855463659488,0.264135020001501,0.288903366541003,
0.314991206662608,0.341079046784212,0.351267085078404,0.355315309150301,
0.381664710560743,0.403487574104964,0.411770819428486,0.416463283580499,
0.443066538814217,0.469275862304419,0.472065635637229),.UNSPECIFIED.);
#1126=B_SPLINE_CURVE_WITH_KNOTS('',3,(#115863,#115864,#115865,#115866,#115867,
#115868,#115869,#115870,#115871,#115872,#115873,#115874,#115875,#115876,
#115877,#115878,#115879,#115880,#115881,#115882,#115883,#115884,#115885,
#115886,#115887,#115888,#115889,#115890,#115891,#115892,#115893,#115894,
#115895,#115896,#115897,#115898,#115899,#115900,#115901,#115902,#115903,
#115904,#115905,#115906,#115907,#115908,#115909,#115910,#115911,#115912,
#115913,#115914,#115915,#115916,#115917,#115918,#115919,#115920,#115921,
#115922,#115923,#115924,#115925,#115926,#115927,#115928,#115929,#115930,
#115931,#115932,#115933,#115934,#115935,#115936,#115937,#115938,#115939,
#115940,#115941,#115942,#115943,#115944,#115945,#115946,#115947),
 .UNSPECIFIED.,.F.,.F.,(4,3,3,3,3,3,3,3,3,3,3,3,3,3,3,3,3,3,3,3,3,3,3,3,
3,3,3,3,4),(0.,0.0260517912929958,0.0527225478357444,0.0776790939050551,
0.0889728021702812,0.0959464342551659,0.100845925350706,0.126855201462979,
0.152534125915518,0.176212517636641,0.192547949849574,0.196620307478408,
0.221672220182029,0.24672413288565,0.272050620811562,0.282513655553444,
0.286631738154676,0.311154771782915,0.335765993221651,0.360166884129707,
0.370324929459797,0.375577976970675,0.399326632351765,0.417608624369275,
0.423111148621278,0.427811298126592,0.450556488913048,0.471648028167475,
0.474022601254778),.UNSPECIFIED.);
#1127=B_SPLINE_CURVE_WITH_KNOTS('',3,(#116164,#116165,#116166,#116167,#116168,
#116169,#116170,#116171,#116172,#116173,#116174,#116175,#116176,#116177,
#116178,#116179,#116180,#116181,#116182,#116183,#116184,#116185,#116186,
#116187,#116188,#116189,#116190,#116191,#116192,#116193,#116194,#116195,
#116196,#116197,#116198,#116199,#116200,#116201,#116202,#116203,#116204,
#116205,#116206,#116207,#116208,#116209,#116210,#116211,#116212,#116213,
#116214,#116215,#116216,#116217,#116218,#116219,#116220,#116221,#116222,
#116223,#116224,#116225,#116226,#116227,#116228,#116229,#116230,#116231,
#116232,#116233,#116234,#116235,#116236,#116237,#116238,#116239,#116240,
#116241,#116242,#116243,#116244,#116245,#116246,#116247,#116248,#116249,
#116250,#116251,#116252,#116253,#116254,#116255,#116256,#116257,#116258,
#116259,#116260,#116261,#116262,#116263,#116264,#116265,#116266),
 .UNSPECIFIED.,.F.,.F.,(4,3,3,3,3,3,3,3,3,3,3,3,3,3,3,3,3,3,3,3,3,3,3,3,
3,3,3,3,3,3,3,3,3,3,4),(-0.950777871811442,-0.906336425390159,-0.861875033089073,
-0.842434685731619,-0.832698894406312,-0.823679279214301,-0.779911530229351,
-0.736812975210593,-0.713111655774817,-0.707528734983928,-0.706840830508988,
-0.663970529007278,-0.620960197429003,-0.578452544067916,-0.53653757030824,
-0.528618153061017,-0.519778489990599,-0.479103795974014,-0.472085166836762,
-0.430141730544586,-0.388512020620237,-0.35295009564229,-0.345831806228506,
-0.34009678874744,-0.299353453374951,-0.258818746671375,-0.246812444972861,
-0.206136253916918,-0.172639040264036,-0.165053203014642,-0.125295016427035,
-0.0858747403745168,-0.046745972523297,-0.0311581910594031,0.),
 .UNSPECIFIED.);
#1128=B_SPLINE_CURVE_WITH_KNOTS('',3,(#116267,#116268,#116269,#116270,#116271,
#116272,#116273,#116274,#116275,#116276,#116277,#116278,#116279,#116280,
#116281,#116282,#116283,#116284,#116285,#116286,#116287,#116288,#116289,
#116290,#116291,#116292,#116293,#116294,#116295,#116296,#116297,#116298,
#116299,#116300,#116301,#116302,#116303,#116304,#116305,#116306,#116307,
#116308,#116309,#116310,#116311,#116312,#116313,#116314,#116315,#116316,
#116317,#116318,#116319,#116320,#116321,#116322,#116323,#116324,#116325,
#116326,#116327,#116328,#116329,#116330,#116331,#116332,#116333,#116334,
#116335,#116336,#116337,#116338,#116339,#116340,#116341,#116342,#116343,
#116344,#116345,#116346,#116347,#116348,#116349,#116350,#116351,#116352,
#116353,#116354,#116355,#116356,#116357,#116358,#116359,#116360,#116361,
#116362,#116363,#116364,#116365,#116366,#116367,#116368,#116369),
 .UNSPECIFIED.,.F.,.F.,(4,3,3,3,3,3,3,3,3,3,3,3,3,3,3,3,3,3,3,3,3,3,3,3,
3,3,3,3,3,3,3,3,3,3,4),(0.,0.0392937243200445,0.0786487924196305,0.118430422481545,
0.157174897280178,0.16530965460934,0.172511921016207,0.214141585432509,
0.254364238175761,0.295024495339404,0.33584270732332,0.340554091141284,
0.347540360366197,0.389002662438925,0.430931272522026,0.437981494075935,
0.479749916301,0.518812960683757,0.524399035770372,0.530138494511844,0.572626647084422,
0.615529815031132,0.658476413958322,0.671400602336179,0.691337520740504,
0.703515645425686,0.711692863472691,0.721145455869737,0.764504689598731,
0.808363873661209,0.829117588621419,0.836453781446258,0.880985314545995,
0.913941349417081,0.950775682567348),.UNSPECIFIED.);
#1129=B_SPLINE_CURVE_WITH_KNOTS('',3,(#116586,#116587,#116588,#116589,#116590,
#116591,#116592,#116593,#116594,#116595,#116596,#116597,#116598,#116599,
#116600,#116601,#116602,#116603,#116604,#116605,#116606,#116607,#116608,
#116609,#116610,#116611,#116612,#116613,#116614,#116615,#116616,#116617,
#116618,#116619,#116620,#116621,#116622,#116623,#116624,#116625,#116626,
#116627,#116628,#116629,#116630,#116631,#116632,#116633,#116634,#116635,
#116636,#116637,#116638,#116639,#116640,#116641,#116642,#116643,#116644,
#116645,#116646,#116647,#116648,#116649,#116650,#116651,#116652,#116653,
#116654,#116655,#116656,#116657,#116658,#116659,#116660,#116661,#116662,
#116663,#116664,#116665,#116666,#116667,#116668,#116669,#116670,#116671,
#116672,#116673,#116674,#116675,#116676,#116677,#116678,#116679,#116680,
#116681,#116682,#116683,#116684,#116685),.UNSPECIFIED.,.F.,.F.,(4,3,3,3,
3,3,3,3,3,3,3,3,3,3,3,3,3,3,3,3,3,3,3,3,3,3,3,3,3,3,3,3,3,4),(-0.954382097139067,
-0.915540356901116,-0.875987953894438,-0.858553371309591,-0.851652578164575,
-0.844316096216611,-0.803953485084634,-0.771951682750547,-0.755904221756574,
-0.746876223962411,-0.741004834362442,-0.7398567607626,-0.698120295630557,
-0.65723238014393,-0.615071640189179,-0.572910900234428,-0.567449445615807,
-0.525372539405531,-0.515246554457167,-0.473498151147521,-0.43027138546824,
-0.387044619788958,-0.380028835389925,-0.33707776560403,-0.293664876803929,
-0.280914982302858,-0.237661647632792,-0.200416680658377,-0.194604991995093,
-0.150716444031498,-0.106377373616171,-0.0619596473153769,-0.0369876293288037,
-2.19658856801564E-6),.UNSPECIFIED.);
#1130=B_SPLINE_CURVE_WITH_KNOTS('',3,(#116686,#116687,#116688,#116689,#116690,
#116691,#116692,#116693,#116694,#116695,#116696,#116697,#116698,#116699,
#116700,#116701,#116702,#116703,#116704,#116705,#116706,#116707,#116708,
#116709,#116710,#116711,#116712,#116713,#116714,#116715,#116716,#116717,
#116718,#116719,#116720,#116721,#116722,#116723,#116724,#116725,#116726,
#116727,#116728,#116729,#116730,#116731,#116732,#116733,#116734,#116735,
#116736,#116737,#116738,#116739,#116740,#116741,#116742,#116743,#116744,
#116745,#116746,#116747,#116748,#116749,#116750,#116751,#116752,#116753,
#116754,#116755,#116756,#116757,#116758,#116759,#116760,#116761,#116762,
#116763,#116764,#116765,#116766,#116767,#116768,#116769,#116770,#116771,
#116772,#116773,#116774,#116775,#116776,#116777,#116778,#116779,#116780,
#116781,#116782,#116783,#116784,#116785,#116786,#116787,#116788),
 .UNSPECIFIED.,.F.,.F.,(4,3,3,3,3,3,3,3,3,3,3,3,3,3,3,3,3,3,3,3,3,3,3,3,
3,3,3,3,3,3,3,3,3,3,4),(3.92004242434274E-15,0.0440097382289256,0.0884882554294149,
0.132783546544066,0.176334546385407,0.187993870420512,0.19423572748739,
0.19979115047153,0.245254179237364,0.288657155098447,0.331818541229242,
0.369239411527086,0.3808541168619,0.388821225436964,0.431108255685869,0.473065176330631,
0.481013297040258,0.523218576167236,0.558979311157592,0.56811322256641,
0.573516263988367,0.614763363362679,0.655642090780445,0.696286761208482,
0.70713567464641,0.734136415169824,0.744264975553648,0.750002339682418,
0.790439331413101,0.830523899179901,0.849662847172381,0.855799185905343,
0.89514518435056,0.923141598833727,0.954382097139069),.UNSPECIFIED.);
#1131=B_SPLINE_CURVE_WITH_KNOTS('',3,(#117005,#117006,#117007,#117008,#117009,
#117010,#117011,#117012,#117013,#117014,#117015,#117016,#117017,#117018,
#117019,#117020,#117021,#117022,#117023,#117024,#117025,#117026,#117027,
#117028,#117029,#117030,#117031,#117032,#117033,#117034,#117035,#117036,
#117037,#117038,#117039,#117040,#117041,#117042,#117043,#117044,#117045,
#117046,#117047,#117048,#117049,#117050,#117051,#117052,#117053,#117054,
#117055,#117056,#117057,#117058,#117059,#117060,#117061,#117062,#117063,
#117064,#117065,#117066,#117067,#117068,#117069,#117070,#117071,#117072,
#117073,#117074,#117075,#117076,#117077,#117078,#117079,#117080,#117081,
#117082,#117083,#117084,#117085,#117086,#117087,#117088,#117089,#117090,
#117091,#117092,#117093,#117094,#117095,#117096,#117097,#117098,#117099,
#117100,#117101,#117102,#117103,#117104,#117105,#117106,#117107,#117108,
#117109,#117110),.UNSPECIFIED.,.F.,.F.,(4,3,3,3,3,3,3,3,3,3,3,3,3,3,3,3,
3,3,3,3,3,3,3,3,3,3,3,3,3,3,3,3,3,3,3,4),(-0.950777871811489,-0.906336436543847,
-0.861875037007214,-0.842434689817133,-0.831093639563838,-0.825301574638444,
-0.781525133147754,-0.738411526679266,-0.713111654821142,-0.707528734408151,
-0.70684083050903,-0.664137304886555,-0.621129293429489,-0.578512194042679,
-0.536486363527969,-0.527113745436322,-0.519453631979133,-0.479103798452372,
-0.472085166836776,-0.430141731436697,-0.388512022347839,-0.352950096664573,
-0.345831809185344,-0.340096789032849,-0.299287338987684,-0.258818748563885,
-0.246812444972867,-0.206034245191202,-0.184174738424728,-0.172639040064828,
-0.16435164756875,-0.124589561125894,-0.0849805995896592,-0.0460567214496698,
-0.0311581910594067,0.),.UNSPECIFIED.);
#1132=B_SPLINE_CURVE_WITH_KNOTS('',3,(#117111,#117112,#117113,#117114,#117115,
#117116,#117117,#117118,#117119,#117120,#117121,#117122,#117123,#117124,
#117125,#117126,#117127,#117128,#117129,#117130,#117131,#117132,#117133,
#117134,#117135,#117136,#117137,#117138,#117139,#117140,#117141,#117142,
#117143,#117144,#117145,#117146,#117147,#117148,#117149,#117150,#117151,
#117152,#117153,#117154,#117155,#117156,#117157,#117158,#117159,#117160,
#117161,#117162,#117163,#117164,#117165,#117166,#117167,#117168,#117169,
#117170,#117171,#117172,#117173,#117174,#117175,#117176,#117177,#117178,
#117179,#117180,#117181,#117182,#117183,#117184,#117185,#117186,#117187,
#117188,#117189,#117190,#117191,#117192,#117193,#117194,#117195,#117196,
#117197,#117198,#117199,#117200,#117201,#117202,#117203,#117204,#117205,
#117206,#117207,#117208,#117209,#117210,#117211,#117212,#117213),
 .UNSPECIFIED.,.F.,.F.,(4,3,3,3,3,3,3,3,3,3,3,3,3,3,3,3,3,3,3,3,3,3,3,3,
3,3,3,3,3,3,3,3,3,3,4),(2.82530270380345E-15,0.0383561142044287,0.0777322538494532,
0.117448352722929,0.157136327544403,0.16530959676955,0.172511917896846,
0.214141585432506,0.254319391003506,0.295111323821477,0.330724243378432,
0.341693770779803,0.34884651352764,0.390592332836265,0.430931232999916,
0.437981494075929,0.47974991115956,0.518812944385605,0.524709771531363,
0.530138484534004,0.572570423222228,0.615574325973383,0.658476390767529,
0.671400602336174,0.701718195721287,0.711077059751642,0.717874112270349,
0.761139330498555,0.804963166413865,0.816774798744654,0.829117599322156,
0.836453798394249,0.880985331409101,0.913941349417075,0.950775682377206),
 .UNSPECIFIED.);
#1133=B_SPLINE_CURVE_WITH_KNOTS('',3,(#117430,#117431,#117432,#117433,#117434,
#117435,#117436,#117437,#117438,#117439,#117440,#117441,#117442,#117443,
#117444,#117445,#117446,#117447,#117448,#117449,#117450,#117451,#117452,
#117453,#117454,#117455,#117456,#117457,#117458,#117459,#117460,#117461,
#117462,#117463,#117464,#117465,#117466,#117467,#117468,#117469,#117470,
#117471,#117472,#117473,#117474,#117475,#117476,#117477,#117478,#117479,
#117480,#117481,#117482,#117483,#117484,#117485,#117486,#117487,#117488,
#117489,#117490,#117491,#117492,#117493,#117494,#117495,#117496,#117497,
#117498,#117499,#117500,#117501,#117502,#117503,#117504,#117505,#117506,
#117507,#117508,#117509,#117510,#117511,#117512,#117513,#117514,#117515,
#117516,#117517,#117518,#117519,#117520,#117521,#117522,#117523,#117524,
#117525,#117526,#117527,#117528,#117529,#117530,#117531,#117532,#117533,
#117534,#117535),.UNSPECIFIED.,.F.,.F.,(4,3,3,3,3,3,3,3,3,3,3,3,3,3,3,3,
3,3,3,3,3,3,3,3,3,3,3,3,3,3,3,3,3,3,3,4),(-0.954382097139027,-0.915540393312973,
-0.875988011034615,-0.858553452015747,-0.851651720979109,-0.84431594622701,
-0.803953347308937,-0.771951616163724,-0.755904188463154,-0.746876173424658,
-0.741004793318458,-0.739856760762583,-0.698120275698938,-0.657232336987902,
-0.615071578747952,-0.572910820508001,-0.567449396059044,-0.525372472030206,
-0.515246554457162,-0.473526932909519,-0.431236741000685,-0.393744912161324,
-0.387044679913831,-0.381221890286597,-0.338027165363517,-0.294874550582207,
-0.28091498230286,-0.237709647788546,-0.212648675820495,-0.200416680015836,
-0.194604990965853,-0.150716441724809,-0.106377371179378,-0.0619596447542818,
-0.0369876293288071,-2.19683063229992E-6),.UNSPECIFIED.);
#1134=B_SPLINE_CURVE_WITH_KNOTS('',3,(#117536,#117537,#117538,#117539,#117540,
#117541,#117542,#117543,#117544,#117545,#117546,#117547,#117548,#117549,
#117550,#117551,#117552,#117553,#117554,#117555,#117556,#117557,#117558,
#117559,#117560,#117561,#117562,#117563,#117564,#117565,#117566,#117567,
#117568,#117569,#117570,#117571,#117572,#117573,#117574,#117575,#117576,
#117577,#117578,#117579,#117580,#117581,#117582,#117583,#117584,#117585,
#117586,#117587,#117588,#117589,#117590,#117591,#117592,#117593,#117594,
#117595,#117596,#117597,#117598,#117599,#117600,#117601,#117602,#117603,
#117604,#117605,#117606,#117607,#117608,#117609,#117610,#117611,#117612,
#117613,#117614,#117615,#117616,#117617,#117618,#117619,#117620,#117621,
#117622,#117623,#117624,#117625,#117626,#117627,#117628,#117629,#117630,
#117631,#117632,#117633,#117634,#117635,#117636,#117637,#117638,#117639,
#117640,#117641),.UNSPECIFIED.,.F.,.F.,(4,3,3,3,3,3,3,3,3,3,3,3,3,3,3,3,
3,3,3,3,3,3,3,3,3,3,3,3,3,3,3,3,3,3,3,4),(0.,0.0440097102619092,0.0884882277676935,
0.13278353303231,0.176334557243214,0.187993903233133,0.194235848510683,
0.199791297605252,0.245254179237363,0.288657161367,0.331818543101246,0.369239414789171,
0.380854128970053,0.388821223648941,0.43103452325887,0.473065169701532,
0.481013297040253,0.523218575748239,0.558979309133477,0.568113222474232,
0.57351626392526,0.614765000689446,0.655861440304519,0.69628675606685,0.707135674646407,
0.734136415169823,0.74426497460981,0.752455611723686,0.792892563016178,
0.833036427742995,0.838982768060298,0.849662831772539,0.855799161052988,
0.895145162238262,0.923141598833728,0.954382097139071),.UNSPECIFIED.);
#1135=B_SPLINE_CURVE_WITH_KNOTS('',3,(#118354,#118355,#118356,#118357,#118358,
#118359,#118360,#118361,#118362,#118363,#118364,#118365,#118366,#118367,
#118368,#118369,#118370,#118371,#118372,#118373,#118374,#118375,#118376,
#118377,#118378,#118379,#118380,#118381,#118382,#118383,#118384,#118385,
#118386,#118387,#118388,#118389,#118390,#118391,#118392,#118393,#118394,
#118395,#118396,#118397,#118398,#118399,#118400,#118401,#118402,#118403,
#118404,#118405,#118406,#118407,#118408,#118409,#118410,#118411,#118412,
#118413,#118414,#118415,#118416,#118417,#118418,#118419,#118420,#118421,
#118422,#118423,#118424,#118425,#118426,#118427,#118428,#118429,#118430,
#118431,#118432,#118433,#118434,#118435,#118436,#118437,#118438,#118439,
#118440,#118441),.UNSPECIFIED.,.F.,.F.,(4,3,3,3,3,3,3,3,3,3,3,3,3,3,3,3,
3,3,3,3,3,3,3,3,3,3,3,3,3,4),(0.,0.0223800415826112,0.0455571510727117,
0.0675550609170155,0.0773342741558292,0.0821512675008773,0.0865889126878389,
0.110577883862217,0.13500817294145,0.157206745152612,0.16567286565653,0.170323051943897,
0.173915800266865,0.198993060769187,0.224022472738035,0.248477223249604,
0.258554635986008,0.264135020444879,0.288903378930059,0.314991216050641,
0.341079053171223,0.351267091230857,0.355315312478378,0.381664715071333,
0.403487578818942,0.410694480570935,0.416463278950785,0.443066534470942,
0.469275862304353,0.472065636725432),.UNSPECIFIED.);
#1136=B_SPLINE_CURVE_WITH_KNOTS('',3,(#119154,#119155,#119156,#119157,#119158,
#119159,#119160,#119161,#119162,#119163,#119164,#119165,#119166,#119167,
#119168,#119169,#119170,#119171,#119172,#119173,#119174,#119175,#119176,
#119177,#119178,#119179,#119180,#119181,#119182,#119183,#119184,#119185,
#119186,#119187,#119188,#119189,#119190,#119191,#119192,#119193,#119194,
#119195,#119196,#119197,#119198,#119199,#119200,#119201,#119202,#119203,
#119204,#119205,#119206,#119207,#119208,#119209,#119210,#119211,#119212,
#119213,#119214,#119215,#119216,#119217,#119218,#119219,#119220,#119221,
#119222,#119223,#119224,#119225,#119226,#119227,#119228,#119229,#119230,
#119231,#119232,#119233,#119234,#119235,#119236,#119237,#119238,#119239,
#119240,#119241,#119242,#119243,#119244),.UNSPECIFIED.,.F.,.F.,(4,3,3,3,
3,3,3,3,3,3,3,3,3,3,3,3,3,3,3,3,3,3,3,3,3,3,3,3,3,3,4),(7.90123170449159E-15,
0.026051780813598,0.0527225352993908,0.0776790852361114,0.0889727992741923,
0.0959464344241781,0.100845925040092,0.126855201361833,0.152534129666993,
0.17621251994363,0.186122361828502,0.19254794682658,0.196620306433238,0.221672219659448,
0.246724132885659,0.27205844796921,0.280886246323336,0.285802388621783,
0.299566540225716,0.311229550951507,0.335915922421445,0.36019020093975,
0.370324932919906,0.375577978970566,0.399326637919176,0.417608625494232,
0.423111151172439,0.427811304835429,0.450556502779003,0.471648028167516,
0.474022601254811),.UNSPECIFIED.);
#1137=B_SPLINE_CURVE_WITH_KNOTS('',3,(#119957,#119958,#119959,#119960,#119961,
#119962,#119963,#119964,#119965,#119966,#119967,#119968,#119969,#119970,
#119971,#119972,#119973,#119974,#119975,#119976,#119977,#119978,#119979,
#119980,#119981,#119982,#119983,#119984,#119985,#119986,#119987,#119988,
#119989,#119990,#119991,#119992,#119993,#119994,#119995,#119996,#119997,
#119998,#119999,#120000,#120001,#120002,#120003,#120004,#120005,#120006,
#120007,#120008,#120009,#120010,#120011,#120012,#120013,#120014,#120015,
#120016,#120017,#120018,#120019,#120020,#120021,#120022,#120023,#120024,
#120025,#120026,#120027,#120028,#120029,#120030,#120031,#120032,#120033,
#120034,#120035,#120036,#120037,#120038,#120039,#120040,#120041,#120042,
#120043,#120044),.UNSPECIFIED.,.F.,.F.,(4,3,3,3,3,3,3,3,3,3,3,3,3,3,3,3,
3,3,3,3,3,3,3,3,3,3,3,3,3,4),(0.,0.0223800646564789,0.0455571919885243,
0.0675550989125488,0.077334309776642,0.0821513465008637,0.0865889382889745,
0.110577925353256,0.135008216272887,0.157206781258753,0.165672911295151,
0.170323260534971,0.173916149941423,0.198993406189961,0.22402247273804,
0.248477212094458,0.258554636746328,0.26413501995488,0.288903363466093,
0.314991204360096,0.341079045254099,0.351267083567837,0.355315308310309,
0.381664709440851,0.403487572943969,0.410694455370546,0.416463284762423,
0.443066539898885,0.469275862304369,0.472065635365967),.UNSPECIFIED.);
#1138=B_SPLINE_CURVE_WITH_KNOTS('',3,(#120757,#120758,#120759,#120760,#120761,
#120762,#120763,#120764,#120765,#120766,#120767,#120768,#120769,#120770,
#120771,#120772,#120773,#120774,#120775,#120776,#120777,#120778,#120779,
#120780,#120781,#120782,#120783,#120784,#120785,#120786,#120787,#120788,
#120789,#120790,#120791,#120792,#120793,#120794,#120795,#120796,#120797,
#120798,#120799,#120800,#120801,#120802,#120803,#120804,#120805,#120806,
#120807,#120808,#120809,#120810,#120811,#120812,#120813,#120814,#120815,
#120816,#120817,#120818,#120819,#120820,#120821,#120822,#120823,#120824,
#120825,#120826,#120827,#120828,#120829,#120830,#120831,#120832,#120833,
#120834,#120835,#120836,#120837,#120838,#120839,#120840,#120841,#120842,
#120843,#120844),.UNSPECIFIED.,.F.,.F.,(4,3,3,3,3,3,3,3,3,3,3,3,3,3,3,3,
3,3,3,3,3,3,3,3,3,3,3,3,3,4),(0.,0.0260517756043454,0.052722529084373,0.0776790809548157,
0.0889727978441528,0.0959464345074647,0.10084592486155,0.126855201263957,
0.152534131466515,0.176212521061365,0.186122361876941,0.192547945329784,
0.196620305916515,0.221672219401092,0.246724132885669,0.27206158277579,
0.282513656118586,0.286631738568381,0.311197492372782,0.335883935060444,
0.360158620946212,0.370324934628168,0.375577979963716,0.399595492014671,
0.417608626052888,0.423111152459427,0.427811308268704,0.450556509740111,
0.471648028167537,0.474022601254832),.UNSPECIFIED.);
#1139=B_SPLINE_CURVE_WITH_KNOTS('',3,(#121557,#121558,#121559,#121560,#121561,
#121562,#121563,#121564,#121565,#121566,#121567,#121568,#121569,#121570,
#121571,#121572,#121573,#121574,#121575,#121576,#121577,#121578,#121579,
#121580,#121581,#121582,#121583,#121584,#121585,#121586,#121587,#121588,
#121589,#121590,#121591,#121592,#121593,#121594,#121595,#121596,#121597,
#121598,#121599,#121600,#121601,#121602,#121603,#121604,#121605,#121606,
#121607,#121608,#121609,#121610,#121611,#121612,#121613,#121614,#121615,
#121616,#121617,#121618,#121619,#121620,#121621,#121622,#121623,#121624,
#121625,#121626,#121627,#121628,#121629,#121630,#121631,#121632,#121633,
#121634,#121635,#121636,#121637,#121638,#121639,#121640,#121641,#121642,
#121643,#121644),.UNSPECIFIED.,.F.,.F.,(4,3,3,3,3,3,3,3,3,3,3,3,3,3,3,3,
3,3,3,3,3,3,3,3,3,3,3,3,3,4),(0.,0.0223800651370379,0.0455571928568217,
0.0675550997304994,0.0773343105434705,0.0833848318194915,0.0865889388358174,
0.110577926266236,0.135008217226719,0.157206782032257,0.165672912272975,
0.170323265017005,0.173916157466764,0.198993413622444,0.224022472738036,
0.248477211854248,0.258554636762497,0.264135019948427,0.288981342589089,
0.314338830546098,0.340111642434369,0.351267083403808,0.355315308234309,
0.381664709331106,0.403487572828058,0.410694454865743,0.416463284884501,
0.443066539997531,0.469275862304369,0.472065635336616),.UNSPECIFIED.);
#1140=B_SPLINE_CURVE_WITH_KNOTS('',3,(#122357,#122358,#122359,#122360,#122361,
#122362,#122363,#122364,#122365,#122366,#122367,#122368,#122369,#122370,
#122371,#122372,#122373,#122374,#122375,#122376,#122377,#122378,#122379,
#122380,#122381,#122382,#122383,#122384,#122385,#122386,#122387,#122388,
#122389,#122390,#122391,#122392,#122393,#122394,#122395,#122396,#122397,
#122398,#122399,#122400,#122401,#122402,#122403,#122404,#122405,#122406,
#122407,#122408,#122409,#122410,#122411,#122412,#122413,#122414,#122415,
#122416,#122417,#122418,#122419,#122420,#122421,#122422,#122423,#122424,
#122425,#122426,#122427,#122428,#122429,#122430,#122431,#122432,#122433,
#122434,#122435,#122436,#122437,#122438,#122439,#122440,#122441,#122442,
#122443,#122444),.UNSPECIFIED.,.F.,.F.,(4,3,3,3,3,3,3,3,3,3,3,3,3,3,3,3,
3,3,3,3,3,3,3,3,3,3,3,3,3,4),(0.,0.0261324658014225,0.0526962913265927,
0.079341535722988,0.0889727984346616,0.0958350432501777,0.10084592493607,
0.126856858695131,0.152713978118554,0.177949856032678,0.186122361857045,
0.192547945950156,0.196620306130287,0.221672219507975,0.246724132885664,
0.272050620322494,0.282513656041832,0.286631738502527,0.311258832154326,
0.335885925806125,0.360166888882926,0.37032493392055,0.375577979558784,
0.399326639542125,0.417608625825101,0.423111151926387,0.42781130682219,
0.450556506836619,0.47164802816751,0.474022601254803),.UNSPECIFIED.);
#1141=B_SPLINE_CURVE_WITH_KNOTS('',3,(#123157,#123158,#123159,#123160,#123161,
#123162,#123163,#123164,#123165,#123166,#123167,#123168,#123169,#123170,
#123171,#123172,#123173,#123174,#123175,#123176,#123177,#123178,#123179,
#123180,#123181,#123182,#123183,#123184,#123185,#123186,#123187,#123188,
#123189,#123190,#123191,#123192,#123193,#123194,#123195,#123196,#123197,
#123198,#123199,#123200,#123201,#123202,#123203,#123204,#123205,#123206,
#123207,#123208,#123209,#123210,#123211,#123212,#123213,#123214,#123215,
#123216,#123217,#123218,#123219,#123220,#123221,#123222,#123223,#123224,
#123225,#123226,#123227,#123228,#123229,#123230,#123231,#123232,#123233,
#123234,#123235,#123236,#123237,#123238,#123239,#123240,#123241),
 .UNSPECIFIED.,.F.,.F.,(4,3,3,3,3,3,3,3,3,3,3,3,3,3,3,3,3,3,3,3,3,3,3,3,
3,3,3,3,4),(0.,0.0222914007901619,0.045467435982572,0.0675550870544155,
0.0821513218453204,0.0865889302954898,0.110629677084234,0.134994651838372,
0.15933803071403,0.165672897048461,0.170323195429502,0.173916040779313,
0.19899329834446,0.224022472738044,0.248477215576034,0.258554636508914,
0.264135020109551,0.288903368301885,0.314991208014035,0.341079047726185,
0.351267085960766,0.355315309607254,0.381664711215564,0.4034875747766,0.410694463232085,
0.416463282945419,0.443066538202942,0.469275862304378,0.472065635791059),
 .UNSPECIFIED.);
#1142=B_SPLINE_CURVE_WITH_KNOTS('',3,(#123954,#123955,#123956,#123957,#123958,
#123959,#123960,#123961,#123962,#123963,#123964,#123965,#123966,#123967,
#123968,#123969,#123970,#123971,#123972,#123973,#123974,#123975,#123976,
#123977,#123978,#123979,#123980,#123981,#123982,#123983,#123984,#123985,
#123986,#123987,#123988,#123989,#123990,#123991,#123992,#123993,#123994,
#123995,#123996,#123997,#123998,#123999,#124000,#124001,#124002,#124003,
#124004,#124005,#124006,#124007,#124008,#124009,#124010,#124011,#124012,
#124013,#124014,#124015,#124016,#124017,#124018,#124019,#124020,#124021,
#124022,#124023,#124024,#124025,#124026,#124027,#124028,#124029,#124030,
#124031,#124032,#124033,#124034,#124035,#124036,#124037,#124038,#124039,
#124040,#124041),.UNSPECIFIED.,.F.,.F.,(4,3,3,3,3,3,3,3,3,3,3,3,3,3,3,3,
3,3,3,3,3,3,3,3,3,3,3,3,3,4),(7.97682625883415E-15,0.0260517932991782,0.052722550215245,
0.077679095575174,0.0889728027275484,0.0959464342222353,0.10084592545247,
0.1268552016093,0.152534125301528,0.176212517229938,0.186122361708183,0.19254795046146,
0.196620307684512,0.221672220285089,0.246724132885667,0.272050620894862,
0.282513655479386,0.286631738114849,0.31115477174714,0.335765993045936,
0.360166883426141,0.370324928797177,0.375577976589965,0.399326631291423,
0.417608624155145,0.423111148097321,0.427811296634432,0.450556486039327,
0.47164802816752,0.474022601254815),.UNSPECIFIED.);
#1143=B_SPLINE_CURVE_WITH_KNOTS('',3,(#124743,#124744,#124745,#124746,#124747,
#124748,#124749,#124750,#124751,#124752,#124753,#124754,#124755,#124756),
 .UNSPECIFIED.,.F.,.F.,(4,2,2,2,2,2,4),(-0.179602182967889,-0.179256977579304,
-0.171704143510179,-0.143638027894992,-0.121065001388227,-0.103941692121038,
-0.0932595456500115),.UNSPECIFIED.);
#1144=B_SPLINE_CURVE_WITH_KNOTS('',3,(#124761,#124762,#124763,#124764,#124765,
#124766,#124767,#124768),.UNSPECIFIED.,.F.,.F.,(4,2,2,4),(-0.000485046858822211,
0.,0.0275595172389922,0.0494496501685093),.UNSPECIFIED.);
#1145=B_SPLINE_CURVE_WITH_KNOTS('',3,(#124769,#124770,#124771,#124772,#124773,
#124774,#124775,#124776,#124777,#124778,#124779,#124780),.UNSPECIFIED.,
 .F.,.F.,(4,2,2,2,2,4),(0.0518378816079573,0.0543463464547439,0.0792065654069019,
0.0971521945631999,0.111639541304113,0.114326698243711),.UNSPECIFIED.);
#1146=B_SPLINE_CURVE_WITH_KNOTS('',3,(#124801,#124802,#124803,#124804,#124805,
#124806,#124807,#124808,#124809,#124810,#124811,#124812),.UNSPECIFIED.,
 .F.,.F.,(4,2,2,2,2,4),(0.129817017894095,0.133096428805707,0.150776811474232,
0.172677687900067,0.203017141504491,0.206078476281295),.UNSPECIFIED.);
#1147=B_SPLINE_CURVE_WITH_KNOTS('',3,(#124814,#124815,#124816,#124817,#124818,
#124819,#124820,#124821),.UNSPECIFIED.,.F.,.F.,(4,2,2,4),(0.195623656529068,
0.221185285948212,0.253367190411721,0.253933591177603),.UNSPECIFIED.);
#1148=B_SPLINE_CURVE_WITH_KNOTS('',3,(#124824,#124825,#124826,#124827,#124828,
#124829,#124830,#124831,#124832,#124833,#124834,#124835,#124836,#124837),
 .UNSPECIFIED.,.F.,.F.,(4,2,2,2,2,2,4),(-0.000415314508934373,0.,0.00908676885214763,
0.0428529422959233,0.0700104135552468,0.0906113630623747,0.103462988682372),
 .UNSPECIFIED.);
#1149=B_SPLINE_CURVE_WITH_KNOTS('',3,(#125335,#125336,#125337,#125338,#125339,
#125340,#125341,#125342,#125343,#125344,#125345,#125346,#125347,#125348),
 .UNSPECIFIED.,.F.,.F.,(4,2,2,2,2,2,4),(-0.000415314508948534,4.04163464848284E-15,
0.00908676885225018,0.0428529422967522,0.070010413556592,0.0906113630640777,
0.103462988684296),.UNSPECIFIED.);
#1150=B_SPLINE_CURVE_WITH_KNOTS('',3,(#125357,#125358,#125359,#125360,#125361,
#125362,#125363,#125364,#125365,#125366,#125367,#125368),.UNSPECIFIED.,
 .F.,.F.,(4,2,2,2,2,4),(-0.20607847627937,-0.203017141502583,-0.172677687898418,
-0.150776811472805,-0.13309642880445,-0.129817017892869),.UNSPECIFIED.);
#1151=B_SPLINE_CURVE_WITH_KNOTS('',3,(#125369,#125370,#125371,#125372,#125373,
#125374,#125375,#125376),.UNSPECIFIED.,.F.,.F.,(4,2,2,4),(-0.253933591178468,
-0.253367190412585,-0.22118528594891,-0.195623656529625),.UNSPECIFIED.);
#1152=B_SPLINE_CURVE_WITH_KNOTS('',3,(#125396,#125397,#125398,#125399,#125400,
#125401,#125402,#125403,#125404,#125405,#125406,#125407,#125408,#125409),
 .UNSPECIFIED.,.F.,.F.,(4,2,2,2,2,2,4),(-0.179602182967605,-0.179256977579029,
-0.171704143509864,-0.143638027894834,-0.121065001388135,-0.103941692120961,
-0.0932595456499447),.UNSPECIFIED.);
#1153=B_SPLINE_CURVE_WITH_KNOTS('',3,(#125413,#125414,#125415,#125416,#125417,
#125418,#125419,#125420),.UNSPECIFIED.,.F.,.F.,(4,2,2,4),(-0.049449650168343,
-0.0275595172389065,0.,0.000485046858821809),.UNSPECIFIED.);
#1154=B_SPLINE_CURVE_WITH_KNOTS('',3,(#125421,#125422,#125423,#125424,#125425,
#125426,#125427,#125428,#125429,#125430,#125431,#125432),.UNSPECIFIED.,
 .F.,.F.,(4,2,2,2,2,4),(-0.114326698231271,-0.111639541291989,-0.0971521945527792,
-0.0792065653985842,-0.0543463464492475,-0.0518378816027395),
 .UNSPECIFIED.);
#1155=B_SPLINE_CURVE_WITH_KNOTS('',3,(#125658,#125659,#125660,#125661),
 .UNSPECIFIED.,.F.,.F.,(4,4),(0.425543658173478,0.45601992980538),
 .UNSPECIFIED.);
#1156=B_SPLINE_CURVE_WITH_KNOTS('',3,(#125665,#125666,#125667,#125668,#125669,
#125670,#125671,#125672,#125673,#125674),.UNSPECIFIED.,.F.,.F.,(4,2,2,2,
4),(-0.396099187348511,-0.387517388693499,-0.378935590038487,-0.34840050848607,
-0.288839883428953),.UNSPECIFIED.);
#1157=B_SPLINE_CURVE_WITH_KNOTS('',3,(#125678,#125679,#125680,#125681,#125682,
#125683,#125684,#125685,#125686,#125687,#125688,#125689,#125690,#125691,
#125692,#125693,#125694,#125695,#125696,#125697,#125698,#125699,#125700,
#125701,#125702,#125703),.UNSPECIFIED.,.F.,.F.,(4,2,2,2,2,2,2,2,2,2,2,2,
4),(0.255174199615659,0.258977839880058,0.262781480144458,0.270388760673256,
0.281246247196537,0.307084793231223,0.382761299423499,0.458437805615774,
0.484276351650461,0.495133838173742,0.50274111870254,0.506544758966939,
0.510348399231339),.UNSPECIFIED.);
#1158=B_SPLINE_CURVE_WITH_KNOTS('',3,(#125707,#125708,#125709,#125710,#125711,
#125712,#125713,#125714,#125715,#125716),.UNSPECIFIED.,.F.,.F.,(4,2,2,2,
4),(-0.107259303919562,-0.047698678862445,-0.0171635973100282,-0.00858179865501664,
-5.10702591327572E-15),.UNSPECIFIED.);
#1159=B_SPLINE_CURVE_WITH_KNOTS('',3,(#125720,#125721,#125722,#125723,#125724,
#125725),.UNSPECIFIED.,.F.,.F.,(4,2,4),(-0.229255666072561,-0.191461818559235,
-0.153667971045909),.UNSPECIFIED.);
#1160=B_SPLINE_CURVE_WITH_KNOTS('',3,(#125729,#125730,#125731,#125732,#125733,
#125734),.UNSPECIFIED.,.F.,.F.,(4,2,4),(-0.629374586597435,-0.551502061005561,
-0.473629535413688),.UNSPECIFIED.);
#1161=B_SPLINE_CURVE_WITH_KNOTS('',3,(#125738,#125739,#125740,#125741,#125742,
#125743),.UNSPECIFIED.,.F.,.F.,(4,2,4),(-2.19173462068589,-2.01009835047604,
-1.80563850045614),.UNSPECIFIED.);
#1162=B_SPLINE_CURVE_WITH_KNOTS('',3,(#125747,#125748,#125749,#125750,#125751,
#125752,#125753,#125754,#125755,#125756,#125757,#125758,#125759,#125760,
#125761,#125762),.UNSPECIFIED.,.F.,.F.,(4,2,2,2,2,2,2,4),(-0.591143586973193,
-0.574347005517868,-0.557550424062543,-0.523957261151894,-0.475997826184756,
-0.428038391217618,-0.391437431812971,-0.357248738805367),.UNSPECIFIED.);
#1163=B_SPLINE_CURVE_WITH_KNOTS('',3,(#125766,#125767,#125768,#125769,#125770,
#125771,#125772,#125773,#125774,#125775,#125776,#125777,#125778,#125779,
#125780,#125781,#125782,#125783,#125784,#125785,#125786,#125787,#125788,
#125789,#125790,#125791),.UNSPECIFIED.,.F.,.F.,(4,2,2,2,2,2,2,2,2,2,2,2,
4),(0.,0.00380879604231436,0.00761759208462871,0.0152351841692574,0.0261059417541897,
0.0519747072078825,0.127764798734132,0.203554890260381,0.229423655714074,
0.240294413299006,0.247912005383635,0.251720801425949,0.255529597468264),
 .UNSPECIFIED.);
#1164=B_SPLINE_CURVE_WITH_KNOTS('',3,(#125795,#125796,#125797,#125798,#125799,
#125800,#125801,#125802,#125803,#125804,#125805,#125806,#125807,#125808,
#125809,#125810),.UNSPECIFIED.,.F.,.F.,(4,2,2,2,2,2,2,4),(-0.233894848167829,
-0.199706155160222,-0.163105195755574,-0.115145760788437,-0.0671863258212992,
-0.0335931629106496,-0.0167965814553248,0.),.UNSPECIFIED.);
#1165=B_SPLINE_CURVE_WITH_KNOTS('',3,(#125818,#125819,#125820,#125821,#125822,
#125823,#125824,#125825,#125826,#125827,#125828,#125829,#125830,#125831,
#125832,#125833),.UNSPECIFIED.,.F.,.F.,(4,2,2,2,2,2,2,4),(-0.295589574301039,
-0.278794522803568,-0.261996615556423,-0.228400801062134,-0.180435395401912,
-0.13246998974169,-0.0958671986171408,-0.0616743717891369),
 .UNSPECIFIED.);
#1166=B_SPLINE_CURVE_WITH_KNOTS('',3,(#125837,#125838,#125839,#125840,#125841,
#125842,#125843,#125844,#125845,#125846,#125847,#125848,#125849,#125850,
#125851,#125852,#125853,#125854,#125855,#125856,#125857,#125858,#125859,
#125860,#125861,#125862),.UNSPECIFIED.,.F.,.F.,(4,2,2,2,2,2,2,2,2,2,2,2,
4),(0.255403168241683,0.259209043849209,0.263015990348529,0.270629883347168,
0.281495880894667,0.307353808398232,0.383103146024835,0.458852483651438,
0.484710411155003,0.495576408702502,0.503190301701141,0.506997248200461,
0.510803123807987),.UNSPECIFIED.);
#1167=B_SPLINE_CURVE_WITH_KNOTS('',3,(#125866,#125867,#125868,#125869,#125870,
#125871,#125872,#125873,#125874,#125875,#125876,#125877,#125878,#125879,
#125880,#125881),.UNSPECIFIED.,.F.,.F.,(4,2,2,2,2,2,2,4),(-0.525961887431026,
-0.491769060603023,-0.455166269478473,-0.407200863818251,-0.35923545815803,
-0.32563964366374,-0.308841736416595,-0.292046684919125),.UNSPECIFIED.);
#1168=B_SPLINE_CURVE_WITH_KNOTS('',3,(#125885,#125886,#125887,#125888,#125889,
#125890,#125891,#125892),.UNSPECIFIED.,.F.,.F.,(4,2,2,4),(-1.80557842881869,
-1.80556058066602,-1.60110476302328,-1.41948692443241),.UNSPECIFIED.);
#1169=B_SPLINE_CURVE_WITH_KNOTS('',3,(#125896,#125897,#125898,#125899,#125900,
#125901),.UNSPECIFIED.,.F.,.F.,(4,2,4),(-0.15576381568435,-0.0783128305768447,
-7.13925426615558E-6),.UNSPECIFIED.);
#1170=B_SPLINE_CURVE_WITH_KNOTS('',3,(#125905,#125906,#125907,#125908,#125909,
#125910,#125911,#125912,#125913,#125914),.UNSPECIFIED.,.F.,.F.,(4,2,2,2,
4),(-0.151179644005164,-0.151176055112586,-0.113501375709474,-0.0758266963063619,
-0.0755936744236418),.UNSPECIFIED.);
#1171=B_SPLINE_CURVE_WITH_KNOTS('',3,(#125918,#125919,#125920,#125921,#125922,
#125923,#125924,#125925,#125926,#125927,#125928,#125929,#125930,#125931),
 .UNSPECIFIED.,.F.,.F.,(4,2,2,2,2,2,4),(-0.199196015359092,-0.199194230558666,
-0.188883836185403,-0.17857344181214,-0.157952653065614,-0.123832754584569,
-0.0897155491016723),.UNSPECIFIED.);
#1172=B_SPLINE_CURVE_WITH_KNOTS('',3,(#125935,#125936,#125937,#125938,#125939,
#125940,#125941,#125942,#125943,#125944,#125945,#125946,#125947,#125948,
#125949,#125950,#125951,#125952,#125953,#125954,#125955,#125956,#125957,
#125958,#125959,#125960,#125961,#125962,#125963,#125964,#125965),
 .UNSPECIFIED.,.F.,.F.,(4,3,2,2,2,2,2,2,2,2,2,2,2,2,4),(0.509893253687354,
0.509894324579146,0.513694670705264,0.517495016831383,0.525095709083619,
0.535944713171104,0.561763938973776,0.637367905723932,0.712971872474088,
0.73879109827676,0.749640102364244,0.757240794616481,0.7610411407426,0.764841486868718,
0.764842557760511),.UNSPECIFIED.);
#1173=B_SPLINE_CURVE_WITH_KNOTS('',3,(#125969,#125970,#125971,#125972,#125973,
#125974,#125975,#125976,#125977,#125978,#125979,#125980,#125981,#125982),
 .UNSPECIFIED.,.F.,.F.,(4,2,2,2,2,2,4),(-0.306485394370277,-0.272368188887381,
-0.238248290406335,-0.217627501659809,-0.207317107286546,-0.197006712913283,
-0.197004928112857),.UNSPECIFIED.);
#1174=B_SPLINE_CURVE_WITH_KNOTS('',3,(#125986,#125987,#125988,#125989,#125990,
#125991),.UNSPECIFIED.,.F.,.F.,(4,2,4),(-0.489035198690406,-0.458517781350602,
-0.458514192458025),.UNSPECIFIED.);
#1175=B_SPLINE_CURVE_WITH_KNOTS('',3,(#125997,#125998,#125999,#126000,#126001,
#126002,#126003,#126004),.UNSPECIFIED.,.F.,.F.,(4,2,2,4),(-0.534100162039546,
-0.533867140156826,-0.496192460753714,-0.489035198690406),.UNSPECIFIED.);
#1176=B_SPLINE_CURVE_WITH_KNOTS('',3,(#126008,#126009,#126010,#126011,#126012,
#126013),.UNSPECIFIED.,.F.,.F.,(4,2,4),(-1.25873888352118,-1.1804331921986,
-1.10298220709109),.UNSPECIFIED.);
#1177=B_SPLINE_CURVE_WITH_KNOTS('',3,(#126017,#126018,#126019,#126020,#126021,
#126022,#126023,#126024,#126025),.UNSPECIFIED.,.F.,.F.,(4,2,3,4),(-0.386073656233604,
-0.204455817642737,0.,1.78481526716903E-5),.UNSPECIFIED.);
#1178=B_SPLINE_CURVE_WITH_KNOTS('',3,(#126030,#126031,#126032,#126033,#126034,
#126035),.UNSPECIFIED.,.F.,.F.,(4,2,4),(-3.61127700091229,-3.40681715089239,
-3.22518088068254),.UNSPECIFIED.);
#1179=B_SPLINE_CURVE_WITH_KNOTS('',3,(#126039,#126040,#126041,#126042,#126043,
#126044),.UNSPECIFIED.,.F.,.F.,(4,2,4),(-0.785102654344136,-0.707230128752262,
-0.629357603160389),.UNSPECIFIED.);
#1180=B_SPLINE_CURVE_WITH_KNOTS('',3,(#126047,#126048,#126049,#126050,#126051,
#126052),.UNSPECIFIED.,.F.,.F.,(4,2,4),(0.380432234778735,0.418226082292058,
0.425543658173478),.UNSPECIFIED.);
#1181=B_SPLINE_CURVE_WITH_KNOTS('',3,(#126064,#126065,#126066,#126067),
 .UNSPECIFIED.,.F.,.F.,(4,4),(0.425543658173478,0.45601992980538),
 .UNSPECIFIED.);
#1182=B_SPLINE_CURVE_WITH_KNOTS('',3,(#126071,#126072,#126073,#126074,#126075,
#126076,#126077,#126078,#126079,#126080),.UNSPECIFIED.,.F.,.F.,(4,2,2,2,
4),(-0.396099187348511,-0.387517388693499,-0.378935590038488,-0.348400508486071,
-0.288839883428954),.UNSPECIFIED.);
#1183=B_SPLINE_CURVE_WITH_KNOTS('',3,(#126084,#126085,#126086,#126087,#126088,
#126089,#126090,#126091,#126092,#126093,#126094,#126095,#126096,#126097,
#126098,#126099,#126100,#126101,#126102,#126103,#126104,#126105,#126106,
#126107,#126108,#126109),.UNSPECIFIED.,.F.,.F.,(4,2,2,2,2,2,2,2,2,2,2,2,
4),(0.255174199615659,0.258977839880058,0.262781480144457,0.270388760673256,
0.281246247196536,0.307084793231223,0.382761299423499,0.458437805615774,
0.48427635165046,0.495133838173741,0.50274111870254,0.506544758966939,0.510348399231338),
 .UNSPECIFIED.);
#1184=B_SPLINE_CURVE_WITH_KNOTS('',3,(#126113,#126114,#126115,#126116,#126117,
#126118,#126119,#126120,#126121,#126122),.UNSPECIFIED.,.F.,.F.,(4,2,2,2,
4),(-0.107259303919562,-0.047698678862445,-0.0171635973100282,-0.00858179865501664,
-5.10702591327572E-15),.UNSPECIFIED.);
#1185=B_SPLINE_CURVE_WITH_KNOTS('',3,(#126126,#126127,#126128,#126129,#126130,
#126131),.UNSPECIFIED.,.F.,.F.,(4,2,4),(-0.229255666072561,-0.191461818559235,
-0.153667971045909),.UNSPECIFIED.);
#1186=B_SPLINE_CURVE_WITH_KNOTS('',3,(#126135,#126136,#126137,#126138,#126139,
#126140),.UNSPECIFIED.,.F.,.F.,(4,2,4),(-0.629374586597435,-0.551502061005562,
-0.47362953541369),.UNSPECIFIED.);
#1187=B_SPLINE_CURVE_WITH_KNOTS('',3,(#126144,#126145,#126146,#126147,#126148,
#126149),.UNSPECIFIED.,.F.,.F.,(4,2,4),(-2.19173462068589,-2.01009835047603,
-1.80563850045614),.UNSPECIFIED.);
#1188=B_SPLINE_CURVE_WITH_KNOTS('',3,(#126153,#126154,#126155,#126156,#126157,
#126158,#126159,#126160,#126161,#126162,#126163,#126164,#126165,#126166,
#126167,#126168),.UNSPECIFIED.,.F.,.F.,(4,2,2,2,2,2,2,4),(-0.591143586973193,
-0.574347005517868,-0.557550424062543,-0.523957261151894,-0.475997826184756,
-0.428038391217618,-0.391437431812971,-0.357248738805362),.UNSPECIFIED.);
#1189=B_SPLINE_CURVE_WITH_KNOTS('',3,(#126172,#126173,#126174,#126175,#126176,
#126177,#126178,#126179,#126180,#126181,#126182,#126183,#126184,#126185,
#126186,#126187,#126188,#126189,#126190,#126191,#126192,#126193,#126194,
#126195,#126196,#126197),.UNSPECIFIED.,.F.,.F.,(4,2,2,2,2,2,2,2,2,2,2,2,
4),(0.,0.00380879604231436,0.00761759208462871,0.0152351841692574,0.0261059417541897,
0.0519747072078817,0.127764798734132,0.203554890260381,0.229423655714074,
0.240294413299006,0.247912005383635,0.251720801425949,0.255529597468264),
 .UNSPECIFIED.);
#1190=B_SPLINE_CURVE_WITH_KNOTS('',3,(#126201,#126202,#126203,#126204,#126205,
#126206,#126207,#126208,#126209,#126210,#126211,#126212,#126213,#126214,
#126215,#126216),.UNSPECIFIED.,.F.,.F.,(4,2,2,2,2,2,2,4),(-0.233894848167831,
-0.199706155160222,-0.163105195755574,-0.115145760788437,-0.0671863258212992,
-0.0335931629106496,-0.0167965814553248,0.),.UNSPECIFIED.);
#1191=B_SPLINE_CURVE_WITH_KNOTS('',3,(#126224,#126225,#126226,#126227,#126228,
#126229,#126230,#126231,#126232,#126233,#126234,#126235,#126236,#126237,
#126238,#126239),.UNSPECIFIED.,.F.,.F.,(4,2,2,2,2,2,2,4),(-0.295589574301039,
-0.278794522803568,-0.261996615556423,-0.228400801062134,-0.180435395401912,
-0.13246998974169,-0.0958671986171408,-0.0616743717891374),
 .UNSPECIFIED.);
#1192=B_SPLINE_CURVE_WITH_KNOTS('',3,(#126243,#126244,#126245,#126246,#126247,
#126248,#126249,#126250,#126251,#126252,#126253,#126254,#126255,#126256,
#126257,#126258,#126259,#126260,#126261,#126262,#126263,#126264,#126265,
#126266,#126267,#126268),.UNSPECIFIED.,.F.,.F.,(4,2,2,2,2,2,2,2,2,2,2,2,
4),(0.255403168241683,0.259209043849209,0.263015990348529,0.270629883347168,
0.281495880894667,0.307353808398233,0.383103146024836,0.458852483651437,
0.484710411155004,0.495576408702501,0.503190301701141,0.50699724820046,
0.510803123807986),.UNSPECIFIED.);
#1193=B_SPLINE_CURVE_WITH_KNOTS('',3,(#126272,#126273,#126274,#126275,#126276,
#126277,#126278,#126279,#126280,#126281,#126282,#126283,#126284,#126285,
#126286,#126287),.UNSPECIFIED.,.F.,.F.,(4,2,2,2,2,2,2,4),(-0.525961887431026,
-0.491769060603023,-0.455166269478473,-0.407200863818251,-0.35923545815803,
-0.32563964366374,-0.308841736416595,-0.292046684919125),.UNSPECIFIED.);
#1194=B_SPLINE_CURVE_WITH_KNOTS('',3,(#126291,#126292,#126293,#126294,#126295,
#126296,#126297,#126298),.UNSPECIFIED.,.F.,.F.,(4,2,2,4),(-1.80557842881869,
-1.80556058066602,-1.60110476302328,-1.41948692443241),.UNSPECIFIED.);
#1195=B_SPLINE_CURVE_WITH_KNOTS('',3,(#126302,#126303,#126304,#126305,#126306,
#126307),.UNSPECIFIED.,.F.,.F.,(4,2,4),(-0.15576381568435,-0.0783128305768447,
-7.13925426615561E-6),.UNSPECIFIED.);
#1196=B_SPLINE_CURVE_WITH_KNOTS('',3,(#126311,#126312,#126313,#126314,#126315,
#126316,#126317,#126318,#126319,#126320),.UNSPECIFIED.,.F.,.F.,(4,2,2,2,
4),(-0.151179644005162,-0.151176055112586,-0.113501375709474,-0.0758266963063619,
-0.0755936744236418),.UNSPECIFIED.);
#1197=B_SPLINE_CURVE_WITH_KNOTS('',3,(#126324,#126325,#126326,#126327,#126328,
#126329,#126330,#126331,#126332,#126333,#126334,#126335,#126336,#126337),
 .UNSPECIFIED.,.F.,.F.,(4,2,2,2,2,2,4),(-0.199196015359092,-0.199194230558666,
-0.188883836185403,-0.17857344181214,-0.157952653065614,-0.123832754584569,
-0.0897155491016734),.UNSPECIFIED.);
#1198=B_SPLINE_CURVE_WITH_KNOTS('',3,(#126341,#126342,#126343,#126344,#126345,
#126346,#126347,#126348,#126349,#126350,#126351,#126352,#126353,#126354,
#126355,#126356,#126357,#126358,#126359,#126360,#126361,#126362,#126363,
#126364,#126365,#126366,#126367,#126368,#126369,#126370,#126371),
 .UNSPECIFIED.,.F.,.F.,(4,3,2,2,2,2,2,2,2,2,2,2,2,2,4),(0.509893253687354,
0.509894324579146,0.513694670705264,0.517495016831383,0.525095709083619,
0.535944713171104,0.561763938973776,0.637367905723932,0.712971872474088,
0.73879109827676,0.749640102364244,0.757240794616481,0.7610411407426,0.764841486868718,
0.764842557760511),.UNSPECIFIED.);
#1199=B_SPLINE_CURVE_WITH_KNOTS('',3,(#126375,#126376,#126377,#126378,#126379,
#126380,#126381,#126382,#126383,#126384,#126385,#126386,#126387,#126388),
 .UNSPECIFIED.,.F.,.F.,(4,2,2,2,2,2,4),(-0.306485394370277,-0.272368188887381,
-0.238248290406335,-0.217627501659809,-0.207317107286546,-0.197006712913283,
-0.197004928112857),.UNSPECIFIED.);
#1200=B_SPLINE_CURVE_WITH_KNOTS('',3,(#126392,#126393,#126394,#126395,#126396,
#126397),.UNSPECIFIED.,.F.,.F.,(4,2,4),(-0.489035198690406,-0.458517781350602,
-0.458514192458025),.UNSPECIFIED.);
#1201=B_SPLINE_CURVE_WITH_KNOTS('',3,(#126403,#126404,#126405,#126406,#126407,
#126408,#126409,#126410),.UNSPECIFIED.,.F.,.F.,(4,2,2,4),(-0.534100162039546,
-0.533867140156826,-0.496192460753714,-0.489035198690406),.UNSPECIFIED.);
#1202=B_SPLINE_CURVE_WITH_KNOTS('',3,(#126414,#126415,#126416,#126417,#126418,
#126419),.UNSPECIFIED.,.F.,.F.,(4,2,4),(-1.25873888352118,-1.1804331921986,
-1.10298220709109),.UNSPECIFIED.);
#1203=B_SPLINE_CURVE_WITH_KNOTS('',3,(#126423,#126424,#126425,#126426,#126427,
#126428,#126429,#126430,#126431),.UNSPECIFIED.,.F.,.F.,(4,2,3,4),(-0.386073656233604,
-0.204455817642737,0.,1.78481526716903E-5),.UNSPECIFIED.);
#1204=B_SPLINE_CURVE_WITH_KNOTS('',3,(#126436,#126437,#126438,#126439,#126440,
#126441),.UNSPECIFIED.,.F.,.F.,(4,2,4),(-3.61127700091229,-3.40681715089239,
-3.22518088068254),.UNSPECIFIED.);
#1205=B_SPLINE_CURVE_WITH_KNOTS('',3,(#126445,#126446,#126447,#126448,#126449,
#126450),.UNSPECIFIED.,.F.,.F.,(4,2,4),(-0.785102654344136,-0.707230128752262,
-0.629357603160389),.UNSPECIFIED.);
#1206=B_SPLINE_CURVE_WITH_KNOTS('',3,(#126453,#126454,#126455,#126456,#126457,
#126458),.UNSPECIFIED.,.F.,.F.,(4,2,4),(0.380432234778735,0.418226082292058,
0.425543658173478),.UNSPECIFIED.);
#1207=B_SPLINE_CURVE_WITH_KNOTS('',3,(#126470,#126471,#126472,#126473),
 .UNSPECIFIED.,.F.,.F.,(4,4),(0.425543658173479,0.45601992980538),
 .UNSPECIFIED.);
#1208=B_SPLINE_CURVE_WITH_KNOTS('',3,(#126477,#126478,#126479,#126480,#126481,
#126482,#126483,#126484,#126485,#126486,#126487,#126488),.UNSPECIFIED.,
 .F.,.F.,(4,2,2,2,2,4),(-0.398283608397278,-0.387975515458133,-0.377667422518988,
-0.357051236640699,-0.322947181787487,-0.288843126934276),.UNSPECIFIED.);
#1209=B_SPLINE_CURVE_WITH_KNOTS('',3,(#126492,#126493,#126494,#126495,#126496,
#126497,#126498,#126499,#126500,#126501,#126502,#126503,#126504,#126505,
#126506,#126507,#126508,#126509,#126510,#126511,#126512,#126513,#126514,
#126515,#126516,#126517),.UNSPECIFIED.,.F.,.F.,(4,2,2,2,2,2,2,2,2,2,2,2,
4),(0.255174199615664,0.258977839880064,0.262781480144463,0.270388760673262,
0.281246247196542,0.307084793231227,0.382761299423505,0.458437805615783,
0.484276351650471,0.495133838173751,0.50274111870255,0.50654475896695,0.510348399231349),
 .UNSPECIFIED.);
#1210=B_SPLINE_CURVE_WITH_KNOTS('',3,(#126521,#126522,#126523,#126524,#126525,
#126526,#126527,#126528,#126529,#126530,#126531,#126532),.UNSPECIFIED.,
 .F.,.F.,(4,2,2,2,2,4),(-0.109440481463008,-0.075336426609796,-0.0412323717565842,
-0.0206161858782945,-0.0103080929391497,-4.88498130835069E-15),
 .UNSPECIFIED.);
#1211=B_SPLINE_CURVE_WITH_KNOTS('',3,(#126536,#126537,#126538,#126539,#126540,
#126541),.UNSPECIFIED.,.F.,.F.,(4,2,4),(-0.229255666072554,-0.191461818559231,
-0.153667971045908),.UNSPECIFIED.);
#1212=B_SPLINE_CURVE_WITH_KNOTS('',3,(#126545,#126546,#126547,#126548,#126549,
#126550),.UNSPECIFIED.,.F.,.F.,(4,2,4),(-0.629374586597435,-0.551502061005562,
-0.473629535413688),.UNSPECIFIED.);
#1213=B_SPLINE_CURVE_WITH_KNOTS('',3,(#126554,#126555,#126556,#126557,#126558,
#126559),.UNSPECIFIED.,.F.,.F.,(4,2,4),(-2.19173462068589,-2.01009835047604,
-1.80563850045615),.UNSPECIFIED.);
#1214=B_SPLINE_CURVE_WITH_KNOTS('',3,(#126563,#126564,#126565,#126566,#126567,
#126568,#126569,#126570,#126571,#126572,#126573,#126574,#126575,#126576,
#126577,#126578),.UNSPECIFIED.,.F.,.F.,(4,2,2,2,2,2,2,4),(-0.591143586973191,
-0.574347005517867,-0.557550424062542,-0.523957261151894,-0.475997826184755,
-0.428038391217617,-0.391437431812969,-0.357248738805361),.UNSPECIFIED.);
#1215=B_SPLINE_CURVE_WITH_KNOTS('',3,(#126582,#126583,#126584,#126585,#126586,
#126587,#126588,#126589,#126590,#126591,#126592,#126593,#126594,#126595,
#126596,#126597,#126598,#126599,#126600,#126601,#126602,#126603,#126604,
#126605,#126606,#126607),.UNSPECIFIED.,.F.,.F.,(4,2,2,2,2,2,2,2,2,2,2,2,
4),(0.,0.00380879604231454,0.00761759208462907,0.0152351841692581,0.0261059417541897,
0.0519747072078822,0.127764798734136,0.203554890260386,0.22942365571408,
0.240294413299011,0.24791200538364,0.251720801425955,0.255529597468269),
 .UNSPECIFIED.);
#1216=B_SPLINE_CURVE_WITH_KNOTS('',3,(#126611,#126612,#126613,#126614,#126615,
#126616,#126617,#126618,#126619,#126620,#126621,#126622,#126623,#126624,
#126625,#126626),.UNSPECIFIED.,.F.,.F.,(4,2,2,2,2,2,2,4),(-0.233894848167828,
-0.199706155160221,-0.163105195755574,-0.115145760788435,-0.0671863258212968,
-0.0335931629106484,-0.0167965814553242,0.),.UNSPECIFIED.);
#1217=B_SPLINE_CURVE_WITH_KNOTS('',3,(#126634,#126635,#126636,#126637,#126638,
#126639,#126640,#126641,#126642,#126643,#126644,#126645,#126646,#126647,
#126648,#126649),.UNSPECIFIED.,.F.,.F.,(4,2,2,2,2,2,2,4),(-0.295589574301038,
-0.278794522803567,-0.261996615556422,-0.228400801062133,-0.180435395401912,
-0.132469989741691,-0.095867198617141,-0.0616743717891376),
 .UNSPECIFIED.);
#1218=B_SPLINE_CURVE_WITH_KNOTS('',3,(#126653,#126654,#126655,#126656,#126657,
#126658,#126659,#126660,#126661,#126662,#126663,#126664,#126665,#126666,
#126667,#126668,#126669,#126670,#126671,#126672,#126673,#126674,#126675,
#126676,#126677,#126678),.UNSPECIFIED.,.F.,.F.,(4,2,2,2,2,2,2,2,2,2,2,2,
4),(0.255403168241688,0.259209043849214,0.263015990348534,0.270629883347173,
0.281495880894669,0.307353808398237,0.38310314602484,0.458852483651447,
0.484710411155011,0.495576408702511,0.50319030170115,0.506997248200469,
0.510803123807995),.UNSPECIFIED.);
#1219=B_SPLINE_CURVE_WITH_KNOTS('',3,(#126682,#126683,#126684,#126685,#126686,
#126687,#126688,#126689,#126690,#126691,#126692,#126693,#126694,#126695,
#126696,#126697),.UNSPECIFIED.,.F.,.F.,(4,2,2,2,2,2,2,4),(-0.525961887431025,
-0.491769060603021,-0.455166269478471,-0.40720086381825,-0.359235458158029,
-0.32563964366374,-0.308841736416595,-0.292046684919124),.UNSPECIFIED.);
#1220=B_SPLINE_CURVE_WITH_KNOTS('',3,(#126701,#126702,#126703,#126704,#126705,
#126706,#126707,#126708),.UNSPECIFIED.,.F.,.F.,(4,2,2,4),(-1.80557842881869,
-1.80556058066602,-1.60110476302328,-1.41948692443242),.UNSPECIFIED.);
#1221=B_SPLINE_CURVE_WITH_KNOTS('',3,(#126712,#126713,#126714,#126715,#126716,
#126717),.UNSPECIFIED.,.F.,.F.,(4,2,4),(-0.155763815684349,-0.0783128305768452,
-7.13925426615562E-6),.UNSPECIFIED.);
#1222=B_SPLINE_CURVE_WITH_KNOTS('',3,(#126721,#126722,#126723,#126724,#126725,
#126726,#126727,#126728,#126729,#126730),.UNSPECIFIED.,.F.,.F.,(4,2,2,2,
4),(-0.151179644004872,-0.151176055112587,-0.113501375709475,-0.0758266963063625,
-0.0755936744236423),.UNSPECIFIED.);
#1223=B_SPLINE_CURVE_WITH_KNOTS('',3,(#126734,#126735,#126736,#126737,#126738,
#126739,#126740,#126741,#126742,#126743,#126744,#126745,#126746,#126747),
 .UNSPECIFIED.,.F.,.F.,(4,2,2,2,2,2,4),(-0.199196015359092,-0.199194230558666,
-0.188883836185403,-0.178573441812139,-0.157952653065613,-0.123832754584568,
-0.0897155491016729),.UNSPECIFIED.);
#1224=B_SPLINE_CURVE_WITH_KNOTS('',3,(#126751,#126752,#126753,#126754,#126755,
#126756,#126757,#126758,#126759,#126760,#126761,#126762,#126763,#126764,
#126765,#126766,#126767,#126768,#126769,#126770,#126771,#126772,#126773,
#126774,#126775,#126776,#126777,#126778,#126779,#126780,#126781),
 .UNSPECIFIED.,.F.,.F.,(4,3,2,2,2,2,2,2,2,2,2,2,2,2,4),(0.509893253687361,
0.509894324579153,0.513694670705272,0.51749501683139,0.525095709083628,
0.535944713171112,0.561763938973786,0.637367905723943,0.7129718724741,0.738791098276774,
0.749640102364255,0.757240794616493,0.761041140742611,0.76484148686873,
0.764842557760522),.UNSPECIFIED.);
#1225=B_SPLINE_CURVE_WITH_KNOTS('',3,(#126785,#126786,#126787,#126788,#126789,
#126790,#126791,#126792,#126793,#126794,#126795,#126796,#126797,#126798),
 .UNSPECIFIED.,.F.,.F.,(4,2,2,2,2,2,4),(-0.306485394370274,-0.27236818888738,
-0.238248290406335,-0.217627501659809,-0.207317107286546,-0.197006712913282,
-0.197004928112857),.UNSPECIFIED.);
#1226=B_SPLINE_CURVE_WITH_KNOTS('',3,(#126802,#126803,#126804,#126805,#126806,
#126807),.UNSPECIFIED.,.F.,.F.,(4,2,4),(-0.489034960252788,-0.458517542912984,
-0.458513954020698),.UNSPECIFIED.);
#1227=B_SPLINE_CURVE_WITH_KNOTS('',3,(#126813,#126814,#126815,#126816,#126817,
#126818,#126819,#126820),.UNSPECIFIED.,.F.,.F.,(4,2,2,4),(-0.534099923601928,
-0.533866901719208,-0.496192222316096,-0.489034960252788),.UNSPECIFIED.);
#1228=B_SPLINE_CURVE_WITH_KNOTS('',3,(#126824,#126825,#126826,#126827,#126828,
#126829),.UNSPECIFIED.,.F.,.F.,(4,2,4),(-1.25874265108256,-1.18043695975999,
-1.10298597465248),.UNSPECIFIED.);
#1229=B_SPLINE_CURVE_WITH_KNOTS('',3,(#126833,#126834,#126835,#126836,#126837,
#126838,#126839,#126840,#126841),.UNSPECIFIED.,.F.,.F.,(4,2,3,4),(-0.386073656233605,
-0.204455817642737,0.,1.78481526712462E-5),.UNSPECIFIED.);
#1230=B_SPLINE_CURVE_WITH_KNOTS('',3,(#126846,#126847,#126848,#126849,#126850,
#126851),.UNSPECIFIED.,.F.,.F.,(4,2,4),(-3.6112770009123,-3.4068171508924,
-3.22518088068255),.UNSPECIFIED.);
#1231=B_SPLINE_CURVE_WITH_KNOTS('',3,(#126855,#126856,#126857,#126858,#126859,
#126860),.UNSPECIFIED.,.F.,.F.,(4,2,4),(-0.785102654344135,-0.707230128752262,
-0.62935760316039),.UNSPECIFIED.);
#1232=B_SPLINE_CURVE_WITH_KNOTS('',3,(#126863,#126864,#126865,#126866,#126867,
#126868),.UNSPECIFIED.,.F.,.F.,(4,2,4),(0.380432234778735,0.418226082292058,
0.425543658173479),.UNSPECIFIED.);
#1233=B_SPLINE_CURVE_WITH_KNOTS('',3,(#128408,#128409,#128410,#128411,#128412,
#128413,#128414,#128415,#128416,#128417,#128418,#128419,#128420,#128421,
#128422,#128423,#128424,#128425,#128426,#128427,#128428,#128429,#128430,
#128431,#128432,#128433,#128434,#128435),.UNSPECIFIED.,.F.,.F.,(4,3,3,3,
3,3,3,3,3,4),(13.8747245557601,13.9615196181783,14.0483128516542,14.1350984649827,
14.2219050359775,14.2896803532321,14.3768161452291,14.4639332383284,14.5510539735215,
14.6348946358168),.UNSPECIFIED.);
#1234=B_SPLINE_CURVE_WITH_KNOTS('',3,(#128438,#128439,#128440,#128441),
 .UNSPECIFIED.,.F.,.F.,(4,4),(14.399609326548,14.6348821374693),
 .UNSPECIFIED.);
#1235=B_SPLINE_CURVE_WITH_KNOTS('',3,(#128447,#128448,#128449,#128450,#128451,
#128452,#128453,#128454,#128455,#128456,#128457,#128458,#128459,#128460,
#128461),.UNSPECIFIED.,.F.,.F.,(4,1,1,1,1,1,1,1,1,1,1,1,4),(15.707963267949,
15.7517228465151,16.2390703442761,16.7264178420371,17.2137653397981,17.7011128375591,
18.1884603353201,18.6758078330811,19.1631553308421,19.6505028286031,20.1378503263641,
20.6251978241251,20.9180878353355),.UNSPECIFIED.);
#1236=B_SPLINE_CURVE_WITH_KNOTS('',3,(#128462,#128463,#128464,#128465,#128466,
#128467,#128468,#128469,#128470,#128471,#128472,#128473,#128474,#128475,
#128476,#128477,#128478,#128479,#128480,#128481,#128482,#128483,#128484,
#128485,#128486,#128487,#128488,#128489,#128490,#128491,#128492,#128493,
#128494,#128495,#128496,#128497,#128498,#128499,#128500,#128501),
 .UNSPECIFIED.,.F.,.F.,(4,3,3,3,3,3,3,3,3,3,3,3,3,4),(14.6348946358168,
14.7220270383631,14.7770278509931,14.864154772311,14.9512651018673,15.0383784614888,
15.1254870919108,15.2126150969663,15.2643753487541,15.3512430161605,15.4404230791076,
15.5272738475405,15.6176185577448,15.707963267949),.UNSPECIFIED.);
#1237=B_SPLINE_CURVE_WITH_KNOTS('',3,(#128503,#128504,#128505,#128506,#128507,
#128508),.UNSPECIFIED.,.F.,.F.,(4,1,1,4),(14.6348821374693,14.886956824309,
15.37430432207,15.707963267949),.UNSPECIFIED.);
#1238=B_SPLINE_CURVE_WITH_KNOTS('',3,(#128509,#128510,#128511,#128512,#128513,
#128514,#128515,#128516,#128517,#128518,#128519,#128520,#128521,#128522,
#128523,#128524,#128525,#128526,#128527,#128528,#128529,#128530,#128531,
#128532,#128533,#128534,#128535,#128536,#128537,#128538,#128539,#128540,
#128541,#128542,#128543,#128544,#128545,#128546,#128547,#128548,#128549,
#128550,#128551,#128552,#128553,#128554,#128555,#128556,#128557,#128558,
#128559,#128560,#128561,#128562,#128563,#128564,#128565,#128566,#128567,
#128568,#128569,#128570,#128571,#128572,#128573,#128574,#128575,#128576,
#128577,#128578,#128579,#128580,#128581,#128582,#128583,#128584,#128585,
#128586,#128587,#128588,#128589,#128590,#128591,#128592,#128593,#128594,
#128595,#128596,#128597,#128598,#128599,#128600,#128601,#128602,#128603,
#128604,#128605,#128606,#128607,#128608,#128609,#128610,#128611,#128612,
#128613,#128614,#128615,#128616,#128617,#128618,#128619,#128620,#128621,
#128622,#128623,#128624,#128625,#128626,#128627,#128628,#128629,#128630,
#128631,#128632,#128633,#128634,#128635,#128636,#128637,#128638,#128639,
#128640,#128641,#128642,#128643,#128644,#128645,#128646,#128647,#128648,
#128649,#128650,#128651,#128652,#128653,#128654,#128655,#128656,#128657,
#128658,#128659,#128660,#128661,#128662,#128663,#128664,#128665,#128666,
#128667,#128668,#128669,#128670,#128671,#128672,#128673,#128674,#128675,
#128676,#128677,#128678,#128679,#128680,#128681,#128682,#128683,#128684,
#128685,#128686,#128687,#128688,#128689,#128690,#128691,#128692,#128693,
#128694,#128695,#128696,#128697,#128698,#128699,#128700,#128701),
 .UNSPECIFIED.,.F.,.F.,(4,3,3,3,3,3,3,3,3,3,3,3,3,3,3,3,3,3,3,3,3,3,3,3,
3,3,3,3,3,3,3,3,3,3,3,3,3,3,3,3,3,3,3,3,3,3,3,3,3,3,3,3,3,3,3,3,3,3,3,3,
3,3,3,3,4),(15.7079632709821,15.7983391757108,15.861651819831,15.9487473765214,
16.0358259589805,16.1229073061607,16.2099838502341,16.2970799349332,16.348999317592,
16.4361366999986,16.523257608915,16.6103816220701,16.6975009223997,16.7846395292193,
16.836346815353,16.923477639889,17.010591951935,17.0977093744499,17.1848221036438,
17.2719542272672,17.323694313114,17.4108212348644,17.4979315648647,17.5850449249431,
17.6721535558284,17.7592815613529,17.811041810875,17.89817343047,17.9852885340787,
18.0724067350533,18.1595202333711,18.2466531048579,18.298389308636,18.3855180458292,
18.4726302215735,18.5597454549696,18.6468559703248,18.7339858611433,18.785736806397,
18.8728666494913,18.9599799520757,19.0470963327356,19.1342080041683,19.2213390545579,
19.273084304158,19.3602139685927,19.4473270839117,19.5344432662626,19.6215547336169,
19.7086855728379,19.7604318019191,19.8475621241585,19.9346759052151,20.0217927586668,
20.1089048985344,20.1960364065272,20.2477792996801,20.334905875275,20.4220158905206,
20.5091289860856,20.5962373815784,20.6833651987953,20.7351267974411,20.8266148316514,
20.9181028658617),.UNSPECIFIED.);
#1239=B_SPLINE_CURVE_WITH_KNOTS('',3,(#128707,#128708,#128709,#128710,#128711,
#128712,#128713,#128714,#128715,#128716,#128717,#128718,#128719,#128720,
#128721,#128722,#128723,#128724,#128725,#128726,#128727,#128728,#128729,
#128730,#128731,#128732,#128733,#128734,#128735,#128736,#128737,#128738,
#128739,#128740,#128741,#128742,#128743,#128744,#128745,#128746,#128747,
#128748,#128749,#128750,#128751,#128752,#128753,#128754,#128755,#128756,
#128757,#128758,#128759,#128760,#128761,#128762,#128763,#128764,#128765,
#128766,#128767,#128768,#128769,#128770,#128771,#128772,#128773,#128774,
#128775,#128776,#128777,#128778,#128779,#128780,#128781,#128782,#128783,
#128784,#128785,#128786,#128787,#128788,#128789,#128790,#128791,#128792,
#128793,#128794,#128795,#128796,#128797,#128798,#128799,#128800,#128801,
#128802,#128803,#128804,#128805,#128806,#128807,#128808,#128809,#128810,
#128811,#128812,#128813,#128814,#128815,#128816,#128817,#128818,#128819,
#128820,#128821,#128822,#128823,#128824,#128825,#128826,#128827,#128828,
#128829,#128830,#128831,#128832,#128833,#128834,#128835,#128836,#128837,
#128838,#128839,#128840,#128841,#128842,#128843,#128844,#128845,#128846,
#128847,#128848,#128849,#128850,#128851,#128852,#128853,#128854,#128855,
#128856,#128857,#128858,#128859,#128860,#128861,#128862,#128863,#128864,
#128865,#128866,#128867,#128868,#128869,#128870,#128871,#128872,#128873,
#128874,#128875,#128876,#128877,#128878,#128879,#128880,#128881,#128882,
#128883,#128884,#128885,#128886,#128887,#128888,#128889,#128890,#128891,
#128892,#128893,#128894,#128895,#128896,#128897,#128898,#128899),
 .UNSPECIFIED.,.F.,.F.,(4,3,3,3,3,3,3,3,3,3,3,3,3,3,3,3,3,3,3,3,3,3,3,3,
3,3,3,3,3,3,3,3,3,3,3,3,3,3,3,3,3,3,3,3,3,3,3,3,3,3,3,3,3,3,3,3,3,3,3,3,
3,3,3,3,4),(21.9911485751285,22.0872403174081,22.1717043008718,22.256147550065,
22.3406073668107,22.425073290183,22.5095952809818,22.5745878151691,22.6660564577372,
22.7575140633748,22.8489170049659,22.9402589752051,23.0314877939314,23.0619353129301,
23.1465147382964,23.2310914061769,23.3157113292589,23.4003521854757,23.485071600267,
23.5492828106911,23.6336777965099,23.7180054398437,23.8022829799558,23.8865276125065,
23.9707730961945,24.0550229839529,24.1392928473558,24.2235982686224,24.3080035693484,
24.3924639475768,24.4770490018942,24.5239778062131,24.6055741796599,24.6870642443223,
24.7684687650888,24.8498084045718,24.9311114331568,25.0123964584351,25.0936820583999,
25.1749868101455,25.256382796226,25.3378246210915,25.4194048181547,25.4986728017351,
25.5832623133344,25.6677481822996,25.7521477829318,25.836478417448,25.9207557824206,
26.0050040171561,26.0892387031326,26.1734754092372,26.2577612684093,26.3420733549027,
26.426466141403,26.4733677972571,26.558092298325,26.6427552017966,26.7273710330639,
26.8119574560143,26.8965425130992,26.9607152950181,27.0519430220872,27.143293741985,
27.2010953298595),.UNSPECIFIED.);
#1240=B_SPLINE_CURVE_WITH_KNOTS('',3,(#128900,#128901,#128902,#128903,#128904,
#128905),.UNSPECIFIED.,.F.,.F.,(4,1,1,4),(20.9180878353355,21.1125453218861,
21.5998928196471,21.9911485578925),.UNSPECIFIED.);
#1241=B_SPLINE_CURVE_WITH_KNOTS('',3,(#128907,#128908,#128909,#128910,#128911,
#128912,#128913,#128914,#128915,#128916,#128917,#128918,#128919,#128920,
#128921,#128922,#128923,#128924,#128925,#128926,#128927,#128928,#128929,
#128930,#128931,#128932,#128933,#128934,#128935,#128936,#128937,#128938,
#128939,#128940,#128941,#128942,#128943,#128944,#128945,#128946,#128947,
#128948,#128949),.UNSPECIFIED.,.F.,.F.,(4,3,3,3,3,3,3,3,3,3,3,3,3,3,4),
(20.9181028658617,21.0052267765094,21.092346700924,21.1794852412345,21.2224742952021,
21.3095858066139,21.3966807230111,21.4837788139183,21.5708722938342,21.6579854628141,
21.7098217929631,21.7974543214401,21.8850676348139,21.972670334226,21.9911485751285),
 .UNSPECIFIED.);
#1242=B_SPLINE_CURVE_WITH_KNOTS('',3,(#128950,#128951,#128952,#128953,#128954,
#128955,#128956,#128957,#128958,#128959,#128960,#128961,#128962,#128963,
#128964,#128965,#128966,#128967,#128968,#128969,#128970,#128971,#128972,
#128973,#128974,#128975,#128976,#128977,#128978,#128979,#128980,#128981,
#128982,#128983,#128984,#128985,#128986,#128987,#128988,#128989,#128990,
#128991,#128992,#128993,#128994,#128995,#128996,#128997,#128998,#128999,
#129000,#129001,#129002,#129003,#129004,#129005,#129006,#129007,#129008,
#129009,#129010,#129011,#129012,#129013,#129014,#129015,#129016,#129017,
#129018,#129019,#129020,#129021,#129022,#129023,#129024,#129025,#129026,
#129027,#129028,#129029,#129030,#129031,#129032,#129033,#129034,#129035,
#129036,#129037,#129038,#129039,#129040,#129041,#129042,#129043,#129044,
#129045,#129046,#129047,#129048,#129049,#129050,#129051,#129052,#129053,
#129054,#129055,#129056,#129057,#129058,#129059,#129060,#129061,#129062,
#129063,#129064,#129065,#129066,#129067,#129068,#129069,#129070,#129071,
#129072,#129073,#129074,#129075,#129076,#129077,#129078,#129079,#129080,
#129081,#129082,#129083,#129084,#129085,#129086,#129087,#129088,#129089,
#129090,#129091,#129092,#129093,#129094,#129095,#129096,#129097,#129098,
#129099,#129100,#129101,#129102,#129103,#129104,#129105,#129106,#129107,
#129108,#129109,#129110,#129111,#129112,#129113,#129114,#129115,#129116,
#129117,#129118,#129119,#129120,#129121,#129122,#129123,#129124,#129125,
#129126,#129127,#129128,#129129,#129130,#129131,#129132,#129133,#129134,
#129135,#129136,#129137,#129138,#129139,#129140,#129141,#129142,#129143,
#129144,#129145),.UNSPECIFIED.,.F.,.F.,(4,3,3,3,3,3,3,3,3,3,3,3,3,3,3,3,
3,3,3,3,3,3,3,3,3,3,3,3,3,3,3,3,3,3,3,3,3,3,3,3,3,3,3,3,3,3,3,3,3,3,3,3,
3,3,3,3,3,3,3,3,3,3,3,3,3,4),(21.9911485753162,22.0800610136685,22.1689995435299,
22.1971692907241,22.2842690753762,22.3713523483423,22.4584390318698,22.5455212647318,
22.6326235308353,22.6845167884851,22.7716274880237,22.8587213011356,22.9458178659101,
23.0329095847879,23.1200206482753,23.1718642862461,23.2591959782146,23.3465122652369,
23.4338313118415,23.5211449598873,23.6084751333609,23.6592117840071,23.745693612034,
23.8321565252024,23.9186248608384,24.0050911555494,24.0915863725888,24.1465592817681,
24.2353201956329,24.3240706428451,24.4128143671018,24.5015423533536,24.5902572024438,
24.6339067795291,24.7183716294415,24.8028157469338,24.887276430042,24.9717432184832,
25.0562660667606,25.1212542772901,25.2127216661248,25.304178010292,25.3955797066455,
25.4869204524289,25.5781480948867,25.6086017750511,25.6931817036893,25.7777588769285,
25.8623793056185,25.9470206674601,26.0317405844674,26.0959492728121,26.1803442406884,
26.2646718670789,26.3489493912654,26.4331940089272,26.5174394793458,26.6016893548485,
26.6859592070289,26.7702646181267,26.854669910358,26.9391302810329,27.0237153293477,
27.0706442683341,27.1522360636597,27.2022275832944),.UNSPECIFIED.);
#1243=B_SPLINE_CURVE_WITH_KNOTS('',3,(#129151,#129152,#129153,#129154,#129155,
#129156,#129157,#129158,#129159,#129160,#129161,#129162,#129163,#129164,
#129165,#129166,#129167,#129168,#129169,#129170,#129171,#129172,#129173,
#129174,#129175,#129176,#129177,#129178,#129179,#129180,#129181,#129182,
#129183,#129184,#129185,#129186,#129187,#129188,#129189,#129190,#129191,
#129192,#129193,#129194,#129195,#129196,#129197,#129198,#129199,#129200,
#129201,#129202,#129203,#129204,#129205,#129206,#129207,#129208,#129209,
#129210,#129211,#129212,#129213,#129214,#129215,#129216,#129217,#129218,
#129219,#129220,#129221,#129222,#129223,#129224,#129225,#129226,#129227,
#129228,#129229,#129230,#129231,#129232,#129233,#129234,#129235,#129236,
#129237,#129238,#129239,#129240,#129241,#129242,#129243,#129244,#129245,
#129246,#129247,#129248,#129249,#129250,#129251,#129252,#129253,#129254,
#129255,#129256,#129257,#129258,#129259,#129260,#129261,#129262,#129263,
#129264,#129265,#129266,#129267,#129268,#129269,#129270,#129271,#129272,
#129273,#129274,#129275,#129276,#129277,#129278,#129279,#129280,#129281,
#129282,#129283,#129284,#129285,#129286,#129287,#129288,#129289,#129290,
#129291,#129292,#129293,#129294,#129295,#129296,#129297,#129298,#129299,
#129300,#129301,#129302,#129303,#129304,#129305,#129306,#129307,#129308,
#129309,#129310,#129311,#129312,#129313,#129314,#129315,#129316,#129317,
#129318,#129319,#129320,#129321,#129322,#129323,#129324,#129325,#129326,
#129327,#129328,#129329,#129330,#129331,#129332,#129333,#129334,#129335,
#129336,#129337,#129338,#129339,#129340,#129341,#129342,#129343,#129344,
#129345,#129346),.UNSPECIFIED.,.F.,.F.,(4,3,3,3,3,3,3,3,3,3,3,3,3,3,3,3,
3,3,3,3,3,3,3,3,3,3,3,3,3,3,3,3,3,3,3,3,3,3,3,3,3,3,3,3,3,3,3,3,3,3,3,3,
3,3,3,3,3,3,3,3,3,3,3,3,3,4),(28.2743338824266,28.3664532240664,28.4227577883011,
28.5092520935557,28.5957221727376,28.6821896165034,28.7686504765288,28.8551332349923,
28.9101052860621,28.9974342563849,29.084749014768,29.1720683332772,29.2593832734799,
29.3467162971122,29.3974527838231,29.4845626300906,29.5716559384561,29.6587525257064,
29.7458445655353,29.8329564077084,29.8848002815841,29.9719013840595,30.0589854167833,
30.1460720162916,30.233153687593,30.3202546601055,30.3721477793451,30.4593061161227,
30.5464483504257,30.6335940378146,30.7207351578585,30.8078956184438,30.8594952771061,
30.9466072614862,31.0337024468151,31.1208004982627,31.2078937641911,31.2950064517671,
31.3468427748671,31.4339808001712,31.5211023922076,31.6082271424273,31.6953472086888,
31.7824866195326,31.8341902726282,31.9213169014601,32.0084269463445,32.0955400358983,
32.1826484052062,32.2697761653463,32.3215377703892,32.4086680911823,32.4957818717525,
32.5828987261604,32.6700108677988,32.7571423788036,32.8088852681502,32.8960149192679,
32.9831280267967,33.0702442097147,33.1573556823675,33.2444865341392,33.2962327659112,
33.3833617272961,33.4704751186365,33.4844725969432),.UNSPECIFIED.);
#1244=B_SPLINE_CURVE_WITH_KNOTS('',3,(#129347,#129348,#129349,#129350,#129351,
#129352,#129353,#129354,#129355,#129356,#129357,#129358,#129359,#129360,
#129361,#129362,#129363,#129364,#129365,#129366,#129367,#129368,#129369,
#129370,#129371,#129372,#129373,#129374,#129375,#129376,#129377,#129378,
#129379,#129380,#129381,#129382,#129383,#129384,#129385,#129386),
 .UNSPECIFIED.,.F.,.F.,(4,3,3,3,3,3,3,3,3,3,3,3,3,4),(27.2010953298595,
27.2925386897041,27.3840098150324,27.4480627927791,27.532586803755,27.6170657800487,
27.7015239814603,27.7859674988434,27.8704340010683,27.9354102905401,28.0240768753705,
28.1127462609405,28.2014356078663,28.2743338823081),.UNSPECIFIED.);
#1245=B_SPLINE_CURVE_WITH_KNOTS('',3,(#129388,#129389,#129390,#129391,#129392,
#129393,#129394,#129395,#129396,#129397,#129398,#129399,#129400,#129401,
#129402,#129403,#129404,#129405,#129406,#129407,#129408,#129409,#129410,
#129411,#129412,#129413,#129414,#129415,#129416,#129417,#129418,#129419,
#129420,#129421,#129422,#129423,#129424,#129425,#129426,#129427),
 .UNSPECIFIED.,.F.,.F.,(4,3,3,3,3,3,3,3,3,3,3,3,3,4),(27.2022275832944,
27.2836626347991,27.3650248243015,27.4500641292459,27.5313531074218,27.6126363277832,
27.6939323660065,27.7752598073724,27.8566840072115,27.9381650758108,28.0197686516609,
28.0453392638561,28.1696765530861,28.2743338823081),.UNSPECIFIED.);
#1246=B_SPLINE_CURVE_WITH_KNOTS('',3,(#129428,#129429,#129430,#129431,#129432,
#129433,#129434,#129435,#129436,#129437,#129438,#129439,#129440,#129441),
 .UNSPECIFIED.,.F.,.F.,(4,1,1,1,1,1,1,1,1,1,1,4),(28.2743353147298,29.0200342593781,
29.5073817571391,29.9947292549001,30.4820767526611,30.9694242504221,31.4567717481831,
31.9441192459441,32.4314667437051,32.9188142414661,33.4061617392271,33.4844854782753),
 .UNSPECIFIED.);
#1247=B_SPLINE_CURVE_WITH_KNOTS('',3,(#129447,#129448,#129449,#129450,#129451,
#129452,#129453,#129454,#129455,#129456,#129457,#129458,#129459,#129460,
#129461,#129462,#129463,#129464,#129465,#129466,#129467,#129468,#129469,
#129470,#129471,#129472,#129473,#129474),.UNSPECIFIED.,.F.,.F.,(4,3,3,3,
3,3,3,3,3,4),(13.8747245557601,13.96151957655,14.0483127680288,14.1350983392423,
14.2219048683033,14.289680353232,14.3768161569056,14.4639332617808,14.5510540087977,
14.6348946376199),.UNSPECIFIED.);
#1248=B_SPLINE_CURVE_WITH_KNOTS('',3,(#129477,#129478,#129479,#129480),
 .UNSPECIFIED.,.F.,.F.,(4,4),(14.399609326548,14.6348821263195),
 .UNSPECIFIED.);
#1249=B_SPLINE_CURVE_WITH_KNOTS('',3,(#129486,#129487,#129488,#129489,#129490,
#129491,#129492,#129493,#129494,#129495,#129496,#129497,#129498,#129499,
#129500),.UNSPECIFIED.,.F.,.F.,(4,1,1,1,1,1,1,1,1,1,1,1,4),(15.707963267949,
15.751722846515,16.239070344276,16.7264178420371,17.2137653397981,17.7011128375591,
18.1884603353201,18.6758078330811,19.1631553308421,19.6505028286031,20.1378503263641,
20.6251978241251,20.9180878171796),.UNSPECIFIED.);
#1250=B_SPLINE_CURVE_WITH_KNOTS('',3,(#129501,#129502,#129503,#129504,#129505,
#129506,#129507,#129508,#129509,#129510,#129511,#129512,#129513,#129514,
#129515,#129516,#129517,#129518,#129519,#129520,#129521,#129522,#129523,
#129524,#129525,#129526,#129527,#129528,#129529,#129530,#129531,#129532,
#129533,#129534,#129535,#129536,#129537,#129538,#129539,#129540),
 .UNSPECIFIED.,.F.,.F.,(4,3,3,3,3,3,3,3,3,3,3,3,3,4),(14.6348946376199,
14.7220270519162,14.777027850993,14.8641547740402,14.9512651053716,15.03837846682,
15.1254870990942,15.2126151060248,15.264375348754,15.3512430123807,15.4404230762728,
15.5272738407879,15.6176185543684,15.707963267949),.UNSPECIFIED.);
#1251=B_SPLINE_CURVE_WITH_KNOTS('',3,(#129542,#129543,#129544,#129545,#129546,
#129547),.UNSPECIFIED.,.F.,.F.,(4,1,1,4),(14.6348821263195,14.886956824309,
15.37430432207,15.707963267949),.UNSPECIFIED.);
#1252=B_SPLINE_CURVE_WITH_KNOTS('',3,(#129548,#129549,#129550,#129551,#129552,
#129553,#129554,#129555,#129556,#129557,#129558,#129559,#129560,#129561,
#129562,#129563,#129564,#129565,#129566,#129567,#129568,#129569,#129570,
#129571,#129572,#129573,#129574,#129575,#129576,#129577,#129578,#129579,
#129580,#129581,#129582,#129583,#129584,#129585,#129586,#129587,#129588,
#129589,#129590,#129591,#129592,#129593,#129594,#129595,#129596,#129597,
#129598,#129599,#129600,#129601,#129602,#129603,#129604,#129605,#129606,
#129607,#129608,#129609,#129610,#129611,#129612,#129613,#129614,#129615,
#129616,#129617,#129618,#129619,#129620,#129621,#129622,#129623,#129624,
#129625,#129626,#129627,#129628,#129629,#129630,#129631,#129632,#129633,
#129634,#129635,#129636,#129637,#129638,#129639,#129640,#129641,#129642,
#129643,#129644,#129645,#129646,#129647,#129648,#129649,#129650,#129651,
#129652,#129653,#129654,#129655,#129656,#129657,#129658,#129659,#129660,
#129661,#129662,#129663,#129664,#129665,#129666,#129667,#129668,#129669,
#129670,#129671,#129672,#129673,#129674,#129675,#129676,#129677,#129678,
#129679,#129680,#129681,#129682,#129683,#129684,#129685,#129686,#129687,
#129688,#129689,#129690,#129691,#129692,#129693,#129694,#129695,#129696,
#129697,#129698,#129699,#129700,#129701,#129702,#129703,#129704,#129705,
#129706,#129707,#129708,#129709,#129710,#129711,#129712,#129713,#129714,
#129715,#129716,#129717,#129718,#129719,#129720,#129721,#129722,#129723,
#129724,#129725,#129726,#129727,#129728,#129729,#129730,#129731,#129732,
#129733,#129734,#129735,#129736,#129737,#129738,#129739,#129740),
 .UNSPECIFIED.,.F.,.F.,(4,3,3,3,3,3,3,3,3,3,3,3,3,3,3,3,3,3,3,3,3,3,3,3,
3,3,3,3,3,3,3,3,3,3,3,3,3,3,3,3,3,3,3,3,3,3,3,3,3,3,3,3,3,3,3,3,3,3,3,3,
3,3,3,3,4),(15.7079632709815,15.7983388023486,15.861651819831,15.9487475083028,
16.0358262241585,16.122907705879,16.2099843848246,16.2970806037435,16.348999317592,
16.4361366409196,16.5232574899998,16.6103814427677,16.6975006825434,16.784639229082,
16.836346815353,16.9234776545726,17.010591981452,17.0977094188805,17.1848221629971,
17.2719543014269,17.323694313114,17.4108212370465,17.4979315692867,17.5850449316705,
17.6721535648929,17.7592815727834,17.811041810875,17.898173425061,17.9852885231696,
18.0724067185609,18.1595202112614,18.2466530771275,18.298389308636,18.3855180493059,
18.4726302285909,18.559745465589,18.6468559845724,18.7339858790278,18.785736806397,
18.8728666485425,18.959979950145,19.0470963297829,19.1342080001734,19.2213390494988,
19.273084304158,19.3602139689286,19.4473270846037,19.534443267337,19.6215547350878,
19.7086855747234,19.760431801919,19.8475621199502,19.9346758967653,20.0217927459667,
20.1089048815892,20.1960363853822,20.24777929968,20.3349058916832,20.4220159234169,
20.5091290354302,20.5962374473095,20.6833652806739,20.735126797441,20.8266148322207,
20.9181028670005),.UNSPECIFIED.);
#1253=B_SPLINE_CURVE_WITH_KNOTS('',3,(#129746,#129747,#129748,#129749,#129750,
#129751,#129752,#129753,#129754,#129755,#129756,#129757,#129758,#129759,
#129760,#129761,#129762,#129763,#129764,#129765,#129766,#129767,#129768,
#129769,#129770,#129771,#129772,#129773,#129774,#129775,#129776,#129777,
#129778,#129779,#129780,#129781,#129782,#129783,#129784,#129785,#129786,
#129787,#129788,#129789,#129790,#129791,#129792,#129793,#129794,#129795,
#129796,#129797,#129798,#129799,#129800,#129801,#129802,#129803,#129804,
#129805,#129806,#129807,#129808,#129809,#129810,#129811,#129812,#129813,
#129814,#129815,#129816,#129817,#129818,#129819,#129820,#129821,#129822,
#129823,#129824,#129825,#129826,#129827,#129828,#129829,#129830,#129831,
#129832,#129833,#129834,#129835,#129836,#129837,#129838,#129839,#129840,
#129841,#129842,#129843,#129844,#129845,#129846,#129847,#129848,#129849,
#129850,#129851,#129852,#129853,#129854,#129855,#129856,#129857,#129858,
#129859,#129860,#129861,#129862,#129863,#129864,#129865,#129866,#129867,
#129868,#129869,#129870,#129871,#129872,#129873,#129874,#129875,#129876,
#129877,#129878,#129879,#129880,#129881,#129882,#129883,#129884,#129885,
#129886,#129887,#129888,#129889,#129890,#129891,#129892,#129893,#129894,
#129895,#129896,#129897,#129898,#129899,#129900,#129901,#129902,#129903,
#129904,#129905,#129906,#129907,#129908,#129909,#129910,#129911,#129912,
#129913,#129914,#129915,#129916,#129917,#129918,#129919,#129920,#129921,
#129922,#129923,#129924,#129925,#129926,#129927,#129928,#129929,#129930,
#129931,#129932,#129933,#129934,#129935,#129936,#129937,#129938),
 .UNSPECIFIED.,.F.,.F.,(4,3,3,3,3,3,3,3,3,3,3,3,3,3,3,3,3,3,3,3,3,3,3,3,
3,3,3,3,3,3,3,3,3,3,3,3,3,3,3,3,3,3,3,3,3,3,3,3,3,3,3,3,3,3,3,3,3,3,3,3,
3,3,3,3,4),(21.9911485751285,22.0872403174081,22.1717077643695,22.2561544844513,
22.3406177643316,22.4250871456575,22.5096125640496,22.5745878151691,22.6660514455681,
22.7575040081467,22.8489019715955,22.9402390467649,23.0314631630385,23.0619353129301,
23.1465167513392,23.2310954406082,23.3157173860693,23.4003602647288,23.4850816883209,
23.5492828106911,23.6336777241022,23.718005299017,23.8022827747739,23.8865273471115,
23.9707727770584,24.0550226151273,24.1392924329723,24.2235978128946,24.3080030789759,
24.392463426326,24.4770484559771,24.5239778062131,24.605573799559,24.687063482264,
24.768467619494,24.8498068741233,24.9311095168766,25.0123941556193,25.0936793685603,
25.1749837330107,25.2563793332897,25.337820772415,25.419400587678,25.4986728017351,
25.583262289203,25.6677481290383,25.7521476956501,25.8364782913607,25.9207556105826,
26.0050037953159,26.0892384271216,26.1734750749651,26.2577608699837,26.3420728889482,
26.4264656031797,26.4733677972571,26.5580943048163,26.642759224378,26.727377075819,
26.811965520082,26.8965525888318,26.9607152950181,27.0519383065955,27.1432841150039,
27.2010954696436),.UNSPECIFIED.);
#1254=B_SPLINE_CURVE_WITH_KNOTS('',3,(#129939,#129940,#129941,#129942,#129943,
#129944),.UNSPECIFIED.,.F.,.F.,(4,1,1,4),(20.9180878171796,21.1125453218861,
21.5998928196471,21.991148557883),.UNSPECIFIED.);
#1255=B_SPLINE_CURVE_WITH_KNOTS('',3,(#129946,#129947,#129948,#129949,#129950,
#129951,#129952,#129953,#129954,#129955,#129956,#129957,#129958,#129959,
#129960,#129961,#129962,#129963,#129964,#129965,#129966,#129967,#129968,
#129969,#129970,#129971,#129972,#129973,#129974,#129975,#129976,#129977,
#129978,#129979,#129980,#129981,#129982,#129983,#129984,#129985,#129986,
#129987,#129988),.UNSPECIFIED.,.F.,.F.,(4,3,3,3,3,3,3,3,3,3,3,3,3,3,4),
(20.9181028670005,21.0052267362147,21.0923466194079,21.179485119142,21.222474295202,
21.3095858862927,21.3966808826214,21.4837790530665,21.5708726121089,21.6579858588928,
21.709821792963,21.797454164746,21.8850673211435,21.9726698643262,21.9911485751285),
 .UNSPECIFIED.);
#1256=B_SPLINE_CURVE_WITH_KNOTS('',3,(#129989,#129990,#129991,#129992,#129993,
#129994,#129995,#129996,#129997,#129998,#129999,#130000,#130001,#130002,
#130003,#130004,#130005,#130006,#130007,#130008,#130009,#130010,#130011,
#130012,#130013,#130014,#130015,#130016,#130017,#130018,#130019,#130020,
#130021,#130022,#130023,#130024,#130025,#130026,#130027,#130028,#130029,
#130030,#130031,#130032,#130033,#130034,#130035,#130036,#130037,#130038,
#130039,#130040,#130041,#130042,#130043,#130044,#130045,#130046,#130047,
#130048,#130049,#130050,#130051,#130052,#130053,#130054,#130055,#130056,
#130057,#130058,#130059,#130060,#130061,#130062,#130063,#130064,#130065,
#130066,#130067,#130068,#130069,#130070,#130071,#130072,#130073,#130074,
#130075,#130076,#130077,#130078,#130079,#130080,#130081,#130082,#130083,
#130084,#130085,#130086,#130087,#130088,#130089,#130090,#130091,#130092,
#130093,#130094,#130095,#130096,#130097,#130098,#130099,#130100,#130101,
#130102,#130103,#130104,#130105,#130106,#130107,#130108,#130109,#130110,
#130111,#130112,#130113,#130114,#130115,#130116,#130117,#130118,#130119,
#130120,#130121,#130122,#130123,#130124,#130125,#130126,#130127,#130128,
#130129,#130130,#130131,#130132,#130133,#130134,#130135,#130136,#130137,
#130138,#130139,#130140,#130141,#130142,#130143,#130144,#130145,#130146,
#130147,#130148,#130149,#130150,#130151,#130152,#130153,#130154,#130155,
#130156,#130157,#130158,#130159,#130160,#130161,#130162,#130163,#130164,
#130165,#130166,#130167,#130168,#130169,#130170,#130171,#130172,#130173,
#130174,#130175,#130176,#130177,#130178,#130179,#130180,#130181,#130182,
#130183,#130184),.UNSPECIFIED.,.F.,.F.,(4,3,3,3,3,3,3,3,3,3,3,3,3,3,3,3,
3,3,3,3,3,3,3,3,3,3,3,3,3,3,3,3,3,3,3,3,3,3,3,3,3,3,3,3,3,3,3,3,3,3,3,3,
3,3,3,3,3,3,3,3,3,3,3,3,3,4),(21.9911485753162,22.0800609495919,22.168999417996,
22.1971692907241,22.2842691742849,22.3713525460866,22.4584393273926,22.5455216572055,
22.6326240181457,22.6845167884851,22.7716275763734,22.8587214790213,22.9458181342347,
23.0329099438452,23.120021097721,23.1718642862461,23.2591953323291,23.3465109695105,
23.4338293669418,23.5211423678883,23.60847190326,23.6592117840071,23.7456953098164,
23.832159927636,23.9186299638456,24.005097953844,24.0915948443439,24.1465592817681,
24.2353164039209,24.3240630384395,24.4128029701689,24.5015271920606,24.5902383597612,
24.6339067795291,24.7183759992437,24.8028244958566,24.8872895482853,24.9717606994971,
25.0562878722159,25.1212542772901,25.212715341686,25.3041653224886,25.3955607374181,
25.486895306588,25.578117015447,25.6086017750511,25.6931842451492,25.7777639703814,
25.8623869523081,25.9470308674618,26.0317533205491,26.0959492728121,26.1803441484525,
26.2646716876325,26.3489491297302,26.433193670525,26.5174390722406,26.6016888841523,
26.6859586779554,26.770264035995,26.8546692836303,26.9391296144661,27.0237146307952,
27.0706442683341,27.1522355848392,27.2022276034959),.UNSPECIFIED.);
#1257=B_SPLINE_CURVE_WITH_KNOTS('',3,(#130190,#130191,#130192,#130193,#130194,
#130195,#130196,#130197,#130198,#130199,#130200,#130201,#130202,#130203,
#130204,#130205,#130206,#130207,#130208,#130209,#130210,#130211,#130212,
#130213,#130214,#130215,#130216,#130217,#130218,#130219,#130220,#130221,
#130222,#130223,#130224,#130225,#130226,#130227,#130228,#130229,#130230,
#130231,#130232,#130233,#130234,#130235,#130236,#130237,#130238,#130239,
#130240,#130241,#130242,#130243,#130244,#130245,#130246,#130247,#130248,
#130249,#130250,#130251,#130252,#130253,#130254,#130255,#130256,#130257,
#130258,#130259,#130260,#130261,#130262,#130263,#130264,#130265,#130266,
#130267,#130268,#130269,#130270,#130271,#130272,#130273,#130274,#130275,
#130276,#130277,#130278,#130279,#130280,#130281,#130282,#130283,#130284,
#130285,#130286,#130287,#130288,#130289,#130290,#130291,#130292,#130293,
#130294,#130295,#130296,#130297,#130298,#130299,#130300,#130301,#130302,
#130303,#130304,#130305,#130306,#130307,#130308,#130309,#130310,#130311,
#130312,#130313,#130314,#130315,#130316,#130317,#130318,#130319,#130320,
#130321,#130322,#130323,#130324,#130325,#130326,#130327,#130328,#130329,
#130330,#130331,#130332,#130333,#130334,#130335,#130336,#130337,#130338,
#130339,#130340,#130341,#130342,#130343,#130344,#130345,#130346,#130347,
#130348,#130349,#130350,#130351,#130352,#130353,#130354,#130355,#130356,
#130357,#130358,#130359,#130360,#130361,#130362,#130363,#130364,#130365,
#130366,#130367,#130368,#130369,#130370,#130371,#130372,#130373,#130374,
#130375,#130376,#130377,#130378,#130379,#130380,#130381,#130382,#130383,
#130384,#130385),.UNSPECIFIED.,.F.,.F.,(4,3,3,3,3,3,3,3,3,3,3,3,3,3,3,3,
3,3,3,3,3,3,3,3,3,3,3,3,3,3,3,3,3,3,3,3,3,3,3,3,3,3,3,3,3,3,3,3,3,3,3,3,
3,3,3,3,3,3,3,3,3,3,3,3,3,4),(28.2743338824266,28.3664499676938,28.4227577883011,
28.5092534192787,28.5957248380328,28.6821936309558,28.768655843137,28.8551399477051,
28.9101052860621,28.9974337506621,29.0847479974582,29.1720668007956,29.2593812251369,
29.3467137364858,29.3974527838231,29.4845627017913,29.5716560821199,29.658752741023,
29.7458448521569,29.8329567644714,29.8848002815841,29.9719014591824,30.0589855683635,
30.1460722455977,30.2331539951607,30.3202550460865,30.3721477793451,30.4593060263713,
30.5464481695862,30.6335937647714,30.7207347922023,30.8078951603531,30.8594952771061,
30.9466073231606,31.0337025710101,31.1208006856437,31.2078940149848,31.2950067657722,
31.3468427748671,31.4339807679861,31.5211023274172,31.6082270447182,31.6953470779628,
31.7824864559265,31.8341902726281,31.9213169142658,32.0084269721101,32.0955400747291,
32.1826484571305,32.2697762302935,32.3215377703891,32.4086680878499,32.4957818650579,
32.5828987160914,32.6700108543567,32.75714236202,32.8088852681501,32.8960149195982,
32.9831280274467,33.0702442106651,33.1573556836068,33.2444865356467,33.2962327659111,
33.3833617264479,33.4704751169556,33.4844725988534),.UNSPECIFIED.);
#1258=B_SPLINE_CURVE_WITH_KNOTS('',3,(#130386,#130387,#130388,#130389,#130390,
#130391,#130392,#130393,#130394,#130395,#130396,#130397,#130398,#130399,
#130400,#130401,#130402,#130403,#130404,#130405,#130406,#130407,#130408,
#130409,#130410,#130411,#130412,#130413,#130414,#130415,#130416,#130417,
#130418,#130419,#130420,#130421,#130422,#130423,#130424,#130425),
 .UNSPECIFIED.,.F.,.F.,(4,3,3,3,3,3,3,3,3,3,3,3,3,4),(27.2010954696436,
27.2925337945715,27.3839999022843,27.4480627927791,27.5325902280114,27.617072650843,
27.7015343147517,27.7859813021922,27.8704512660146,27.9354102905401,28.0240739238239,
28.1127403128143,28.2014266288529,28.2743338823081),.UNSPECIFIED.);
#1259=B_SPLINE_CURVE_WITH_KNOTS('',3,(#130427,#130428,#130429,#130430,#130431,
#130432,#130433,#130434,#130435,#130436,#130437,#130438,#130439,#130440,
#130441,#130442,#130443,#130444,#130445,#130446,#130447,#130448,#130449,
#130450,#130451,#130452,#130453,#130454,#130455,#130456,#130457,#130458,
#130459,#130460,#130461,#130462,#130463,#130464,#130465,#130466),
 .UNSPECIFIED.,.F.,.F.,(4,3,3,3,3,3,3,3,3,3,3,3,3,4),(27.2022276034959,
27.2836621718988,27.3650238767157,27.4500633001082,27.5313517914947,27.6126345246834,
27.6939300756229,27.7752570298697,27.8566807447005,27.9381613288421,28.0197644242444,
28.0453392638561,28.1696867713369,28.2743338823081),.UNSPECIFIED.);
#1260=B_SPLINE_CURVE_WITH_KNOTS('',3,(#130467,#130468,#130469,#130470,#130471,
#130472,#130473,#130474,#130475,#130476,#130477,#130478,#130479,#130480),
 .UNSPECIFIED.,.F.,.F.,(4,1,1,1,1,1,1,1,1,1,1,4),(28.2743353127056,29.0200342593781,
29.5073817571391,29.9947292549001,30.4820767526611,30.9694242504221,31.4567717481831,
31.9441192459441,32.4314667437051,32.9188142414661,33.4061617392271,33.4844854751707),
 .UNSPECIFIED.);
#1261=B_SPLINE_CURVE_WITH_KNOTS('',3,(#130486,#130487,#130488,#130489,#130490,
#130491,#130492,#130493),.UNSPECIFIED.,.F.,.F.,(4,1,1,1,1,4),(15.707963267949,
15.8622700343739,16.8611064843358,17.8599429342977,18.8587793842595,19.7647623348627),
 .UNSPECIFIED.);
#1262=B_SPLINE_CURVE_WITH_KNOTS('',3,(#130495,#130496,#130497,#130498,#130499,
#130500,#130501,#130502,#130503,#130504,#130505,#130506,#130507,#130508,
#130509,#130510,#130511,#130512,#130513,#130514,#130515,#130516,#130517,
#130518,#130519,#130520,#130521,#130522,#130523,#130524,#130525,#130526,
#130527,#130528,#130529,#130530,#130531,#130532,#130533,#130534,#130535,
#130536,#130537,#130538,#130539,#130540,#130541,#130542,#130543,#130544,
#130545,#130546,#130547,#130548,#130549,#130550,#130551,#130552),
 .UNSPECIFIED.,.F.,.F.,(4,3,3,3,3,3,3,3,3,3,3,3,3,3,3,3,3,3,3,4),(13.8757070305574,
13.9742332816752,14.0726192270832,14.1714710217493,14.269679438043,14.3678547454402,
14.4660265209369,14.5653782868057,14.6636879754741,14.7635607799431,14.8634335844121,
14.9606976685948,15.0578044132827,15.154822913635,15.2517842191042,15.3487193065272,
15.4457083690103,15.5427241666821,15.6398692546785,15.707963267949),
 .UNSPECIFIED.);
#1263=B_SPLINE_CURVE_WITH_KNOTS('',3,(#130556,#130557,#130558,#130559,#130560),
 .UNSPECIFIED.,.F.,.F.,(4,1,4),(14.3986268518925,15.3974633018543,15.707963267949),
 .UNSPECIFIED.);
#1264=B_SPLINE_CURVE_WITH_KNOTS('',3,(#130561,#130562,#130563,#130564,#130565,
#130566,#130567,#130568),.UNSPECIFIED.,.F.,.F.,(4,1,1,1,1,4),(15.707963267949,
16.3962997518162,17.3951362017781,18.39397265174,19.3928091017018,19.7659327733658),
 .UNSPECIFIED.);
#1265=B_SPLINE_CURVE_WITH_KNOTS('',3,(#130574,#130575,#130576,#130577,#130578,
#130579,#130580,#130581),.UNSPECIFIED.,.F.,.F.,(4,1,1,1,1,4),(21.9911485751286,
22.854125184107,23.8529616340689,24.8517980840308,25.8506345339927,26.0493850673138),
 .UNSPECIFIED.);
#1266=B_SPLINE_CURVE_WITH_KNOTS('',3,(#130582,#130583,#130584,#130585,#130586,
#130587,#130588),.UNSPECIFIED.,.F.,.F.,(4,1,1,1,4),(19.7647623348627,19.8576158342214,
20.8564522841833,21.8552887341452,21.9911485751286),.UNSPECIFIED.);
#1267=B_SPLINE_CURVE_WITH_KNOTS('',3,(#130590,#130591,#130592,#130593,#130594,
#130595),.UNSPECIFIED.,.F.,.F.,(4,1,1,4),(19.7659327733658,20.3916455516637,
21.3904820016256,21.9911485751286),.UNSPECIFIED.);
#1268=B_SPLINE_CURVE_WITH_KNOTS('',3,(#130596,#130597,#130598,#130599,#130600,
#130601,#130602,#130603,#130604,#130605,#130606,#130607,#130608,#130609,
#130610,#130611,#130612,#130613,#130614,#130615,#130616,#130617,#130618,
#130619,#130620,#130621,#130622,#130623,#130624,#130625,#130626,#130627,
#130628,#130629,#130630,#130631,#130632,#130633,#130634,#130635,#130636,
#130637,#130638,#130639,#130640,#130641,#130642,#130643,#130644,#130645,
#130646,#130647,#130648,#130649,#130650,#130651,#130652,#130653,#130654,
#130655,#130656,#130657,#130658,#130659,#130660,#130661,#130662,#130663,
#130664,#130665,#130666,#130667,#130668,#130669,#130670,#130671,#130672,
#130673,#130674,#130675,#130676,#130677,#130678,#130679,#130680,#130681,
#130682,#130683,#130684,#130685,#130686,#130687,#130688,#130689,#130690,
#130691,#130692,#130693,#130694,#130695,#130696,#130697,#130698,#130699,
#130700,#130701,#130702,#130703,#130704,#130705,#130706,#130707,#130708,
#130709,#130710,#130711,#130712,#130713,#130714,#130715,#130716,#130717,
#130718,#130719),.UNSPECIFIED.,.F.,.F.,(4,3,3,3,3,3,3,3,3,3,3,3,3,3,3,3,
3,3,3,3,3,3,3,3,3,3,3,3,3,3,3,3,3,3,3,3,3,3,3,3,3,4),(21.9911487995834,
22.0999040669592,22.2090426071739,22.318716159435,22.3893184515875,22.4879213274736,
22.5863838945598,22.6866052704335,22.7848896590421,22.8831410757094,22.9813889965946,
23.0830804728333,23.1814696748722,23.2848122882107,23.3881549015493,23.486755194993,
23.585215198191,23.685437217356,23.7837191074787,23.8819680557453,23.9802135417613,
24.0819079941988,24.1802948708398,24.2836431111755,24.3869913515112,24.4855869791747,
24.584042226434,24.6842654233139,24.7825423701227,24.8807863158073,24.9790267464169,
25.0807270101809,25.1791087505825,25.2824682760278,25.3858278014731,25.4844081043906,
25.5828572791635,25.6812050451075,25.7794880184323,25.8777310276212,25.9759959080335,
26.0480412283342),.UNSPECIFIED.);
#1269=B_SPLINE_CURVE_WITH_KNOTS('',3,(#130725,#130726,#130727,#130728,#130729,
#130730,#130731,#130732,#130733,#130734,#130735,#130736,#130737,#130738,
#130739,#130740,#130741,#130742,#130743,#130744,#130745,#130746,#130747,
#130748,#130749,#130750,#130751,#130752,#130753,#130754,#130755,#130756,
#130757,#130758,#130759,#130760,#130761,#130762,#130763,#130764,#130765,
#130766,#130767,#130768,#130769,#130770,#130771,#130772,#130773,#130774,
#130775,#130776,#130777,#130778,#130779,#130780,#130781,#130782,#130783,
#130784,#130785,#130786,#130787,#130788,#130789,#130790,#130791,#130792,
#130793,#130794,#130795,#130796,#130797,#130798,#130799,#130800,#130801,
#130802,#130803,#130804,#130805,#130806,#130807,#130808,#130809,#130810,
#130811,#130812,#130813,#130814,#130815,#130816,#130817,#130818,#130819,
#130820,#130821,#130822,#130823,#130824,#130825,#130826,#130827,#130828,
#130829,#130830,#130831,#130832,#130833,#130834,#130835,#130836,#130837,
#130838,#130839,#130840,#130841,#130842,#130843,#130844,#130845,#130846,
#130847,#130848),.UNSPECIFIED.,.F.,.F.,(4,3,3,3,3,3,3,3,3,3,3,3,3,3,3,3,
3,3,3,3,3,3,3,3,3,3,3,3,3,3,3,3,3,3,3,3,3,3,3,3,3,4),(28.2743338823082,
28.3746245108422,28.4749734042942,28.5754886326583,28.6760922711292,28.7769068634701,
28.8471438838783,28.9457420298706,29.0441998338806,29.1444223963755,29.2427019757815,
29.3409485766512,29.4391916815761,29.5408888446421,29.6392732799478,29.742626806894,
29.8459803338402,29.9445784592305,30.0430362424602,30.1432588101279,30.2415383684702,
30.3397849482168,30.4380280319867,30.5397252199405,30.6381096342302,30.7414632090161,
30.844816783802,30.9434149029363,31.0418726797403,31.1420952489933,31.2403748005386,
31.3386213733642,31.4368644500979,31.5385616460144,31.6369460530499,31.7402996434069,
31.8436532337639,31.9422528703022,32.0406907036442,32.139033758075,32.2373181769404,
32.3317147877909),.UNSPECIFIED.);
#1270=B_SPLINE_CURVE_WITH_KNOTS('',3,(#130849,#130850,#130851,#130852,#130853,
#130854),.UNSPECIFIED.,.F.,.F.,(4,1,1,4),(26.0493850673138,26.8494709839545,
27.8483074339164,28.2743284150372),.UNSPECIFIED.);
#1271=B_SPLINE_CURVE_WITH_KNOTS('',3,(#130856,#130857,#130858,#130859,#130860,
#130861,#130862,#130863,#130864,#130865,#130866,#130867,#130868,#130869,
#130870,#130871,#130872,#130873,#130874,#130875,#130876,#130877,#130878,
#130879,#130880,#130881,#130882,#130883,#130884,#130885,#130886,#130887,
#130888,#130889,#130890,#130891,#130892,#130893,#130894,#130895,#130896,
#130897,#130898,#130899,#130900,#130901,#130902,#130903,#130904,#130905,
#130906,#130907,#130908,#130909,#130910,#130911,#130912,#130913,#130914,
#130915,#130916,#130917,#130918,#130919,#130920,#130921,#130922,#130923,
#130924,#130925,#130926,#130927,#130928),.UNSPECIFIED.,.F.,.F.,(4,3,3,3,
3,3,3,3,3,3,3,3,3,3,3,3,3,3,3,3,3,3,3,3,4),(26.0480412283342,26.1464094056132,
26.2448398400683,26.3434312868597,26.3846642514349,26.4832625888546,26.5817205901414,
26.6819431040484,26.7802228937311,26.8784697092845,26.9767130330315,27.0784099501228,
27.1767946124098,27.2801476569033,27.3835007013968,27.4808124354761,27.5800026163015,
27.6770619119092,27.7740624145151,27.8710350582304,27.9718597641926,28.0689211628773,
28.1660361043295,28.2632831523914,28.2743338820794),.UNSPECIFIED.);
#1272=B_SPLINE_CURVE_WITH_KNOTS('',3,(#130929,#130930,#130931,#130932,#130933,
#130934,#130935,#130936,#130937,#130938,#130939,#130940,#130941,#130942,
#130943,#130944,#130945,#130946,#130947,#130948,#130949,#130950,#130951,
#130952,#130953,#130954,#130955,#130956,#130957,#130958,#130959,#130960,
#130961,#130962,#130963,#130964,#130965,#130966,#130967,#130968,#130969,
#130970,#130971,#130972,#130973,#130974,#130975,#130976,#130977,#130978,
#130979,#130980,#130981,#130982,#130983,#130984,#130985,#130986,#130987,
#130988,#130989,#130990,#130991,#130992,#130993,#130994,#130995,#130996,
#130997,#130998,#130999,#131000,#131001,#131002,#131003,#131004,#131005,
#131006,#131007,#131008,#131009,#131010,#131011,#131012,#131013,#131014,
#131015,#131016,#131017,#131018,#131019,#131020,#131021,#131022,#131023,
#131024,#131025,#131026,#131027,#131028,#131029,#131030,#131031,#131032,
#131033,#131034,#131035,#131036,#131037,#131038,#131039,#131040,#131041,
#131042,#131043,#131044,#131045,#131046,#131047,#131048,#131049,#131050,
#131051,#131052),.UNSPECIFIED.,.F.,.F.,(4,3,3,3,3,3,3,3,3,3,3,3,3,3,3,3,
3,3,3,3,3,3,3,3,3,3,3,3,3,3,3,3,3,3,3,3,3,3,3,3,3,4),(28.2743338823082,
28.3823371513587,28.4809354101241,28.5793933280734,28.6796158622293,28.7778955576022,
28.8761422749412,28.9743854966836,29.0760825228428,29.1744670746393,29.27782033798,
29.3811736013206,29.4797717427214,29.5782295425657,29.6784521061552,29.7767316824828,
29.8749782806886,29.9732213833692,30.0749185503475,30.1733029844888,30.2766565178856,
30.3800100512824,30.4786081310516,30.5770658678374,30.6772884470132,30.775567957224,
30.8738144883134,30.9720575229635,31.0737547675337,31.1721391320451,31.2754928166447,
31.3788465012443,31.4774477473609,31.5759078066966,31.6742504131636,31.7725287580314,
31.8707723649811,31.969010716645,32.0673303011073,32.165692245105,32.2642027660236,
32.3314303398525),.UNSPECIFIED.);
#1273=B_SPLINE_CURVE_WITH_KNOTS('',3,(#131058,#131059,#131060,#131061,#131062,
#131063,#131064,#131065,#131066,#131067,#131068,#131069,#131070,#131071,
#131072,#131073,#131074,#131075,#131076,#131077,#131078,#131079,#131080,
#131081,#131082,#131083,#131084,#131085,#131086,#131087,#131088,#131089,
#131090,#131091,#131092,#131093,#131094,#131095,#131096,#131097,#131098,
#131099,#131100,#131101,#131102,#131103,#131104,#131105,#131106,#131107,
#131108,#131109,#131110,#131111,#131112,#131113,#131114,#131115,#131116,
#131117,#131118,#131119,#131120,#131121,#131122,#131123,#131124,#131125,
#131126,#131127,#131128,#131129,#131130,#131131,#131132,#131133,#131134,
#131135,#131136,#131137,#131138,#131139,#131140,#131141,#131142,#131143,
#131144,#131145,#131146,#131147,#131148,#131149,#131150,#131151,#131152,
#131153,#131154,#131155,#131156,#131157,#131158,#131159,#131160,#131161,
#131162,#131163,#131164,#131165,#131166,#131167,#131168,#131169,#131170,
#131171,#131172,#131173,#131174,#131175,#131176,#131177,#131178,#131179,
#131180,#131181),.UNSPECIFIED.,.F.,.F.,(4,3,3,3,3,3,3,3,3,3,3,3,3,3,3,3,
3,3,3,3,3,3,3,3,3,3,3,3,3,3,3,3,3,3,3,3,3,3,3,3,3,4),(34.5575191897594,
34.6782345503758,34.8009387396348,34.8401625836495,34.9387607091264,35.0372184923827,
35.1374410600363,35.2357206182558,35.3339671978241,35.4322102813602,35.533907469423,
35.6322918833412,35.7356454584763,35.8389990336114,35.9375971585486,36.036054941259,
36.1362775090483,36.234557066711,36.3328036457193,36.4310467286934,36.5327439174134,
36.6311283307699,36.7344819071716,36.8378354835733,36.9364336084869,37.0348913911719,
37.1351139589673,37.2333935165999,37.3316400955765,37.4298831785171,37.5315803672716,
37.629964780591,37.7333183570631,37.8366719335352,37.9352415778354,38.0336830992399,
38.1320262040974,38.2303004962056,38.3285627936512,38.4268127465159,38.5251372404659,
38.6142676516065),.UNSPECIFIED.);
#1274=B_SPLINE_CURVE_WITH_KNOTS('',3,(#131182,#131183,#131184,#131185,#131186,
#131187,#131188,#131189,#131190,#131191,#131192,#131193,#131194,#131195,
#131196,#131197,#131198,#131199,#131200,#131201,#131202,#131203,#131204,
#131205,#131206,#131207,#131208,#131209,#131210,#131211,#131212,#131213,
#131214,#131215,#131216,#131217,#131218,#131219,#131220,#131221,#131222,
#131223,#131224,#131225,#131226,#131227,#131228,#131229,#131230,#131231,
#131232,#131233,#131234,#131235,#131236,#131237,#131238,#131239,#131240,
#131241,#131242,#131243,#131244,#131245,#131246,#131247,#131248,#131249,
#131250,#131251,#131252,#131253,#131254),.UNSPECIFIED.,.F.,.F.,(4,3,3,3,
3,3,3,3,3,3,3,3,3,3,3,3,3,3,3,3,3,3,3,3,4),(32.3317147877909,32.4299572675061,
32.5330903715611,32.631472295279,32.7299238178561,32.8285286698518,32.8424896837258,
32.9410878085162,33.0395455910852,33.1397681589105,33.2380477164451,33.3362942953312,
33.4345373781883,33.5362345670632,33.6346189803181,33.7379725570029,33.8413261336877,
33.9390973941519,34.0367388270572,34.1342810926927,34.2317547370095,34.3292101035806,
34.4266554953363,34.5241539309141,34.5575191894878),.UNSPECIFIED.);
#1275=B_SPLINE_CURVE_WITH_KNOTS('',3,(#131256,#131257,#131258,#131259,#131260,
#131261,#131262,#131263,#131264,#131265,#131266,#131267,#131268,#131269,
#131270,#131271,#131272,#131273,#131274,#131275,#131276,#131277,#131278,
#131279,#131280,#131281,#131282,#131283,#131284,#131285,#131286,#131287,
#131288,#131289,#131290,#131291,#131292,#131293,#131294,#131295,#131296,
#131297,#131298,#131299,#131300,#131301,#131302,#131303,#131304,#131305,
#131306,#131307,#131308,#131309,#131310,#131311,#131312,#131313,#131314,
#131315,#131316,#131317,#131318,#131319,#131320,#131321,#131322,#131323,
#131324,#131325),.UNSPECIFIED.,.F.,.F.,(4,3,3,3,3,3,3,3,3,3,3,3,3,3,3,3,
3,3,3,3,3,3,3,4),(32.3314303398525,32.3776829512062,32.4762810765961,32.5747388598254,
32.6749614274933,32.7732409858351,32.8714875655812,32.9697306493509,33.0714278373052,
33.1698122515945,33.2731658263813,33.3765194011681,33.4751175203003,33.5735752971024,
33.6737978663559,33.7720774178991,33.8703239907224,33.9685670674539,34.0702642633729,
34.1686486704062,34.272002260768,34.3753558511299,34.5238559809544,34.5575191894878),
 .UNSPECIFIED.);
#1276=B_SPLINE_CURVE_WITH_KNOTS('',3,(#131326,#131327,#131328,#131329,#131330,
#131331,#131332,#131333),.UNSPECIFIED.,.F.,.F.,(4,1,1,1,1,4),(34.5575241470784,
35.3741923010918,36.3730287510537,37.3718652010156,38.3707016509774,38.615783154936),
 .UNSPECIFIED.);
#1277=B_SPLINE_CURVE_WITH_KNOTS('',3,(#131339,#131340,#131341,#131342,#131343,
#131344,#131345,#131346,#131347,#131348,#131349,#131350,#131351,#131352,
#131353,#131354,#131355,#131356,#131357,#131358,#131359,#131360,#131361,
#131362,#131363,#131364,#131365,#131366,#131367,#131368,#131369,#131370,
#131371,#131372,#131373,#131374,#131375,#131376,#131377,#131378,#131379,
#131380,#131381,#131382,#131383,#131384,#131385,#131386,#131387,#131388,
#131389,#131390,#131391,#131392,#131393,#131394,#131395,#131396,#131397,
#131398,#131399,#131400,#131401,#131402,#131403,#131404,#131405,#131406,
#131407,#131408,#131409,#131410,#131411,#131412,#131413,#131414,#131415,
#131416,#131417,#131418,#131419,#131420,#131421,#131422,#131423,#131424,
#131425,#131426,#131427,#131428,#131429,#131430,#131431,#131432,#131433,
#131434,#131435,#131436,#131437,#131438,#131439,#131440,#131441,#131442,
#131443,#131444,#131445,#131446,#131447,#131448,#131449,#131450,#131451,
#131452,#131453,#131454,#131455,#131456,#131457,#131458,#131459,#131460,
#131461,#131462),.UNSPECIFIED.,.F.,.F.,(4,3,3,3,3,3,3,3,3,3,3,3,3,3,3,3,
3,3,3,3,3,3,3,3,3,3,3,3,3,3,3,3,3,3,3,3,3,3,3,3,3,4),(40.8407044969197,
40.9391705387198,41.037496428004,41.1368115911763,41.2349607512892,41.3330774110127,
41.4311912274061,41.5313978539002,41.6296531901072,41.7308354617449,41.8320177333826,
41.9306158583836,42.0290736411577,42.129296208931,42.2275757666565,42.3258223457271,
42.424065428763,42.5257626174084,42.6241470308246,42.7275006070845,42.8308541833445,
42.9294523083471,43.0279100911229,43.1281326588958,43.2264122166228,43.3246587956951,
43.4229018787323,43.5245990673758,43.6229834807933,43.7263370570498,43.8296906333064,
43.9282887583114,44.0267465410896,44.1269691088619,44.2252486665915,44.3234952456664,
44.4217383287063,44.5234355173468,44.621819930767,44.7251735070177,44.8285270832683,
44.898397957106),.UNSPECIFIED.);
#1278=B_SPLINE_CURVE_WITH_KNOTS('',3,(#131463,#131464,#131465,#131466,#131467,
#131468,#131469,#131470,#131471,#131472,#131473,#131474,#131475,#131476,
#131477,#131478,#131479,#131480,#131481,#131482,#131483,#131484,#131485,
#131486,#131487,#131488,#131489,#131490,#131491,#131492,#131493,#131494,
#131495,#131496,#131497,#131498,#131499,#131500,#131501,#131502,#131503,
#131504,#131505,#131506,#131507,#131508,#131509,#131510,#131511,#131512,
#131513,#131514,#131515,#131516,#131517,#131518,#131519,#131520,#131521,
#131522,#131523,#131524,#131525,#131526,#131527,#131528,#131529,#131530,
#131531,#131532,#131533,#131534,#131535),.UNSPECIFIED.,.F.,.F.,(4,3,3,3,
3,3,3,3,3,3,3,3,3,3,3,3,3,3,3,3,3,3,3,3,4),(38.6142676516065,38.7127107058196,
38.8113099209326,38.835508383497,38.9341065084865,39.032564291249,39.1327868590252,
39.231066416739,39.3293129957981,39.4275560788223,39.5292532674815,39.6276376808862,
39.7309912571726,39.8343448334589,39.9329429584521,40.0314007412181,40.1316233089935,
40.2299028667105,40.3281494457725,40.4263925287995,40.5280897174548,40.6264741308619,
40.7298277071414,40.8331812834208,40.8407044966674),.UNSPECIFIED.);
#1279=B_SPLINE_CURVE_WITH_KNOTS('',3,(#131537,#131538,#131539,#131540,#131541,
#131542),.UNSPECIFIED.,.F.,.F.,(4,1,1,4),(38.615783154936,39.3695381009393,
40.3683745509012,40.8407024149445),.UNSPECIFIED.);
#1280=B_SPLINE_CURVE_WITH_KNOTS('',3,(#131543,#131544,#131545,#131546,#131547,
#131548,#131549,#131550,#131551,#131552,#131553,#131554,#131555,#131556,
#131557,#131558,#131559,#131560,#131561,#131562,#131563,#131564,#131565,
#131566,#131567,#131568,#131569,#131570,#131571,#131572,#131573,#131574,
#131575,#131576,#131577,#131578,#131579,#131580,#131581,#131582,#131583,
#131584,#131585,#131586,#131587,#131588,#131589,#131590,#131591,#131592,
#131593,#131594,#131595,#131596,#131597,#131598,#131599,#131600,#131601,
#131602,#131603,#131604,#131605,#131606,#131607,#131608,#131609,#131610,
#131611,#131612,#131613,#131614,#131615,#131616,#131617,#131618,#131619,
#131620,#131621,#131622,#131623,#131624,#131625,#131626,#131627,#131628,
#131629,#131630,#131631,#131632,#131633,#131634,#131635,#131636,#131637,
#131638,#131639,#131640,#131641,#131642,#131643,#131644,#131645,#131646,
#131647,#131648,#131649,#131650,#131651,#131652,#131653,#131654,#131655,
#131656,#131657,#131658,#131659,#131660,#131661,#131662,#131663,#131664,
#131665,#131666,#131667,#131668,#131669),.UNSPECIFIED.,.F.,.F.,(4,3,3,3,
3,3,3,3,3,3,3,3,3,3,3,3,3,3,3,3,3,3,3,3,3,3,3,3,3,3,3,3,3,3,3,3,3,3,3,3,
3,3,4),(40.8407044966674,40.9425310419932,41.0487010317106,41.1508691915795,
41.253165848555,41.355678560324,41.3672110008631,41.4658091258526,41.5642669086151,
41.6644894763913,41.7627690341051,41.8610156131641,41.9592586961882,42.0609558848474,
42.1593402982522,42.2626938745385,42.3660474508249,42.4646455758181,42.5631033585841,
42.6633259263595,42.7616054840764,42.8598520631385,42.9580951461656,43.0597923348209,
43.1581767482281,43.2615303245075,43.3648839007868,43.4634820258002,43.561939808587,
43.6621623763572,43.7604419340954,43.858688513179,43.9569315962279,44.0586287848581,
44.1570131982872,44.260366774518,44.3637203507487,44.462314022054,44.5607732131585,
44.6591152246784,44.7573894748803,44.8556332863466,44.8979422931065),
 .UNSPECIFIED.);
#1281=B_SPLINE_CURVE_WITH_KNOTS('',3,(#131675,#131676,#131677,#131678,#131679,
#131680,#131681,#131682),.UNSPECIFIED.,.F.,.F.,(4,1,1,1,1,4),(47.123889803847,
47.8250364331539,48.8238728831158,49.8227093330776,50.8215457830395,51.1819113926155),
 .UNSPECIFIED.);
#1282=B_SPLINE_CURVE_WITH_KNOTS('',3,(#131683,#131684,#131685,#131686,#131687,
#131688,#131689,#131690,#131691,#131692,#131693,#131694,#131695,#131696,
#131697,#131698,#131699,#131700,#131701,#131702,#131703,#131704,#131705,
#131706,#131707,#131708,#131709,#131710,#131711,#131712,#131713,#131714,
#131715,#131716,#131717,#131718,#131719,#131720,#131721,#131722,#131723,
#131724,#131725,#131726,#131727,#131728,#131729,#131730,#131731,#131732,
#131733,#131734,#131735,#131736,#131737,#131738,#131739,#131740,#131741,
#131742,#131743,#131744,#131745,#131746,#131747,#131748,#131749,#131750,
#131751,#131752),.UNSPECIFIED.,.F.,.F.,(4,3,3,3,3,3,3,3,3,3,3,3,3,3,3,3,
3,3,3,3,3,3,3,4),(44.898397957106,44.9968932559775,45.0952714816404,45.1935672870477,
45.2918209506617,45.3900619643857,45.4883197993756,45.5866859408243,45.6851136892991,
45.7837031645335,45.8273635332301,45.9259616582337,46.0244194410106,46.1246420087832,
46.2229215665112,46.3211681455843,46.4194112286229,46.5211084172651,46.619492830684,
46.722846406938,46.826199983192,46.9466622822371,47.0654828012668,47.1238896269795),
 .UNSPECIFIED.);
#1283=B_SPLINE_CURVE_WITH_KNOTS('',3,(#131754,#131755,#131756,#131757,#131758,
#131759,#131760,#131761,#131762,#131763,#131764,#131765,#131766,#131767,
#131768,#131769,#131770,#131771,#131772,#131773,#131774,#131775,#131776,
#131777,#131778,#131779,#131780,#131781,#131782,#131783,#131784,#131785,
#131786,#131787,#131788,#131789,#131790,#131791,#131792,#131793,#131794,
#131795,#131796,#131797,#131798,#131799,#131800,#131801,#131802,#131803,
#131804,#131805,#131806,#131807,#131808,#131809,#131810,#131811,#131812,
#131813,#131814,#131815,#131816,#131817,#131818,#131819,#131820,#131821,
#131822,#131823),.UNSPECIFIED.,.F.,.F.,(4,3,3,3,3,3,3,3,3,3,3,3,3,3,3,3,
3,3,3,3,3,3,3,4),(44.8979422931065,44.996192493912,45.0945462233762,45.1929541967959,
45.2915321292331,45.3625568007106,45.4611549257132,45.5596127084888,45.6598352762618,
45.7581148339886,45.8563614130606,45.9546044960977,46.0563016847413,46.1546860981588,
46.2580396744156,46.3613932506724,46.4587199838046,46.5559210250952,46.6530274701205,
46.750070296518,46.8471124553622,46.9441490048065,47.0412721236584,47.123889803847),
 .UNSPECIFIED.);
#1284=B_SPLINE_CURVE_WITH_KNOTS('',3,(#131824,#131825,#131826,#131827,#131828,
#131829,#131830,#131831),.UNSPECIFIED.,.F.,.F.,(4,1,1,1,1,4),(47.1238901029355,
47.3602297006343,48.3590661505962,49.3579026005581,50.3567390505199,51.1803881837399),
 .UNSPECIFIED.);
#1285=B_SPLINE_CURVE_WITH_KNOTS('',3,(#131837,#131838,#131839,#131840,#131841,
#131842,#131843,#131844,#131845,#131846,#131847,#131848,#131849,#131850,
#131851,#131852,#131853,#131854,#131855,#131856,#131857,#131858,#131859,
#131860,#131861,#131862,#131863,#131864,#131865,#131866,#131867,#131868,
#131869,#131870,#131871,#131872,#131873,#131874,#131875,#131876,#131877,
#131878,#131879,#131880,#131881,#131882,#131883,#131884,#131885,#131886,
#131887,#131888,#131889,#131890,#131891,#131892,#131893,#131894,#131895,
#131896,#131897,#131898,#131899,#131900,#131901,#131902,#131903,#131904,
#131905,#131906,#131907,#131908,#131909,#131910,#131911,#131912,#131913,
#131914,#131915,#131916,#131917,#131918,#131919,#131920,#131921,#131922,
#131923,#131924,#131925,#131926,#131927,#131928,#131929,#131930,#131931,
#131932,#131933,#131934,#131935,#131936,#131937,#131938,#131939,#131940,
#131941,#131942,#131943,#131944,#131945,#131946,#131947,#131948,#131949,
#131950,#131951,#131952,#131953,#131954,#131955,#131956,#131957,#131958,
#131959,#131960),.UNSPECIFIED.,.F.,.F.,(4,3,3,3,3,3,3,3,3,3,3,3,3,3,3,3,
3,3,3,3,3,3,3,3,3,3,3,3,3,3,3,3,3,3,3,3,3,3,3,3,3,4),(53.4070755243489,
53.5149520672591,53.6231638610545,53.7318758460054,53.8180551329251,53.9166532579288,
54.0151110407055,54.1153336084782,54.2136131662063,54.3118597452796,54.4101028283181,
54.5118000169604,54.6101844303791,54.7135380066331,54.816891582887,54.9154897078907,
55.0139474906675,55.1141700584402,55.2124496161683,55.3106961952417,55.4089392782802,
55.5106364669224,55.6090208803412,55.7123744565951,55.8157280328489,55.9143261578526,
56.0127839406294,56.1130065084021,56.2112860661302,56.3095326452036,56.4077757282421,
56.5094729168843,56.6078573303031,56.7112109065569,56.8145644828108,56.913145227458,
57.0115945031628,57.1099420320524,57.2082227592543,57.3064633876106,57.404720555686,
57.463995963324),.UNSPECIFIED.);
#1286=B_SPLINE_CURVE_WITH_KNOTS('',3,(#131961,#131962,#131963,#131964,#131965,
#131966),.UNSPECIFIED.,.F.,.F.,(4,1,1,4),(51.1819113926155,51.8203822330014,
52.8192186829633,53.4070751110266),.UNSPECIFIED.);
#1287=B_SPLINE_CURVE_WITH_KNOTS('',3,(#131968,#131969,#131970,#131971,#131972,
#131973,#131974),.UNSPECIFIED.,.F.,.F.,(4,1,1,1,4),(51.1803881837399,51.3555755004818,
52.3544119504437,53.3532484004055,53.4070751110266),.UNSPECIFIED.);
#1288=B_SPLINE_CURVE_WITH_KNOTS('',3,(#131975,#131976,#131977,#131978,#131979,
#131980,#131981,#131982,#131983,#131984,#131985,#131986,#131987,#131988,
#131989,#131990,#131991,#131992,#131993,#131994,#131995,#131996,#131997,
#131998,#131999,#132000,#132001,#132002,#132003,#132004,#132005,#132006,
#132007,#132008,#132009,#132010,#132011,#132012,#132013,#132014,#132015,
#132016,#132017,#132018,#132019,#132020,#132021,#132022,#132023,#132024,
#132025,#132026,#132027,#132028,#132029,#132030,#132031,#132032,#132033,
#132034,#132035,#132036,#132037,#132038,#132039,#132040,#132041,#132042,
#132043,#132044,#132045,#132046,#132047,#132048,#132049,#132050,#132051,
#132052,#132053,#132054,#132055,#132056,#132057,#132058,#132059,#132060,
#132061,#132062,#132063,#132064,#132065,#132066,#132067,#132068,#132069,
#132070,#132071,#132072,#132073,#132074,#132075,#132076,#132077,#132078,
#132079,#132080,#132081,#132082,#132083,#132084,#132085,#132086,#132087,
#132088,#132089,#132090,#132091,#132092,#132093,#132094,#132095,#132096,
#132097,#132098,#132099,#132100,#132101),.UNSPECIFIED.,.F.,.F.,(4,3,3,3,
3,3,3,3,3,3,3,3,3,3,3,3,3,3,3,3,3,3,3,3,3,3,3,3,3,3,3,3,3,3,3,3,3,3,3,3,
3,3,4),(53.4070751110266,53.5048543854907,53.6024983707771,53.7000367768844,
53.7975186210124,53.8949743677961,53.9924344477706,54.0899931990357,54.1876041339867,
54.2853815723762,54.3520848503674,54.4506829753711,54.549140758148,54.6493633259206,
54.7476428836488,54.8458894627222,54.9441325457611,55.0458297344031,55.1442141478219,
55.2475677240756,55.3509213003293,55.4495194253329,55.5479772081095,55.6481997758822,
55.7464793336103,55.8447259126838,55.9429689957221,56.0446661843644,56.1430505977832,
56.2464041740372,56.3497577502912,56.4483558752949,56.5468136580716,56.6470362258442,
56.7453157835724,56.8435623626457,56.9418054456843,57.0435026343265,57.1418870477453,
57.2452406239991,57.348594200253,57.4471969426027,57.464911377198),
 .UNSPECIFIED.);
#1289=B_SPLINE_CURVE_WITH_KNOTS('',3,(#132107,#132108,#132109,#132110,#132111,
#132112,#132113,#132114),.UNSPECIFIED.,.F.,.F.,(4,1,1,1,1,4),(59.6902604182062,
59.8110738326964,60.8099102826583,61.8087467326201,62.807583182582,63.7472418106748),
 .UNSPECIFIED.);
#1290=B_SPLINE_CURVE_WITH_KNOTS('',3,(#132115,#132116,#132117,#132118,#132119,
#132120,#132121,#132122,#132123,#132124,#132125,#132126,#132127,#132128,
#132129,#132130,#132131,#132132,#132133,#132134,#132135,#132136,#132137,
#132138,#132139,#132140,#132141,#132142,#132143,#132144,#132145,#132146,
#132147,#132148,#132149,#132150,#132151,#132152,#132153,#132154,#132155,
#132156,#132157,#132158,#132159,#132160,#132161,#132162,#132163,#132164,
#132165,#132166,#132167,#132168,#132169,#132170,#132171,#132172,#132173,
#132174,#132175,#132176,#132177,#132178,#132179,#132180,#132181,#132182,
#132183,#132184),.UNSPECIFIED.,.F.,.F.,(4,3,3,3,3,3,3,3,3,3,3,3,3,3,3,3,
3,3,3,3,3,3,3,4),(57.463995963324,57.5623571570582,57.6607771651584,57.7593619663573,
57.8134009327726,57.9119990577763,58.010456840553,58.1106794083257,58.2089589660538,
58.3072055451272,58.4054486281658,58.507145816808,58.6055302302267,58.7088838064806,
58.8122373827345,58.9094791608007,59.0070768179764,59.1040671063403,59.2009981633324,
59.2979009849175,59.3959908432397,59.4929780422904,59.5916192302483,59.6902604182062),
 .UNSPECIFIED.);
#1291=B_SPLINE_CURVE_WITH_KNOTS('',3,(#132186,#132187,#132188,#132189,#132190,
#132191,#132192,#132193,#132194,#132195,#132196,#132197,#132198,#132199,
#132200,#132201,#132202,#132203,#132204,#132205,#132206,#132207,#132208,
#132209,#132210,#132211,#132212,#132213,#132214,#132215,#132216,#132217,
#132218,#132219,#132220,#132221,#132222,#132223,#132224,#132225,#132226,
#132227,#132228,#132229,#132230,#132231,#132232,#132233,#132234,#132235,
#132236,#132237,#132238,#132239,#132240,#132241,#132242,#132243,#132244,
#132245,#132246,#132247,#132248,#132249,#132250,#132251,#132252),
 .UNSPECIFIED.,.F.,.F.,(4,3,3,3,3,3,3,3,3,3,3,3,3,3,3,3,3,3,3,3,3,3,4),
(57.464911377198,57.5633474036735,57.6616774189312,57.7599496840526,57.8581937126486,
57.956438983539,58.0547832757564,58.1531751763202,58.2517448625486,58.3474306502149,
58.4460287752185,58.5444865579953,58.644709125768,58.7429886834961,58.8412352625696,
58.9394783456082,59.0411755342503,59.1395599476692,59.242913523923,59.3462671001768,
59.460882914029,59.5755716660042,59.6902604179793),.UNSPECIFIED.);
#1292=B_SPLINE_CURVE_WITH_KNOTS('',3,(#132253,#132254,#132255,#132256,#132257,
#132258,#132259,#132260,#132261,#132262,#132263,#132264,#132265,#132266,
#132267,#132268,#132269,#132270,#132271,#132272,#132273,#132274,#132275,
#132276,#132277,#132278,#132279,#132280,#132281,#132282,#132283,#132284,
#132285,#132286,#132287,#132288,#132289,#132290,#132291,#132292,#132293,
#132294,#132295,#132296,#132297,#132298,#132299,#132300,#132301,#132302,
#132303,#132304,#132305,#132306,#132307,#132308,#132309,#132310,#132311,
#132312,#132313,#132314,#132315,#132316,#132317,#132318,#132319,#132320,
#132321,#132322,#132323,#132324,#132325,#132326,#132327,#132328,#132329,
#132330,#132331,#132332,#132333,#132334,#132335,#132336,#132337,#132338,
#132339,#132340,#132341,#132342,#132343,#132344,#132345,#132346,#132347,
#132348,#132349,#132350,#132351,#132352,#132353,#132354,#132355,#132356,
#132357,#132358,#132359,#132360,#132361,#132362,#132363,#132364,#132365,
#132366,#132367,#132368,#132369,#132370,#132371,#132372,#132373,#132374,
#132375,#132376),.UNSPECIFIED.,.F.,.F.,(4,3,3,3,3,3,3,3,3,3,3,3,3,3,3,3,
3,3,3,3,3,3,3,3,3,3,3,3,3,3,3,3,3,3,3,3,3,3,3,3,3,4),(59.6902604182062,
59.788634173056,59.8869985815969,59.985382791999,60.0838846667639,60.1824499292132,
60.2811933482969,60.3451035501387,60.4437016751424,60.542159457919,60.6423820256917,
60.7406615834199,60.8389081624933,60.9371512455318,61.0388484341739,61.1372328475928,
61.2405864238466,61.3439400001005,61.4425381251042,61.5409959078811,61.6412184756537,
61.7394980333819,61.8377446124552,61.9359876954937,62.0376848841359,62.1360692975546,
62.2394228738085,62.3427764500624,62.4413745750661,62.5398323578432,62.6400549256158,
62.738334483344,62.8365810624174,62.9348241454559,63.036521334098,63.1349057475167,
63.2382593237705,63.3416129000243,63.4431811229531,63.5416227638002,63.6447542777698,
63.7478857917395),.UNSPECIFIED.);
#1293=B_SPLINE_CURVE_WITH_KNOTS('',3,(#132382,#132383,#132384,#132385,#132386,
#132387,#132388,#132389,#132390,#132391,#132392,#132393,#132394,#132395,
#132396,#132397,#132398,#132399,#132400,#132401,#132402,#132403,#132404,
#132405,#132406,#132407,#132408,#132409,#132410,#132411,#132412,#132413,
#132414,#132415,#132416,#132417,#132418,#132419,#132420,#132421,#132422,
#132423,#132424,#132425,#132426,#132427,#132428,#132429,#132430,#132431,
#132432,#132433,#132434,#132435,#132436,#132437,#132438,#132439,#132440,
#132441,#132442,#132443,#132444,#132445,#132446,#132447,#132448,#132449,
#132450,#132451,#132452,#132453,#132454,#132455,#132456,#132457,#132458,
#132459,#132460,#132461,#132462,#132463,#132464,#132465,#132466,#132467,
#132468,#132469,#132470,#132471,#132472,#132473,#132474,#132475,#132476,
#132477,#132478,#132479,#132480,#132481,#132482,#132483,#132484,#132485,
#132486,#132487,#132488,#132489,#132490,#132491,#132492,#132493,#132494,
#132495,#132496,#132497,#132498,#132499,#132500,#132501,#132502,#132503,
#132504,#132505,#132506,#132507,#132508),.UNSPECIFIED.,.F.,.F.,(4,3,3,3,
3,3,3,3,3,3,3,3,3,3,3,3,3,3,3,3,3,3,3,3,3,3,3,3,3,3,3,3,3,3,3,3,3,3,3,3,
3,3,4),(65.9734457253857,66.0704340596178,66.1673127975359,66.2641328887561,
66.3609254267911,66.4577214670339,66.5546134226803,66.6515579893417,66.7486626585401,
66.8029289824295,66.9015271074332,66.99998489021,67.1002074579826,67.1984870157107,
67.2967335947841,67.3949766778227,67.4966738664648,67.5950582798837,67.6984118561375,
67.8017654323914,67.9003635573952,67.9988213401717,68.0990439079444,68.1973234656725,
68.2955700447459,68.3938131277845,68.4955103164266,68.5938947298455,68.6972483060993,
68.8006018823532,68.8992000073569,68.9976577901335,69.0978803579062,69.1961599156345,
69.2944064947079,69.3926495777463,69.4943467663885,69.5927311798073,69.6960847560612,
69.7994383323151,69.8980412657762,69.996491840234,70.0313849422026),
 .UNSPECIFIED.);
#1294=B_SPLINE_CURVE_WITH_KNOTS('',3,(#132509,#132510,#132511,#132512,#132513,
#132514,#132515),.UNSPECIFIED.,.F.,.F.,(4,1,1,1,4),(63.7472418106748,63.8064196325439,
64.8052560825058,65.8040925324676,65.9734457253857),.UNSPECIFIED.);
#1295=B_SPLINE_CURVE_WITH_KNOTS('',3,(#132517,#132518,#132519,#132520,#132521,
#132522,#132523,#132524,#132525,#132526,#132527,#132528,#132529,#132530,
#132531,#132532,#132533,#132534,#132535,#132536,#132537,#132538,#132539,
#132540,#132541,#132542,#132543,#132544,#132545,#132546,#132547,#132548,
#132549,#132550,#132551,#132552,#132553,#132554,#132555,#132556,#132557,
#132558,#132559,#132560,#132561,#132562,#132563,#132564,#132565,#132566,
#132567,#132568,#132569,#132570,#132571,#132572,#132573,#132574,#132575,
#132576,#132577,#132578,#132579,#132580,#132581,#132582,#132583,#132584,
#132585,#132586),.UNSPECIFIED.,.F.,.F.,(4,3,3,3,3,3,3,3,3,3,3,3,3,3,3,3,
3,3,3,3,3,3,3,4),(63.7478857917395,63.8461305577829,63.9443750416371,64.0433936187244,
64.1417828184941,64.2411160842401,64.3404493499862,64.43904747499,64.5375052577667,
64.6377278255393,64.7360073832675,64.8342539623408,64.9324970453792,65.0341942340214,
65.1325786474403,65.2359322236941,65.339285799948,65.4384637976082,65.5374980774499,
65.6364173808601,65.7352455972602,65.8340208922134,65.9327849002204,65.9734457253857),
 .UNSPECIFIED.);
#1296=B_SPLINE_CURVE_WITH_KNOTS('',3,(#132587,#132588,#132589,#132590,#132591,
#132592,#132593,#132594,#132595,#132596,#132597,#132598,#132599,#132600,
#132601,#132602,#132603,#132604,#132605,#132606,#132607,#132608,#132609,
#132610,#132611,#132612,#132613,#132614,#132615,#132616,#132617,#132618,
#132619,#132620,#132621,#132622,#132623,#132624,#132625,#132626,#132627,
#132628,#132629,#132630,#132631,#132632,#132633,#132634,#132635,#132636,
#132637,#132638,#132639,#132640,#132641,#132642,#132643,#132644,#132645,
#132646,#132647,#132648,#132649,#132650,#132651,#132652,#132653,#132654,
#132655,#132656,#132657,#132658,#132659,#132660,#132661,#132662,#132663,
#132664,#132665,#132666,#132667,#132668,#132669,#132670,#132671,#132672,
#132673,#132674,#132675,#132676,#132677,#132678,#132679,#132680,#132681,
#132682,#132683,#132684,#132685,#132686,#132687,#132688,#132689,#132690,
#132691,#132692,#132693,#132694,#132695,#132696,#132697,#132698,#132699,
#132700,#132701,#132702,#132703,#132704,#132705,#132706,#132707,#132708,
#132709,#132710),.UNSPECIFIED.,.F.,.F.,(4,3,3,3,3,3,3,3,3,3,3,3,3,3,3,3,
3,3,3,3,3,3,3,3,3,3,3,3,3,3,3,3,3,3,3,3,3,3,3,3,3,4),(65.9734457256204,
66.0848798050745,66.1968635637055,66.3094957826849,66.3381222499099,66.4367203749136,
66.5351781576904,66.635400725463,66.7336802831912,66.8319268622646,66.9301699453032,
67.0318671339454,67.1302515473642,67.233605123618,67.3369586998718,67.4355568248755,
67.5340146076523,67.634237175425,67.7325167331531,67.8307633122265,67.929006395265,
68.0307035839072,68.129087997326,68.2324415735798,68.3357951498337,68.4343932748374,
68.5328510576141,68.6330736253868,68.7313531831149,68.8295997621883,68.9278428452268,
69.029540033869,69.1279244472878,69.2312780235416,69.3346315997955,69.4332079436479,
69.5316540255028,69.6299995615628,69.7300683995431,69.8283147700062,69.929294841745,
70.0302749134839),.UNSPECIFIED.);
#1297=B_SPLINE_CURVE_WITH_KNOTS('',3,(#132716,#132717,#132718,#132719,#132720,
#132721,#132722,#132723),.UNSPECIFIED.,.F.,.F.,(4,1,1,1,1,4),(72.2566310325654,
72.7959476822007,73.7947841321626,74.7936205821245,75.7924570320864,76.3138574458811),
 .UNSPECIFIED.);
#1298=B_SPLINE_CURVE_WITH_KNOTS('',3,(#132724,#132725,#132726,#132727,#132728,
#132729,#132730,#132731,#132732,#132733,#132734,#132735,#132736,#132737,
#132738,#132739,#132740,#132741,#132742,#132743,#132744,#132745,#132746,
#132747,#132748,#132749,#132750,#132751,#132752,#132753,#132754,#132755,
#132756,#132757,#132758,#132759,#132760,#132761,#132762,#132763,#132764,
#132765,#132766,#132767,#132768,#132769,#132770,#132771,#132772,#132773,
#132774,#132775,#132776,#132777,#132778,#132779,#132780,#132781,#132782,
#132783,#132784,#132785,#132786,#132787,#132788,#132789,#132790,#132791,
#132792,#132793),.UNSPECIFIED.,.F.,.F.,(4,3,3,3,3,3,3,3,3,3,3,3,3,3,3,3,
3,3,3,3,3,3,3,4),(70.0313849422026,70.1297027318843,70.2279679340465,70.3262100542967,
70.4244585681002,70.5228092667787,70.6212122014149,70.7197874226758,70.798274782277,
70.8968729072807,70.9953306900576,71.0955532578302,71.1938328155585,71.2920793946319,
71.3903224776702,71.4920196663123,71.5904040797312,71.693757655985,71.7971112322389,
71.9028340905518,72.0081993817381,72.1133399321502,72.2181701837247,72.2566308185864),
 .UNSPECIFIED.);
#1299=B_SPLINE_CURVE_WITH_KNOTS('',3,(#132795,#132796,#132797,#132798,#132799,
#132800,#132801,#132802,#132803,#132804,#132805,#132806,#132807,#132808,
#132809,#132810,#132811,#132812,#132813,#132814,#132815,#132816,#132817,
#132818,#132819,#132820,#132821,#132822,#132823,#132824,#132825,#132826,
#132827,#132828,#132829,#132830,#132831,#132832,#132833,#132834,#132835,
#132836,#132837,#132838,#132839,#132840,#132841,#132842,#132843,#132844,
#132845,#132846,#132847,#132848,#132849,#132850,#132851,#132852,#132853,
#132854,#132855,#132856,#132857,#132858,#132859,#132860,#132861,#132862,
#132863,#132864),.UNSPECIFIED.,.F.,.F.,(4,3,3,3,3,3,3,3,3,3,3,3,3,3,3,3,
3,3,3,3,3,3,3,4),(70.0302749134839,70.1286604417134,70.2310642457354,70.3334680497574,
70.4320661747611,70.5305239575379,70.6307465253105,70.7290260830387,70.8272726621121,
70.9255157451505,71.0272129337927,71.1255973472116,71.2289509234654,71.3323044997193,
71.4298807240689,71.5273176349422,71.6246428433671,71.7219081150621,71.8191441424517,
71.9163815796696,72.0137087835221,72.1110862397607,72.2086145464313,72.2566310325654),
 .UNSPECIFIED.);
#1300=B_SPLINE_CURVE_WITH_KNOTS('',3,(#132865,#132866,#132867,#132868,#132869,
#132870,#132871,#132872),.UNSPECIFIED.,.F.,.F.,(4,1,1,1,1,4),(72.2566310325654,
72.3311409496812,73.329977399643,74.3288138496049,75.3276502995668,76.3138964032405),
 .UNSPECIFIED.);
#1301=B_SPLINE_CURVE_WITH_KNOTS('',3,(#132878,#132879,#132880,#132881,#132882,
#132883,#132884,#132885,#132886,#132887,#132888,#132889,#132890,#132891,
#132892,#132893,#132894,#132895,#132896,#132897,#132898,#132899,#132900,
#132901,#132902,#132903,#132904,#132905,#132906,#132907,#132908,#132909,
#132910,#132911,#132912,#132913,#132914,#132915,#132916,#132917,#132918,
#132919,#132920,#132921,#132922,#132923,#132924,#132925,#132926,#132927,
#132928,#132929,#132930,#132931,#132932,#132933,#132934,#132935,#132936,
#132937,#132938,#132939,#132940,#132941,#132942,#132943,#132944,#132945,
#132946,#132947,#132948,#132949,#132950,#132951,#132952,#132953,#132954,
#132955,#132956,#132957,#132958,#132959,#132960,#132961,#132962,#132963,
#132964,#132965,#132966,#132967,#132968,#132969,#132970,#132971,#132972,
#132973,#132974,#132975,#132976,#132977,#132978,#132979,#132980,#132981,
#132982,#132983,#132984,#132985,#132986,#132987,#132988,#132989,#132990,
#132991,#132992,#132993,#132994,#132995,#132996,#132997,#132998,#132999,
#133000,#133001),.UNSPECIFIED.,.F.,.F.,(4,3,3,3,3,3,3,3,3,3,3,3,3,3,3,3,
3,3,3,3,3,3,3,3,3,3,3,3,3,3,3,3,3,3,3,3,3,3,3,3,3,4),(78.5398164397795,
78.6677108218205,78.788966381972,78.8875645069757,78.9860222897525,79.0862448575251,
79.1845244152533,79.2827709943266,79.381014077365,79.4827112660072,79.581095679426,
79.68444925568,79.7878028319339,79.8864009569376,79.9848587397144,80.0850813074871,
80.1833608652152,80.2816074442886,80.379850527327,80.4815477159692,80.579932129388,
80.6832857056419,80.7866392818957,80.8852374068994,80.9836951896762,81.0839177574489,
81.182197315177,81.2804438942504,81.3786869772889,81.480384165931,81.5787685793498,
81.6821221556037,81.7854757318576,81.8868624824842,81.9852993415052,82.0836395026602,
82.1819125647065,82.2801480543488,82.3784063402449,82.4766798066968,82.5750348018018,
82.5965697368708),.UNSPECIFIED.);
#1302=B_SPLINE_CURVE_WITH_KNOTS('',3,(#133002,#133003,#133004,#133005,#133006,
#133007),.UNSPECIFIED.,.F.,.F.,(4,1,1,4),(76.3138574458811,76.7912934820482,
77.7901299320101,78.539816339745),.UNSPECIFIED.);
#1303=B_SPLINE_CURVE_WITH_KNOTS('',3,(#133009,#133010,#133011,#133012,#133013,
#133014,#133015),.UNSPECIFIED.,.F.,.F.,(4,1,1,1,4),(76.3138964032405,76.3264867495287,
77.3253231994905,78.3241596494524,78.539816339745),.UNSPECIFIED.);
#1304=B_SPLINE_CURVE_WITH_KNOTS('',3,(#133016,#133017,#133018,#133019,#133020,
#133021,#133022,#133023,#133024,#133025,#133026,#133027,#133028,#133029,
#133030,#133031,#133032,#133033,#133034,#133035,#133036,#133037,#133038,
#133039,#133040,#133041,#133042,#133043,#133044,#133045,#133046,#133047,
#133048,#133049,#133050,#133051,#133052,#133053,#133054,#133055,#133056,
#133057,#133058,#133059,#133060,#133061,#133062,#133063,#133064,#133065,
#133066,#133067,#133068,#133069,#133070,#133071,#133072,#133073,#133074,
#133075,#133076,#133077,#133078,#133079,#133080,#133081,#133082,#133083,
#133084,#133085,#133086,#133087,#133088,#133089,#133090,#133091,#133092,
#133093,#133094,#133095,#133096,#133097,#133098,#133099,#133100,#133101,
#133102,#133103,#133104,#133105,#133106,#133107,#133108,#133109,#133110,
#133111,#133112,#133113,#133114,#133115,#133116,#133117,#133118,#133119,
#133120,#133121,#133122,#133123,#133124,#133125,#133126,#133127,#133128,
#133129,#133130,#133131,#133132,#133133,#133134,#133135,#133136,#133137,
#133138,#133139),.UNSPECIFIED.,.F.,.F.,(4,3,3,3,3,3,3,3,3,3,3,3,3,3,3,3,
3,3,3,3,3,3,3,3,3,3,3,3,3,3,3,3,3,3,3,3,3,3,3,3,3,4),(78.539816339745,78.6377138097037,
78.7346673304385,78.8315786913981,78.9284788661295,79.0271081744507,79.124135318513,
79.2235657089636,79.3229960994143,79.421594224418,79.5200520071948,79.6202745749675,
79.7185541326956,79.816800711769,79.9150437948074,80.0167409834496,80.1151253968684,
80.2184789731223,80.3218325493762,80.4204306743799,80.5188884571566,80.6191110249293,
80.7173905826575,80.8156371617309,80.9138802447692,81.0155774334114,81.1139618468302,
81.2173154230841,81.320668999338,81.4192671243417,81.5177249071183,81.617947474891,
81.7162270326191,81.8144736116923,81.9127166947308,82.0144138833731,82.1127982967919,
82.2161518730459,82.3195054492999,82.4180964129972,82.5165362141383,82.5977152782637),
 .UNSPECIFIED.);
#1305=B_SPLINE_CURVE_WITH_KNOTS('',3,(#133145,#133146,#133147,#133148,#133149,
#133150,#133151,#133152),.UNSPECIFIED.,.F.,.F.,(4,1,1,1,1,4),(84.8230070322059,
85.7808215317051,86.779657981667,87.7784944316288,88.7773308815907,88.8809435586522),
 .UNSPECIFIED.);
#1306=B_SPLINE_CURVE_WITH_KNOTS('',3,(#133153,#133154,#133155,#133156,#133157,
#133158,#133159,#133160,#133161,#133162,#133163,#133164,#133165,#133166,
#133167,#133168,#133169,#133170,#133171,#133172,#133173,#133174,#133175,
#133176,#133177,#133178,#133179,#133180,#133181,#133182,#133183,#133184,
#133185,#133186,#133187,#133188,#133189,#133190,#133191,#133192,#133193,
#133194,#133195,#133196,#133197,#133198,#133199,#133200,#133201,#133202,
#133203,#133204,#133205,#133206,#133207,#133208,#133209,#133210,#133211,
#133212,#133213,#133214,#133215,#133216,#133217,#133218,#133219,#133220,
#133221,#133222),.UNSPECIFIED.,.F.,.F.,(4,3,3,3,3,3,3,3,3,3,3,3,3,3,3,3,
3,3,3,3,3,3,3,4),(82.5965697368708,82.6951414027961,82.7843121818195,82.8829103068232,
82.9813680896,83.0815906573726,83.1798702151008,83.2781167941742,83.3763598772127,
83.4780570658548,83.5764414792737,83.6797950555275,83.7831486317814,83.8817467567851,
83.9802045395619,84.0804271073345,84.1787066650626,84.276953244136,84.3751963271744,
84.4768935158166,84.5752779292354,84.6786315054893,84.7819850817432,84.8230016469246),
 .UNSPECIFIED.);
#1307=B_SPLINE_CURVE_WITH_KNOTS('',3,(#133224,#133225,#133226,#133227,#133228,
#133229,#133230,#133231,#133232,#133233,#133234,#133235,#133236,#133237,
#133238,#133239,#133240,#133241,#133242,#133243,#133244,#133245,#133246,
#133247,#133248,#133249,#133250,#133251,#133252,#133253,#133254,#133255,
#133256,#133257,#133258,#133259,#133260,#133261,#133262,#133263,#133264,
#133265,#133266,#133267,#133268,#133269,#133270,#133271,#133272,#133273,
#133274,#133275,#133276,#133277,#133278,#133279,#133280,#133281,#133282,
#133283,#133284,#133285,#133286,#133287,#133288,#133289,#133290,#133291,
#133292,#133293),.UNSPECIFIED.,.F.,.F.,(4,3,3,3,3,3,3,3,3,3,3,3,3,3,3,3,
3,3,3,3,3,3,3,4),(82.5977152782637,82.6960046491985,82.7942553193272,82.8924967767674,
82.9907584919828,83.0891304482576,83.1875671008218,83.2861621677909,83.3183418992618,
83.4169400242655,83.5153978070424,83.6156203748151,83.7138999325432,83.8121465116165,
83.9103895946546,84.0120867832969,84.1104711967158,84.2138247729697,84.3171783492237,
84.4205578302507,84.5236543867489,84.6265834813182,84.7292989065995,84.8230016469246),
 .UNSPECIFIED.);
#1308=B_SPLINE_CURVE_WITH_KNOTS('',3,(#133294,#133295,#133296,#133297,#133298,
#133299,#133300,#133301,#133302,#133303,#133304,#133305,#133306,#133307,
#133308,#133309,#133310,#133311,#133312,#133313,#133314,#133315,#133316,
#133317,#133318,#133319,#133320,#133321,#133322,#133323,#133324,#133325,
#133326,#133327,#133328,#133329,#133330,#133331,#133332,#133333,#133334,
#133335,#133336,#133337,#133338,#133339,#133340,#133341,#133342,#133343,
#133344,#133345,#133346,#133347,#133348,#133349,#133350,#133351,#133352,
#133353,#133354,#133355,#133356,#133357,#133358,#133359,#133360,#133361,
#133362,#133363,#133364,#133365,#133366,#133367,#133368,#133369,#133370,
#133371,#133372,#133373,#133374,#133375,#133376,#133377,#133378,#133379,
#133380,#133381,#133382,#133383,#133384,#133385,#133386,#133387,#133388,
#133389,#133390,#133391,#133392,#133393,#133394,#133395,#133396,#133397,
#133398,#133399,#133400,#133401,#133402,#133403,#133404,#133405,#133406,
#133407,#133408,#133409,#133410,#133411,#133412,#133413,#133414,#133415,
#133416,#133417),.UNSPECIFIED.,.F.,.F.,(4,3,3,3,3,3,3,3,3,3,3,3,3,3,3,3,
3,3,3,3,3,3,3,3,3,3,3,3,3,3,3,3,3,3,3,3,3,3,3,3,3,4),(84.8230016472006,
84.9261861619504,85.0296647966981,85.1332945907093,85.2372126194225,85.3160147991855,
85.4146129241892,85.513070706966,85.6132932747387,85.7115728324668,85.8098194115402,
85.9080624945788,86.009759683221,86.1081440966398,86.2114976728936,86.3148512491474,
86.4134493741511,86.5119071569279,86.6121297247005,86.7104092824287,86.8086558615021,
86.9068989445406,87.0085961331828,87.1069805466016,87.2103341228555,87.3136876991093,
87.412285824113,87.5107436068897,87.6109661746624,87.7092457323906,87.8074923114639,
87.9057353945024,88.0074325831446,88.1058169965634,88.2091705728173,88.3125241490712,
88.411113786503,88.5095698168581,88.6079122101868,88.7061871882877,88.8044419893942,
88.8801389537999),.UNSPECIFIED.);
#1309=B_SPLINE_CURVE_WITH_KNOTS('',3,(#133423,#133424,#133425,#133426,#133427,
#133428,#133429,#133430,#133431,#133432,#133433,#133434,#133435,#133436,
#133437,#133438,#133439,#133440,#133441,#133442,#133443,#133444,#133445,
#133446,#133447,#133448,#133449,#133450,#133451,#133452,#133453,#133454,
#133455,#133456,#133457,#133458,#133459,#133460,#133461,#133462,#133463,
#133464,#133465,#133466,#133467,#133468,#133469,#133470,#133471,#133472,
#133473,#133474,#133475,#133476,#133477,#133478,#133479,#133480,#133481,
#133482,#133483,#133484,#133485,#133486,#133487,#133488,#133489,#133490,
#133491,#133492,#133493,#133494,#133495,#133496,#133497,#133498,#133499,
#133500,#133501,#133502,#133503,#133504,#133505,#133506,#133507,#133508,
#133509,#133510,#133511,#133512,#133513,#133514,#133515,#133516,#133517,
#133518,#133519,#133520,#133521,#133522,#133523,#133524,#133525,#133526,
#133527,#133528,#133529,#133530,#133531,#133532,#133533,#133534,#133535,
#133536,#133537,#133538,#133539,#133540,#133541,#133542,#133543,#133544,
#133545,#133546),.UNSPECIFIED.,.F.,.F.,(4,3,3,3,3,3,3,3,3,3,3,3,3,3,3,3,
3,3,3,3,3,3,3,3,3,3,3,3,3,3,3,3,3,3,3,3,3,3,3,3,3,4),(91.1061869541041,
91.2043419644769,91.3024795334305,91.4006291648839,91.4988897541855,91.5972075103077,
91.6957053368612,91.7738402314764,91.8724383564801,91.9708961392567,92.0711187070294,
92.1693982647575,92.2676448438309,92.3658879268695,92.4675851155117,92.5659695289305,
92.6693231051843,92.7726766814382,92.8712748064418,92.9697325892184,93.0699551569911,
93.1682347147193,93.2664812937927,93.364724376831,93.4664215654733,93.564805978892,
93.668159555146,93.7715131314001,93.8701112564038,93.9685690391806,94.0687916069532,
94.1670711646813,94.2653177437548,94.3635608267933,94.4652580154355,94.5636424288542,
94.6669960051081,94.770349581362,94.8689185475044,94.9673651080001,95.0657083030471,
95.1638473408373),.UNSPECIFIED.);
#1310=B_SPLINE_CURVE_WITH_KNOTS('',3,(#133547,#133548,#133549,#133550,#133551,
#133552),.UNSPECIFIED.,.F.,.F.,(4,1,1,4),(88.8809435586522,89.7761673315526,
90.7750037815145,91.1061798195662),.UNSPECIFIED.);
#1311=B_SPLINE_CURVE_WITH_KNOTS('',3,(#133554,#133555,#133556,#133557,#133558,
#133559,#133560,#133561,#133562,#133563,#133564,#133565,#133566,#133567,
#133568,#133569,#133570,#133571,#133572,#133573,#133574,#133575,#133576,
#133577,#133578,#133579,#133580,#133581,#133582,#133583,#133584,#133585,
#133586,#133587,#133588,#133589,#133590,#133591,#133592,#133593,#133594,
#133595,#133596,#133597,#133598,#133599,#133600,#133601,#133602,#133603,
#133604,#133605,#133606,#133607,#133608,#133609,#133610,#133611,#133612,
#133613,#133614,#133615,#133616,#133617,#133618,#133619,#133620,#133621,
#133622,#133623,#133624,#133625,#133626),.UNSPECIFIED.,.F.,.F.,(4,3,3,3,
3,3,3,3,3,3,3,3,3,3,3,3,3,3,3,3,3,3,3,3,4),(88.8801389537999,88.9783987981197,
89.076767980697,89.1752004097067,89.2737927972633,89.311360599033,89.4099587240367,
89.5084165068134,89.6086390745861,89.7069186323142,89.8051652113876,89.9034082944261,
90.0051054830683,90.1034898964871,90.206843472741,90.3101970489949,90.409695787095,
90.5067185530535,90.6036495481492,90.70051989818,90.801936662084,90.8988156754799,
90.9957205549589,91.0927209416414,91.1061869537961),.UNSPECIFIED.);
#1312=B_SPLINE_CURVE_WITH_KNOTS('',3,(#133627,#133628,#133629,#133630,#133631,
#133632,#133633,#133634,#133635,#133636,#133637,#133638,#133639,#133640,
#133641,#133642,#133643,#133644,#133645,#133646,#133647,#133648,#133649,
#133650,#133651,#133652,#133653,#133654,#133655,#133656,#133657,#133658,
#133659,#133660,#133661,#133662,#133663,#133664,#133665,#133666,#133667,
#133668,#133669,#133670,#133671,#133672,#133673,#133674,#133675,#133676,
#133677,#133678,#133679,#133680,#133681,#133682,#133683,#133684,#133685,
#133686,#133687,#133688,#133689,#133690,#133691,#133692,#133693,#133694,
#133695,#133696,#133697,#133698,#133699,#133700,#133701,#133702,#133703,
#133704,#133705,#133706,#133707,#133708,#133709,#133710,#133711,#133712,
#133713,#133714,#133715,#133716,#133717,#133718,#133719,#133720,#133721,
#133722,#133723,#133724,#133725,#133726,#133727,#133728,#133729,#133730,
#133731,#133732,#133733,#133734,#133735,#133736,#133737,#133738,#133739,
#133740,#133741,#133742,#133743,#133744,#133745,#133746,#133747,#133748,
#133749,#133750),.UNSPECIFIED.,.F.,.F.,(4,3,3,3,3,3,3,3,3,3,3,3,3,3,3,3,
3,3,3,3,3,3,3,3,3,3,3,3,3,3,3,3,3,3,3,3,3,3,3,3,3,4),(91.1061869541041,
91.2465035596787,91.3090334989568,91.4076316239605,91.5060894067373,91.60631197451,
91.7045915322382,91.8028381113116,91.9010811943501,92.0027783829923,92.1011627964111,
92.2045163726649,92.3078699489186,92.4064680739223,92.5049258566991,92.6051484244717,
92.7034279821999,92.8016745612733,92.8999176443118,93.001614832954,93.0999992463728,
93.2033528226266,93.3067063988805,93.4053045238842,93.5037623066609,93.6039848744336,
93.7022644321618,93.8005110112352,93.8987540942737,94.0004512829158,94.0988356963346,
94.2021892725885,94.3055428488424,94.4041508037239,94.5025891903039,94.6009312472713,
94.6992065724891,94.7974446925389,94.8957159603349,94.9940021459913,95.0923959721904,
95.1629909577287),.UNSPECIFIED.);
#1313=B_SPLINE_CURVE_WITH_KNOTS('',3,(#133756,#133757,#133758,#133759,#133760,
#133761,#133762,#133763),.UNSPECIFIED.,.F.,.F.,(4,1,1,1,1,4),(97.3893797691262,
97.7668589312476,98.7656953812095,99.7645318311714,100.763368281133,101.445901991804),
 .UNSPECIFIED.);
#1314=B_SPLINE_CURVE_WITH_KNOTS('',3,(#133764,#133765,#133766,#133767,#133768,
#133769,#133770,#133771,#133772,#133773,#133774,#133775,#133776,#133777,
#133778,#133779,#133780,#133781,#133782,#133783,#133784,#133785,#133786,
#133787,#133788,#133789,#133790,#133791,#133792,#133793,#133794,#133795,
#133796,#133797,#133798,#133799,#133800,#133801,#133802,#133803,#133804,
#133805,#133806,#133807,#133808,#133809,#133810,#133811,#133812,#133813,
#133814,#133815,#133816,#133817,#133818,#133819,#133820,#133821,#133822,
#133823,#133824,#133825,#133826,#133827,#133828,#133829,#133830,#133831,
#133832,#133833,#133834,#133835,#133836),.UNSPECIFIED.,.F.,.F.,(4,3,3,3,
3,3,3,3,3,3,3,3,3,3,3,3,3,3,3,3,3,3,3,3,4),(95.1638473408373,95.2620943086999,
95.3603371625601,95.4625493797511,95.5609328931331,95.6593867503051,95.7579931826896,
95.7691860313238,95.8677841563276,95.9662419391048,96.0664645068774,96.1647440646056,
96.262990643679,96.3612337267177,96.4629309153597,96.5613153287784,96.664668905032,
96.7680224812857,96.8674993725788,96.9668292609828,97.0660403563902,97.1651524247997,
97.2642075332236,97.3632407686268,97.3893722612837),.UNSPECIFIED.);
#1315=B_SPLINE_CURVE_WITH_KNOTS('',3,(#133838,#133839,#133840,#133841,#133842,
#133843,#133844,#133845,#133846,#133847,#133848,#133849,#133850,#133851,
#133852,#133853,#133854,#133855,#133856,#133857,#133858,#133859,#133860,
#133861,#133862,#133863,#133864,#133865,#133866,#133867,#133868,#133869,
#133870,#133871,#133872,#133873,#133874,#133875,#133876,#133877,#133878,
#133879,#133880,#133881,#133882,#133883,#133884,#133885,#133886,#133887,
#133888,#133889,#133890,#133891,#133892,#133893,#133894,#133895,#133896,
#133897,#133898,#133899,#133900,#133901,#133902,#133903,#133904,#133905,
#133906,#133907),.UNSPECIFIED.,.F.,.F.,(4,3,3,3,3,3,3,3,3,3,3,3,3,3,3,3,
3,3,3,3,3,3,3,4),(95.1629909577287,95.2615808373963,95.3043792988043,95.402977423808,
95.5014352065847,95.6016577743574,95.6999373320855,95.7981839111589,95.8964269941974,
95.9981241828395,96.0965085962583,96.1998621725122,96.3032157487661,96.4018138737698,
96.5002716565466,96.6004942243192,96.6987737820474,96.7970203611207,96.8952634441592,
96.9969606328014,97.0953450462201,97.1986986224741,97.302052198728,97.3893722612837),
 .UNSPECIFIED.);
#1316=B_SPLINE_CURVE_WITH_KNOTS('',3,(#133908,#133909,#133910,#133911,#133912,
#133913,#133914,#133915),.UNSPECIFIED.,.F.,.F.,(4,1,1,1,1,4),(97.3893809711856,
98.3008886486899,99.2997250986518,100.298561548614,101.297397998576,101.447496653669),
 .UNSPECIFIED.);
#1317=B_SPLINE_CURVE_WITH_KNOTS('',3,(#133921,#133922,#133923,#133924,#133925,
#133926,#133927,#133928,#133929,#133930,#133931,#133932,#133933,#133934,
#133935,#133936,#133937,#133938,#133939,#133940,#133941,#133942,#133943,
#133944,#133945,#133946,#133947,#133948,#133949,#133950,#133951,#133952,
#133953,#133954,#133955,#133956,#133957,#133958,#133959,#133960,#133961,
#133962,#133963,#133964,#133965,#133966,#133967,#133968,#133969,#133970,
#133971,#133972,#133973,#133974,#133975,#133976,#133977,#133978,#133979,
#133980,#133981,#133982,#133983,#133984,#133985,#133986,#133987,#133988,
#133989,#133990,#133991,#133992,#133993,#133994,#133995,#133996,#133997,
#133998,#133999,#134000,#134001,#134002,#134003,#134004,#134005,#134006,
#134007,#134008,#134009,#134010,#134011,#134012,#134013,#134014,#134015,
#134016,#134017,#134018,#134019,#134020,#134021,#134022,#134023,#134024,
#134025,#134026,#134027,#134028,#134029,#134030,#134031,#134032,#134033,
#134034,#134035,#134036,#134037,#134038,#134039,#134040,#134041,#134042,
#134043,#134044),.UNSPECIFIED.,.F.,.F.,(4,3,3,3,3,3,3,3,3,3,3,3,3,3,3,3,
3,3,3,3,3,3,3,3,3,3,3,3,3,3,3,3,3,3,3,3,3,3,3,3,3,4),(103.672557568463,
103.759877631019,103.858475756023,103.956933538799,104.057156106572,104.1554356643,
104.253682243374,104.351925326412,104.453622515054,104.552006928473,104.655360504727,
104.758714080981,104.857312205985,104.955769988761,105.055992556534,105.154272114262,
105.252518693335,105.350761776374,105.452458965016,105.550843378435,105.654196954689,
105.757550530943,105.856148655947,105.954606438723,106.054829006496,106.153108564224,
106.251355143297,106.349598226336,106.451295414978,106.549679828397,106.65303340465,
106.756386980904,106.854986798947,106.953445809627,107.05178876834,107.150068003063,
107.248313037022,107.346553353054,107.444881222501,107.543251670454,107.641785788162,
107.72975655935),.UNSPECIFIED.);
#1318=B_SPLINE_CURVE_WITH_KNOTS('',3,(#134045,#134046,#134047,#134048,#134049,
#134050),.UNSPECIFIED.,.F.,.F.,(4,1,1,4),(101.445901991804,101.762204731095,
102.761041181057,103.67254885852),.UNSPECIFIED.);
#1319=B_SPLINE_CURVE_WITH_KNOTS('',3,(#134052,#134053,#134054,#134055,#134056,
#134057),.UNSPECIFIED.,.F.,.F.,(4,1,1,4),(101.447496653669,102.296234448537,
103.295070898499,103.672550060583),.UNSPECIFIED.);
#1320=B_SPLINE_CURVE_WITH_KNOTS('',3,(#134058,#134059,#134060,#134061,#134062,
#134063,#134064,#134065,#134066,#134067,#134068,#134069,#134070,#134071,
#134072,#134073,#134074,#134075,#134076,#134077,#134078,#134079,#134080,
#134081,#134082,#134083,#134084,#134085,#134086,#134087,#134088,#134089,
#134090,#134091,#134092,#134093,#134094,#134095,#134096,#134097,#134098,
#134099,#134100,#134101,#134102,#134103,#134104,#134105,#134106,#134107,
#134108,#134109,#134110,#134111,#134112,#134113,#134114,#134115,#134116,
#134117,#134118,#134119,#134120,#134121,#134122,#134123,#134124,#134125,
#134126,#134127,#134128,#134129,#134130,#134131,#134132,#134133,#134134,
#134135,#134136,#134137,#134138,#134139,#134140,#134141,#134142,#134143,
#134144,#134145,#134146,#134147,#134148,#134149,#134150,#134151,#134152,
#134153,#134154,#134155,#134156,#134157,#134158,#134159,#134160,#134161,
#134162,#134163,#134164,#134165,#134166,#134167,#134168,#134169,#134170,
#134171,#134172,#134173,#134174,#134175,#134176,#134177,#134178,#134179,
#134180,#134181,#134182,#134183,#134184),.UNSPECIFIED.,.F.,.F.,(4,3,3,3,
3,3,3,3,3,3,3,3,3,3,3,3,3,3,3,3,3,3,3,3,3,3,3,3,3,3,3,3,3,3,3,3,3,3,3,3,
3,3,4),(103.672557568463,103.771601702603,103.870660322484,103.96976131202,
104.06899945985,104.168318657834,104.267812431338,104.293907348461,104.392505473465,
104.490963256241,104.591185824014,104.689465381742,104.787711960816,104.885955043854,
104.987652232496,105.086036645915,105.189390222169,105.292743798423,105.391341923427,
105.489799706203,105.590022273976,105.688301831704,105.786548410778,105.884791493816,
105.986488682459,106.084873095877,106.188226672131,106.291580248385,106.390178373389,
106.488636156165,106.588858723938,106.687138281666,106.785384860739,106.883627943778,
106.98532513242,107.083709545839,107.187063122093,107.290416698347,107.38902306257,
107.48746439492,107.585810440424,107.684086111434,107.730086430664),
 .UNSPECIFIED.);
#1321=B_SPLINE_CURVE_WITH_KNOTS('',3,(#134190,#134191,#134192,#134193,#134194,
#134195,#134196,#134197,#134198,#134199,#134200,#134201,#134202,#134203,
#134204,#134205,#134206,#134207,#134208,#134209,#134210,#134211,#134212,
#134213,#134214,#134215,#134216,#134217,#134218,#134219,#134220,#134221,
#134222,#134223,#134224,#134225,#134226,#134227,#134228,#134229,#134230,
#134231,#134232,#134233,#134234,#134235,#134236,#134237,#134238,#134239,
#134240,#134241,#134242,#134243,#134244,#134245,#134246,#134247,#134248,
#134249,#134250,#134251,#134252,#134253,#134254,#134255,#134256,#134257,
#134258,#134259,#134260,#134261,#134262,#134263,#134264,#134265,#134266,
#134267,#134268,#134269,#134270,#134271,#134272,#134273,#134274,#134275,
#134276,#134277,#134278,#134279,#134280,#134281,#134282,#134283,#134284,
#134285,#134286,#134287,#134288,#134289,#134290,#134291,#134292,#134293,
#134294,#134295,#134296,#134297,#134298,#134299,#134300,#134301,#134302,
#134303,#134304,#134305,#134306,#134307,#134308,#134309,#134310,#134311,
#134312,#134313,#134314,#134315,#134316),.UNSPECIFIED.,.F.,.F.,(4,3,3,3,
3,3,3,3,3,3,3,3,3,3,3,3,3,3,3,3,3,3,3,3,3,3,3,3,3,3,3,3,3,3,3,3,3,3,3,3,
3,3,4),(109.955742875951,110.055241614051,110.152151423466,110.249014842069,
110.345862894414,110.447330365999,110.544300028994,110.641334438529,110.738518045248,
110.751732780752,110.850330905756,110.948788688532,111.049011256305,111.147290814033,
111.245537393106,111.343780476145,111.445477664787,111.543862078206,111.64721565446,
111.750569230714,111.849167355718,111.947625138495,112.047847706267,112.146127263995,
112.244373843069,112.342616926107,112.44431411475,112.542698528168,112.646052104422,
112.749405680676,112.84800380568,112.946461588456,113.046684156229,113.144963713957,
113.24321029303,113.341453376069,113.443150564711,113.54153497813,113.644888554384,
113.748242130638,113.846836224884,113.945278284704,114.013656815439),
 .UNSPECIFIED.);
#1322=B_SPLINE_CURVE_WITH_KNOTS('',3,(#134317,#134318,#134319,#134320,#134321,
#134322,#134323,#134324,#134325,#134326,#134327,#134328,#134329,#134330,
#134331,#134332,#134333,#134334,#134335,#134336,#134337,#134338,#134339,
#134340,#134341,#134342,#134343,#134344,#134345,#134346,#134347,#134348,
#134349,#134350,#134351,#134352,#134353,#134354,#134355,#134356,#134357,
#134358,#134359,#134360,#134361,#134362,#134363,#134364,#134365,#134366,
#134367,#134368,#134369,#134370,#134371,#134372,#134373,#134374,#134375,
#134376,#134377,#134378,#134379,#134380,#134381,#134382,#134383,#134384,
#134385,#134386),.UNSPECIFIED.,.F.,.F.,(4,3,3,3,3,3,3,3,3,3,3,3,3,3,3,3,
3,3,3,3,3,3,3,4),(107.72975655935,107.755223430866,107.85382155587,107.952279338646,
108.052501906419,108.150781464147,108.249028043221,108.347271126259,108.448968314901,
108.54735272832,108.650706304574,108.754059880828,108.852658005832,108.951115788608,
109.051338356381,109.149617914109,109.247864493183,109.346107576221,109.447804764863,
109.546189178282,109.649542754536,109.75289633079,109.893212936353,109.955742875643),
 .UNSPECIFIED.);
#1323=B_SPLINE_CURVE_WITH_KNOTS('',3,(#134388,#134389,#134390,#134391,#134392,
#134393,#134394,#134395,#134396,#134397,#134398,#134399,#134400,#134401,
#134402,#134403,#134404,#134405,#134406,#134407,#134408,#134409,#134410,
#134411,#134412,#134413,#134414,#134415,#134416,#134417,#134418,#134419,
#134420,#134421,#134422,#134423,#134424,#134425,#134426,#134427,#134428,
#134429,#134430,#134431,#134432,#134433,#134434,#134435,#134436,#134437,
#134438,#134439,#134440,#134441,#134442,#134443,#134444,#134445,#134446,
#134447,#134448,#134449,#134450,#134451,#134452,#134453,#134454,#134455,
#134456,#134457),.UNSPECIFIED.,.F.,.F.,(4,3,3,3,3,3,3,3,3,3,3,3,3,3,3,3,
3,3,3,3,3,3,3,4),(107.730086430664,107.828327794563,107.926578893471,108.024934180009,
108.123344704879,108.221924049223,108.289253148309,108.387851273313,108.486309056089,
108.586531623862,108.68481118159,108.783057760664,108.881300843702,108.982998032344,
109.081382445763,109.184736022017,109.288089598271,109.386591328536,109.484956309733,
109.583214317042,109.681399820025,109.779540599734,109.877698313766,109.955742875643),
 .UNSPECIFIED.);
#1324=B_SPLINE_CURVE_WITH_KNOTS('',3,(#134458,#134459,#134460,#134461,#134462,
#134463,#134464,#134465),.UNSPECIFIED.,.F.,.F.,(4,1,1,1,1,4),(109.95575001023,
110.286926048232,111.285762498194,112.284598948156,113.283435398118,114.012186952595),
 .UNSPECIFIED.);
#1325=B_SPLINE_CURVE_WITH_KNOTS('',3,(#134471,#134472,#134473,#134474,#134475,
#134476,#134477,#134478,#134479,#134480,#134481,#134482,#134483,#134484,
#134485,#134486,#134487,#134488,#134489,#134490,#134491,#134492,#134493,
#134494,#134495,#134496,#134497,#134498,#134499,#134500,#134501,#134502,
#134503,#134504,#134505,#134506,#134507,#134508,#134509,#134510,#134511,
#134512,#134513,#134514,#134515,#134516,#134517,#134518,#134519,#134520,
#134521,#134522,#134523,#134524,#134525,#134526,#134527,#134528,#134529,
#134530,#134531,#134532,#134533,#134534,#134535,#134536,#134537,#134538,
#134539,#134540,#134541,#134542,#134543,#134544,#134545,#134546,#134547,
#134548,#134549,#134550,#134551,#134552,#134553,#134554,#134555,#134556,
#134557,#134558,#134559,#134560,#134561,#134562,#134563,#134564,#134565,
#134566,#134567,#134568,#134569,#134570,#134571,#134572,#134573,#134574,
#134575,#134576,#134577,#134578,#134579,#134580,#134581,#134582,#134583,
#134584,#134585,#134586,#134587,#134588,#134589,#134590,#134591,#134592,
#134593,#134594),.UNSPECIFIED.,.F.,.F.,(4,3,3,3,3,3,3,3,3,3,3,3,3,3,3,3,
3,3,3,3,3,3,3,3,3,3,3,3,3,3,3,3,3,3,3,3,3,3,3,3,3,4),(116.238928182823,
116.341566510357,116.44447107289,116.547509821617,116.650828963887,116.744751480523,
116.843349605527,116.941807388303,117.042029956076,117.140309513804,117.238556092878,
117.336799175916,117.438496364558,117.536880777977,117.640234354231,117.743587930485,
117.842186055489,117.940643838265,118.040866406038,118.139145963766,118.23739254284,
118.335635625878,118.43733281452,118.535717227939,118.639070804193,118.742424380447,
118.841022505451,118.939480288227,119.039702856,119.137982413728,119.236228992802,
119.33447207584,119.436169264482,119.534553677901,119.637907254155,119.741260830409,
119.839851983057,119.938309194705,120.036651331114,120.134925920021,120.233176074197,
120.296103404723),.UNSPECIFIED.);
#1326=B_SPLINE_CURVE_WITH_KNOTS('',3,(#134595,#134596,#134597,#134598,#134599,
#134600,#134601,#134602,#134603,#134604,#134605,#134606,#134607,#134608,
#134609,#134610,#134611,#134612,#134613,#134614,#134615,#134616,#134617,
#134618,#134619,#134620,#134621,#134622,#134623,#134624,#134625,#134626,
#134627,#134628,#134629,#134630,#134631,#134632,#134633,#134634,#134635,
#134636,#134637,#134638,#134639,#134640,#134641,#134642,#134643,#134644,
#134645,#134646,#134647,#134648,#134649,#134650,#134651,#134652,#134653,
#134654,#134655,#134656,#134657,#134658,#134659,#134660,#134661,#134662,
#134663,#134664),.UNSPECIFIED.,.F.,.F.,(4,3,3,3,3,3,3,3,3,3,3,3,3,3,3,3,
3,3,3,3,3,3,3,4),(114.013656815439,114.111953393044,114.210207429762,114.308448417959,
114.406705828895,114.505071319279,114.603498058463,114.702086913916,114.747078580599,
114.845676705603,114.944134488379,115.044357056152,115.14263661388,115.240883192953,
115.339126275992,115.440823464634,115.539207878053,115.642561454307,115.745915030561,
115.84988875933,115.953561696348,116.057054365164,116.160309146371,116.238928182547),
 .UNSPECIFIED.);
#1327=B_SPLINE_CURVE_WITH_KNOTS('',3,(#134666,#134667,#134668,#134669,#134670,
#134671),.UNSPECIFIED.,.F.,.F.,(4,1,1,4),(114.012186952595,114.28227184808,
115.281108298042,116.238922797563),.UNSPECIFIED.);
#1328=B_SPLINE_CURVE_WITH_KNOTS('',3,(#134672,#134673,#134674,#134675,#134676,
#134677,#134678,#134679,#134680,#134681,#134682,#134683,#134684,#134685,
#134686,#134687,#134688,#134689,#134690,#134691,#134692,#134693,#134694,
#134695,#134696,#134697,#134698,#134699,#134700,#134701,#134702,#134703,
#134704,#134705,#134706,#134707,#134708,#134709,#134710,#134711,#134712,
#134713,#134714,#134715,#134716,#134717,#134718,#134719,#134720,#134721,
#134722,#134723,#134724,#134725,#134726,#134727,#134728,#134729,#134730,
#134731,#134732,#134733,#134734,#134735,#134736,#134737,#134738,#134739,
#134740,#134741,#134742,#134743,#134744,#134745,#134746,#134747,#134748,
#134749,#134750,#134751,#134752,#134753,#134754,#134755,#134756,#134757,
#134758,#134759,#134760,#134761,#134762,#134763,#134764,#134765,#134766,
#134767,#134768,#134769,#134770,#134771,#134772,#134773,#134774,#134775,
#134776,#134777,#134778,#134779,#134780,#134781,#134782,#134783,#134784,
#134785,#134786,#134787,#134788,#134789,#134790,#134791,#134792,#134793,
#134794,#134795,#134796,#134797,#134798),.UNSPECIFIED.,.F.,.F.,(4,3,3,3,
3,3,3,3,3,3,3,3,3,3,3,3,3,3,3,3,3,3,3,3,3,3,3,3,3,3,3,3,3,3,3,3,3,3,3,3,
3,3,4),(116.238928182823,116.279944748004,116.378542873008,116.477000655784,
116.577223223557,116.675502781285,116.773749360358,116.871992443397,116.973689632039,
117.072074045458,117.175427621712,117.278781197966,117.37737932297,117.475837105746,
117.576059673519,117.674339231247,117.77258581032,117.870828893359,117.972526082001,
118.07091049542,118.174264071673,118.277617647927,118.376215772931,118.474673555707,
118.57489612348,118.673175681208,118.771422260282,118.86966534332,118.971362531962,
119.069746945381,119.173100521635,119.276454097889,119.375052222893,119.47351000567,
119.573732573442,119.67201213117,119.770258710244,119.868501793282,119.970198981925,
120.068583395343,120.171936971597,120.275290547851,120.296396923363),
 .UNSPECIFIED.);
#1329=B_SPLINE_CURVE_WITH_KNOTS('',3,(#134804,#134805,#134806,#134807,#134808,
#134809,#134810,#134811),.UNSPECIFIED.,.F.,.F.,(4,1,1,1,1,4),(122.522113490002,
122.737770180294,123.736606630256,124.735443080218,125.73427953018,126.578666824116),
 .UNSPECIFIED.);
#1330=B_SPLINE_CURVE_WITH_KNOTS('',3,(#134812,#134813,#134814,#134815,#134816,
#134817,#134818,#134819,#134820,#134821,#134822,#134823,#134824,#134825,
#134826,#134827,#134828,#134829,#134830,#134831,#134832,#134833,#134834,
#134835,#134836,#134837,#134838,#134839,#134840,#134841,#134842,#134843,
#134844,#134845,#134846,#134847,#134848,#134849,#134850,#134851,#134852,
#134853,#134854,#134855,#134856,#134857,#134858,#134859,#134860,#134861,
#134862,#134863,#134864,#134865,#134866,#134867,#134868,#134869,#134870,
#134871,#134872,#134873,#134874,#134875,#134876,#134877,#134878,#134879,
#134880,#134881),.UNSPECIFIED.,.F.,.F.,(4,3,3,3,3,3,3,3,3,3,3,3,3,3,3,3,
3,3,3,3,3,3,3,4),(120.296103404723,120.394359158487,120.492722069624,120.591144783415,
120.689731197345,120.740097280371,120.838695405375,120.937153188151,121.037375755924,
121.135655313652,121.233901892726,121.332144975764,121.433842164406,121.532226577825,
121.635580154079,121.738933730333,121.836831200292,121.933909156543,122.030894120917,
122.127817176647,122.226391254986,122.323316910845,122.422715200424,122.522113490002),
 .UNSPECIFIED.);
#1331=B_SPLINE_CURVE_WITH_KNOTS('',3,(#134883,#134884,#134885,#134886,#134887,
#134888,#134889,#134890,#134891,#134892,#134893,#134894,#134895,#134896,
#134897,#134898,#134899,#134900,#134901,#134902,#134903,#134904,#134905,
#134906,#134907,#134908,#134909,#134910,#134911,#134912,#134913,#134914,
#134915,#134916,#134917,#134918,#134919,#134920,#134921,#134922,#134923,
#134924,#134925,#134926,#134927,#134928,#134929,#134930,#134931,#134932,
#134933,#134934,#134935,#134936,#134937,#134938,#134939,#134940,#134941,
#134942,#134943,#134944,#134945,#134946,#134947,#134948,#134949),
 .UNSPECIFIED.,.F.,.F.,(4,3,3,3,3,3,3,3,3,3,3,3,3,3,3,3,3,3,3,3,3,3,4),
(120.296396923363,120.394962257504,120.493394284,120.591721846097,120.689992664195,
120.788236250281,120.886482082457,120.98482755966,121.083221546878,121.181792233539,
121.274126997813,121.372725122817,121.471182905593,121.571405473366,121.669685031094,
121.767931610168,121.866174693206,121.967871881848,122.066256295267,122.169609871521,
122.272963447775,122.400857829823,122.522113389964),.UNSPECIFIED.);
#1332=B_SPLINE_CURVE_WITH_KNOTS('',3,(#134950,#134951,#134952,#134953,#134954,
#134955,#134956,#134957),.UNSPECIFIED.,.F.,.F.,(4,1,1,1,1,4),(122.522113490002,
123.271799897737,124.270636347699,125.26947279766,126.268309247622,126.580285757902),
 .UNSPECIFIED.);
#1333=B_SPLINE_CURVE_WITH_KNOTS('',3,(#134963,#134964,#134965,#134966,#134967,
#134968,#134969,#134970,#134971,#134972,#134973,#134974,#134975,#134976,
#134977,#134978,#134979,#134980,#134981,#134982,#134983,#134984,#134985,
#134986,#134987,#134988,#134989,#134990,#134991,#134992,#134993,#134994,
#134995,#134996,#134997,#134998,#134999,#135000,#135001,#135002,#135003,
#135004,#135005,#135006,#135007,#135008,#135009,#135010,#135011,#135012,
#135013,#135014,#135015,#135016,#135017,#135018,#135019,#135020,#135021,
#135022,#135023,#135024,#135025,#135026,#135027,#135028,#135029,#135030,
#135031,#135032,#135033,#135034,#135035,#135036,#135037,#135038,#135039,
#135040,#135041,#135042,#135043,#135044,#135045,#135046,#135047,#135048,
#135049,#135050,#135051,#135052,#135053,#135054,#135055,#135056,#135057,
#135058,#135059,#135060,#135061,#135062,#135063,#135064,#135065,#135066,
#135067,#135068,#135069,#135070,#135071,#135072,#135073,#135074,#135075,
#135076,#135077,#135078,#135079,#135080,#135081,#135082,#135083,#135084,
#135085,#135086,#135087,#135088,#135089),.UNSPECIFIED.,.F.,.F.,(4,3,3,3,
3,3,3,3,3,3,3,3,3,3,3,3,3,3,3,3,3,3,3,3,3,3,3,3,3,3,3,3,3,3,3,3,3,3,3,3,
3,3,4),(128.805298797182,128.902840431273,129.000250613517,129.097560812666,
129.194818343698,129.292053887497,129.389298094495,129.486642967568,129.584044330746,
129.68160592498,129.729625330028,129.828223455032,129.926681237808,130.026903805581,
130.125183363309,130.223429942382,130.321673025421,130.423370214063,130.521754627482,
130.625108203735,130.728461779989,130.827059904993,130.925517687769,131.025740255542,
131.12401981327,131.222266392343,131.320509475382,131.422206664024,131.520591077443,
131.623944653697,131.727298229951,131.825896354955,131.924354137732,132.024576705504,
132.122856263232,132.221102842306,132.319345925344,132.421043113987,132.519427527405,
132.622781103659,132.726134679913,132.824726637206,132.863178377909),
 .UNSPECIFIED.);
#1334=B_SPLINE_CURVE_WITH_KNOTS('',3,(#135090,#135091,#135092,#135093,#135094,
#135095,#135096),.UNSPECIFIED.,.F.,.F.,(4,1,1,1,4),(126.578666824116,126.733115980142,
127.731952430104,128.730788880066,128.805298797182),.UNSPECIFIED.);
#1335=B_SPLINE_CURVE_WITH_KNOTS('',3,(#135098,#135099,#135100,#135101,#135102,
#135103),.UNSPECIFIED.,.F.,.F.,(4,1,1,4),(126.580285757902,127.267145697584,
128.265982147546,128.805298797182),.UNSPECIFIED.);
#1336=B_SPLINE_CURVE_WITH_KNOTS('',3,(#135104,#135105,#135106,#135107,#135108,
#135109,#135110,#135111,#135112,#135113,#135114,#135115,#135116,#135117,
#135118,#135119,#135120,#135121,#135122,#135123,#135124,#135125,#135126,
#135127,#135128,#135129,#135130,#135131,#135132,#135133,#135134,#135135,
#135136,#135137,#135138,#135139,#135140,#135141,#135142,#135143,#135144,
#135145,#135146,#135147,#135148,#135149,#135150,#135151,#135152,#135153,
#135154,#135155,#135156,#135157,#135158,#135159,#135160,#135161,#135162,
#135163,#135164,#135165,#135166,#135167,#135168,#135169,#135170,#135171,
#135172,#135173,#135174,#135175,#135176,#135177,#135178,#135179,#135180,
#135181,#135182,#135183,#135184,#135185,#135186,#135187,#135188,#135189,
#135190,#135191,#135192,#135193,#135194,#135195,#135196,#135197,#135198,
#135199,#135200,#135201,#135202,#135203,#135204,#135205,#135206,#135207,
#135208,#135209,#135210,#135211,#135212,#135213,#135214,#135215,#135216,
#135217,#135218,#135219,#135220,#135221,#135222,#135223,#135224,#135225,
#135226,#135227),.UNSPECIFIED.,.F.,.F.,(4,3,3,3,3,3,3,3,3,3,3,3,3,3,3,3,
3,3,3,3,3,3,3,3,3,3,3,3,3,3,3,3,3,3,3,3,3,3,3,3,3,4),(128.805299011162,
128.910085619872,129.015255759152,129.120630109634,129.226318351048,129.264818597508,
129.363416722512,129.461874505289,129.562097073061,129.660376630789,129.758623209863,
129.856866292901,129.958563481543,130.056947894962,130.160301471216,130.26365504747,
130.362253172474,130.460710955251,130.560933523023,130.659213080752,130.757459659825,
130.855702742864,130.957399931506,131.055784344924,131.159137921178,131.262491497432,
131.361089622436,131.459547405212,131.559769972985,131.658049530713,131.756296109786,
131.854539192825,131.956236381467,132.054620794886,132.15797437114,132.261327947394,
132.3599137847,132.458366887935,132.559360488958,132.657635692185,132.759988492106,
132.862341292026),.UNSPECIFIED.);
#1337=B_SPLINE_CURVE_WITH_KNOTS('',3,(#135233,#135234,#135235,#135236,#135237,
#135238,#135239,#135240,#135241,#135242,#135243,#135244,#135245,#135246,
#135247,#135248,#135249,#135250,#135251,#135252,#135253,#135254,#135255,
#135256,#135257,#135258,#135259,#135260,#135261,#135262,#135263,#135264,
#135265,#135266,#135267,#135268,#135269,#135270,#135271,#135272,#135273,
#135274,#135275,#135276,#135277,#135278,#135279,#135280,#135281,#135282,
#135283,#135284,#135285,#135286,#135287,#135288,#135289,#135290,#135291,
#135292,#135293,#135294,#135295,#135296,#135297,#135298,#135299,#135300,
#135301,#135302,#135303,#135304,#135305,#135306,#135307,#135308,#135309,
#135310,#135311,#135312,#135313,#135314,#135315,#135316,#135317,#135318,
#135319,#135320,#135321,#135322,#135323,#135324,#135325,#135326,#135327,
#135328,#135329,#135330,#135331,#135332,#135333,#135334,#135335,#135336,
#135337,#135338,#135339,#135340,#135341,#135342,#135343,#135344,#135345,
#135346,#135347,#135348,#135349,#135350,#135351,#135352,#135353,#135354,
#135355,#135356,#135357,#135358,#135359),.UNSPECIFIED.,.F.,.F.,(4,3,3,3,
3,3,3,3,3,3,3,3,3,3,3,3,3,3,3,3,3,3,3,3,3,3,3,3,3,3,3,3,3,3,3,3,3,3,3,3,
3,3,4),(135.088484104361,135.187254556185,135.286029876603,135.384838499173,
135.483776463585,135.582788468007,135.681976179005,135.722644029799,135.821242154803,
135.91969993758,136.019922505352,136.11820206308,136.216448642154,136.314691725192,
136.416388913835,136.514773327253,136.618126903507,136.721480479761,136.820078604765,
136.918536387541,137.018758955314,137.117038513042,137.215285092115,137.313528175154,
137.415225363796,137.513609777215,137.616963353469,137.720316929723,137.818915054727,
137.917372837503,138.017595405276,138.115874963004,138.214121542077,138.312364625116,
138.414061813758,138.512446227177,138.61579980343,138.719153379684,138.817761602494,
138.916204188041,139.014551352306,139.112826031216,139.146050617851),
 .UNSPECIFIED.);
#1338=B_SPLINE_CURVE_WITH_KNOTS('',3,(#135360,#135361,#135362,#135363,#135364,
#135365,#135366,#135367,#135368,#135369,#135370,#135371,#135372,#135373,
#135374,#135375,#135376,#135377,#135378,#135379,#135380,#135381,#135382,
#135383,#135384,#135385,#135386,#135387,#135388,#135389,#135390,#135391,
#135392,#135393,#135394,#135395,#135396,#135397,#135398,#135399,#135400,
#135401,#135402,#135403,#135404,#135405,#135406,#135407,#135408,#135409,
#135410,#135411,#135412,#135413,#135414,#135415,#135416,#135417,#135418,
#135419,#135420,#135421,#135422,#135423,#135424,#135425,#135426,#135427,
#135428,#135429),.UNSPECIFIED.,.F.,.F.,(4,3,3,3,3,3,3,3,3,3,3,3,3,3,3,3,
3,3,3,3,3,3,3,4),(132.863178377909,132.961590295424,133.059905700764,133.1581695721,
133.256411413507,133.354660699864,133.453012805454,133.551418091656,133.649994565059,
133.724971129875,133.823569254879,133.922027037656,134.022249605428,134.120529163156,
134.21877574223,134.317018825268,134.41871601391,134.517100427329,134.620454003583,
134.723807579837,134.8363385207,134.948409000642,135.059693750754,135.088484104126),
 .UNSPECIFIED.);
#1339=B_SPLINE_CURVE_WITH_KNOTS('',3,(#135431,#135432,#135433,#135434,#135435,
#135436,#135437,#135438,#135439,#135440,#135441,#135442,#135443,#135444,
#135445,#135446,#135447,#135448,#135449,#135450,#135451,#135452,#135453,
#135454,#135455,#135456,#135457,#135458,#135459,#135460,#135461,#135462,
#135463,#135464,#135465,#135466,#135467,#135468,#135469,#135470,#135471,
#135472,#135473,#135474,#135475,#135476,#135477,#135478,#135479,#135480,
#135481,#135482,#135483,#135484,#135485,#135486,#135487,#135488,#135489,
#135490,#135491,#135492,#135493,#135494,#135495,#135496,#135497,#135498,
#135499,#135500),.UNSPECIFIED.,.F.,.F.,(4,3,3,3,3,3,3,3,3,3,3,3,3,3,3,3,
3,3,3,3,3,3,3,4),(132.862341292026,132.961797068358,133.060185474839,133.160174936097,
133.260164397355,133.358762522359,133.457220305135,133.557442872908,133.655722430636,
133.753969009709,133.852212092748,133.95390928139,134.052293694809,134.155647271063,
134.259000847317,134.356128675187,134.453094160804,134.549968416923,134.6467826177,
134.743567858739,134.84039997176,134.937256811786,135.034231214226,135.088484104361),
 .UNSPECIFIED.);
#1340=B_SPLINE_CURVE_WITH_KNOTS('',3,(#135501,#135502,#135503,#135504,#135505,
#135506,#135507,#135508),.UNSPECIFIED.,.F.,.F.,(4,1,1,1,1,4),(135.088484104361,
135.257837297279,136.256673747241,137.255510197203,138.254346647165,139.145213395082),
 .UNSPECIFIED.);
#1341=B_SPLINE_CURVE_WITH_KNOTS('',3,(#135514,#135515,#135516,#135517,#135518,
#135519,#135520,#135521,#135522,#135523,#135524,#135525,#135526,#135527,
#135528,#135529,#135530,#135531,#135532,#135533,#135534,#135535,#135536,
#135537,#135538,#135539,#135540,#135541,#135542,#135543,#135544,#135545,
#135546,#135547,#135548,#135549,#135550,#135551,#135552,#135553,#135554,
#135555,#135556,#135557,#135558,#135559,#135560,#135561,#135562,#135563,
#135564,#135565,#135566,#135567,#135568,#135569,#135570,#135571,#135572,
#135573,#135574,#135575,#135576,#135577,#135578,#135579,#135580,#135581,
#135582,#135583,#135584,#135585,#135586,#135587,#135588,#135589,#135590,
#135591,#135592,#135593,#135594,#135595,#135596,#135597,#135598,#135599,
#135600,#135601,#135602,#135603,#135604,#135605,#135606,#135607,#135608,
#135609,#135610,#135611,#135612,#135613,#135614,#135615,#135616,#135617,
#135618,#135619,#135620,#135621,#135622,#135623,#135624,#135625,#135626,
#135627,#135628,#135629,#135630,#135631,#135632,#135633,#135634,#135635,
#135636,#135637),.UNSPECIFIED.,.F.,.F.,(4,3,3,3,3,3,3,3,3,3,3,3,3,3,3,3,
3,3,3,3,3,3,3,3,3,3,3,3,3,3,3,3,3,3,3,3,3,3,3,3,3,4),(141.371669411768,
141.485016004535,141.600339367052,141.71566272957,141.814260854574,141.91271863735,
142.012941205123,142.111220762851,142.209467341925,142.307710424963,142.409407613605,
142.507792027024,142.611145603278,142.714499179532,142.813097304536,142.911555087312,
143.011777655085,143.110057212813,143.208303791887,143.306546874925,143.408244063567,
143.506628476986,143.60998205324,143.713335629494,143.811933754498,143.910391537275,
144.010614105047,144.108893662775,144.207140241849,144.305383324887,144.40708051353,
144.505464926948,144.608818503202,144.712172079456,144.810746601831,144.909191401419,
145.007536191859,145.105810581997,145.204060790383,145.302298022114,145.400579631078,
145.428467337346),.UNSPECIFIED.);
#1342=B_SPLINE_CURVE_WITH_KNOTS('',3,(#135638,#135639,#135640,#135641,#135642,
#135643,#135644,#135645,#135646,#135647,#135648,#135649,#135650,#135651,
#135652,#135653,#135654,#135655,#135656,#135657,#135658,#135659,#135660,
#135661,#135662,#135663,#135664,#135665,#135666,#135667,#135668,#135669,
#135670,#135671,#135672,#135673,#135674,#135675,#135676,#135677,#135678,
#135679,#135680,#135681,#135682,#135683,#135684,#135685,#135686,#135687,
#135688,#135689,#135690,#135691,#135692,#135693,#135694,#135695,#135696,
#135697,#135698,#135699,#135700,#135701,#135702,#135703,#135704,#135705,
#135706,#135707),.UNSPECIFIED.,.F.,.F.,(4,3,3,3,3,3,3,3,3,3,3,3,3,3,3,3,
3,3,3,3,3,3,3,4),(139.146050617851,139.244292880757,139.342541047598,139.440891102591,
139.539292953647,139.637867605968,139.717989829646,139.81658795465,139.915045737427,
140.015268305199,140.113547862927,140.211794442001,140.310037525039,140.411734713681,
140.5101191271,140.613472703354,140.716826279608,140.815569227393,140.914173010821,
141.012667061739,141.111081830931,141.209449097701,141.307822396312,141.371669411541),
 .UNSPECIFIED.);
#1343=B_SPLINE_CURVE_WITH_KNOTS('',3,(#135709,#135710,#135711,#135712,#135713,
#135714,#135715),.UNSPECIFIED.,.F.,.F.,(4,1,1,1,4),(139.145213395082,139.253183097127,
140.252019547089,141.25085599705,141.371669411541),.UNSPECIFIED.);
#1344=B_SPLINE_CURVE_WITH_KNOTS('',3,(#135716,#135717,#135718,#135719,#135720,
#135721,#135722,#135723,#135724,#135725,#135726,#135727,#135728,#135729,
#135730,#135731,#135732,#135733,#135734,#135735,#135736,#135737,#135738,
#135739,#135740,#135741,#135742,#135743,#135744,#135745,#135746,#135747,
#135748,#135749,#135750,#135751,#135752,#135753,#135754,#135755,#135756,
#135757,#135758,#135759,#135760,#135761,#135762,#135763,#135764,#135765,
#135766,#135767,#135768,#135769,#135770,#135771,#135772,#135773,#135774,
#135775,#135776,#135777,#135778,#135779,#135780,#135781,#135782,#135783,
#135784,#135785,#135786,#135787,#135788,#135789,#135790,#135791,#135792,
#135793,#135794,#135795,#135796,#135797,#135798,#135799,#135800,#135801,
#135802,#135803,#135804,#135805,#135806,#135807,#135808,#135809,#135810,
#135811,#135812,#135813,#135814,#135815,#135816,#135817,#135818,#135819,
#135820,#135821,#135822,#135823,#135824,#135825,#135826,#135827,#135828,
#135829,#135830,#135831,#135832,#135833,#135834,#135835,#135836,#135837,
#135838,#135839),.UNSPECIFIED.,.F.,.F.,(4,3,3,3,3,3,3,3,3,3,3,3,3,3,3,3,
3,3,3,3,3,3,3,3,3,3,3,3,3,3,3,3,3,3,3,3,3,3,3,3,3,4),(141.371669411541,
141.468831254161,141.566438903267,141.66339620349,141.760311911022,141.857216996242,
141.955335858935,142.052368429038,142.151030438025,142.249692447012,142.348290572016,
142.446748354792,142.546970922565,142.645250480293,142.743497059367,142.841740142405,
142.943437331047,143.041821744466,143.14517532072,143.248528896974,143.347127021978,
143.445584804754,143.545807372527,143.644086930255,143.742333509329,143.840576592367,
143.942273781009,144.040658194428,144.144011770682,144.247365346936,144.34596347194,
144.444421254716,144.544643822489,144.642923380217,144.741169959291,144.839413042329,
144.941110230971,145.03949464439,145.142848220644,145.246201796898,145.344774861155,
145.42960468327),.UNSPECIFIED.);
#1345=B_SPLINE_CURVE_WITH_KNOTS('',3,(#135845,#135846,#135847,#135848,#135849,
#135850,#135851,#135852,#135853),.UNSPECIFIED.,.F.,.F.,(4,1,1,1,1,1,4),
(147.65485471872,147.708681429341,148.707517879303,149.706354329265,150.705190779227,
151.704027229189,151.712252768111),.UNSPECIFIED.);
#1346=B_SPLINE_CURVE_WITH_KNOTS('',3,(#135854,#135855,#135856,#135857,#135858,
#135859,#135860,#135861,#135862,#135863,#135864,#135865,#135866,#135867,
#135868,#135869,#135870,#135871,#135872,#135873,#135874,#135875,#135876,
#135877,#135878,#135879,#135880,#135881,#135882,#135883,#135884,#135885,
#135886,#135887,#135888,#135889,#135890,#135891,#135892,#135893,#135894,
#135895,#135896,#135897,#135898,#135899,#135900,#135901,#135902,#135903,
#135904,#135905,#135906,#135907,#135908,#135909,#135910,#135911,#135912,
#135913,#135914,#135915,#135916,#135917,#135918,#135919,#135920,#135921,
#135922,#135923),.UNSPECIFIED.,.F.,.F.,(4,3,3,3,3,3,3,3,3,3,3,3,3,3,3,3,
3,3,3,3,3,3,3,4),(145.428467337346,145.526865630197,145.625438451516,145.711008529418,
145.809606654422,145.908064437198,146.008287004971,146.106566562699,146.204813141772,
146.303056224811,146.404753413453,146.503137826872,146.606491403125,146.709844979379,
146.807643480436,146.905302408374,147.002849316603,147.100335701354,147.197792033696,
147.295248746519,147.392798083501,147.490396206244,147.588155506493,147.65485471872),
 .UNSPECIFIED.);
#1347=B_SPLINE_CURVE_WITH_KNOTS('',3,(#135925,#135926,#135927,#135928,#135929,
#135930,#135931,#135932,#135933,#135934,#135935,#135936,#135937,#135938,
#135939,#135940,#135941,#135942,#135943,#135944,#135945,#135946,#135947,
#135948,#135949,#135950,#135951,#135952,#135953,#135954,#135955,#135956,
#135957,#135958,#135959,#135960,#135961,#135962,#135963,#135964,#135965,
#135966,#135967,#135968,#135969,#135970,#135971,#135972,#135973,#135974,
#135975,#135976,#135977,#135978,#135979,#135980,#135981,#135982,#135983,
#135984,#135985,#135986,#135987,#135988,#135989,#135990,#135991,#135992,
#135993,#135994),.UNSPECIFIED.,.F.,.F.,(4,3,3,3,3,3,3,3,3,3,3,3,3,3,3,3,
3,3,3,3,3,3,3,4),(145.42960468327,145.531533878718,145.629819454555,145.728068466941,
145.826310401823,145.924574729419,146.022950479282,146.121392844886,146.219991608955,
146.24503824686,146.343636371864,146.442094154641,146.542316722413,146.640596280141,
146.738842859215,146.837085942253,146.938783130896,147.037167544314,147.140521120568,
147.243874696822,147.352569174393,147.460952550047,147.568802109383,147.654854305396),
 .UNSPECIFIED.);
#1348=B_SPLINE_CURVE_WITH_KNOTS('',3,(#135995,#135996,#135997,#135998,#135999,
#136000,#136001,#136002),.UNSPECIFIED.,.F.,.F.,(4,1,1,1,1,4),(147.65485471872,
148.242711146784,149.241547596745,150.240384046707,151.239220496669,151.712342689598),
 .UNSPECIFIED.);
#1349=B_SPLINE_CURVE_WITH_KNOTS('',3,(#136008,#136009,#136010,#136011,#136012,
#136013,#136014,#136015,#136016,#136017,#136018,#136019,#136020,#136021,
#136022,#136023,#136024,#136025,#136026,#136027,#136028,#136029,#136030,
#136031,#136032,#136033,#136034,#136035,#136036,#136037,#136038,#136039,
#136040,#136041,#136042,#136043,#136044,#136045,#136046,#136047,#136048,
#136049,#136050,#136051,#136052,#136053,#136054,#136055,#136056,#136057,
#136058,#136059,#136060,#136061,#136062,#136063,#136064,#136065,#136066,
#136067,#136068,#136069,#136070,#136071,#136072,#136073,#136074,#136075,
#136076,#136077,#136078,#136079,#136080,#136081,#136082,#136083,#136084,
#136085,#136086,#136087,#136088,#136089,#136090,#136091,#136092,#136093,
#136094,#136095,#136096,#136097,#136098,#136099,#136100,#136101,#136102,
#136103,#136104,#136105,#136106,#136107,#136108,#136109,#136110,#136111,
#136112,#136113,#136114,#136115,#136116,#136117,#136118,#136119,#136120,
#136121,#136122,#136123,#136124,#136125,#136126,#136127,#136128,#136129,
#136130,#136131),.UNSPECIFIED.,.F.,.F.,(4,3,3,3,3,3,3,3,3,3,3,3,3,3,3,3,
3,3,3,3,3,3,3,3,3,3,3,3,3,3,3,3,3,3,3,3,3,3,3,3,3,4),(153.9380400259,154.035163898234,
154.132222574362,154.229246955324,154.326267897773,154.423381488606,154.520541056366,
154.617870832504,154.700536579074,154.799134704076,154.897592486852,154.997815054625,
155.096094612352,155.194341191424,155.292584274461,155.394281463105,155.492665876523,
155.596019452779,155.699373029036,155.797971154037,155.896428936811,155.996651504585,
156.09493106231,156.193177641381,156.291420724417,156.393117913062,156.491502326478,
156.594855902738,156.698209478998,156.796807604012,156.895265386799,156.995487954569,
157.093767512308,157.192014091391,157.29025717444,157.39195436307,157.490338776498,
157.593692352729,157.69704592896,157.79563212985,157.895770613718,157.995909097586),
 .UNSPECIFIED.);
#1350=B_SPLINE_CURVE_WITH_KNOTS('',3,(#136132,#136133,#136134,#136135,#136136,
#136137),.UNSPECIFIED.,.F.,.F.,(4,1,1,4),(151.712252768111,152.702863679151,
153.701700129113,153.938039726867),.UNSPECIFIED.);
#1351=B_SPLINE_CURVE_WITH_KNOTS('',3,(#136139,#136140,#136141,#136142,#136143,
#136144),.UNSPECIFIED.,.F.,.F.,(4,1,1,4),(151.712342689598,152.238056946631,
153.236893396593,153.9380400259),.UNSPECIFIED.);
#1352=B_SPLINE_CURVE_WITH_KNOTS('',3,(#136145,#136146,#136147,#136148,#136149,
#136150,#136151,#136152,#136153,#136154,#136155,#136156,#136157,#136158,
#136159,#136160,#136161,#136162,#136163,#136164,#136165,#136166,#136167,
#136168,#136169,#136170,#136171,#136172,#136173,#136174,#136175,#136176,
#136177,#136178,#136179,#136180,#136181,#136182,#136183,#136184,#136185,
#136186,#136187,#136188,#136189,#136190,#136191,#136192,#136193,#136194,
#136195,#136196,#136197,#136198,#136199,#136200,#136201,#136202,#136203,
#136204,#136205,#136206,#136207,#136208,#136209,#136210,#136211,#136212,
#136213,#136214,#136215,#136216,#136217,#136218,#136219,#136220,#136221,
#136222,#136223,#136224,#136225,#136226,#136227,#136228,#136229,#136230,
#136231,#136232,#136233,#136234,#136235,#136236,#136237,#136238,#136239,
#136240,#136241,#136242,#136243,#136244,#136245,#136246,#136247,#136248,
#136249,#136250,#136251,#136252,#136253,#136254,#136255,#136256,#136257,
#136258,#136259,#136260,#136261,#136262,#136263,#136264,#136265,#136266,
#136267,#136268),.UNSPECIFIED.,.F.,.F.,(4,3,3,3,3,3,3,3,3,3,3,3,3,3,3,3,
3,3,3,3,3,3,3,3,3,3,3,3,3,3,3,3,3,3,3,3,3,3,3,3,3,4),(153.938040202769,
154.056659980237,154.176963650994,154.235729846555,154.334327971559,154.432785754335,
154.533008322108,154.631287879836,154.729534458909,154.827777541948,154.92947473059,
155.027859144009,155.131212720263,155.234566296517,155.33316442152,155.431622204296,
155.531844772069,155.630124329797,155.72837090887,155.826613991908,155.928311180551,
156.026695593969,156.130049170224,156.233402746479,156.332000871484,156.430458654262,
156.530681222034,156.628960779764,156.727207358839,156.825450441879,156.927147630519,
157.025532043939,157.12888562019,157.23223919644,157.330809964381,157.429252216959,
157.527595662269,157.625869905304,157.724128943531,157.822375482211,157.920688283601,
157.994794042337),.UNSPECIFIED.);
#1353=B_SPLINE_CURVE_WITH_KNOTS('',3,(#136274,#136275,#136276,#136277,#136278,
#136279,#136280,#136281),.UNSPECIFIED.,.F.,.F.,(4,1,1,1,1,4),(160.221227414795,
160.693555278846,161.692391728808,162.691228178769,163.690064628731,164.278110089382),
 .UNSPECIFIED.);
#1354=B_SPLINE_CURVE_WITH_KNOTS('',3,(#136282,#136283,#136284,#136285,#136286,
#136287,#136288,#136289,#136290,#136291,#136292,#136293,#136294,#136295,
#136296,#136297,#136298,#136299,#136300,#136301,#136302,#136303,#136304,
#136305,#136306,#136307,#136308,#136309,#136310,#136311,#136312,#136313,
#136314,#136315,#136316,#136317,#136318,#136319,#136320,#136321,#136322,
#136323,#136324,#136325,#136326,#136327,#136328,#136329,#136330,#136331,
#136332,#136333,#136334,#136335,#136336,#136337,#136338,#136339,#136340,
#136341,#136342,#136343,#136344,#136345,#136346,#136347,#136348,#136349,
#136350,#136351),.UNSPECIFIED.,.F.,.F.,(4,3,3,3,3,3,3,3,3,3,3,3,3,3,3,3,
3,3,3,3,3,3,3,4),(157.995909097586,158.094187889713,158.192434178687,158.290677446715,
158.391978679767,158.490363789568,158.593123084245,158.695882378922,158.794480503912,
158.892938286675,158.993160854451,159.091440412165,159.189686991225,159.287930074249,
159.389627262908,159.488011676312,159.591365252598,159.694718828884,159.797216560019,
159.903218753284,160.005303397591,160.107256278835,160.209067828953,160.22122533308),
 .UNSPECIFIED.);
#1355=B_SPLINE_CURVE_WITH_KNOTS('',3,(#136353,#136354,#136355,#136356,#136357,
#136358,#136359,#136360,#136361,#136362,#136363,#136364,#136365,#136366,
#136367,#136368,#136369,#136370,#136371,#136372,#136373,#136374,#136375,
#136376,#136377,#136378,#136379,#136380,#136381,#136382,#136383,#136384,
#136385,#136386,#136387,#136388,#136389,#136390,#136391,#136392,#136393,
#136394,#136395,#136396,#136397,#136398,#136399,#136400,#136401,#136402,
#136403,#136404,#136405,#136406,#136407,#136408,#136409,#136410,#136411,
#136412,#136413,#136414,#136415,#136416,#136417,#136418,#136419,#136420,
#136421,#136422),.UNSPECIFIED.,.F.,.F.,(4,3,3,3,3,3,3,3,3,3,3,3,3,3,3,3,
3,3,3,3,3,3,3,4),(157.994794042337,158.093225162031,158.191816728715,158.231075646402,
158.329673771403,158.428131554177,158.528354121951,158.626633679676,158.724880258747,
158.823123341783,158.924820530428,159.023204943844,159.126558520104,159.229912096364,
159.328378576654,159.426704810661,159.526019875932,159.624169149678,159.722285836342,
159.820399593048,159.920606027993,160.018861091251,160.120043212039,160.221225332828),
 .UNSPECIFIED.);
#1356=B_SPLINE_CURVE_WITH_KNOTS('',3,(#136423,#136424,#136425,#136426,#136427,
#136428,#136429,#136430,#136431,#136432,#136433,#136434,#136435,#136436,
#136437,#136438,#136439,#136440,#136441,#136442,#136443,#136444,#136445,
#136446,#136447,#136448,#136449,#136450,#136451,#136452,#136453,#136454,
#136455,#136456,#136457,#136458,#136459,#136460,#136461,#136462,#136463,
#136464,#136465,#136466,#136467,#136468,#136469,#136470,#136471,#136472,
#136473,#136474,#136475,#136476,#136477,#136478,#136479,#136480,#136481,
#136482,#136483,#136484,#136485,#136486,#136487,#136488,#136489,#136490,
#136491,#136492,#136493,#136494,#136495,#136496,#136497,#136498,#136499,
#136500,#136501,#136502,#136503,#136504,#136505,#136506,#136507,#136508,
#136509,#136510,#136511,#136512,#136513,#136514,#136515,#136516,#136517,
#136518,#136519,#136520,#136521,#136522,#136523,#136524,#136525,#136526,
#136527,#136528,#136529,#136530,#136531,#136532,#136533,#136534,#136535,
#136536,#136537,#136538,#136539,#136540,#136541,#136542,#136543,#136544,
#136545,#136546,#136547,#136548,#136549),.UNSPECIFIED.,.F.,.F.,(4,3,3,3,
3,3,3,3,3,3,3,3,3,3,3,3,3,3,3,3,3,3,3,3,3,3,3,3,3,3,3,3,3,3,3,3,3,3,3,3,
3,3,4),(160.22122533308,160.228748546326,160.327346671318,160.425804454083,
160.526027021859,160.624306579575,160.722553158637,160.820796241664,160.92249343032,
161.020877843728,161.124231420008,161.227584996288,161.326183121278,161.424640904041,
161.524863471817,161.623143029531,161.72138960859,161.819632691614,161.921329880273,
162.019714293678,162.123067869964,162.22642144625,162.325019571326,162.423477354175,
162.52369992193,162.62197947973,162.720226058876,162.818469141986,162.920166330543,
163.018550744032,163.121904320122,163.225257896212,163.323856021116,163.422313803793,
163.522536371591,163.62081592922,163.719062508196,163.817305591138,163.919002779897,
164.017387193222,164.120740769698,164.224094346174,164.278857755076),
 .UNSPECIFIED.);
#1357=B_SPLINE_CURVE_WITH_KNOTS('',3,(#136555,#136556,#136557,#136558,#136559,
#136560,#136561,#136562,#136563,#136564,#136565,#136566,#136567,#136568,
#136569,#136570,#136571,#136572,#136573,#136574,#136575,#136576,#136577,
#136578,#136579,#136580,#136581,#136582,#136583,#136584,#136585,#136586,
#136587,#136588,#136589,#136590,#136591,#136592,#136593,#136594,#136595,
#136596,#136597,#136598,#136599,#136600,#136601,#136602,#136603,#136604,
#136605,#136606,#136607,#136608,#136609,#136610,#136611,#136612,#136613,
#136614,#136615,#136616,#136617,#136618,#136619,#136620,#136621,#136622,
#136623,#136624,#136625,#136626,#136627,#136628,#136629,#136630,#136631,
#136632,#136633,#136634,#136635,#136636,#136637,#136638,#136639,#136640,
#136641,#136642,#136643,#136644,#136645,#136646,#136647,#136648,#136649,
#136650,#136651,#136652,#136653,#136654,#136655,#136656,#136657,#136658,
#136659,#136660,#136661,#136662,#136663,#136664,#136665,#136666,#136667,
#136668,#136669,#136670,#136671,#136672,#136673,#136674,#136675,#136676,
#136677,#136678),.UNSPECIFIED.,.F.,.F.,(4,3,3,3,3,3,3,3,3,3,3,3,3,3,3,3,
3,3,3,3,3,3,3,3,3,3,3,3,3,3,3,3,3,3,3,3,3,3,3,3,3,4),(166.504410640259,
166.652910770048,166.686573978617,166.78517209724,166.883629873641,166.983852443008,
167.08213199442,167.180378567212,167.278621644013,167.380318840155,167.478703247507,
167.582056838043,167.685410428579,167.784008554557,167.882466338249,167.982688905786,
168.080968464281,168.179215044066,168.277458127759,168.379155315454,168.477539729381,
168.580893303961,168.684246878541,168.782845025208,168.88130282975,168.981525392094,
169.079804971676,169.17805157259,169.276294677425,169.377991840195,169.476376275083,
169.579729801793,169.683083328503,169.781689728101,169.88012748496,169.97846945026,
170.076745220522,170.174984321675,170.273261950963,170.371554713658,170.469968414811,
170.561255430934),.UNSPECIFIED.);
#1358=B_SPLINE_CURVE_WITH_KNOTS('',3,(#136679,#136680,#136681,#136682,#136683,
#136684),.UNSPECIFIED.,.F.,.F.,(4,1,1,4),(164.278110089382,164.688901078693,
165.687737528655,166.504405682607),.UNSPECIFIED.);
#1359=B_SPLINE_CURVE_WITH_KNOTS('',3,(#136686,#136687,#136688,#136689,#136690,
#136691,#136692,#136693,#136694,#136695,#136696,#136697,#136698,#136699,
#136700,#136701,#136702,#136703,#136704,#136705,#136706,#136707,#136708,
#136709,#136710,#136711,#136712,#136713,#136714,#136715,#136716,#136717,
#136718,#136719,#136720,#136721,#136722,#136723,#136724,#136725,#136726,
#136727,#136728,#136729,#136730,#136731,#136732,#136733,#136734,#136735,
#136736,#136737,#136738,#136739,#136740,#136741,#136742,#136743,#136744,
#136745,#136746,#136747,#136748,#136749,#136750,#136751,#136752,#136753,
#136754,#136755),.UNSPECIFIED.,.F.,.F.,(4,3,3,3,3,3,3,3,3,3,3,3,3,3,3,3,
3,3,3,3,3,3,3,4),(164.278857755076,164.377373896582,164.475767937975,164.574072811189,
164.672331019042,164.770572058965,164.868825403572,164.967184449585,165.065601043159,
165.164183843334,165.222930796135,165.321528921635,165.419986704909,165.520209272557,
165.618488830783,165.716735410353,165.814978493886,165.916675681939,166.015060095843,
166.11841367097,166.221767246097,166.344599874415,166.465474953167,166.504410639987),
 .UNSPECIFIED.);
#1360=B_SPLINE_CURVE_WITH_KNOTS('',3,(#136756,#136757,#136758,#136759,#136760,
#136761,#136762,#136763,#136764,#136765,#136766,#136767,#136768,#136769,
#136770,#136771,#136772,#136773,#136774,#136775,#136776,#136777,#136778,
#136779,#136780,#136781,#136782,#136783,#136784,#136785,#136786,#136787,
#136788,#136789,#136790,#136791,#136792,#136793,#136794,#136795,#136796,
#136797,#136798,#136799,#136800,#136801,#136802,#136803,#136804,#136805,
#136806,#136807,#136808,#136809,#136810,#136811,#136812,#136813,#136814,
#136815,#136816,#136817,#136818,#136819,#136820,#136821,#136822,#136823,
#136824,#136825,#136826,#136827,#136828,#136829,#136830,#136831,#136832,
#136833,#136834,#136835,#136836,#136837,#136838,#136839,#136840,#136841,
#136842,#136843,#136844,#136845,#136846,#136847,#136848,#136849,#136850,
#136851,#136852,#136853,#136854,#136855,#136856,#136857,#136858,#136859,
#136860,#136861,#136862,#136863,#136864,#136865,#136866,#136867,#136868,
#136869,#136870,#136871,#136872,#136873,#136874,#136875,#136876,#136877,
#136878,#136879,#136880,#136881,#136882),.UNSPECIFIED.,.F.,.F.,(4,3,3,3,
3,3,3,3,3,3,3,3,3,3,3,3,3,3,3,3,3,3,3,3,3,3,3,3,3,3,3,3,3,3,3,3,3,3,3,3,
3,3,4),(166.504410640259,166.6019131263,166.699371433808,166.79681599036,
166.894277201722,166.991846173226,167.089478292235,167.187269535436,167.220603696059,
167.319201820914,167.417659603534,167.517882171345,167.616161728897,167.714408307787,
167.812651390635,167.914348579482,168.012732992696,168.116086569359,168.219440146021,
168.318038274349,168.416496060462,168.516718627402,168.614998188473,168.713244770885,
168.811487857253,168.913185041936,169.011569458627,169.114923027305,169.218276595983,
169.316874714603,169.415332491002,169.51555506037,169.61383461178,169.71208118457,
169.810324261369,169.912021457513,170.010405864863,170.113759455404,170.217113045945,
170.315689889886,170.414143809236,170.512486666534,170.56219066747),
 .UNSPECIFIED.);
#1361=B_SPLINE_CURVE_WITH_KNOTS('',3,(#136888,#136889,#136890,#136891,#136892,
#136893,#136894,#136895,#136896,#136897,#136898,#136899,#136900,#136901,
#136902,#136903,#136904,#136905,#136906,#136907,#136908,#136909,#136910,
#136911,#136912,#136913,#136914,#136915,#136916,#136917,#136918,#136919,
#136920,#136921,#136922,#136923,#136924,#136925,#136926,#136927,#136928,
#136929,#136930,#136931,#136932,#136933,#136934,#136935,#136936,#136937,
#136938,#136939,#136940,#136941,#136942,#136943,#136944,#136945,#136946,
#136947,#136948,#136949,#136950,#136951,#136952,#136953,#136954,#136955,
#136956,#136957,#136958,#136959,#136960,#136961,#136962,#136963,#136964,
#136965,#136966,#136967,#136968,#136969,#136970,#136971,#136972,#136973,
#136974,#136975,#136976,#136977,#136978,#136979,#136980,#136981,#136982,
#136983,#136984,#136985,#136986,#136987,#136988,#136989,#136990,#136991,
#136992,#136993,#136994,#136995,#136996,#136997,#136998,#136999,#137000,
#137001,#137002,#137003,#137004,#137005,#137006,#137007,#137008,#137009,
#137010,#137011,#137012,#137013,#137014),.UNSPECIFIED.,.F.,.F.,(4,3,3,3,
3,3,3,3,3,3,3,3,3,3,3,3,3,3,3,3,3,3,3,3,3,3,3,3,3,3,3,3,3,3,3,3,3,3,3,3,
3,3,4),(172.787595947668,172.884841559506,172.984040005612,173.081071838667,
173.178059271087,173.275033215733,173.375882193887,173.472980628238,173.570144972561,
173.667458410759,173.67842912835,173.777027506202,173.875485539322,173.975708044196,
174.073987844422,174.172234662569,174.270477980966,174.372174880302,174.470559517526,
174.573912547919,174.677265578312,174.775864529236,174.874323143897,174.974545504444,
175.072825902575,175.171073323387,175.269317248384,175.371013443357,175.469398690653,
175.572750359463,175.676102028274,175.774697491594,175.873152609552,175.973375843138,
176.071652747408,176.169896682952,176.268137135791,176.369837471402,176.468219314363,
176.571578896299,176.674938478236,176.773518525278,176.845520762148),
 .UNSPECIFIED.);
#1362=B_SPLINE_CURVE_WITH_KNOTS('',3,(#137015,#137016,#137017,#137018,#137019,
#137020,#137021,#137022,#137023,#137024,#137025,#137026,#137027,#137028,
#137029,#137030,#137031,#137032,#137033,#137034,#137035,#137036,#137037,
#137038,#137039,#137040,#137041,#137042,#137043,#137044,#137045,#137046,
#137047,#137048,#137049,#137050,#137051,#137052,#137053,#137054,#137055,
#137056,#137057,#137058,#137059,#137060,#137061,#137062,#137063,#137064,
#137065,#137066,#137067,#137068,#137069,#137070,#137071,#137072,#137073,
#137074,#137075,#137076,#137077,#137078,#137079,#137080,#137081,#137082,
#137083,#137084),.UNSPECIFIED.,.F.,.F.,(4,3,3,3,3,3,3,3,3,3,3,3,3,3,3,3,
3,3,3,3,3,3,3,4),(170.561255430934,170.659855746347,170.681919778464,170.780517924844,
170.878975728609,170.979198291086,171.077477868714,171.175724467241,171.273967569265,
171.375664734055,171.474049165113,171.57740269677,171.680756228426,171.779354490085,
171.877812410303,171.978034943814,172.076314639908,172.174561357392,172.272804578702,
172.374501603624,172.472886153556,172.576239415972,172.679592678388,172.787595947439),
 .UNSPECIFIED.);
#1363=B_SPLINE_CURVE_WITH_KNOTS('',3,(#137086,#137087,#137088,#137089,#137090,
#137091,#137092,#137093,#137094,#137095,#137096,#137097,#137098,#137099,
#137100,#137101,#137102,#137103,#137104,#137105,#137106,#137107,#137108,
#137109,#137110,#137111,#137112,#137113,#137114,#137115,#137116,#137117,
#137118,#137119,#137120,#137121,#137122,#137123,#137124,#137125,#137126,
#137127,#137128,#137129,#137130,#137131,#137132,#137133,#137134,#137135,
#137136,#137137,#137138,#137139,#137140,#137141,#137142,#137143,#137144,
#137145,#137146,#137147,#137148,#137149,#137150,#137151,#137152,#137153,
#137154,#137155),.UNSPECIFIED.,.F.,.F.,(4,3,3,3,3,3,3,3,3,3,3,3,3,3,3,3,
3,3,3,3,3,3,3,4),(170.56219066747,170.660450504082,170.758691702558,170.856943736123,
170.95530060812,171.053713706999,171.152294500948,171.215949495907,171.314547642582,
171.413005447132,171.513228009474,171.611507589065,171.709754189987,171.807997294831,
171.909694457591,172.008078892487,172.111432419178,172.214785945869,172.315617765289,
172.416285943601,172.51678187547,172.617176498695,172.717484580153,172.787595947439),
 .UNSPECIFIED.);
#1364=B_SPLINE_CURVE_WITH_KNOTS('',3,(#137156,#137157,#137158,#137159,#137160,
#137161,#137162,#137163),.UNSPECIFIED.,.F.,.F.,(4,1,1,1,1,4),(172.787601414733,
173.21362239583,174.212458845792,175.211295295754,176.210131745716,176.844282066305),
 .UNSPECIFIED.);
#1365=B_SPLINE_CURVE_WITH_KNOTS('',3,(#137169,#137170,#137171,#137172,#137173,
#137174,#137175,#137176),.UNSPECIFIED.,.F.,.F.,(4,1,1,1,1,4),(179.070781254618,
179.671447828121,180.670284278083,181.669120728045,182.667957178007,183.128402534571),
 .UNSPECIFIED.);
#1366=B_SPLINE_CURVE_WITH_KNOTS('',3,(#137177,#137178,#137179,#137180,#137181,
#137182,#137183,#137184,#137185,#137186,#137187,#137188,#137189,#137190,
#137191,#137192,#137193,#137194,#137195,#137196,#137197,#137198,#137199,
#137200,#137201,#137202,#137203,#137204,#137205,#137206,#137207,#137208,
#137209,#137210,#137211,#137212,#137213,#137214,#137215,#137216,#137217,
#137218,#137219,#137220,#137221,#137222,#137223,#137224,#137225,#137226,
#137227,#137228,#137229,#137230,#137231,#137232,#137233,#137234,#137235,
#137236,#137237,#137238,#137239,#137240,#137241,#137242,#137243,#137244,
#137245,#137246),.UNSPECIFIED.,.F.,.F.,(4,3,3,3,3,3,3,3,3,3,3,3,3,3,3,3,
3,3,3,3,3,3,3,4),(176.845520762148,176.949052532905,177.047346579314,177.145600669623,
177.243844290299,177.342106909026,177.440479022331,177.538914695786,177.637509892069,
177.673774928198,177.772377752086,177.87084027796,177.971061665485,178.069346039597,
178.167597451746,178.265845378085,178.367536878104,178.465926110356,178.569268744257,
178.672611378159,178.782250156969,178.891545552981,179.000249474037,179.070781030164),
 .UNSPECIFIED.);
#1367=B_SPLINE_CURVE_WITH_KNOTS('',3,(#137248,#137249,#137250,#137251,#137252,
#137253),.UNSPECIFIED.,.F.,.F.,(4,1,1,4),(176.844282066305,177.208968195678,
178.20780464564,179.070781254618),.UNSPECIFIED.);
#1368=B_SPLINE_CURVE_WITH_KNOTS('',3,(#137254,#137255,#137256,#137257,#137258,
#137259,#137260,#137261),.UNSPECIFIED.,.F.,.F.,(4,1,1,1,1,4),(179.070781254618,
179.206641095602,180.205477545564,181.204313995525,182.203150445487,183.12768829285),
 .UNSPECIFIED.);
#1369=B_SPLINE_CURVE_WITH_KNOTS('',3,(#137267,#137268,#137269,#137270,#137271,
#137272,#137273,#137274),.UNSPECIFIED.,.F.,.F.,(4,1,1,1,1,4),(15.707963267949,
15.8622700343739,16.8611064843358,17.8599429342977,18.8587793842595,19.7647623489133),
 .UNSPECIFIED.);
#1370=B_SPLINE_CURVE_WITH_KNOTS('',3,(#137276,#137277,#137278,#137279,#137280,
#137281,#137282,#137283,#137284,#137285,#137286,#137287,#137288,#137289,
#137290,#137291,#137292,#137293,#137294,#137295,#137296,#137297,#137298,
#137299,#137300,#137301,#137302,#137303,#137304,#137305,#137306,#137307,
#137308,#137309,#137310,#137311,#137312,#137313,#137314,#137315,#137316,
#137317,#137318,#137319,#137320,#137321,#137322,#137323,#137324,#137325,
#137326,#137327,#137328,#137329,#137330,#137331,#137332,#137333),
 .UNSPECIFIED.,.F.,.F.,(4,3,3,3,3,3,3,3,3,3,3,3,3,3,3,3,3,3,3,4),(13.8757070305518,
13.9742335824856,14.0726198317922,14.1714715508697,14.2696802764454,14.3678558944916,
14.4660279816071,14.5653793823083,14.6636893819281,14.7635614831701,14.8634335844121,
14.9606976623845,15.0578044029831,15.1548229005499,15.2517842045426,15.3487192918042,
15.4457083561665,15.542724156859,15.6398692496992,15.707963267949),
 .UNSPECIFIED.);
#1371=B_SPLINE_CURVE_WITH_KNOTS('',3,(#137337,#137338,#137339,#137340,#137341),
 .UNSPECIFIED.,.F.,.F.,(4,1,4),(14.3986268518925,15.3974633018543,15.707963267949),
 .UNSPECIFIED.);
#1372=B_SPLINE_CURVE_WITH_KNOTS('',3,(#137342,#137343,#137344,#137345,#137346,
#137347,#137348,#137349),.UNSPECIFIED.,.F.,.F.,(4,1,1,1,1,4),(15.707963267949,
16.3962997518162,17.3951362017781,18.39397265174,19.3928091017018,19.7659327976564),
 .UNSPECIFIED.);
#1373=B_SPLINE_CURVE_WITH_KNOTS('',3,(#137355,#137356,#137357,#137358,#137359,
#137360,#137361,#137362),.UNSPECIFIED.,.F.,.F.,(4,1,1,1,1,4),(21.9911485751286,
22.854125184107,23.8529616340689,24.8517980840308,25.8506345339927,26.0493850849933),
 .UNSPECIFIED.);
#1374=B_SPLINE_CURVE_WITH_KNOTS('',3,(#137363,#137364,#137365,#137366,#137367,
#137368,#137369),.UNSPECIFIED.,.F.,.F.,(4,1,1,1,4),(19.7647623489133,19.8576158342214,
20.8564522841833,21.8552887341452,21.9911485751286),.UNSPECIFIED.);
#1375=B_SPLINE_CURVE_WITH_KNOTS('',3,(#137371,#137372,#137373,#137374,#137375,
#137376),.UNSPECIFIED.,.F.,.F.,(4,1,1,4),(19.7659327976564,20.3916455516637,
21.3904820016256,21.9911485751286),.UNSPECIFIED.);
#1376=B_SPLINE_CURVE_WITH_KNOTS('',3,(#137377,#137378,#137379,#137380,#137381,
#137382,#137383,#137384,#137385,#137386,#137387,#137388,#137389,#137390,
#137391,#137392,#137393,#137394,#137395,#137396,#137397,#137398,#137399,
#137400,#137401,#137402,#137403,#137404,#137405,#137406,#137407,#137408,
#137409,#137410,#137411,#137412,#137413,#137414,#137415,#137416,#137417,
#137418,#137419,#137420,#137421,#137422,#137423,#137424,#137425,#137426,
#137427,#137428,#137429,#137430,#137431,#137432,#137433,#137434,#137435,
#137436,#137437,#137438,#137439,#137440,#137441,#137442,#137443,#137444,
#137445,#137446,#137447,#137448,#137449,#137450,#137451,#137452,#137453,
#137454,#137455,#137456,#137457,#137458,#137459,#137460,#137461,#137462,
#137463,#137464,#137465,#137466,#137467,#137468,#137469,#137470,#137471,
#137472,#137473,#137474,#137475,#137476,#137477,#137478,#137479,#137480,
#137481,#137482,#137483,#137484,#137485,#137486,#137487,#137488,#137489,
#137490,#137491,#137492,#137493,#137494,#137495,#137496,#137497,#137498,
#137499,#137500),.UNSPECIFIED.,.F.,.F.,(4,3,3,3,3,3,3,3,3,3,3,3,3,3,3,3,
3,3,3,3,3,3,3,3,3,3,3,3,3,3,3,3,3,3,3,3,3,3,3,3,3,4),(21.9911487995803,
22.0999040794723,22.2090426325292,22.3187161977535,22.3893184515875,22.4879213239996,
22.5863838875782,22.6866052643246,22.7848896493686,22.8831410624577,22.9813889797561,
23.0830804602044,23.1814696586711,23.2848122801102,23.3881549015493,23.4867551943387,
23.5852151968621,23.6854372161932,23.7837191055958,23.8819680531268,23.9802135383925,
24.0819079916722,24.180294867534,24.2836431095226,24.3869913515112,24.4855869806887,
24.584042229485,24.6842654259835,24.7825423743751,24.8807863216562,24.9790267538739,
25.0807270157737,25.1791087577961,25.2824682796346,25.3858278014731,25.4844081036999,
25.582857277776,25.681205043018,25.7794880156384,25.8777310241197,25.9759959038317,
26.0480412469177),.UNSPECIFIED.);
#1377=B_SPLINE_CURVE_WITH_KNOTS('',3,(#137506,#137507,#137508,#137509,#137510,
#137511,#137512,#137513,#137514,#137515,#137516,#137517,#137518,#137519,
#137520,#137521,#137522,#137523,#137524,#137525,#137526,#137527,#137528,
#137529,#137530,#137531,#137532,#137533,#137534,#137535,#137536,#137537,
#137538,#137539,#137540,#137541,#137542,#137543,#137544,#137545,#137546,
#137547,#137548,#137549,#137550,#137551,#137552,#137553,#137554,#137555,
#137556,#137557,#137558,#137559,#137560,#137561,#137562,#137563,#137564,
#137565,#137566,#137567,#137568,#137569,#137570,#137571,#137572,#137573,
#137574,#137575,#137576,#137577,#137578,#137579,#137580,#137581,#137582,
#137583,#137584,#137585,#137586,#137587,#137588,#137589,#137590,#137591,
#137592,#137593,#137594,#137595,#137596,#137597,#137598,#137599,#137600,
#137601,#137602,#137603,#137604,#137605,#137606,#137607,#137608,#137609,
#137610,#137611,#137612,#137613,#137614,#137615,#137616,#137617,#137618,
#137619,#137620,#137621,#137622,#137623,#137624,#137625,#137626,#137627,
#137628,#137629),.UNSPECIFIED.,.F.,.F.,(4,3,3,3,3,3,3,3,3,3,3,3,3,3,3,3,
3,3,3,3,3,3,3,3,3,3,3,3,3,3,3,3,3,3,3,3,3,3,3,3,3,4),(28.2743338823082,
28.3746245106389,28.4749734038845,28.5754886320393,28.6760922702991,28.7769068624285,
28.8471438838783,28.9457420299505,29.0441998340411,29.144422396516,29.2427019760045,
29.3409485769573,29.4391916819654,29.5408888449341,29.6392732803233,29.7426268070817,
29.8459803338402,29.9445784592259,30.0430362424512,30.14325881012,30.2415383684582,
30.3397849482008,30.4380280319671,30.5397252199258,30.6381096342122,30.7414632090071,
30.844816783802,30.9434149029152,31.0418726796983,31.1420952489565,31.2403748004797,
31.3386213732828,31.4368644499936,31.5385616459362,31.6369460529487,31.7402996433563,
31.8436532337639,31.9422528703135,32.0406907036684,32.1390337581124,32.2373181769969,
32.331714806246),.UNSPECIFIED.);
#1378=B_SPLINE_CURVE_WITH_KNOTS('',3,(#137630,#137631,#137632,#137633,#137634,
#137635),.UNSPECIFIED.,.F.,.F.,(4,1,1,4),(26.0493850849933,26.8494709839545,
27.8483074339164,28.2743284148063),.UNSPECIFIED.);
#1379=B_SPLINE_CURVE_WITH_KNOTS('',3,(#137637,#137638,#137639,#137640,#137641,
#137642,#137643,#137644,#137645,#137646,#137647,#137648,#137649,#137650,
#137651,#137652,#137653,#137654,#137655,#137656,#137657,#137658,#137659,
#137660,#137661,#137662,#137663,#137664,#137665,#137666,#137667,#137668,
#137669,#137670,#137671,#137672,#137673,#137674,#137675,#137676,#137677,
#137678,#137679,#137680,#137681,#137682,#137683,#137684,#137685,#137686,
#137687,#137688,#137689,#137690,#137691,#137692,#137693,#137694,#137695,
#137696,#137697,#137698,#137699,#137700,#137701,#137702,#137703,#137704,
#137705,#137706,#137707,#137708,#137709),.UNSPECIFIED.,.F.,.F.,(4,3,3,3,
3,3,3,3,3,3,3,3,3,3,3,3,3,3,3,3,3,3,3,3,4),(26.0480412469177,26.1464094234963,
26.2448398572573,26.3434313033546,26.3846642514349,26.4832625887837,26.5817205899964,
26.6819431039214,26.7802228935228,26.8784697089924,26.976713032653,27.078409949839,
27.1767946120344,27.2801476567156,27.3835007013968,27.4808124357131,27.5800026165089,
27.6770619123618,27.7740624152157,27.8710350591815,27.971859764906,28.0689211638456,
28.1660361055543,28.2632831538734,28.2743338820794),.UNSPECIFIED.);
#1380=B_SPLINE_CURVE_WITH_KNOTS('',3,(#137710,#137711,#137712,#137713,#137714,
#137715,#137716,#137717,#137718,#137719,#137720,#137721,#137722,#137723,
#137724,#137725,#137726,#137727,#137728,#137729,#137730,#137731,#137732,
#137733,#137734,#137735,#137736,#137737,#137738,#137739,#137740,#137741,
#137742,#137743,#137744,#137745,#137746,#137747,#137748,#137749,#137750,
#137751,#137752,#137753,#137754,#137755,#137756,#137757,#137758,#137759,
#137760,#137761,#137762,#137763,#137764,#137765,#137766,#137767,#137768,
#137769,#137770,#137771,#137772,#137773,#137774,#137775,#137776,#137777,
#137778,#137779,#137780,#137781,#137782,#137783,#137784,#137785,#137786,
#137787,#137788,#137789,#137790,#137791,#137792,#137793,#137794,#137795,
#137796,#137797,#137798,#137799,#137800,#137801,#137802,#137803,#137804,
#137805,#137806,#137807,#137808,#137809,#137810,#137811,#137812,#137813,
#137814,#137815,#137816,#137817,#137818,#137819,#137820,#137821,#137822,
#137823,#137824,#137825,#137826,#137827,#137828,#137829,#137830,#137831,
#137832,#137833),.UNSPECIFIED.,.F.,.F.,(4,3,3,3,3,3,3,3,3,3,3,3,3,3,3,3,
3,3,3,3,3,3,3,3,3,3,3,3,3,3,3,3,3,3,3,3,3,3,3,3,3,4),(28.2743338823082,
28.3823371513587,28.480935409995,28.5793933278136,28.679615862002,28.7778955572416,
28.8761422744467,28.9743854960547,29.0760825223712,29.1744670740333,29.277820337677,
29.3811736013206,29.479771742719,29.5782295425603,29.6784521061506,29.7767316824742,
29.8749782806757,29.9732213833518,30.0749185503345,30.1733029844702,30.2766565178763,
30.3800100512824,30.4786081310924,30.5770658679195,30.6772884470851,30.7755679573387,
30.8738144884713,30.972057523165,31.0737547676848,31.1721391322403,31.2754928167423,
31.3788465012443,31.4774477473365,31.5759078066478,31.6742504130914,31.772528757936,
31.8707723648629,31.9690107165043,32.0673303009497,32.1656922449306,32.2642027658455,
32.3314303584533),.UNSPECIFIED.);
#1381=B_SPLINE_CURVE_WITH_KNOTS('',3,(#137839,#137840,#137841,#137842,#137843,
#137844,#137845,#137846,#137847,#137848,#137849,#137850,#137851,#137852,
#137853,#137854,#137855,#137856,#137857,#137858,#137859,#137860,#137861,
#137862,#137863,#137864,#137865,#137866,#137867,#137868,#137869,#137870,
#137871,#137872,#137873,#137874,#137875,#137876,#137877,#137878,#137879,
#137880,#137881,#137882,#137883,#137884,#137885,#137886,#137887,#137888,
#137889,#137890,#137891,#137892,#137893,#137894,#137895,#137896,#137897,
#137898,#137899,#137900,#137901,#137902,#137903,#137904,#137905,#137906,
#137907,#137908,#137909,#137910,#137911,#137912,#137913,#137914,#137915,
#137916,#137917,#137918,#137919,#137920,#137921,#137922,#137923,#137924,
#137925,#137926,#137927,#137928,#137929,#137930,#137931,#137932,#137933,
#137934,#137935,#137936,#137937,#137938,#137939,#137940,#137941,#137942,
#137943,#137944,#137945,#137946,#137947,#137948,#137949,#137950,#137951,
#137952,#137953,#137954,#137955,#137956,#137957,#137958,#137959,#137960,
#137961,#137962),.UNSPECIFIED.,.F.,.F.,(4,3,3,3,3,3,3,3,3,3,3,3,3,3,3,3,
3,3,3,3,3,3,3,3,3,3,3,3,3,3,3,3,3,3,3,3,3,3,3,3,3,4),(34.5575191897594,
34.6782345503606,34.8009387396023,34.8401625836495,34.9387607091287,35.0372184923872,
35.1374410600403,35.2357206182622,35.3339671978329,35.4322102813714,35.5339074694314,
35.6322918833521,35.7356454584817,35.8389990336114,35.9375971585481,36.0360549412581,
36.1362775090475,36.2345570667098,36.3328036457178,36.4310467286914,36.5327439174119,
36.631128330768,36.7344819071707,36.8378354835733,36.9364336084865,37.034891391171,
37.1351139589665,37.2333935165987,37.3316400955749,37.4298831785151,37.5315803672701,
37.629964780589,37.7333183570621,37.8366719335352,37.9352415778344,38.0336830992384,
38.1320262040958,38.2303004962045,38.3285627936546,38.4268127465241,38.5251372404893,
38.6142676701194),.UNSPECIFIED.);
#1382=B_SPLINE_CURVE_WITH_KNOTS('',3,(#137963,#137964,#137965,#137966,#137967,
#137968,#137969,#137970,#137971,#137972,#137973,#137974,#137975,#137976,
#137977,#137978,#137979,#137980,#137981,#137982,#137983,#137984,#137985,
#137986,#137987,#137988,#137989,#137990,#137991,#137992,#137993,#137994,
#137995,#137996,#137997,#137998,#137999,#138000,#138001,#138002,#138003,
#138004,#138005,#138006,#138007,#138008,#138009,#138010,#138011,#138012,
#138013,#138014,#138015,#138016,#138017,#138018,#138019,#138020,#138021,
#138022,#138023,#138024,#138025,#138026,#138027,#138028,#138029,#138030,
#138031,#138032,#138033,#138034,#138035),.UNSPECIFIED.,.F.,.F.,(4,3,3,3,
3,3,3,3,3,3,3,3,3,3,3,3,3,3,3,3,3,3,3,3,4),(32.331714806246,32.4299572859773,
32.5330903854144,32.6314723091546,32.7299238317575,32.8285286837753,32.8424896837258,
32.9410878085145,33.0395455910814,33.1397681589072,33.2380477164402,33.3362942953243,
33.4345373781797,33.5362345670567,33.6346189803101,33.7379725569989,33.8413261336877,
33.9390973941501,34.0367388270535,34.1342810926874,34.2317547370029,34.3292101035722,
34.4266554953253,34.5241539309012,34.5575191894878),.UNSPECIFIED.);
#1383=B_SPLINE_CURVE_WITH_KNOTS('',3,(#138037,#138038,#138039,#138040,#138041,
#138042,#138043,#138044,#138045,#138046,#138047,#138048,#138049,#138050,
#138051,#138052,#138053,#138054,#138055,#138056,#138057,#138058,#138059,
#138060,#138061,#138062,#138063,#138064,#138065,#138066,#138067,#138068,
#138069,#138070,#138071,#138072,#138073,#138074,#138075,#138076,#138077,
#138078,#138079,#138080,#138081,#138082,#138083,#138084,#138085,#138086,
#138087,#138088,#138089,#138090,#138091,#138092,#138093,#138094,#138095,
#138096,#138097,#138098,#138099,#138100,#138101,#138102,#138103,#138104,
#138105,#138106),.UNSPECIFIED.,.F.,.F.,(4,3,3,3,3,3,3,3,3,3,3,3,3,3,3,3,
3,3,3,3,3,3,3,4),(32.3314303584533,32.3776829512062,32.4762810765974,32.5747388598281,
32.6749614274956,32.7732409858386,32.8714875655859,32.9697306493566,33.0714278373095,
33.1698122515998,33.2731658263839,33.3765194011681,33.4751175203064,33.5735752971148,
33.6737978663667,33.7720774179164,33.8703239907463,33.9685670674843,34.0702642633957,
34.1686486704357,34.2720022607828,34.3753558511299,34.52385598093,34.5575191894878),
 .UNSPECIFIED.);
#1384=B_SPLINE_CURVE_WITH_KNOTS('',3,(#138107,#138108,#138109,#138110,#138111,
#138112,#138113,#138114),.UNSPECIFIED.,.F.,.F.,(4,1,1,1,1,4),(34.5575241472562,
35.3741923010918,36.3730287510537,37.3718652010156,38.3707016509774,38.6157831736331),
 .UNSPECIFIED.);
#1385=B_SPLINE_CURVE_WITH_KNOTS('',3,(#138120,#138121,#138122,#138123,#138124,
#138125,#138126,#138127,#138128,#138129,#138130,#138131,#138132,#138133,
#138134,#138135,#138136,#138137,#138138,#138139,#138140,#138141,#138142,
#138143,#138144,#138145,#138146,#138147,#138148,#138149,#138150,#138151,
#138152,#138153,#138154,#138155,#138156,#138157,#138158,#138159,#138160,
#138161,#138162,#138163,#138164,#138165,#138166,#138167,#138168,#138169,
#138170,#138171,#138172,#138173,#138174,#138175,#138176,#138177,#138178,
#138179,#138180,#138181,#138182,#138183,#138184,#138185,#138186,#138187,
#138188,#138189,#138190,#138191,#138192,#138193,#138194,#138195,#138196,
#138197,#138198,#138199,#138200,#138201,#138202,#138203,#138204,#138205,
#138206,#138207,#138208,#138209,#138210,#138211,#138212,#138213,#138214,
#138215,#138216,#138217,#138218,#138219,#138220,#138221,#138222,#138223,
#138224,#138225,#138226,#138227,#138228,#138229,#138230,#138231,#138232,
#138233,#138234,#138235,#138236,#138237,#138238,#138239,#138240,#138241,
#138242,#138243),.UNSPECIFIED.,.F.,.F.,(4,3,3,3,3,3,3,3,3,3,3,3,3,3,3,3,
3,3,3,3,3,3,3,3,3,3,3,3,3,3,3,3,3,3,3,3,3,3,3,3,3,4),(40.8407044969197,
40.93917053872,41.0374964280042,41.1368115911765,41.2349607512895,41.3330774110131,
41.4311912274065,41.5313978539005,41.6296531901077,41.7308354617452,41.8320177333826,
41.9306158583837,42.029073641158,42.1292962089313,42.2275757666567,42.3258223457274,
42.4240654287631,42.5257626174085,42.6241470308247,42.7275006070846,42.8308541833445,
42.929452308347,43.0279100911226,43.1281326588955,43.2264122166225,43.3246587956947,
43.4229018787318,43.5245990673755,43.622983480793,43.7263370570497,43.8296906333064,
43.9282887583114,44.0267465410897,44.126969108862,44.2252486665916,44.3234952456663,
44.4217383287063,44.5234355173468,44.621819930767,44.7251735070177,44.8285270832683,
44.8983979756935),.UNSPECIFIED.);
#1386=B_SPLINE_CURVE_WITH_KNOTS('',3,(#138244,#138245,#138246,#138247,#138248,
#138249,#138250,#138251,#138252,#138253,#138254,#138255,#138256,#138257,
#138258,#138259,#138260,#138261,#138262,#138263,#138264,#138265,#138266,
#138267,#138268,#138269,#138270,#138271,#138272,#138273,#138274,#138275,
#138276,#138277,#138278,#138279,#138280,#138281,#138282,#138283,#138284,
#138285,#138286,#138287,#138288,#138289,#138290,#138291,#138292,#138293,
#138294,#138295,#138296,#138297,#138298,#138299,#138300,#138301,#138302,
#138303,#138304,#138305,#138306,#138307,#138308,#138309,#138310,#138311,
#138312,#138313,#138314,#138315,#138316),.UNSPECIFIED.,.F.,.F.,(4,3,3,3,
3,3,3,3,3,3,3,3,3,3,3,3,3,3,3,3,3,3,3,3,4),(38.6142676701194,38.712710724348,
38.8113099394713,38.835508383497,38.9341065084864,39.0325642912488,39.132786859025,
39.2310664167387,39.3293129957977,39.4275560788219,39.5292532674811,39.6276376808858,
39.7309912571723,39.8343448334589,39.9329429584521,40.0314007412181,40.1316233089935,
40.2299028667104,40.3281494457725,40.4263925287994,40.5280897174548,40.6264741308618,
40.7298277071413,40.8331812834208,40.8407044966674),.UNSPECIFIED.);
#1387=B_SPLINE_CURVE_WITH_KNOTS('',3,(#138318,#138319,#138320,#138321,#138322,
#138323),.UNSPECIFIED.,.F.,.F.,(4,1,1,4),(38.6157831736331,39.3695381009393,
40.3683745509012,40.8407024149681),.UNSPECIFIED.);
#1388=B_SPLINE_CURVE_WITH_KNOTS('',3,(#138324,#138325,#138326,#138327,#138328,
#138329,#138330,#138331,#138332,#138333,#138334,#138335,#138336,#138337,
#138338,#138339,#138340,#138341,#138342,#138343,#138344,#138345,#138346,
#138347,#138348,#138349,#138350,#138351,#138352,#138353,#138354,#138355,
#138356,#138357,#138358,#138359,#138360,#138361,#138362,#138363,#138364,
#138365,#138366,#138367,#138368,#138369,#138370,#138371,#138372,#138373,
#138374,#138375,#138376,#138377,#138378,#138379,#138380,#138381,#138382,
#138383,#138384,#138385,#138386,#138387,#138388,#138389,#138390,#138391,
#138392,#138393,#138394,#138395,#138396,#138397,#138398,#138399,#138400,
#138401,#138402,#138403,#138404,#138405,#138406,#138407,#138408,#138409,
#138410,#138411,#138412,#138413,#138414,#138415,#138416,#138417,#138418,
#138419,#138420,#138421,#138422,#138423,#138424,#138425,#138426,#138427,
#138428,#138429,#138430,#138431,#138432,#138433,#138434,#138435,#138436,
#138437,#138438,#138439,#138440,#138441,#138442,#138443,#138444,#138445,
#138446,#138447,#138448,#138449,#138450),.UNSPECIFIED.,.F.,.F.,(4,3,3,3,
3,3,3,3,3,3,3,3,3,3,3,3,3,3,3,3,3,3,3,3,3,3,3,3,3,3,3,3,3,3,3,3,3,3,3,3,
3,3,4),(40.8407044966674,40.942531041993,41.0487010317105,41.1508691915792,
41.2531658485542,41.3556785603229,41.3672110008631,41.4658091258526,41.564266908615,
41.6644894763912,41.7627690341051,41.8610156131643,41.9592586961885,42.0609558848476,
42.1593402982524,42.2626938745386,42.3660474508249,42.4646455758181,42.5631033585841,
42.6633259263594,42.7616054840765,42.8598520631385,42.9580951461654,43.0597923348207,
43.1581767482279,43.2615303245073,43.3648839007868,43.4634820258002,43.5619398085867,
43.662162376357,43.7604419340952,43.8586885131789,43.9569315962276,44.0586287848578,
44.1570131982869,44.2603667745178,44.3637203507487,44.4623140220514,44.5607732131543,
44.6591152246742,44.7573894748763,44.8556332863477,44.8979423115668),
 .UNSPECIFIED.);
#1389=B_SPLINE_CURVE_WITH_KNOTS('',3,(#138456,#138457,#138458,#138459,#138460,
#138461,#138462,#138463),.UNSPECIFIED.,.F.,.F.,(4,1,1,1,1,4),(47.123889803847,
47.8250364331539,48.8238728831158,49.8227093330776,50.8215457830395,51.1819114106253),
 .UNSPECIFIED.);
#1390=B_SPLINE_CURVE_WITH_KNOTS('',3,(#138464,#138465,#138466,#138467,#138468,
#138469,#138470,#138471,#138472,#138473,#138474,#138475,#138476,#138477,
#138478,#138479,#138480,#138481,#138482,#138483,#138484,#138485,#138486,
#138487,#138488,#138489,#138490,#138491,#138492,#138493,#138494,#138495,
#138496,#138497,#138498,#138499,#138500,#138501,#138502,#138503,#138504,
#138505,#138506,#138507,#138508,#138509,#138510,#138511,#138512,#138513,
#138514,#138515,#138516,#138517,#138518,#138519,#138520,#138521,#138522,
#138523,#138524,#138525,#138526,#138527,#138528,#138529,#138530,#138531,
#138532,#138533),.UNSPECIFIED.,.F.,.F.,(4,3,3,3,3,3,3,3,3,3,3,3,3,3,3,3,
3,3,3,3,3,3,3,4),(44.8983979756935,44.9968932745396,45.0952715001835,45.1935673055801,
45.2918209691891,45.3900619829137,45.4883198179094,45.5866859593671,45.685113707856,
45.7837031830992,45.8273635332301,45.9259616582337,46.0244194410103,46.124642008783,
46.222921566511,46.3211681455842,46.4194112286227,46.521108417265,46.6194928306837,
46.7228464069379,46.826199983192,46.9466622822371,47.0654828012677,47.1238896269617),
 .UNSPECIFIED.);
#1391=B_SPLINE_CURVE_WITH_KNOTS('',3,(#138535,#138536,#138537,#138538,#138539,
#138540,#138541,#138542,#138543,#138544,#138545,#138546,#138547,#138548,
#138549,#138550,#138551,#138552,#138553,#138554,#138555,#138556,#138557,
#138558,#138559,#138560,#138561,#138562,#138563,#138564,#138565,#138566,
#138567,#138568,#138569,#138570,#138571,#138572,#138573,#138574,#138575,
#138576,#138577,#138578,#138579,#138580,#138581,#138582,#138583,#138584,
#138585,#138586,#138587,#138588,#138589,#138590,#138591,#138592,#138593,
#138594,#138595,#138596,#138597,#138598,#138599,#138600,#138601,#138602,
#138603,#138604),.UNSPECIFIED.,.F.,.F.,(4,3,3,3,3,3,3,3,3,3,3,3,3,3,3,3,
3,3,3,3,3,3,3,4),(44.8979423115668,44.996192512377,45.094546241849,45.1929542152813,
45.2915321477256,45.3625568007106,45.4611549257132,45.5596127084887,45.6598352762616,
45.7581148339886,45.8563614130607,45.9546044960983,46.0563016847418,46.1546860981594,
46.2580396744159,46.3613932506724,46.4587199838046,46.5559210250953,46.6530274701202,
46.750070296518,46.8471124553623,46.9441490048067,47.0412721236587,47.123889803847),
 .UNSPECIFIED.);
#1392=B_SPLINE_CURVE_WITH_KNOTS('',3,(#138605,#138606,#138607,#138608,#138609,
#138610,#138611,#138612),.UNSPECIFIED.,.F.,.F.,(4,1,1,1,1,4),(47.1238901027736,
47.3602297006343,48.3590661505962,49.3579026005581,50.3567390505199,51.1803882021177),
 .UNSPECIFIED.);
#1393=B_SPLINE_CURVE_WITH_KNOTS('',3,(#138618,#138619,#138620,#138621,#138622,
#138623,#138624,#138625,#138626,#138627,#138628,#138629,#138630,#138631,
#138632,#138633,#138634,#138635,#138636,#138637,#138638,#138639,#138640,
#138641,#138642,#138643,#138644,#138645,#138646,#138647,#138648,#138649,
#138650,#138651,#138652,#138653,#138654,#138655,#138656,#138657,#138658,
#138659,#138660,#138661,#138662,#138663,#138664,#138665,#138666,#138667,
#138668,#138669,#138670,#138671,#138672,#138673,#138674,#138675,#138676,
#138677,#138678,#138679,#138680,#138681,#138682,#138683,#138684,#138685,
#138686,#138687,#138688,#138689,#138690,#138691,#138692,#138693,#138694,
#138695,#138696,#138697,#138698,#138699,#138700,#138701,#138702,#138703,
#138704,#138705,#138706,#138707,#138708,#138709,#138710,#138711,#138712,
#138713,#138714,#138715,#138716,#138717,#138718,#138719,#138720,#138721,
#138722,#138723,#138724,#138725,#138726,#138727,#138728,#138729,#138730,
#138731,#138732,#138733,#138734,#138735,#138736,#138737,#138738,#138739,
#138740,#138741),.UNSPECIFIED.,.F.,.F.,(4,3,3,3,3,3,3,3,3,3,3,3,3,3,3,3,
3,3,3,3,3,3,3,3,3,3,3,3,3,3,3,3,3,3,3,3,3,3,3,3,3,4),(53.4070755243672,
53.5149520672774,53.6231638610727,53.7318758460234,53.8180551329251,53.9166532579288,
54.0151110407056,54.1153336084783,54.2136131662065,54.3118597452798,54.4101028283184,
54.5118000169605,54.6101844303793,54.7135380066332,54.816891582887,54.9154897078907,
55.0139474906675,55.1141700584402,55.2124496161683,55.3106961952417,55.4089392782802,
55.5106364669224,55.6090208803412,55.712374456595,55.8157280328489,55.9143261578525,
56.0127839406293,56.113006508402,56.2112860661301,56.3095326452035,56.407775728242,
56.5094729168842,56.607857330303,56.7112109065569,56.8145644828108,56.9131452274561,
57.0115945031595,57.1099420320482,57.208222759252,57.3064633876105,57.4047205556955,
57.463995981799),.UNSPECIFIED.);
#1394=B_SPLINE_CURVE_WITH_KNOTS('',3,(#138742,#138743,#138744,#138745,#138746,
#138747),.UNSPECIFIED.,.F.,.F.,(4,1,1,4),(51.1819114106253,51.8203822330014,
52.8192186829633,53.4070751110266),.UNSPECIFIED.);
#1395=B_SPLINE_CURVE_WITH_KNOTS('',3,(#138749,#138750,#138751,#138752,#138753,
#138754,#138755),.UNSPECIFIED.,.F.,.F.,(4,1,1,1,4),(51.1803882021177,51.3555755004818,
52.3544119504437,53.3532484004055,53.4070751110266),.UNSPECIFIED.);
#1396=B_SPLINE_CURVE_WITH_KNOTS('',3,(#138756,#138757,#138758,#138759,#138760,
#138761,#138762,#138763,#138764,#138765,#138766,#138767,#138768,#138769,
#138770,#138771,#138772,#138773,#138774,#138775,#138776,#138777,#138778,
#138779,#138780,#138781,#138782,#138783,#138784,#138785,#138786,#138787,
#138788,#138789,#138790,#138791,#138792,#138793,#138794,#138795,#138796,
#138797,#138798,#138799,#138800,#138801,#138802,#138803,#138804,#138805,
#138806,#138807,#138808,#138809,#138810,#138811,#138812,#138813,#138814,
#138815,#138816,#138817,#138818,#138819,#138820,#138821,#138822,#138823,
#138824,#138825,#138826,#138827,#138828,#138829,#138830,#138831,#138832,
#138833,#138834,#138835,#138836,#138837,#138838,#138839,#138840,#138841,
#138842,#138843,#138844,#138845,#138846,#138847,#138848,#138849,#138850,
#138851,#138852,#138853,#138854,#138855,#138856,#138857,#138858,#138859,
#138860,#138861,#138862,#138863,#138864,#138865,#138866,#138867,#138868,
#138869,#138870,#138871,#138872,#138873,#138874,#138875,#138876,#138877,
#138878,#138879,#138880,#138881,#138882),.UNSPECIFIED.,.F.,.F.,(4,3,3,3,
3,3,3,3,3,3,3,3,3,3,3,3,3,3,3,3,3,3,3,3,3,3,3,3,3,3,3,3,3,3,3,3,3,3,3,3,
3,3,4),(53.4070751110266,53.5048543854907,53.602498370777,53.7000367768844,
53.7975186210123,53.894974367796,53.9924344477701,54.0899931990352,54.1876041339862,
54.2853815723757,54.3520848503674,54.4506829753711,54.5491407581478,54.6493633259205,
54.7476428836486,54.8458894627221,54.9441325457605,55.0458297344027,55.1442141478216,
55.2475677240754,55.3509213003293,55.449519425333,55.5479772081098,55.6481997758825,
55.7464793336106,55.844725912684,55.9429689957225,56.0446661843647,56.1430505977836,
56.2464041740374,56.3497577502912,56.4483558752949,56.5468136580716,56.6470362258443,
56.7453157835724,56.8435623626458,56.9418054456842,57.0435026343264,57.1418870477453,
57.2452406239991,57.348594200253,57.4471969425917,57.4649113957591),
 .UNSPECIFIED.);
#1397=B_SPLINE_CURVE_WITH_KNOTS('',3,(#138888,#138889,#138890,#138891,#138892,
#138893,#138894,#138895),.UNSPECIFIED.,.F.,.F.,(4,1,1,1,1,4),(59.6902604182062,
59.8110738326964,60.8099102826583,61.8087467326201,62.807583182582,63.7472418296146),
 .UNSPECIFIED.);
#1398=B_SPLINE_CURVE_WITH_KNOTS('',3,(#138896,#138897,#138898,#138899,#138900,
#138901,#138902,#138903,#138904,#138905,#138906,#138907,#138908,#138909,
#138910,#138911,#138912,#138913,#138914,#138915,#138916,#138917,#138918,
#138919,#138920,#138921,#138922,#138923,#138924,#138925,#138926,#138927,
#138928,#138929,#138930,#138931,#138932,#138933,#138934,#138935,#138936,
#138937,#138938,#138939,#138940,#138941,#138942,#138943,#138944,#138945,
#138946,#138947,#138948,#138949,#138950,#138951,#138952,#138953,#138954,
#138955,#138956,#138957,#138958,#138959,#138960,#138961,#138962,#138963,
#138964,#138965),.UNSPECIFIED.,.F.,.F.,(4,3,3,3,3,3,3,3,3,3,3,3,3,3,3,3,
3,3,3,3,3,3,3,4),(57.463995981799,57.5623571755417,57.6607771836555,57.7593619848624,
57.8134009327726,57.9119990577763,58.010456840553,58.1106794083257,58.2089589660538,
58.3072055451272,58.4054486281657,58.5071458168079,58.6055302302267,58.7088838064806,
58.8122373827345,58.9094791608007,59.0070768179764,59.1040671063404,59.2009981633325,
59.2979009849178,59.3959908432399,59.4929780422907,59.5916192302484,59.6902604182062),
 .UNSPECIFIED.);
#1399=B_SPLINE_CURVE_WITH_KNOTS('',3,(#138967,#138968,#138969,#138970,#138971,
#138972,#138973,#138974,#138975,#138976,#138977,#138978,#138979,#138980,
#138981,#138982,#138983,#138984,#138985,#138986,#138987,#138988,#138989,
#138990,#138991,#138992,#138993,#138994,#138995,#138996,#138997,#138998,
#138999,#139000,#139001,#139002,#139003,#139004,#139005,#139006,#139007,
#139008,#139009,#139010,#139011,#139012,#139013,#139014,#139015,#139016,
#139017,#139018,#139019,#139020,#139021,#139022,#139023,#139024,#139025,
#139026,#139027,#139028,#139029,#139030,#139031,#139032,#139033),
 .UNSPECIFIED.,.F.,.F.,(4,3,3,3,3,3,3,3,3,3,3,3,3,3,3,3,3,3,3,3,3,3,4),
(57.4649113957591,57.5633474222124,57.6616774374564,57.7599497025695,57.8581937311631,
57.9564390020565,58.0547832942804,58.1531751948557,58.2517448810895,58.3474306502149,
58.4460287752185,58.5444865579955,58.6447091257682,58.7429886834964,58.8412352625699,
58.9394783456084,59.0411755342505,59.1395599476693,59.2429135239231,59.3462671001768,
59.4608829140302,59.5755716660047,59.6902604179793),.UNSPECIFIED.);
#1400=B_SPLINE_CURVE_WITH_KNOTS('',3,(#139034,#139035,#139036,#139037,#139038,
#139039,#139040,#139041,#139042,#139043,#139044,#139045,#139046,#139047,
#139048,#139049,#139050,#139051,#139052,#139053,#139054,#139055,#139056,
#139057,#139058,#139059,#139060,#139061,#139062,#139063,#139064,#139065,
#139066,#139067,#139068,#139069,#139070,#139071,#139072,#139073,#139074,
#139075,#139076,#139077,#139078,#139079,#139080,#139081,#139082,#139083,
#139084,#139085,#139086,#139087,#139088,#139089,#139090,#139091,#139092,
#139093,#139094,#139095,#139096,#139097,#139098,#139099,#139100,#139101,
#139102,#139103,#139104,#139105,#139106,#139107,#139108,#139109,#139110,
#139111,#139112,#139113,#139114,#139115,#139116,#139117,#139118,#139119,
#139120,#139121,#139122,#139123,#139124,#139125,#139126,#139127,#139128,
#139129,#139130,#139131,#139132,#139133,#139134,#139135,#139136,#139137,
#139138,#139139,#139140,#139141,#139142,#139143,#139144,#139145,#139146,
#139147,#139148,#139149,#139150,#139151,#139152,#139153,#139154,#139155,
#139156,#139157),.UNSPECIFIED.,.F.,.F.,(4,3,3,3,3,3,3,3,3,3,3,3,3,3,3,3,
3,3,3,3,3,3,3,3,3,3,3,3,3,3,3,3,3,3,3,3,3,3,3,3,3,4),(59.6902604182062,
59.7886341730559,59.8869985815967,59.985382791999,60.0838846667639,60.182449929213,
60.2811933482967,60.3451035501387,60.4437016751424,60.5421594579189,60.6423820256916,
60.7406615834198,60.8389081624931,60.9371512455316,61.0388484341738,61.1372328475927,
61.2405864238466,61.3439400001005,61.4425381251042,61.5409959078809,61.6412184756536,
61.7394980333817,61.8377446124552,61.9359876954936,62.0376848841358,62.1360692975546,
62.2394228738085,62.3427764500624,62.4413745750661,62.5398323578428,62.6400549256155,
62.7383344833436,62.836581062417,62.9348241454557,63.0365213340978,63.1349057475167,
63.2382593237705,63.3416129000243,63.4431811275695,63.5416227684091,63.644754289307,
63.7478858102049),.UNSPECIFIED.);
#1401=B_SPLINE_CURVE_WITH_KNOTS('',3,(#139163,#139164,#139165,#139166,#139167,
#139168,#139169,#139170,#139171,#139172,#139173,#139174,#139175,#139176,
#139177,#139178,#139179,#139180,#139181,#139182,#139183,#139184,#139185,
#139186,#139187,#139188,#139189,#139190,#139191,#139192,#139193,#139194,
#139195,#139196,#139197,#139198,#139199,#139200,#139201,#139202,#139203,
#139204,#139205,#139206,#139207,#139208,#139209,#139210,#139211,#139212,
#139213,#139214,#139215,#139216,#139217,#139218,#139219,#139220,#139221,
#139222,#139223,#139224,#139225,#139226,#139227,#139228,#139229,#139230,
#139231,#139232,#139233,#139234,#139235,#139236,#139237,#139238,#139239,
#139240,#139241,#139242,#139243,#139244,#139245,#139246,#139247,#139248,
#139249,#139250,#139251,#139252,#139253,#139254,#139255,#139256,#139257,
#139258,#139259,#139260,#139261,#139262,#139263,#139264,#139265,#139266,
#139267,#139268,#139269,#139270,#139271,#139272,#139273,#139274,#139275,
#139276,#139277,#139278,#139279,#139280,#139281,#139282,#139283,#139284,
#139285,#139286,#139287,#139288,#139289),.UNSPECIFIED.,.F.,.F.,(4,3,3,3,
3,3,3,3,3,3,3,3,3,3,3,3,3,3,3,3,3,3,3,3,3,3,3,3,3,3,3,3,3,3,3,3,3,3,3,3,
3,3,4),(65.9734457253857,66.0704340596177,66.1673127975357,66.2641328887558,
66.3609254267909,66.4577214670338,66.5546134226801,66.6515579893416,66.7486626585398,
66.8029289824295,66.9015271074333,66.9999848902101,67.1002074579827,67.1984870157109,
67.2967335947843,67.3949766778227,67.4966738664649,67.5950582798838,67.6984118561376,
67.8017654323914,67.9003635573951,67.998821340172,68.0990439079447,68.1973234656729,
68.2955700447463,68.3938131277847,68.4955103164269,68.5938947298456,68.6972483060994,
68.8006018823532,68.8992000073568,68.9976577901335,69.0978803579062,69.1961599156343,
69.2944064947076,69.3926495777462,69.4943467663884,69.5927311798071,69.6960847560611,
69.7994383323151,69.8980412657704,69.9964918402226,70.0313849607115),
 .UNSPECIFIED.);
#1402=B_SPLINE_CURVE_WITH_KNOTS('',3,(#139290,#139291,#139292,#139293,#139294,
#139295,#139296),.UNSPECIFIED.,.F.,.F.,(4,1,1,1,4),(63.7472418296146,63.8064196325439,
64.8052560825058,65.8040925324676,65.9734457253857),.UNSPECIFIED.);
#1403=B_SPLINE_CURVE_WITH_KNOTS('',3,(#139298,#139299,#139300,#139301,#139302,
#139303,#139304,#139305,#139306,#139307,#139308,#139309,#139310,#139311,
#139312,#139313,#139314,#139315,#139316,#139317,#139318,#139319,#139320,
#139321,#139322,#139323,#139324,#139325,#139326,#139327,#139328,#139329,
#139330,#139331,#139332,#139333,#139334,#139335,#139336,#139337,#139338,
#139339,#139340,#139341,#139342,#139343,#139344,#139345,#139346,#139347,
#139348,#139349,#139350,#139351,#139352,#139353,#139354,#139355,#139356,
#139357,#139358,#139359,#139360,#139361,#139362,#139363,#139364,#139365,
#139366,#139367),.UNSPECIFIED.,.F.,.F.,(4,3,3,3,3,3,3,3,3,3,3,3,3,3,3,3,
3,3,3,3,3,3,3,4),(63.7478858102049,63.8461305762455,63.9443750601028,64.0433936325736,
64.1417828323517,64.2411160911689,64.3404493499862,64.43904747499,64.5375052577664,
64.6377278255391,64.7360073832672,64.8342539623405,64.9324970453789,65.0341942340212,
65.1325786474399,65.235932223694,65.339285799948,65.4384637976082,65.53749807745,
65.6364173808604,65.7352455972605,65.8340208922139,65.932784900221,65.9734457253857),
 .UNSPECIFIED.);
#1404=B_SPLINE_CURVE_WITH_KNOTS('',3,(#139368,#139369,#139370,#139371,#139372,
#139373,#139374,#139375,#139376,#139377,#139378,#139379,#139380,#139381,
#139382,#139383,#139384,#139385,#139386,#139387,#139388,#139389,#139390,
#139391,#139392,#139393,#139394,#139395,#139396,#139397,#139398,#139399,
#139400,#139401,#139402,#139403,#139404,#139405,#139406,#139407,#139408,
#139409,#139410,#139411,#139412,#139413,#139414,#139415,#139416,#139417,
#139418,#139419,#139420,#139421,#139422,#139423,#139424,#139425,#139426,
#139427,#139428,#139429,#139430,#139431,#139432,#139433,#139434,#139435,
#139436,#139437,#139438,#139439,#139440,#139441,#139442,#139443,#139444,
#139445,#139446,#139447,#139448,#139449,#139450,#139451,#139452,#139453,
#139454,#139455,#139456,#139457,#139458,#139459,#139460,#139461,#139462,
#139463,#139464,#139465,#139466,#139467,#139468,#139469,#139470,#139471,
#139472,#139473,#139474,#139475,#139476,#139477,#139478,#139479,#139480,
#139481,#139482,#139483,#139484,#139485,#139486,#139487,#139488,#139489,
#139490,#139491),.UNSPECIFIED.,.F.,.F.,(4,3,3,3,3,3,3,3,3,3,3,3,3,3,3,3,
3,3,3,3,3,3,3,3,3,3,3,3,3,3,3,3,3,3,3,3,3,3,3,3,3,4),(65.9734457256204,
66.0848798050741,66.1968635637043,66.309495782683,66.3381222499099,66.4367203749136,
66.5351781576904,66.6354007254631,66.7336802831912,66.8319268622646,66.9301699453032,
67.0318671339454,67.1302515473642,67.233605123618,67.3369586998718,67.4355568248755,
67.5340146076523,67.6342371754249,67.7325167331531,67.8307633122265,67.929006395265,
68.0307035839072,68.129087997326,68.2324415735798,68.3357951498337,68.4343932748374,
68.5328510576141,68.6330736253868,68.7313531831149,68.8295997621883,68.9278428452268,
69.029540033869,69.1279244472878,69.2312780235416,69.3346315997955,69.4332079436462,
69.5316540255,69.6299995615592,69.7300684041619,69.8283147746266,69.9292948532983,
70.03027493197),.UNSPECIFIED.);
#1405=B_SPLINE_CURVE_WITH_KNOTS('',3,(#139497,#139498,#139499,#139500,#139501,
#139502,#139503,#139504),.UNSPECIFIED.,.F.,.F.,(4,1,1,1,1,4),(72.2566310325654,
72.7959476822007,73.7947841321626,74.7936205821245,75.7924570320864,76.313857464374),
 .UNSPECIFIED.);
#1406=B_SPLINE_CURVE_WITH_KNOTS('',3,(#139505,#139506,#139507,#139508,#139509,
#139510,#139511,#139512,#139513,#139514,#139515,#139516,#139517,#139518,
#139519,#139520,#139521,#139522,#139523,#139524,#139525,#139526,#139527,
#139528,#139529,#139530,#139531,#139532,#139533,#139534,#139535,#139536,
#139537,#139538,#139539,#139540,#139541,#139542,#139543,#139544,#139545,
#139546,#139547,#139548,#139549,#139550,#139551,#139552,#139553,#139554,
#139555,#139556,#139557,#139558,#139559,#139560,#139561,#139562,#139563,
#139564,#139565,#139566,#139567,#139568,#139569,#139570,#139571,#139572,
#139573,#139574),.UNSPECIFIED.,.F.,.F.,(4,3,3,3,3,3,3,3,3,3,3,3,3,3,3,3,
3,3,3,3,3,3,3,4),(70.0313849607115,70.1297027503805,70.2279679525357,70.3262100727843,
70.4244585865919,70.5228092852778,70.6212122199263,70.7197874411937,70.798274782277,
70.8968729072807,70.9953306900577,71.0955532578304,71.1938328155586,71.292079394632,
71.3903224776701,71.4920196663123,71.5904040797311,71.693757655985,71.7971112322389,
71.9028340905511,72.0081993817375,72.1133399321499,72.2181701837239,72.2566308185779),
 .UNSPECIFIED.);
#1407=B_SPLINE_CURVE_WITH_KNOTS('',3,(#139576,#139577,#139578,#139579,#139580,
#139581,#139582,#139583,#139584,#139585,#139586,#139587,#139588,#139589,
#139590,#139591,#139592,#139593,#139594,#139595,#139596,#139597,#139598,
#139599,#139600,#139601,#139602,#139603,#139604,#139605,#139606,#139607,
#139608,#139609,#139610,#139611,#139612,#139613,#139614,#139615,#139616,
#139617,#139618,#139619,#139620,#139621,#139622,#139623,#139624,#139625,
#139626,#139627,#139628,#139629,#139630,#139631,#139632,#139633,#139634,
#139635,#139636,#139637,#139638,#139639,#139640,#139641,#139642,#139643,
#139644,#139645),.UNSPECIFIED.,.F.,.F.,(4,3,3,3,3,3,3,3,3,3,3,3,3,3,3,3,
3,3,3,3,3,3,3,4),(70.03027493197,70.1286604602104,70.2310642549839,70.3334680497574,
70.4320661747611,70.5305239575378,70.6307465253105,70.7290260830386,70.827272662112,
70.9255157451505,71.0272129337927,71.1255973472115,71.2289509234654,71.3323044997193,
71.4298807240688,71.5273176349421,71.6246428433669,71.721908115062,71.8191441424516,
71.9163815796695,72.013708783522,72.1110862397604,72.2086145464311,72.2566310325654),
 .UNSPECIFIED.);
#1408=B_SPLINE_CURVE_WITH_KNOTS('',3,(#139646,#139647,#139648,#139649,#139650,
#139651,#139652,#139653),.UNSPECIFIED.,.F.,.F.,(4,1,1,1,1,4),(72.2566310325654,
72.3311409496812,73.329977399643,74.3288138496049,75.3276502995668,76.3138964218534),
 .UNSPECIFIED.);
#1409=B_SPLINE_CURVE_WITH_KNOTS('',3,(#139659,#139660,#139661,#139662,#139663,
#139664,#139665,#139666,#139667,#139668,#139669,#139670,#139671,#139672,
#139673,#139674,#139675,#139676,#139677,#139678,#139679,#139680,#139681,
#139682,#139683,#139684,#139685,#139686,#139687,#139688,#139689,#139690,
#139691,#139692,#139693,#139694,#139695,#139696,#139697,#139698,#139699,
#139700,#139701,#139702,#139703,#139704,#139705,#139706,#139707,#139708,
#139709,#139710,#139711,#139712,#139713,#139714,#139715,#139716,#139717,
#139718,#139719,#139720,#139721,#139722,#139723,#139724,#139725,#139726,
#139727,#139728,#139729,#139730,#139731,#139732,#139733,#139734,#139735,
#139736,#139737,#139738,#139739,#139740,#139741,#139742,#139743,#139744,
#139745,#139746,#139747,#139748,#139749,#139750,#139751,#139752,#139753,
#139754,#139755,#139756,#139757,#139758,#139759,#139760,#139761,#139762,
#139763,#139764,#139765,#139766,#139767,#139768,#139769,#139770,#139771,
#139772,#139773,#139774,#139775,#139776,#139777,#139778,#139779,#139780,
#139781,#139782),.UNSPECIFIED.,.F.,.F.,(4,3,3,3,3,3,3,3,3,3,3,3,3,3,3,3,
3,3,3,3,3,3,3,3,3,3,3,3,3,3,3,3,3,3,3,3,3,3,3,3,3,4),(78.5398164398184,
78.6677108218573,78.788966381972,78.8875645069757,78.9860222897525,79.0862448575251,
79.1845244152533,79.2827709943267,79.3810140773652,79.4827112660074,79.5810956794262,
79.6844492556801,79.7878028319339,79.8864009569376,79.9848587397143,80.085081307487,
80.1833608652152,80.2816074442885,80.379850527327,80.4815477159692,80.579932129388,
80.6832857056419,80.7866392818957,80.8852374068994,80.9836951896762,81.0839177574488,
81.182197315177,81.2804438942504,81.3786869772889,81.4803841659311,81.5787685793499,
81.6821221556037,81.7854757318576,81.8868624848001,81.9852993438176,82.0836395049705,
82.1819125670158,82.2801480566582,82.3784063425592,82.4766798090168,82.5750348041364,
82.5965697553975),.UNSPECIFIED.);
#1410=B_SPLINE_CURVE_WITH_KNOTS('',3,(#139783,#139784,#139785,#139786,#139787,
#139788),.UNSPECIFIED.,.F.,.F.,(4,1,1,4),(76.313857464374,76.7912934820482,
77.7901299320101,78.539816339745),.UNSPECIFIED.);
#1411=B_SPLINE_CURVE_WITH_KNOTS('',3,(#139790,#139791,#139792,#139793,#139794,
#139795,#139796),.UNSPECIFIED.,.F.,.F.,(4,1,1,1,4),(76.3138964218534,76.3264867495287,
77.3253231994905,78.3241596494524,78.539816339745),.UNSPECIFIED.);
#1412=B_SPLINE_CURVE_WITH_KNOTS('',3,(#139797,#139798,#139799,#139800,#139801,
#139802,#139803,#139804,#139805,#139806,#139807,#139808,#139809,#139810,
#139811,#139812,#139813,#139814,#139815,#139816,#139817,#139818,#139819,
#139820,#139821,#139822,#139823,#139824,#139825,#139826,#139827,#139828,
#139829,#139830,#139831,#139832,#139833,#139834,#139835,#139836,#139837,
#139838,#139839,#139840,#139841,#139842,#139843,#139844,#139845,#139846,
#139847,#139848,#139849,#139850,#139851,#139852,#139853,#139854,#139855,
#139856,#139857,#139858,#139859,#139860,#139861,#139862,#139863,#139864,
#139865,#139866,#139867,#139868,#139869,#139870,#139871,#139872,#139873,
#139874,#139875,#139876,#139877,#139878,#139879,#139880,#139881,#139882,
#139883,#139884,#139885,#139886,#139887,#139888,#139889,#139890,#139891,
#139892,#139893,#139894,#139895,#139896,#139897,#139898,#139899,#139900,
#139901,#139902,#139903,#139904,#139905,#139906,#139907,#139908,#139909,
#139910,#139911,#139912,#139913,#139914,#139915,#139916,#139917,#139918,
#139919,#139920),.UNSPECIFIED.,.F.,.F.,(4,3,3,3,3,3,3,3,3,3,3,3,3,3,3,3,
3,3,3,3,3,3,3,3,3,3,3,3,3,3,3,3,3,3,3,3,3,3,3,3,3,4),(78.539816339745,78.6377138097037,
78.7346673304385,78.831578691398,78.9284788661294,79.0271081744506,79.1241353185128,
79.2235657089636,79.3229960994143,79.421594224418,79.5200520071949,79.6202745749676,
79.7185541326958,79.8168007117691,79.9150437948075,80.0167409834497,80.1151253968685,
80.2184789731224,80.3218325493762,80.4204306743799,80.5188884571567,80.6191110249294,
80.7173905826575,80.8156371617308,80.9138802447693,81.0155774334115,81.1139618468302,
81.2173154230841,81.320668999338,81.4192671243417,81.5177249071184,81.6179474748911,
81.7162270326192,81.8144736116927,81.912716694731,82.0144138833732,82.112798296792,
82.2161518730459,82.3195054492999,82.4180964129928,82.516536214131,82.5977152967569),
 .UNSPECIFIED.);
#1413=B_SPLINE_CURVE_WITH_KNOTS('',3,(#139926,#139927,#139928,#139929,#139930,
#139931,#139932,#139933),.UNSPECIFIED.,.F.,.F.,(4,1,1,1,1,4),(84.8230070319889,
85.7808215317051,86.779657981667,87.7784944316289,88.7773308815907,88.8809435767746),
 .UNSPECIFIED.);
#1414=B_SPLINE_CURVE_WITH_KNOTS('',3,(#139934,#139935,#139936,#139937,#139938,
#139939,#139940,#139941,#139942,#139943,#139944,#139945,#139946,#139947,
#139948,#139949,#139950,#139951,#139952,#139953,#139954,#139955,#139956,
#139957,#139958,#139959,#139960,#139961,#139962,#139963,#139964,#139965,
#139966,#139967,#139968,#139969,#139970,#139971,#139972,#139973,#139974,
#139975,#139976,#139977,#139978,#139979,#139980,#139981,#139982,#139983,
#139984,#139985,#139986,#139987,#139988,#139989,#139990,#139991,#139992,
#139993,#139994,#139995,#139996,#139997,#139998,#139999,#140000,#140001,
#140002,#140003),.UNSPECIFIED.,.F.,.F.,(4,3,3,3,3,3,3,3,3,3,3,3,3,3,3,3,
3,3,3,3,3,3,3,4),(82.5965697553975,82.6951414213286,82.7843121818195,82.8829103068232,
82.9813680896,83.0815906573726,83.1798702151008,83.2781167941742,83.3763598772127,
83.4780570658549,83.5764414792737,83.6797950555275,83.7831486317814,83.8817467567851,
83.9802045395617,84.0804271073344,84.1787066650626,84.276953244136,84.3751963271744,
84.4768935158166,84.5752779292354,84.6786315054893,84.7819850817432,84.8230016469246),
 .UNSPECIFIED.);
#1415=B_SPLINE_CURVE_WITH_KNOTS('',3,(#140005,#140006,#140007,#140008,#140009,
#140010,#140011,#140012,#140013,#140014,#140015,#140016,#140017,#140018,
#140019,#140020,#140021,#140022,#140023,#140024,#140025,#140026,#140027,
#140028,#140029,#140030,#140031,#140032,#140033,#140034,#140035,#140036,
#140037,#140038,#140039,#140040,#140041,#140042,#140043,#140044,#140045,
#140046,#140047,#140048,#140049,#140050,#140051,#140052,#140053,#140054,
#140055,#140056,#140057,#140058,#140059,#140060,#140061,#140062,#140063,
#140064,#140065,#140066,#140067,#140068,#140069,#140070,#140071,#140072,
#140073,#140074),.UNSPECIFIED.,.F.,.F.,(4,3,3,3,3,3,3,3,3,3,3,3,3,3,3,3,
3,3,3,3,3,3,3,4),(82.5977152967569,82.6960046676817,82.794255337806,82.892496795247,
82.9907585104692,83.0891304667538,83.1875671193328,83.2861621863113,83.3183418992618,
83.4169400242654,83.5153978070423,83.615620374815,83.713899932543,83.8121465116164,
83.9103895946548,84.0120867832971,84.1104711967159,84.2138247729698,84.3171783492237,
84.420557830251,84.523654386749,84.6265834813182,84.7292989065994,84.8230016469246),
 .UNSPECIFIED.);
#1416=B_SPLINE_CURVE_WITH_KNOTS('',3,(#140075,#140076,#140077,#140078,#140079,
#140080,#140081,#140082,#140083,#140084,#140085,#140086,#140087,#140088,
#140089,#140090,#140091,#140092,#140093,#140094,#140095,#140096,#140097,
#140098,#140099,#140100,#140101,#140102,#140103,#140104,#140105,#140106,
#140107,#140108,#140109,#140110,#140111,#140112,#140113,#140114,#140115,
#140116,#140117,#140118,#140119,#140120,#140121,#140122,#140123,#140124,
#140125,#140126,#140127,#140128,#140129,#140130,#140131,#140132,#140133,
#140134,#140135,#140136,#140137,#140138,#140139,#140140,#140141,#140142,
#140143,#140144,#140145,#140146,#140147,#140148,#140149,#140150,#140151,
#140152,#140153,#140154,#140155,#140156,#140157,#140158,#140159,#140160,
#140161,#140162,#140163,#140164,#140165,#140166,#140167,#140168,#140169,
#140170,#140171,#140172,#140173,#140174,#140175,#140176,#140177,#140178,
#140179,#140180,#140181,#140182,#140183,#140184,#140185,#140186,#140187,
#140188,#140189,#140190,#140191,#140192,#140193,#140194,#140195,#140196,
#140197,#140198),.UNSPECIFIED.,.F.,.F.,(4,3,3,3,3,3,3,3,3,3,3,3,3,3,3,3,
3,3,3,3,3,3,3,3,3,3,3,3,3,3,3,3,3,3,3,3,3,3,3,3,3,4),(84.8230016472006,
84.9261861619503,85.029664796698,85.133294590709,85.2372126194223,85.3160147991855,
85.4146129241892,85.513070706966,85.6132932747387,85.7115728324668,85.8098194115402,
85.9080624945788,86.0097596832209,86.1081440966397,86.2114976728936,86.3148512491474,
86.4134493741511,86.5119071569278,86.6121297247005,86.7104092824287,86.8086558615021,
86.9068989445406,87.0085961331828,87.1069805466016,87.2103341228554,87.3136876991093,
87.412285824113,87.5107436068897,87.6109661746624,87.7092457323905,87.8074923114639,
87.9057353945024,88.0074325831446,88.1058169965634,88.2091705728173,88.3125241490712,
88.4111137865008,88.5095698168543,88.6079122101835,88.7061871882851,88.8044419893987,
88.8801389722626),.UNSPECIFIED.);
#1417=B_SPLINE_CURVE_WITH_KNOTS('',3,(#140204,#140205,#140206,#140207,#140208,
#140209,#140210,#140211,#140212,#140213,#140214,#140215,#140216,#140217,
#140218,#140219,#140220,#140221,#140222,#140223,#140224,#140225,#140226,
#140227,#140228,#140229,#140230,#140231,#140232,#140233,#140234,#140235,
#140236,#140237,#140238,#140239,#140240,#140241,#140242,#140243,#140244,
#140245,#140246,#140247,#140248,#140249,#140250,#140251,#140252,#140253,
#140254,#140255,#140256,#140257,#140258,#140259,#140260,#140261,#140262,
#140263,#140264,#140265,#140266,#140267,#140268,#140269,#140270,#140271,
#140272,#140273,#140274,#140275,#140276,#140277,#140278,#140279,#140280,
#140281,#140282,#140283,#140284,#140285,#140286,#140287,#140288,#140289,
#140290,#140291,#140292,#140293,#140294,#140295,#140296,#140297,#140298,
#140299,#140300,#140301,#140302,#140303,#140304,#140305,#140306,#140307,
#140308,#140309,#140310,#140311,#140312,#140313,#140314,#140315,#140316,
#140317,#140318,#140319,#140320,#140321,#140322,#140323,#140324,#140325,
#140326,#140327),.UNSPECIFIED.,.F.,.F.,(4,3,3,3,3,3,3,3,3,3,3,3,3,3,3,3,
3,3,3,3,3,3,3,3,3,3,3,3,3,3,3,3,3,3,3,3,3,3,3,3,3,4),(91.1061869541041,
91.2043419644769,91.3024795334306,91.4006291648835,91.4988897541851,91.5972075103073,
91.6957053368608,91.7738402314764,91.8724383564801,91.9708961392569,92.0711187070296,
92.1693982647577,92.2676448438311,92.3658879268697,92.4675851155118,92.5659695289307,
92.6693231051844,92.7726766814382,92.8712748064418,92.9697325892187,93.0699551569914,
93.1682347147194,93.2664812937929,93.3647243768315,93.4664215654736,93.5648059788925,
93.6681595551463,93.7715131314001,93.8701112564039,93.9685690391807,94.0687916069534,
94.1670711646815,94.2653177437549,94.3635608267936,94.4652580154357,94.5636424288545,
94.6669960051082,94.770349581362,94.8689185475017,94.9673651079953,95.0657083030438,
95.1638473593045),.UNSPECIFIED.);
#1418=B_SPLINE_CURVE_WITH_KNOTS('',3,(#140328,#140329,#140330,#140331,#140332,
#140333),.UNSPECIFIED.,.F.,.F.,(4,1,1,4),(88.8809435767746,89.7761673315526,
90.7750037815145,91.1061798190739),.UNSPECIFIED.);
#1419=B_SPLINE_CURVE_WITH_KNOTS('',3,(#140335,#140336,#140337,#140338,#140339,
#140340,#140341,#140342,#140343,#140344,#140345,#140346,#140347,#140348,
#140349,#140350,#140351,#140352,#140353,#140354,#140355,#140356,#140357,
#140358,#140359,#140360,#140361,#140362,#140363,#140364,#140365,#140366,
#140367,#140368,#140369,#140370,#140371,#140372,#140373,#140374,#140375,
#140376,#140377,#140378,#140379,#140380,#140381,#140382,#140383,#140384,
#140385,#140386,#140387,#140388,#140389,#140390,#140391,#140392,#140393,
#140394,#140395,#140396,#140397,#140398,#140399,#140400,#140401,#140402,
#140403,#140404,#140405,#140406,#140407),.UNSPECIFIED.,.F.,.F.,(4,3,3,3,
3,3,3,3,3,3,3,3,3,3,3,3,3,3,3,3,3,3,3,3,4),(88.8801389722626,88.9783988165887,
89.0767679991754,89.1752004281995,89.2737928157651,89.311360599033,89.4099587240367,
89.5084165068134,89.6086390745861,89.7069186323143,89.8051652113877,89.9034082944262,
90.0051054830683,90.1034898964872,90.206843472741,90.3101970489949,90.409695787095,
90.5067185530535,90.6036495481492,90.70051989818,90.801936662084,90.8988156754798,
90.9957205549588,91.0927209416413,91.1061869537961),.UNSPECIFIED.);
#1420=B_SPLINE_CURVE_WITH_KNOTS('',3,(#140408,#140409,#140410,#140411,#140412,
#140413,#140414,#140415,#140416,#140417,#140418,#140419,#140420,#140421,
#140422,#140423,#140424,#140425,#140426,#140427,#140428,#140429,#140430,
#140431,#140432,#140433,#140434,#140435,#140436,#140437,#140438,#140439,
#140440,#140441,#140442,#140443,#140444,#140445,#140446,#140447,#140448,
#140449,#140450,#140451,#140452,#140453,#140454,#140455,#140456,#140457,
#140458,#140459,#140460,#140461,#140462,#140463,#140464,#140465,#140466,
#140467,#140468,#140469,#140470,#140471,#140472,#140473,#140474,#140475,
#140476,#140477,#140478,#140479,#140480,#140481,#140482,#140483,#140484,
#140485,#140486,#140487,#140488,#140489,#140490,#140491,#140492,#140493,
#140494,#140495,#140496,#140497,#140498,#140499,#140500,#140501,#140502,
#140503,#140504,#140505,#140506,#140507,#140508,#140509,#140510,#140511,
#140512,#140513,#140514,#140515,#140516,#140517,#140518,#140519,#140520,
#140521,#140522,#140523,#140524,#140525,#140526,#140527,#140528,#140529,
#140530,#140531),.UNSPECIFIED.,.F.,.F.,(4,3,3,3,3,3,3,3,3,3,3,3,3,3,3,3,
3,3,3,3,3,3,3,3,3,3,3,3,3,3,3,3,3,3,3,3,3,3,3,3,3,4),(91.1061869541041,
91.2465035596788,91.3090334989568,91.4076316239605,91.5060894067373,91.6063119745099,
91.7045915322381,91.8028381113114,91.90108119435,92.0027783829921,92.1011627964109,
92.2045163726648,92.3078699489186,92.4064680739223,92.5049258566991,92.6051484244718,
92.7034279821999,92.8016745612733,92.8999176443119,93.001614832954,93.0999992463728,
93.2033528226267,93.3067063988805,93.4053045238842,93.5037623066609,93.6039848744336,
93.7022644321617,93.8005110112351,93.8987540942736,94.0004512829158,94.0988356963346,
94.2021892725885,94.3055428488424,94.4041508037225,94.502589190302,94.6009312472693,
94.6992065724876,94.7974446925382,94.8957159603398,94.9940021460021,95.0923959722183,
95.1629909762769),.UNSPECIFIED.);
#1421=B_SPLINE_CURVE_WITH_KNOTS('',3,(#140537,#140538,#140539,#140540,#140541,
#140542,#140543,#140544),.UNSPECIFIED.,.F.,.F.,(4,1,1,1,1,4),(97.389379769506,
97.7668589312476,98.7656953812095,99.7645318311714,100.763368281133,101.445902010813),
 .UNSPECIFIED.);
#1422=B_SPLINE_CURVE_WITH_KNOTS('',3,(#140545,#140546,#140547,#140548,#140549,
#140550,#140551,#140552,#140553,#140554,#140555,#140556,#140557,#140558,
#140559,#140560,#140561,#140562,#140563,#140564,#140565,#140566,#140567,
#140568,#140569,#140570,#140571,#140572,#140573,#140574,#140575,#140576,
#140577,#140578,#140579,#140580,#140581,#140582,#140583,#140584,#140585,
#140586,#140587,#140588,#140589,#140590,#140591,#140592,#140593,#140594,
#140595,#140596,#140597,#140598,#140599,#140600,#140601,#140602,#140603,
#140604,#140605,#140606,#140607,#140608,#140609,#140610,#140611,#140612,
#140613,#140614,#140615,#140616,#140617),.UNSPECIFIED.,.F.,.F.,(4,3,3,3,
3,3,3,3,3,3,3,3,3,3,3,3,3,3,3,3,3,3,3,3,4),(95.1638473593045,95.2620943271636,
95.3603371810261,95.4625493936005,95.5609329069904,95.6593867641743,95.7579931965668,
95.7691860313239,95.8677841563275,95.9662419391043,96.066464506877,96.1647440646051,
96.2629906436785,96.361233726717,96.4629309153592,96.5613153287779,96.6646689050318,
96.7680224812857,96.867499372579,96.9668292609829,97.0660403563902,97.1651524247998,
97.264207533224,97.3632407686273,97.3893722612837),.UNSPECIFIED.);
#1423=B_SPLINE_CURVE_WITH_KNOTS('',3,(#140619,#140620,#140621,#140622,#140623,
#140624,#140625,#140626,#140627,#140628,#140629,#140630,#140631,#140632,
#140633,#140634,#140635,#140636,#140637,#140638,#140639,#140640,#140641,
#140642,#140643,#140644,#140645,#140646,#140647,#140648,#140649,#140650,
#140651,#140652,#140653,#140654,#140655,#140656,#140657,#140658,#140659,
#140660,#140661,#140662,#140663,#140664,#140665,#140666,#140667,#140668,
#140669,#140670,#140671,#140672,#140673,#140674,#140675,#140676,#140677,
#140678,#140679,#140680,#140681,#140682,#140683,#140684,#140685,#140686,
#140687,#140688),.UNSPECIFIED.,.F.,.F.,(4,3,3,3,3,3,3,3,3,3,3,3,3,3,3,3,
3,3,3,3,3,3,3,4),(95.1629909762769,95.2615808559533,95.3043792988043,95.402977423808,
95.5014352065847,95.6016577743574,95.6999373320855,95.7981839111589,95.8964269941974,
95.9981241828396,96.0965085962583,96.1998621725122,96.3032157487661,96.4018138737698,
96.5002716565465,96.6004942243192,96.6987737820473,96.7970203611207,96.8952634441592,
96.9969606328014,97.0953450462202,97.1986986224741,97.302052198728,97.3893722612837),
 .UNSPECIFIED.);
#1424=B_SPLINE_CURVE_WITH_KNOTS('',3,(#140689,#140690,#140691,#140692,#140693,
#140694,#140695,#140696),.UNSPECIFIED.,.F.,.F.,(4,1,1,1,1,4),(97.3893809713061,
98.3008886486899,99.2997250986518,100.298561548614,101.297397998576,101.447496672416),
 .UNSPECIFIED.);
#1425=B_SPLINE_CURVE_WITH_KNOTS('',3,(#140702,#140703,#140704,#140705,#140706,
#140707,#140708,#140709,#140710,#140711,#140712,#140713,#140714,#140715,
#140716,#140717,#140718,#140719,#140720,#140721,#140722,#140723,#140724,
#140725,#140726,#140727,#140728,#140729,#140730,#140731,#140732,#140733,
#140734,#140735,#140736,#140737,#140738,#140739,#140740,#140741,#140742,
#140743,#140744,#140745,#140746,#140747,#140748,#140749,#140750,#140751,
#140752,#140753,#140754,#140755,#140756,#140757,#140758,#140759,#140760,
#140761,#140762,#140763,#140764,#140765,#140766,#140767,#140768,#140769,
#140770,#140771,#140772,#140773,#140774,#140775,#140776,#140777,#140778,
#140779,#140780,#140781,#140782,#140783,#140784,#140785,#140786,#140787,
#140788,#140789,#140790,#140791,#140792,#140793,#140794,#140795,#140796,
#140797,#140798,#140799,#140800,#140801,#140802,#140803,#140804,#140805,
#140806,#140807,#140808,#140809,#140810,#140811,#140812,#140813,#140814,
#140815,#140816,#140817,#140818,#140819,#140820,#140821,#140822,#140823,
#140824,#140825),.UNSPECIFIED.,.F.,.F.,(4,3,3,3,3,3,3,3,3,3,3,3,3,3,3,3,
3,3,3,3,3,3,3,3,3,3,3,3,3,3,3,3,3,3,3,3,3,3,3,3,3,4),(103.672557568463,
103.759877631019,103.858475756023,103.9569335388,104.057156106572,104.1554356643,
104.253682243374,104.351925326412,104.453622515055,104.552006928473,104.655360504727,
104.758714080981,104.857312205985,104.955769988761,105.055992556534,105.154272114262,
105.252518693336,105.350761776374,105.452458965016,105.550843378435,105.654196954689,
105.757550530943,105.856148655947,105.954606438723,106.054829006496,106.153108564224,
106.251355143297,106.349598226336,106.451295414978,106.549679828396,106.65303340465,
106.756386980904,106.854986798946,106.953445809625,107.051788768338,107.150068003062,
107.248313037023,107.346553353057,107.444881222511,107.543251670472,107.641785788201,
107.729756577966),.UNSPECIFIED.);
#1426=B_SPLINE_CURVE_WITH_KNOTS('',3,(#140826,#140827,#140828,#140829,#140830,
#140831),.UNSPECIFIED.,.F.,.F.,(4,1,1,4),(101.445902010813,101.762204731095,
102.761041181057,103.672548858934),.UNSPECIFIED.);
#1427=B_SPLINE_CURVE_WITH_KNOTS('',3,(#140833,#140834,#140835,#140836,#140837,
#140838),.UNSPECIFIED.,.F.,.F.,(4,1,1,4),(101.447496672416,102.296234448537,
103.295070898499,103.672550060693),.UNSPECIFIED.);
#1428=B_SPLINE_CURVE_WITH_KNOTS('',3,(#140839,#140840,#140841,#140842,#140843,
#140844,#140845,#140846,#140847,#140848,#140849,#140850,#140851,#140852,
#140853,#140854,#140855,#140856,#140857,#140858,#140859,#140860,#140861,
#140862,#140863,#140864,#140865,#140866,#140867,#140868,#140869,#140870,
#140871,#140872,#140873,#140874,#140875,#140876,#140877,#140878,#140879,
#140880,#140881,#140882,#140883,#140884,#140885,#140886,#140887,#140888,
#140889,#140890,#140891,#140892,#140893,#140894,#140895,#140896,#140897,
#140898,#140899,#140900,#140901,#140902,#140903,#140904,#140905,#140906,
#140907,#140908,#140909,#140910,#140911,#140912,#140913,#140914,#140915,
#140916,#140917,#140918,#140919,#140920,#140921,#140922,#140923,#140924,
#140925,#140926,#140927,#140928,#140929,#140930,#140931,#140932,#140933,
#140934,#140935,#140936,#140937,#140938,#140939,#140940,#140941,#140942,
#140943,#140944,#140945,#140946,#140947,#140948,#140949,#140950,#140951,
#140952,#140953,#140954,#140955,#140956,#140957,#140958,#140959,#140960,
#140961,#140962,#140963,#140964,#140965),.UNSPECIFIED.,.F.,.F.,(4,3,3,3,
3,3,3,3,3,3,3,3,3,3,3,3,3,3,3,3,3,3,3,3,3,3,3,3,3,3,3,3,3,3,3,3,3,3,3,3,
3,3,4),(103.672557568463,103.771601702603,103.870660322484,103.96976131202,
104.06899945985,104.168318657834,104.267812431338,104.293907348461,104.392505473465,
104.490963256242,104.591185824014,104.689465381742,104.787711960816,104.885955043854,
104.987652232496,105.086036645915,105.189390222169,105.292743798423,105.391341923427,
105.489799706204,105.590022273976,105.688301831704,105.786548410778,105.884791493816,
105.986488682458,106.084873095877,106.188226672131,106.291580248385,106.390178373389,
106.488636156165,106.588858723938,106.687138281666,106.78538486074,106.883627943778,
106.98532513242,107.083709545839,107.187063122093,107.290416698347,107.389023062568,
107.487464394916,107.585810440419,107.68408611143,107.730086449126),
 .UNSPECIFIED.);
#1429=B_SPLINE_CURVE_WITH_KNOTS('',3,(#140971,#140972,#140973,#140974,#140975,
#140976,#140977,#140978,#140979,#140980,#140981,#140982,#140983,#140984,
#140985,#140986,#140987,#140988,#140989,#140990,#140991,#140992,#140993,
#140994,#140995,#140996,#140997,#140998,#140999,#141000,#141001,#141002,
#141003,#141004,#141005,#141006,#141007,#141008,#141009,#141010,#141011,
#141012,#141013,#141014,#141015,#141016,#141017,#141018,#141019,#141020,
#141021,#141022,#141023,#141024,#141025,#141026,#141027,#141028,#141029,
#141030,#141031,#141032,#141033,#141034,#141035,#141036,#141037,#141038,
#141039,#141040,#141041,#141042,#141043,#141044,#141045,#141046,#141047,
#141048,#141049,#141050,#141051,#141052,#141053,#141054,#141055,#141056,
#141057,#141058,#141059,#141060,#141061,#141062,#141063,#141064,#141065,
#141066,#141067,#141068,#141069,#141070,#141071,#141072,#141073,#141074,
#141075,#141076,#141077,#141078,#141079,#141080,#141081,#141082,#141083,
#141084,#141085,#141086,#141087,#141088,#141089,#141090,#141091,#141092,
#141093,#141094,#141095,#141096,#141097),.UNSPECIFIED.,.F.,.F.,(4,3,3,3,
3,3,3,3,3,3,3,3,3,3,3,3,3,3,3,3,3,3,3,3,3,3,3,3,3,3,3,3,3,3,3,3,3,3,3,3,
3,3,4),(109.955742875951,110.055241614051,110.152151423466,110.249014842069,
110.345862894414,110.447330365999,110.544300028994,110.641334438529,110.738518045248,
110.751732780752,110.850330905756,110.948788688532,111.049011256305,111.147290814033,
111.245537393107,111.343780476145,111.445477664787,111.543862078206,111.64721565446,
111.750569230714,111.849167355718,111.947625138495,112.047847706267,112.146127263996,
112.244373843069,112.342616926107,112.44431411475,112.542698528168,112.646052104422,
112.749405680676,112.84800380568,112.946461588456,113.046684156229,113.144963713957,
113.24321029303,113.341453376069,113.443150564711,113.54153497813,113.644888554384,
113.748242130638,113.846836224879,113.945278284695,114.013656833936),
 .UNSPECIFIED.);
#1430=B_SPLINE_CURVE_WITH_KNOTS('',3,(#141098,#141099,#141100,#141101,#141102,
#141103,#141104,#141105,#141106,#141107,#141108,#141109,#141110,#141111,
#141112,#141113,#141114,#141115,#141116,#141117,#141118,#141119,#141120,
#141121,#141122,#141123,#141124,#141125,#141126,#141127,#141128,#141129,
#141130,#141131,#141132,#141133,#141134,#141135,#141136,#141137,#141138,
#141139,#141140,#141141,#141142,#141143,#141144,#141145,#141146,#141147,
#141148,#141149,#141150,#141151,#141152,#141153,#141154,#141155,#141156,
#141157,#141158,#141159,#141160,#141161,#141162,#141163,#141164,#141165,
#141166,#141167),.UNSPECIFIED.,.F.,.F.,(4,3,3,3,3,3,3,3,3,3,3,3,3,3,3,3,
3,3,3,3,3,3,3,4),(107.729756577966,107.755223430866,107.85382155587,107.952279338647,
108.052501906419,108.150781464147,108.249028043221,108.347271126259,108.448968314901,
108.54735272832,108.650706304574,108.754059880828,108.852658005832,108.951115788608,
109.051338356381,109.149617914109,109.247864493183,109.346107576221,109.447804764863,
109.546189178282,109.649542754536,109.75289633079,109.893212936358,109.955742875643),
 .UNSPECIFIED.);
#1431=B_SPLINE_CURVE_WITH_KNOTS('',3,(#141169,#141170,#141171,#141172,#141173,
#141174,#141175,#141176,#141177,#141178,#141179,#141180,#141181,#141182,
#141183,#141184,#141185,#141186,#141187,#141188,#141189,#141190,#141191,
#141192,#141193,#141194,#141195,#141196,#141197,#141198,#141199,#141200,
#141201,#141202,#141203,#141204,#141205,#141206,#141207,#141208,#141209,
#141210,#141211,#141212,#141213,#141214,#141215,#141216,#141217,#141218,
#141219,#141220,#141221,#141222,#141223,#141224,#141225,#141226,#141227,
#141228,#141229,#141230,#141231,#141232,#141233,#141234,#141235,#141236,
#141237,#141238),.UNSPECIFIED.,.F.,.F.,(4,3,3,3,3,3,3,3,3,3,3,3,3,3,3,3,
3,3,3,3,3,3,3,4),(107.730086449126,107.828327813024,107.926578911936,108.024934198482,
108.123344723364,108.221924067715,108.289253148309,108.387851273313,108.48630905609,
108.586531623862,108.684811181591,108.783057760664,108.881300843703,108.982998032345,
109.081382445763,109.184736022017,109.288089598271,109.386591328535,109.484956309733,
109.583214317042,109.681399820024,109.779540599734,109.877698313765,109.955742875643),
 .UNSPECIFIED.);
#1432=B_SPLINE_CURVE_WITH_KNOTS('',3,(#141239,#141240,#141241,#141242,#141243,
#141244,#141245,#141246),.UNSPECIFIED.,.F.,.F.,(4,1,1,1,1,4),(109.955750010087,
110.286926048232,111.285762498194,112.284598948156,113.283435398118,114.012186970914),
 .UNSPECIFIED.);
#1433=B_SPLINE_CURVE_WITH_KNOTS('',3,(#141252,#141253,#141254,#141255,#141256,
#141257,#141258,#141259,#141260,#141261,#141262,#141263,#141264,#141265,
#141266,#141267,#141268,#141269,#141270,#141271,#141272,#141273,#141274,
#141275,#141276,#141277,#141278,#141279,#141280,#141281,#141282,#141283,
#141284,#141285,#141286,#141287,#141288,#141289,#141290,#141291,#141292,
#141293,#141294,#141295,#141296,#141297,#141298,#141299,#141300,#141301,
#141302,#141303,#141304,#141305,#141306,#141307,#141308,#141309,#141310,
#141311,#141312,#141313,#141314,#141315,#141316,#141317,#141318,#141319,
#141320,#141321,#141322,#141323,#141324,#141325,#141326,#141327,#141328,
#141329,#141330,#141331,#141332,#141333,#141334,#141335,#141336,#141337,
#141338,#141339,#141340,#141341,#141342,#141343,#141344,#141345,#141346,
#141347,#141348,#141349,#141350,#141351,#141352,#141353,#141354,#141355,
#141356,#141357,#141358,#141359,#141360,#141361,#141362,#141363,#141364,
#141365,#141366,#141367,#141368,#141369,#141370,#141371,#141372,#141373,
#141374,#141375),.UNSPECIFIED.,.F.,.F.,(4,3,3,3,3,3,3,3,3,3,3,3,3,3,3,3,
3,3,3,3,3,3,3,3,3,3,3,3,3,3,3,3,3,3,3,3,3,3,3,3,3,4),(116.238928182823,
116.341566510357,116.44447107289,116.547509821617,116.650828963887,116.744751480523,
116.843349605527,116.941807388303,117.042029956076,117.140309513804,117.238556092878,
117.336799175916,117.438496364558,117.536880777977,117.640234354231,117.743587930485,
117.842186055489,117.940643838266,118.040866406038,118.139145963766,118.23739254284,
118.335635625878,118.437332814521,118.535717227939,118.639070804193,118.742424380447,
118.841022505451,118.939480288228,119.039702856,119.137982413728,119.236228992802,
119.33447207584,119.436169264482,119.534553677901,119.637907254155,119.741260830409,
119.839851983055,119.9383091947,120.03665133111,120.134925920017,120.2331760742,
120.296103423185),.UNSPECIFIED.);
#1434=B_SPLINE_CURVE_WITH_KNOTS('',3,(#141376,#141377,#141378,#141379,#141380,
#141381,#141382,#141383,#141384,#141385,#141386,#141387,#141388,#141389,
#141390,#141391,#141392,#141393,#141394,#141395,#141396,#141397,#141398,
#141399,#141400,#141401,#141402,#141403,#141404,#141405,#141406,#141407,
#141408,#141409,#141410,#141411,#141412,#141413,#141414,#141415,#141416,
#141417,#141418,#141419,#141420,#141421,#141422,#141423,#141424,#141425,
#141426,#141427,#141428,#141429,#141430,#141431,#141432,#141433,#141434,
#141435,#141436,#141437,#141438,#141439,#141440,#141441,#141442,#141443,
#141444,#141445),.UNSPECIFIED.,.F.,.F.,(4,3,3,3,3,3,3,3,3,3,3,3,3,3,3,3,
3,3,3,3,3,3,3,4),(114.013656833936,114.111953411531,114.210207448244,114.308448436441,
114.406705847382,114.505071337775,114.603498076973,114.702086932435,114.747078580599,
114.845676705603,114.94413448838,115.044357056152,115.14263661388,115.240883192954,
115.339126275992,115.440823464634,115.539207878053,115.642561454307,115.745915030561,
115.84988875933,115.953561696348,116.057054365164,116.160309146371,116.238928182547),
 .UNSPECIFIED.);
#1435=B_SPLINE_CURVE_WITH_KNOTS('',3,(#141447,#141448,#141449,#141450,#141451,
#141452),.UNSPECIFIED.,.F.,.F.,(4,1,1,4),(114.012186970914,114.28227184808,
115.281108298042,116.2389227975),.UNSPECIFIED.);
#1436=B_SPLINE_CURVE_WITH_KNOTS('',3,(#141453,#141454,#141455,#141456,#141457,
#141458,#141459,#141460,#141461,#141462,#141463,#141464,#141465,#141466,
#141467,#141468,#141469,#141470,#141471,#141472,#141473,#141474,#141475,
#141476,#141477,#141478,#141479,#141480,#141481,#141482,#141483,#141484,
#141485,#141486,#141487,#141488,#141489,#141490,#141491,#141492,#141493,
#141494,#141495,#141496,#141497,#141498,#141499,#141500,#141501,#141502,
#141503,#141504,#141505,#141506,#141507,#141508,#141509,#141510,#141511,
#141512,#141513,#141514,#141515,#141516,#141517,#141518,#141519,#141520,
#141521,#141522,#141523,#141524,#141525,#141526,#141527,#141528,#141529,
#141530,#141531,#141532,#141533,#141534,#141535,#141536,#141537,#141538,
#141539,#141540,#141541,#141542,#141543,#141544,#141545,#141546,#141547,
#141548,#141549,#141550,#141551,#141552,#141553,#141554,#141555,#141556,
#141557,#141558,#141559,#141560,#141561,#141562,#141563,#141564,#141565,
#141566,#141567,#141568,#141569,#141570,#141571,#141572,#141573,#141574,
#141575,#141576,#141577,#141578,#141579),.UNSPECIFIED.,.F.,.F.,(4,3,3,3,
3,3,3,3,3,3,3,3,3,3,3,3,3,3,3,3,3,3,3,3,3,3,3,3,3,3,3,3,3,3,3,3,3,3,3,3,
3,3,4),(116.238928182823,116.279944748004,116.378542873008,116.477000655784,
116.577223223557,116.675502781285,116.773749360358,116.871992443397,116.973689632039,
117.072074045458,117.175427621712,117.278781197966,117.37737932297,117.475837105746,
117.576059673519,117.674339231247,117.77258581032,117.870828893359,117.972526082001,
118.07091049542,118.174264071673,118.277617647927,118.376215772931,118.474673555707,
118.57489612348,118.673175681208,118.771422260282,118.86966534332,118.971362531962,
119.069746945381,119.173100521635,119.276454097889,119.375052222893,119.47351000567,
119.573732573442,119.67201213117,119.770258710244,119.868501793282,119.970198981924,
120.068583395343,120.171936971597,120.275290547851,120.296396941981),
 .UNSPECIFIED.);
#1437=B_SPLINE_CURVE_WITH_KNOTS('',3,(#141585,#141586,#141587,#141588,#141589,
#141590,#141591,#141592),.UNSPECIFIED.,.F.,.F.,(4,1,1,1,1,4),(122.522113490002,
122.737770180294,123.736606630256,124.735443080218,125.73427953018,126.578666843287),
 .UNSPECIFIED.);
#1438=B_SPLINE_CURVE_WITH_KNOTS('',3,(#141593,#141594,#141595,#141596,#141597,
#141598,#141599,#141600,#141601,#141602,#141603,#141604,#141605,#141606,
#141607,#141608,#141609,#141610,#141611,#141612,#141613,#141614,#141615,
#141616,#141617,#141618,#141619,#141620,#141621,#141622,#141623,#141624,
#141625,#141626,#141627,#141628,#141629,#141630,#141631,#141632,#141633,
#141634,#141635,#141636,#141637,#141638,#141639,#141640,#141641,#141642,
#141643,#141644,#141645,#141646,#141647,#141648,#141649,#141650,#141651,
#141652,#141653,#141654,#141655,#141656,#141657,#141658,#141659,#141660,
#141661,#141662),.UNSPECIFIED.,.F.,.F.,(4,3,3,3,3,3,3,3,3,3,3,3,3,3,3,3,
3,3,3,3,3,3,3,4),(120.296103423185,120.394359176955,120.492722088099,120.591144801905,
120.689731215843,120.740097280371,120.838695405375,120.937153188151,121.037375755924,
121.135655313652,121.233901892726,121.332144975764,121.433842164406,121.532226577825,
121.635580154079,121.738933730333,121.836831200292,121.933909156543,122.030894120917,
122.127817176647,122.226391254986,122.323316910845,122.422715200423,122.522113490002),
 .UNSPECIFIED.);
#1439=B_SPLINE_CURVE_WITH_KNOTS('',3,(#141664,#141665,#141666,#141667,#141668,
#141669,#141670,#141671,#141672,#141673,#141674,#141675,#141676,#141677,
#141678,#141679,#141680,#141681,#141682,#141683,#141684,#141685,#141686,
#141687,#141688,#141689,#141690,#141691,#141692,#141693,#141694,#141695,
#141696,#141697,#141698,#141699,#141700,#141701,#141702,#141703,#141704,
#141705,#141706,#141707,#141708,#141709,#141710,#141711,#141712,#141713,
#141714,#141715,#141716,#141717,#141718,#141719,#141720,#141721,#141722,
#141723,#141724,#141725,#141726,#141727,#141728,#141729,#141730),
 .UNSPECIFIED.,.F.,.F.,(4,3,3,3,3,3,3,3,3,3,3,3,3,3,3,3,3,3,3,3,3,3,4),
(120.296396941981,120.394962276094,120.493394302568,120.591721864652,120.689992682742,
120.788236268825,120.886482101004,120.984827578214,121.083221565444,121.18179225211,
121.274126997813,121.372725122817,121.471182905594,121.571405473366,121.669685031094,
121.767931610168,121.866174693206,121.967871881848,122.066256295267,122.169609871521,
122.272963447775,122.40085782982,122.522113389975),.UNSPECIFIED.);
#1440=B_SPLINE_CURVE_WITH_KNOTS('',3,(#141731,#141732,#141733,#141734,#141735,
#141736,#141737,#141738),.UNSPECIFIED.,.F.,.F.,(4,1,1,1,1,4),(122.522113490002,
123.271799897737,124.270636347699,125.26947279766,126.268309247622,126.580285776533),
 .UNSPECIFIED.);
#1441=B_SPLINE_CURVE_WITH_KNOTS('',3,(#141744,#141745,#141746,#141747,#141748,
#141749,#141750,#141751,#141752,#141753,#141754,#141755,#141756,#141757,
#141758,#141759,#141760,#141761,#141762,#141763,#141764,#141765,#141766,
#141767,#141768,#141769,#141770,#141771,#141772,#141773,#141774,#141775,
#141776,#141777,#141778,#141779,#141780,#141781,#141782,#141783,#141784,
#141785,#141786,#141787,#141788,#141789,#141790,#141791,#141792,#141793,
#141794,#141795,#141796,#141797,#141798,#141799,#141800,#141801,#141802,
#141803,#141804,#141805,#141806,#141807,#141808,#141809,#141810,#141811,
#141812,#141813,#141814,#141815,#141816,#141817,#141818,#141819,#141820,
#141821,#141822,#141823,#141824,#141825,#141826,#141827,#141828,#141829,
#141830,#141831,#141832,#141833,#141834,#141835,#141836,#141837,#141838,
#141839,#141840,#141841,#141842,#141843,#141844,#141845,#141846,#141847,
#141848,#141849,#141850,#141851,#141852,#141853,#141854,#141855,#141856,
#141857,#141858,#141859,#141860,#141861,#141862,#141863,#141864,#141865,
#141866,#141867,#141868,#141869,#141870),.UNSPECIFIED.,.F.,.F.,(4,3,3,3,
3,3,3,3,3,3,3,3,3,3,3,3,3,3,3,3,3,3,3,3,3,3,3,3,3,3,3,3,3,3,3,3,3,3,3,3,
3,3,4),(128.805298797182,128.902840431273,129.000250613517,129.097560812666,
129.194818343698,129.292053887498,129.389298094495,129.486642967569,129.584044330746,
129.681605924981,129.729625330028,129.828223455032,129.926681237808,130.026903805581,
130.125183363309,130.223429942382,130.321673025421,130.423370214063,130.521754627481,
130.625108203735,130.728461779989,130.827059904993,130.925517687769,131.025740255542,
131.12401981327,131.222266392343,131.320509475382,131.422206664024,131.520591077443,
131.623944653697,131.727298229951,131.825896354955,131.924354137732,132.024576705504,
132.122856263232,132.221102842306,132.319345925344,132.421043113986,132.519427527405,
132.622781103659,132.726134679913,132.824726637196,132.863178396459),
 .UNSPECIFIED.);
#1442=B_SPLINE_CURVE_WITH_KNOTS('',3,(#141871,#141872,#141873,#141874,#141875,
#141876,#141877),.UNSPECIFIED.,.F.,.F.,(4,1,1,1,4),(126.578666843287,126.733115980142,
127.731952430104,128.730788880066,128.805298797182),.UNSPECIFIED.);
#1443=B_SPLINE_CURVE_WITH_KNOTS('',3,(#141879,#141880,#141881,#141882,#141883,
#141884),.UNSPECIFIED.,.F.,.F.,(4,1,1,4),(126.580285776533,127.267145697584,
128.265982147546,128.805298797182),.UNSPECIFIED.);
#1444=B_SPLINE_CURVE_WITH_KNOTS('',3,(#141885,#141886,#141887,#141888,#141889,
#141890,#141891,#141892,#141893,#141894,#141895,#141896,#141897,#141898,
#141899,#141900,#141901,#141902,#141903,#141904,#141905,#141906,#141907,
#141908,#141909,#141910,#141911,#141912,#141913,#141914,#141915,#141916,
#141917,#141918,#141919,#141920,#141921,#141922,#141923,#141924,#141925,
#141926,#141927,#141928,#141929,#141930,#141931,#141932,#141933,#141934,
#141935,#141936,#141937,#141938,#141939,#141940,#141941,#141942,#141943,
#141944,#141945,#141946,#141947,#141948,#141949,#141950,#141951,#141952,
#141953,#141954,#141955,#141956,#141957,#141958,#141959,#141960,#141961,
#141962,#141963,#141964,#141965,#141966,#141967,#141968,#141969,#141970,
#141971,#141972,#141973,#141974,#141975,#141976,#141977,#141978,#141979,
#141980,#141981,#141982,#141983,#141984,#141985,#141986,#141987,#141988,
#141989,#141990,#141991,#141992,#141993,#141994,#141995,#141996,#141997,
#141998,#141999,#142000,#142001,#142002,#142003,#142004,#142005,#142006,
#142007,#142008),.UNSPECIFIED.,.F.,.F.,(4,3,3,3,3,3,3,3,3,3,3,3,3,3,3,3,
3,3,3,3,3,3,3,3,3,3,3,3,3,3,3,3,3,3,3,3,3,3,3,3,3,4),(128.805299011159,
128.91008561987,129.01525575915,129.120630109632,129.226318351047,129.264818597508,
129.363416722512,129.461874505288,129.562097073061,129.660376630789,129.758623209863,
129.856866292901,129.958563481543,130.056947894962,130.160301471216,130.26365504747,
130.362253172474,130.460710955251,130.560933523023,130.659213080751,130.757459659825,
130.855702742863,130.957399931506,131.055784344924,131.159137921178,131.262491497432,
131.361089622436,131.459547405212,131.559769972985,131.658049530713,131.756296109787,
131.854539192825,131.956236381467,132.054620794886,132.15797437114,132.261327947394,
132.359913784698,132.458366887932,132.559360493572,132.657635696798,132.759988503645,
132.862341310493),.UNSPECIFIED.);
#1445=B_SPLINE_CURVE_WITH_KNOTS('',3,(#142014,#142015,#142016,#142017,#142018,
#142019,#142020,#142021,#142022,#142023,#142024,#142025,#142026,#142027,
#142028,#142029,#142030,#142031,#142032,#142033,#142034,#142035,#142036,
#142037,#142038,#142039,#142040,#142041,#142042,#142043,#142044,#142045,
#142046,#142047,#142048,#142049,#142050,#142051,#142052,#142053,#142054,
#142055,#142056,#142057,#142058,#142059,#142060,#142061,#142062,#142063,
#142064,#142065,#142066,#142067,#142068,#142069,#142070,#142071,#142072,
#142073,#142074,#142075,#142076,#142077,#142078,#142079,#142080,#142081,
#142082,#142083,#142084,#142085,#142086,#142087,#142088,#142089,#142090,
#142091,#142092,#142093,#142094,#142095,#142096,#142097,#142098,#142099,
#142100,#142101,#142102,#142103,#142104,#142105,#142106,#142107,#142108,
#142109,#142110,#142111,#142112,#142113,#142114,#142115,#142116,#142117,
#142118,#142119,#142120,#142121,#142122,#142123,#142124,#142125,#142126,
#142127,#142128,#142129,#142130,#142131,#142132,#142133,#142134,#142135,
#142136,#142137,#142138,#142139,#142140),.UNSPECIFIED.,.F.,.F.,(4,3,3,3,
3,3,3,3,3,3,3,3,3,3,3,3,3,3,3,3,3,3,3,3,3,3,3,3,3,3,3,3,3,3,3,3,3,3,3,3,
3,3,4),(135.088484104361,135.187254556185,135.286029876604,135.384838499174,
135.483776463585,135.582788468008,135.681976179005,135.722644029799,135.821242154803,
135.919699937579,136.019922505352,136.11820206308,136.216448642154,136.314691725192,
136.416388913834,136.514773327253,136.618126903507,136.721480479761,136.820078604765,
136.918536387542,137.018758955314,137.117038513042,137.215285092116,137.313528175154,
137.415225363796,137.513609777215,137.616963353469,137.720316929723,137.818915054727,
137.917372837503,138.017595405276,138.115874963004,138.214121542077,138.312364625116,
138.414061813758,138.512446227176,138.61579980343,138.719153379684,138.817761602491,
138.916204188037,139.0145513523,139.112826031211,139.146050636314),
 .UNSPECIFIED.);
#1446=B_SPLINE_CURVE_WITH_KNOTS('',3,(#142141,#142142,#142143,#142144,#142145,
#142146,#142147,#142148,#142149,#142150,#142151,#142152,#142153,#142154,
#142155,#142156,#142157,#142158,#142159,#142160,#142161,#142162,#142163,
#142164,#142165,#142166,#142167,#142168,#142169,#142170,#142171,#142172,
#142173,#142174,#142175,#142176,#142177,#142178,#142179,#142180,#142181,
#142182,#142183,#142184,#142185,#142186,#142187,#142188,#142189,#142190,
#142191,#142192,#142193,#142194,#142195,#142196,#142197,#142198,#142199,
#142200,#142201,#142202,#142203,#142204,#142205,#142206,#142207,#142208,
#142209,#142210),.UNSPECIFIED.,.F.,.F.,(4,3,3,3,3,3,3,3,3,3,3,3,3,3,3,3,
3,3,3,3,3,3,3,4),(132.863178396459,132.961590313953,133.059905719281,133.15816959061,
133.256411432016,133.354660718376,133.453012823974,133.551418110189,133.649994583599,
133.724971129875,133.823569254879,133.922027037656,134.022249605428,134.120529163156,
134.21877574223,134.317018825268,134.41871601391,134.517100427329,134.620454003583,
134.723807579837,134.8363385207,134.948409000641,135.059693750754,135.088484104126),
 .UNSPECIFIED.);
#1447=B_SPLINE_CURVE_WITH_KNOTS('',3,(#142212,#142213,#142214,#142215,#142216,
#142217,#142218,#142219,#142220,#142221,#142222,#142223,#142224,#142225,
#142226,#142227,#142228,#142229,#142230,#142231,#142232,#142233,#142234,
#142235,#142236,#142237,#142238,#142239,#142240,#142241,#142242,#142243,
#142244,#142245,#142246,#142247,#142248,#142249,#142250,#142251,#142252,
#142253,#142254,#142255,#142256,#142257,#142258,#142259,#142260,#142261,
#142262,#142263,#142264,#142265,#142266,#142267,#142268,#142269,#142270,
#142271,#142272,#142273,#142274,#142275,#142276,#142277,#142278,#142279,
#142280,#142281),.UNSPECIFIED.,.F.,.F.,(4,3,3,3,3,3,3,3,3,3,3,3,3,3,3,3,
3,3,3,3,3,3,3,4),(132.862341310493,132.961797082208,133.060185488697,133.160174943026,
133.260164397355,133.358762522359,133.457220305135,133.557442872908,133.655722430636,
133.753969009709,133.852212092748,133.95390928139,134.052293694809,134.155647271063,
134.259000847317,134.356128675187,134.453094160804,134.549968416923,134.6467826177,
134.743567858739,134.84039997176,134.937256811787,135.034231214226,135.088484104361),
 .UNSPECIFIED.);
#1448=B_SPLINE_CURVE_WITH_KNOTS('',3,(#142282,#142283,#142284,#142285,#142286,
#142287,#142288,#142289),.UNSPECIFIED.,.F.,.F.,(4,1,1,1,1,4),(135.088484104361,
135.257837297279,136.256673747241,137.255510197203,138.254346647165,139.14521341354),
 .UNSPECIFIED.);
#1449=B_SPLINE_CURVE_WITH_KNOTS('',3,(#142295,#142296,#142297,#142298,#142299,
#142300,#142301,#142302,#142303,#142304,#142305,#142306,#142307,#142308,
#142309,#142310,#142311,#142312,#142313,#142314,#142315,#142316,#142317,
#142318,#142319,#142320,#142321,#142322,#142323,#142324,#142325,#142326,
#142327,#142328,#142329,#142330,#142331,#142332,#142333,#142334,#142335,
#142336,#142337,#142338,#142339,#142340,#142341,#142342,#142343,#142344,
#142345,#142346,#142347,#142348,#142349,#142350,#142351,#142352,#142353,
#142354,#142355,#142356,#142357,#142358,#142359,#142360,#142361,#142362,
#142363,#142364,#142365,#142366,#142367,#142368,#142369,#142370,#142371,
#142372,#142373,#142374,#142375,#142376,#142377,#142378,#142379,#142380,
#142381,#142382,#142383,#142384,#142385,#142386,#142387,#142388,#142389,
#142390,#142391,#142392,#142393,#142394,#142395,#142396,#142397,#142398,
#142399,#142400,#142401,#142402,#142403,#142404,#142405,#142406,#142407,
#142408,#142409,#142410,#142411,#142412,#142413,#142414,#142415,#142416,
#142417,#142418),.UNSPECIFIED.,.F.,.F.,(4,3,3,3,3,3,3,3,3,3,3,3,3,3,3,3,
3,3,3,3,3,3,3,3,3,3,3,3,3,3,3,3,3,3,3,3,3,3,3,3,3,4),(141.371669411768,
141.485016004534,141.600339367052,141.71566272957,141.814260854574,141.912718637351,
142.012941205123,142.111220762851,142.209467341925,142.307710424963,142.409407613605,
142.507792027024,142.611145603278,142.714499179532,142.813097304536,142.911555087312,
143.011777655085,143.110057212813,143.208303791887,143.306546874925,143.408244063567,
143.506628476986,143.60998205324,143.713335629494,143.811933754498,143.910391537275,
144.010614105047,144.108893662775,144.207140241849,144.305383324887,144.40708051353,
144.505464926948,144.608818503202,144.712172079456,144.810746601829,144.909191401416,
145.007536191856,145.105810581993,145.204060790382,145.302298022117,145.400579631092,
145.428467355838),.UNSPECIFIED.);
#1450=B_SPLINE_CURVE_WITH_KNOTS('',3,(#142419,#142420,#142421,#142422,#142423,
#142424,#142425,#142426,#142427,#142428,#142429,#142430,#142431,#142432,
#142433,#142434,#142435,#142436,#142437,#142438,#142439,#142440,#142441,
#142442,#142443,#142444,#142445,#142446,#142447,#142448,#142449,#142450,
#142451,#142452,#142453,#142454,#142455,#142456,#142457,#142458,#142459,
#142460,#142461,#142462,#142463,#142464,#142465,#142466,#142467,#142468,
#142469,#142470,#142471,#142472,#142473,#142474,#142475,#142476,#142477,
#142478,#142479,#142480,#142481,#142482,#142483,#142484,#142485,#142486,
#142487,#142488),.UNSPECIFIED.,.F.,.F.,(4,3,3,3,3,3,3,3,3,3,3,3,3,3,3,3,
3,3,3,3,3,3,3,4),(139.146050636314,139.244292899219,139.342541066063,139.440891121064,
139.539292972132,139.637867624459,139.717989829646,139.81658795465,139.915045737426,
140.015268305199,140.113547862927,140.211794442001,140.310037525039,140.411734713681,
140.5101191271,140.613472703354,140.716826279608,140.815569227393,140.914173010821,
141.012667061739,141.111081830931,141.209449097702,141.307822396312,141.371669411541),
 .UNSPECIFIED.);
#1451=B_SPLINE_CURVE_WITH_KNOTS('',3,(#142490,#142491,#142492,#142493,#142494,
#142495,#142496),.UNSPECIFIED.,.F.,.F.,(4,1,1,1,4),(139.14521341354,139.253183097127,
140.252019547089,141.25085599705,141.371669411541),.UNSPECIFIED.);
#1452=B_SPLINE_CURVE_WITH_KNOTS('',3,(#142497,#142498,#142499,#142500,#142501,
#142502,#142503,#142504,#142505,#142506,#142507,#142508,#142509,#142510,
#142511,#142512,#142513,#142514,#142515,#142516,#142517,#142518,#142519,
#142520,#142521,#142522,#142523,#142524,#142525,#142526,#142527,#142528,
#142529,#142530,#142531,#142532,#142533,#142534,#142535,#142536,#142537,
#142538,#142539,#142540,#142541,#142542,#142543,#142544,#142545,#142546,
#142547,#142548,#142549,#142550,#142551,#142552,#142553,#142554,#142555,
#142556,#142557,#142558,#142559,#142560,#142561,#142562,#142563,#142564,
#142565,#142566,#142567,#142568,#142569,#142570,#142571,#142572,#142573,
#142574,#142575,#142576,#142577,#142578,#142579,#142580,#142581,#142582,
#142583,#142584,#142585,#142586,#142587,#142588,#142589,#142590,#142591,
#142592,#142593,#142594,#142595,#142596,#142597,#142598,#142599,#142600,
#142601,#142602,#142603,#142604,#142605,#142606,#142607,#142608,#142609,
#142610,#142611,#142612,#142613,#142614,#142615,#142616,#142617,#142618,
#142619,#142620),.UNSPECIFIED.,.F.,.F.,(4,3,3,3,3,3,3,3,3,3,3,3,3,3,3,3,
3,3,3,3,3,3,3,3,3,3,3,3,3,3,3,3,3,3,3,3,3,3,3,3,3,4),(141.371669411541,
141.468831254161,141.566438903267,141.66339620349,141.760311911022,141.857216996242,
141.955335858935,142.052368429038,142.151030438025,142.249692447012,142.348290572016,
142.446748354792,142.546970922565,142.645250480293,142.743497059367,142.841740142405,
142.943437331047,143.041821744466,143.14517532072,143.248528896974,143.347127021978,
143.445584804755,143.545807372527,143.644086930256,143.742333509329,143.840576592367,
143.94227378101,144.040658194428,144.144011770682,144.247365346936,144.34596347194,
144.444421254716,144.544643822489,144.642923380217,144.741169959291,144.839413042329,
144.941110230971,145.03949464439,145.142848220644,145.246201796898,145.344774861149,
145.429604701798),.UNSPECIFIED.);
#1453=B_SPLINE_CURVE_WITH_KNOTS('',3,(#142626,#142627,#142628,#142629,#142630,
#142631,#142632,#142633,#142634),.UNSPECIFIED.,.F.,.F.,(4,1,1,1,1,1,4),
(147.65485471872,147.708681429341,148.707517879303,149.706354329265,150.705190779227,
151.704027229189,151.712252786696),.UNSPECIFIED.);
#1454=B_SPLINE_CURVE_WITH_KNOTS('',3,(#142635,#142636,#142637,#142638,#142639,
#142640,#142641,#142642,#142643,#142644,#142645,#142646,#142647,#142648,
#142649,#142650,#142651,#142652,#142653,#142654,#142655,#142656,#142657,
#142658,#142659,#142660,#142661,#142662,#142663,#142664,#142665,#142666,
#142667,#142668,#142669,#142670,#142671,#142672,#142673,#142674,#142675,
#142676,#142677,#142678,#142679,#142680,#142681,#142682,#142683,#142684,
#142685,#142686,#142687,#142688,#142689,#142690,#142691,#142692,#142693,
#142694,#142695,#142696,#142697,#142698,#142699,#142700,#142701,#142702,
#142703,#142704),.UNSPECIFIED.,.F.,.F.,(4,3,3,3,3,3,3,3,3,3,3,3,3,3,3,3,
3,3,3,3,3,3,3,4),(145.428467355838,145.526865648701,145.625438470026,145.711008529418,
145.809606654422,145.908064437198,146.008287004971,146.106566562699,146.204813141772,
146.303056224811,146.404753413453,146.503137826872,146.606491403125,146.709844979379,
146.807643480436,146.905302408374,147.002849316603,147.100335701354,147.197792033696,
147.295248746519,147.392798083501,147.490396206244,147.588155506493,147.65485471872),
 .UNSPECIFIED.);
#1455=B_SPLINE_CURVE_WITH_KNOTS('',3,(#142706,#142707,#142708,#142709,#142710,
#142711,#142712,#142713,#142714,#142715,#142716,#142717,#142718,#142719,
#142720,#142721,#142722,#142723,#142724,#142725,#142726,#142727,#142728,
#142729,#142730,#142731,#142732,#142733,#142734,#142735,#142736,#142737,
#142738,#142739,#142740,#142741,#142742,#142743,#142744,#142745,#142746,
#142747,#142748,#142749,#142750,#142751,#142752,#142753,#142754,#142755,
#142756,#142757,#142758,#142759,#142760,#142761,#142762,#142763,#142764,
#142765,#142766,#142767,#142768,#142769,#142770,#142771,#142772,#142773,
#142774,#142775),.UNSPECIFIED.,.F.,.F.,(4,3,3,3,3,3,3,3,3,3,3,3,3,3,3,3,
3,3,3,3,3,3,3,4),(145.429604701798,145.531533894931,145.629819470759,145.728068483142,
145.826310418025,145.924574745627,146.022950495499,146.121392861116,146.219991625193,
146.24503824686,146.343636371864,146.44209415464,146.542316722413,146.640596280141,
146.738842859215,146.837085942253,146.938783130896,147.037167544314,147.140521120568,
147.243874696822,147.352569174392,147.460952550046,147.568802109382,147.654854305401),
 .UNSPECIFIED.);
#1456=B_SPLINE_CURVE_WITH_KNOTS('',3,(#142776,#142777,#142778,#142779,#142780,
#142781,#142782,#142783),.UNSPECIFIED.,.F.,.F.,(4,1,1,1,1,4),(147.65485471872,
148.242711146784,149.241547596745,150.240384046707,151.239220496669,151.712342708042),
 .UNSPECIFIED.);
#1457=B_SPLINE_CURVE_WITH_KNOTS('',3,(#142789,#142790,#142791,#142792,#142793,
#142794,#142795,#142796,#142797,#142798,#142799,#142800,#142801,#142802,
#142803,#142804,#142805,#142806,#142807,#142808,#142809,#142810,#142811,
#142812,#142813,#142814,#142815,#142816,#142817,#142818,#142819,#142820,
#142821,#142822,#142823,#142824,#142825,#142826,#142827,#142828,#142829,
#142830,#142831,#142832,#142833,#142834,#142835,#142836,#142837,#142838,
#142839,#142840,#142841,#142842,#142843,#142844,#142845,#142846,#142847,
#142848,#142849,#142850,#142851,#142852,#142853,#142854,#142855,#142856,
#142857,#142858,#142859,#142860,#142861,#142862,#142863,#142864,#142865,
#142866,#142867,#142868,#142869,#142870,#142871,#142872,#142873,#142874,
#142875,#142876,#142877,#142878,#142879,#142880,#142881,#142882,#142883,
#142884,#142885,#142886,#142887,#142888,#142889,#142890,#142891,#142892,
#142893,#142894,#142895,#142896,#142897,#142898,#142899,#142900,#142901,
#142902,#142903,#142904,#142905,#142906,#142907,#142908,#142909,#142910,
#142911,#142912),.UNSPECIFIED.,.F.,.F.,(4,3,3,3,3,3,3,3,3,3,3,3,3,3,3,3,
3,3,3,3,3,3,3,3,3,3,3,3,3,3,3,3,3,3,3,3,3,3,3,3,3,4),(153.9380400259,154.035163898234,
154.132222574363,154.229246955325,154.326267897773,154.423381488606,154.520541056366,
154.617870832504,154.700536579074,154.799134704076,154.897592486852,154.997815054625,
155.096094612352,155.194341191424,155.292584274461,155.394281463105,155.492665876522,
155.596019452779,155.699373029036,155.797971154037,155.896428936811,155.996651504584,
156.09493106231,156.193177641381,156.291420724416,156.393117913062,156.491502326478,
156.594855902738,156.698209478998,156.796807604012,156.895265386799,156.995487954569,
157.093767512308,157.192014091391,157.29025717444,157.39195436307,157.490338776499,
157.59369235273,157.69704592896,157.795632129846,157.89577062296,157.995909116073),
 .UNSPECIFIED.);
#1458=B_SPLINE_CURVE_WITH_KNOTS('',3,(#142913,#142914,#142915,#142916,#142917,
#142918),.UNSPECIFIED.,.F.,.F.,(4,1,1,4),(151.712252786696,152.702863679151,
153.701700129113,153.93803972631),.UNSPECIFIED.);
#1459=B_SPLINE_CURVE_WITH_KNOTS('',3,(#142920,#142921,#142922,#142923,#142924,
#142925),.UNSPECIFIED.,.F.,.F.,(4,1,1,4),(151.712342708042,152.238056946631,
153.236893396593,153.9380400259),.UNSPECIFIED.);
#1460=B_SPLINE_CURVE_WITH_KNOTS('',3,(#142926,#142927,#142928,#142929,#142930,
#142931,#142932,#142933,#142934,#142935,#142936,#142937,#142938,#142939,
#142940,#142941,#142942,#142943,#142944,#142945,#142946,#142947,#142948,
#142949,#142950,#142951,#142952,#142953,#142954,#142955,#142956,#142957,
#142958,#142959,#142960,#142961,#142962,#142963,#142964,#142965,#142966,
#142967,#142968,#142969,#142970,#142971,#142972,#142973,#142974,#142975,
#142976,#142977,#142978,#142979,#142980,#142981,#142982,#142983,#142984,
#142985,#142986,#142987,#142988,#142989,#142990,#142991,#142992,#142993,
#142994,#142995,#142996,#142997,#142998,#142999,#143000,#143001,#143002,
#143003,#143004,#143005,#143006,#143007,#143008,#143009,#143010,#143011,
#143012,#143013,#143014,#143015,#143016,#143017,#143018,#143019,#143020,
#143021,#143022,#143023,#143024,#143025,#143026,#143027,#143028,#143029,
#143030,#143031,#143032,#143033,#143034,#143035,#143036,#143037,#143038,
#143039,#143040,#143041,#143042,#143043,#143044,#143045,#143046,#143047,
#143048,#143049),.UNSPECIFIED.,.F.,.F.,(4,3,3,3,3,3,3,3,3,3,3,3,3,3,3,3,
3,3,3,3,3,3,3,3,3,3,3,3,3,3,3,3,3,3,3,3,3,3,3,3,3,4),(153.938040202764,
154.056659980231,154.176963650987,154.235729846555,154.334327971559,154.432785754335,
154.533008322108,154.631287879836,154.729534458909,154.827777541948,154.92947473059,
155.027859144009,155.131212720263,155.234566296517,155.33316442152,155.431622204296,
155.531844772069,155.630124329797,155.72837090887,155.826613991908,155.928311180551,
156.026695593969,156.130049170224,156.233402746479,156.332000871484,156.430458654262,
156.530681222034,156.628960779764,156.727207358839,156.825450441878,156.927147630519,
157.025532043939,157.128885620189,157.23223919644,157.33080996438,157.429252216957,
157.527595662266,157.625869905301,157.724128943532,157.822375482216,157.92068828362,
157.994794060844),.UNSPECIFIED.);
#1461=B_SPLINE_CURVE_WITH_KNOTS('',3,(#143055,#143056,#143057,#143058,#143059,
#143060,#143061,#143062),.UNSPECIFIED.,.F.,.F.,(4,1,1,1,1,4),(160.221227414876,
160.693555278846,161.692391728808,162.691228178769,163.690064628731,164.278110108105),
 .UNSPECIFIED.);
#1462=B_SPLINE_CURVE_WITH_KNOTS('',3,(#143063,#143064,#143065,#143066,#143067,
#143068,#143069,#143070,#143071,#143072,#143073,#143074,#143075,#143076,
#143077,#143078,#143079,#143080,#143081,#143082,#143083,#143084,#143085,
#143086,#143087,#143088,#143089,#143090,#143091,#143092,#143093,#143094,
#143095,#143096,#143097,#143098,#143099,#143100,#143101,#143102,#143103,
#143104,#143105,#143106,#143107,#143108,#143109,#143110,#143111,#143112,
#143113,#143114,#143115,#143116,#143117,#143118,#143119,#143120,#143121,
#143122,#143123,#143124,#143125,#143126,#143127,#143128,#143129,#143130,
#143131,#143132),.UNSPECIFIED.,.F.,.F.,(4,3,3,3,3,3,3,3,3,3,3,3,3,3,3,3,
3,3,3,3,3,3,3,4),(157.995909116073,158.094187908191,158.192434197162,158.290677465192,
158.391978693625,158.490363803434,158.593123091178,158.695882378922,158.794480503912,
158.892938286674,158.993160854451,159.091440412165,159.189686991224,159.287930074247,
159.389627262907,159.488011676311,159.591365252598,159.694718828884,159.797216560019,
159.903218753284,160.005303397592,160.107256278837,160.209067828956,160.22122533308),
 .UNSPECIFIED.);
#1463=B_SPLINE_CURVE_WITH_KNOTS('',3,(#143134,#143135,#143136,#143137,#143138,
#143139,#143140,#143141,#143142,#143143,#143144,#143145,#143146,#143147,
#143148,#143149,#143150,#143151,#143152,#143153,#143154,#143155,#143156,
#143157,#143158,#143159,#143160,#143161,#143162,#143163,#143164,#143165,
#143166,#143167,#143168,#143169,#143170,#143171,#143172,#143173,#143174,
#143175,#143176,#143177,#143178,#143179,#143180,#143181,#143182,#143183,
#143184,#143185,#143186,#143187,#143188,#143189,#143190,#143191,#143192,
#143193,#143194,#143195,#143196,#143197,#143198,#143199,#143200,#143201,
#143202,#143203),.UNSPECIFIED.,.F.,.F.,(4,3,3,3,3,3,3,3,3,3,3,3,3,3,3,3,
3,3,3,3,3,3,3,4),(157.994794060844,158.093225180553,158.191816747246,158.231075646402,
158.329673771403,158.428131554177,158.528354121951,158.626633679676,158.724880258747,
158.823123341783,158.924820530428,159.023204943844,159.126558520104,159.229912096364,
159.328378576654,159.426704810661,159.526019875932,159.624169149677,159.722285836342,
159.820399593048,159.920606027993,160.018861091251,160.120043212039,160.221225332828),
 .UNSPECIFIED.);
#1464=B_SPLINE_CURVE_WITH_KNOTS('',3,(#143204,#143205,#143206,#143207,#143208,
#143209,#143210,#143211,#143212,#143213,#143214,#143215,#143216,#143217,
#143218,#143219,#143220,#143221,#143222,#143223,#143224,#143225,#143226,
#143227,#143228,#143229,#143230,#143231,#143232,#143233,#143234,#143235,
#143236,#143237,#143238,#143239,#143240,#143241,#143242,#143243,#143244,
#143245,#143246,#143247,#143248,#143249,#143250,#143251,#143252,#143253,
#143254,#143255,#143256,#143257,#143258,#143259,#143260,#143261,#143262,
#143263,#143264,#143265,#143266,#143267,#143268,#143269,#143270,#143271,
#143272,#143273,#143274,#143275,#143276,#143277,#143278,#143279,#143280,
#143281,#143282,#143283,#143284,#143285,#143286,#143287,#143288,#143289,
#143290,#143291,#143292,#143293,#143294,#143295,#143296,#143297,#143298,
#143299,#143300,#143301,#143302,#143303,#143304,#143305,#143306,#143307,
#143308,#143309,#143310,#143311,#143312,#143313,#143314,#143315,#143316,
#143317,#143318,#143319,#143320,#143321,#143322,#143323,#143324,#143325,
#143326,#143327,#143328,#143329,#143330),.UNSPECIFIED.,.F.,.F.,(4,3,3,3,
3,3,3,3,3,3,3,3,3,3,3,3,3,3,3,3,3,3,3,3,3,3,3,3,3,3,3,3,3,3,3,3,3,3,3,3,
3,3,4),(160.22122533308,160.228748546326,160.327346671318,160.425804454083,
160.526027021859,160.624306579575,160.722553158637,160.820796241665,160.92249343032,
161.020877843728,161.124231420008,161.227584996288,161.326183121278,161.424640904041,
161.524863471817,161.623143029531,161.72138960859,161.819632691614,161.921329880273,
162.019714293678,162.123067869964,162.22642144625,162.325019571326,162.423477354175,
162.52369992193,162.62197947973,162.720226058876,162.818469141986,162.920166330542,
163.018550744032,163.121904320122,163.225257896212,163.323856021116,163.422313803793,
163.522536371591,163.620815929221,163.719062508197,163.817305591139,163.919002779898,
164.017387193223,164.120740769699,164.224094346174,164.278857773673),
 .UNSPECIFIED.);
#1465=B_SPLINE_CURVE_WITH_KNOTS('',3,(#143336,#143337,#143338,#143339,#143340,
#143341,#143342,#143343,#143344,#143345,#143346,#143347,#143348,#143349,
#143350,#143351,#143352,#143353,#143354,#143355,#143356,#143357,#143358,
#143359,#143360,#143361,#143362,#143363,#143364,#143365,#143366,#143367,
#143368,#143369,#143370,#143371,#143372,#143373,#143374,#143375,#143376,
#143377,#143378,#143379,#143380,#143381,#143382,#143383,#143384,#143385,
#143386,#143387,#143388,#143389,#143390,#143391,#143392,#143393,#143394,
#143395,#143396,#143397,#143398,#143399,#143400,#143401,#143402,#143403,
#143404,#143405,#143406,#143407,#143408,#143409,#143410,#143411,#143412,
#143413,#143414,#143415,#143416,#143417,#143418,#143419,#143420,#143421,
#143422,#143423,#143424,#143425,#143426,#143427,#143428,#143429,#143430,
#143431,#143432,#143433,#143434,#143435,#143436,#143437,#143438,#143439,
#143440,#143441,#143442,#143443,#143444,#143445,#143446,#143447,#143448,
#143449,#143450,#143451,#143452,#143453,#143454,#143455,#143456,#143457,
#143458,#143459),.UNSPECIFIED.,.F.,.F.,(4,3,3,3,3,3,3,3,3,3,3,3,3,3,3,3,
3,3,3,3,3,3,3,3,3,3,3,3,3,3,3,3,3,3,3,3,3,3,3,3,3,4),(166.504410640259,
166.652910770224,166.686573978617,166.785172097217,166.883629873595,166.983852442968,
167.082131994357,167.180378567127,167.278621643905,167.380318840074,167.478703247404,
167.582056837991,167.685410428579,167.784008554554,167.882466338243,167.98268890578,
168.080968464273,168.179215044053,168.277458127742,168.379155315442,168.477539729364,
168.580893303952,168.684246878541,168.782845025291,168.881302829915,168.981525392239,
169.079804971904,169.178051572901,169.27629467782,169.377991840491,169.47637627546,
169.579729801982,169.683083328503,169.781689727948,169.880127484655,169.978469449804,
170.076745219915,170.174984320919,170.273261950065,170.371554712618,170.469968413646,
170.561255449419),.UNSPECIFIED.);
#1466=B_SPLINE_CURVE_WITH_KNOTS('',3,(#143460,#143461,#143462,#143463,#143464,
#143465),.UNSPECIFIED.,.F.,.F.,(4,1,1,4),(164.278110108105,164.688901078693,
165.687737528655,166.504405683219),.UNSPECIFIED.);
#1467=B_SPLINE_CURVE_WITH_KNOTS('',3,(#143467,#143468,#143469,#143470,#143471,
#143472,#143473,#143474,#143475,#143476,#143477,#143478,#143479,#143480,
#143481,#143482,#143483,#143484,#143485,#143486,#143487,#143488,#143489,
#143490,#143491,#143492,#143493,#143494,#143495,#143496,#143497,#143498,
#143499,#143500,#143501,#143502,#143503,#143504,#143505,#143506,#143507,
#143508,#143509,#143510,#143511,#143512,#143513,#143514,#143515,#143516,
#143517,#143518,#143519,#143520,#143521,#143522,#143523,#143524,#143525,
#143526,#143527,#143528,#143529,#143530,#143531,#143532,#143533,#143534,
#143535,#143536),.UNSPECIFIED.,.F.,.F.,(4,3,3,3,3,3,3,3,3,3,3,3,3,3,3,3,
3,3,3,3,3,3,3,4),(164.278857773673,164.377373915153,164.475767956526,164.574072829728,
164.672331037576,164.770572077498,164.868825422111,164.967184468132,165.065601061719,
165.164183861903,165.222930796135,165.321528921634,165.419986704907,165.520209272556,
165.618488830781,165.71673541035,165.814978493883,165.916675681936,166.01506009584,
166.118413670969,166.221767246097,166.344599874419,166.465474953174,166.504410639987),
 .UNSPECIFIED.);
#1468=B_SPLINE_CURVE_WITH_KNOTS('',3,(#143537,#143538,#143539,#143540,#143541,
#143542,#143543,#143544,#143545,#143546,#143547,#143548,#143549,#143550,
#143551,#143552,#143553,#143554,#143555,#143556,#143557,#143558,#143559,
#143560,#143561,#143562,#143563,#143564,#143565,#143566,#143567,#143568,
#143569,#143570,#143571,#143572,#143573,#143574,#143575,#143576,#143577,
#143578,#143579,#143580,#143581,#143582,#143583,#143584,#143585,#143586,
#143587,#143588,#143589,#143590,#143591,#143592,#143593,#143594,#143595,
#143596,#143597,#143598,#143599,#143600,#143601,#143602,#143603,#143604,
#143605,#143606,#143607,#143608,#143609,#143610,#143611,#143612,#143613,
#143614,#143615,#143616,#143617,#143618,#143619,#143620,#143621,#143622,
#143623,#143624,#143625,#143626,#143627,#143628,#143629,#143630,#143631,
#143632,#143633,#143634,#143635,#143636,#143637,#143638,#143639,#143640,
#143641,#143642,#143643,#143644,#143645,#143646,#143647,#143648,#143649,
#143650,#143651,#143652,#143653,#143654,#143655,#143656,#143657,#143658,
#143659,#143660,#143661,#143662,#143663),.UNSPECIFIED.,.F.,.F.,(4,3,3,3,
3,3,3,3,3,3,3,3,3,3,3,3,3,3,3,3,3,3,3,3,3,3,3,3,3,3,3,3,3,3,3,3,3,3,3,3,
3,3,4),(166.504410640259,166.6019131263,166.699371433809,166.796815990361,
166.894277201725,166.991846173229,167.089478292238,167.18726953544,167.220603696059,
167.319201820915,167.417659603535,167.517882171346,167.616161728898,167.714408307788,
167.812651390637,167.914348579483,168.012732992698,168.11608656936,168.219440146021,
168.318038274345,168.416496060454,168.516718627395,168.614998188462,168.71324477087,
168.811487857233,168.913185041921,169.011569458608,169.114923027296,169.218276595983,
169.31687471461,169.415332491016,169.515555060382,169.613834611798,169.712081184595,
169.8103242614,169.912021457536,170.010405864893,170.113759455419,170.217113045945,
170.315689889884,170.414143809231,170.512486666529,170.562190685947),
 .UNSPECIFIED.);
#1469=B_SPLINE_CURVE_WITH_KNOTS('',3,(#143669,#143670,#143671,#143672,#143673,
#143674,#143675,#143676,#143677,#143678,#143679,#143680,#143681,#143682,
#143683,#143684,#143685,#143686,#143687,#143688,#143689,#143690,#143691,
#143692,#143693,#143694,#143695,#143696,#143697,#143698,#143699,#143700,
#143701,#143702,#143703,#143704,#143705,#143706,#143707,#143708,#143709,
#143710,#143711,#143712,#143713,#143714,#143715,#143716,#143717,#143718,
#143719,#143720,#143721,#143722,#143723,#143724,#143725,#143726,#143727,
#143728,#143729,#143730,#143731,#143732,#143733,#143734,#143735,#143736,
#143737,#143738,#143739,#143740,#143741,#143742,#143743,#143744,#143745,
#143746,#143747,#143748,#143749,#143750,#143751,#143752,#143753,#143754,
#143755,#143756,#143757,#143758,#143759,#143760,#143761,#143762,#143763,
#143764,#143765,#143766,#143767,#143768,#143769,#143770,#143771,#143772,
#143773,#143774,#143775,#143776,#143777,#143778,#143779,#143780,#143781,
#143782,#143783,#143784,#143785,#143786,#143787,#143788,#143789,#143790,
#143791,#143792,#143793,#143794,#143795),.UNSPECIFIED.,.F.,.F.,(4,3,3,3,
3,3,3,3,3,3,3,3,3,3,3,3,3,3,3,3,3,3,3,3,3,3,3,3,3,3,3,3,3,3,3,3,3,3,3,3,
3,3,4),(172.787595947668,172.884841558621,172.984040004837,173.081071837019,
173.17805926857,173.275033212353,173.375882191352,173.472980624861,173.57014496835,
173.667458405729,173.67842912835,173.777027506528,173.875485539969,173.975708044762,
174.07398784529,174.172234663731,174.270477982414,174.372174881388,174.470559518877,
174.573912548594,174.677265578312,174.775864531657,174.874323148753,174.974545508693,
175.072825909276,175.171073332541,175.26931725999,175.371013452061,175.469398701777,
175.572750365025,175.676102028274,175.774697486027,175.873152598412,175.97337583339,
176.071652732112,176.169896662128,176.268137109468,176.36983745166,176.468219289246,
176.571578883741,176.674938478236,176.773518528001,176.845520779382),
 .UNSPECIFIED.);
#1470=B_SPLINE_CURVE_WITH_KNOTS('',3,(#143796,#143797,#143798,#143799,#143800,
#143801,#143802,#143803,#143804,#143805,#143806,#143807,#143808,#143809,
#143810,#143811,#143812,#143813,#143814,#143815,#143816,#143817,#143818,
#143819,#143820,#143821,#143822,#143823,#143824,#143825,#143826,#143827,
#143828,#143829,#143830,#143831,#143832,#143833,#143834,#143835,#143836,
#143837,#143838,#143839,#143840,#143841,#143842,#143843,#143844,#143845,
#143846,#143847,#143848,#143849,#143850,#143851,#143852,#143853,#143854,
#143855,#143856,#143857,#143858,#143859,#143860,#143861,#143862,#143863,
#143864,#143865),.UNSPECIFIED.,.F.,.F.,(4,3,3,3,3,3,3,3,3,3,3,3,3,3,3,3,
3,3,3,3,3,3,3,4),(170.561255449419,170.659855764701,170.681919778464,170.780517924865,
170.87897572865,170.979198291122,171.077477868766,171.175724467309,171.273967569347,
171.375664734117,171.474049165186,171.577402696806,171.680756228426,171.779354490543,
171.877812411222,171.978034944618,172.076314641176,172.174561359122,172.272804580894,
172.374501605268,172.472886155656,172.576239417022,172.679592678388,172.787595947439),
 .UNSPECIFIED.);
#1471=B_SPLINE_CURVE_WITH_KNOTS('',3,(#143867,#143868,#143869,#143870,#143871,
#143872,#143873,#143874,#143875,#143876,#143877,#143878,#143879,#143880,
#143881,#143882,#143883,#143884,#143885,#143886,#143887,#143888,#143889,
#143890,#143891,#143892,#143893,#143894,#143895,#143896,#143897,#143898,
#143899,#143900,#143901,#143902,#143903,#143904,#143905,#143906,#143907,
#143908,#143909,#143910,#143911,#143912,#143913,#143914,#143915,#143916,
#143917,#143918,#143919,#143920,#143921,#143922,#143923,#143924,#143925,
#143926,#143927,#143928,#143929,#143930,#143931,#143932,#143933,#143934,
#143935,#143936),.UNSPECIFIED.,.F.,.F.,(4,3,3,3,3,3,3,3,3,3,3,3,3,3,3,3,
3,3,3,3,3,3,3,4),(170.562190685947,170.660450522553,170.75869172103,170.856943754601,
170.955300626607,171.053713725501,171.152294519458,171.215949495907,171.314547642559,
171.413005447084,171.513228009432,171.611507588999,171.709754189896,171.807997294717,
171.909694457505,172.008078892377,172.111432419123,172.214785945869,172.31561776535,
172.416285943722,172.516781875652,172.617176498936,172.717484580452,172.787595947439),
 .UNSPECIFIED.);
#1472=B_SPLINE_CURVE_WITH_KNOTS('',3,(#143937,#143938,#143939,#143940,#143941,
#143942,#143943,#143944),.UNSPECIFIED.,.F.,.F.,(4,1,1,1,1,4),(172.787601414666,
173.21362239583,174.212458845792,175.211295295754,176.210131745716,176.844282084543),
 .UNSPECIFIED.);
#1473=B_SPLINE_CURVE_WITH_KNOTS('',3,(#143950,#143951,#143952,#143953,#143954,
#143955,#143956,#143957),.UNSPECIFIED.,.F.,.F.,(4,1,1,1,1,4),(179.070781254618,
179.671447828121,180.670284278083,181.669120728045,182.667957178007,183.128402575235),
 .UNSPECIFIED.);
#1474=B_SPLINE_CURVE_WITH_KNOTS('',3,(#143958,#143959,#143960,#143961,#143962,
#143963,#143964,#143965,#143966,#143967,#143968,#143969,#143970,#143971,
#143972,#143973,#143974,#143975,#143976,#143977,#143978,#143979,#143980,
#143981,#143982,#143983,#143984,#143985,#143986,#143987,#143988,#143989,
#143990,#143991,#143992,#143993,#143994,#143995,#143996,#143997,#143998,
#143999,#144000,#144001,#144002,#144003,#144004,#144005,#144006,#144007,
#144008,#144009,#144010,#144011,#144012,#144013,#144014,#144015,#144016,
#144017,#144018,#144019,#144020,#144021,#144022,#144023,#144024,#144025,
#144026,#144027),.UNSPECIFIED.,.F.,.F.,(4,3,3,3,3,3,3,3,3,3,3,3,3,3,3,3,
3,3,3,3,3,3,3,4),(176.845520779382,176.949052547984,177.047346597006,177.145600689888,
177.243844313097,177.342106934313,177.440479050025,177.538914725845,177.637509924401,
177.673774928198,177.772377764237,177.87084030234,177.971061686817,178.069346073264,
178.167597497761,178.265845436446,178.367536921874,178.465926166336,178.569268772248,
178.672611378159,178.782250112465,178.89154546425,179.000249342496,179.070781030154),
 .UNSPECIFIED.);
#1475=B_SPLINE_CURVE_WITH_KNOTS('',3,(#144029,#144030,#144031,#144032,#144033,
#144034),.UNSPECIFIED.,.F.,.F.,(4,1,1,4),(176.844282084543,177.208968195678,
178.20780464564,179.070781254618),.UNSPECIFIED.);
#1476=B_SPLINE_CURVE_WITH_KNOTS('',3,(#144035,#144036,#144037,#144038,#144039,
#144040,#144041,#144042),.UNSPECIFIED.,.F.,.F.,(4,1,1,1,1,4),(179.070781254618,
179.206641095602,180.205477545564,181.204313995525,182.203150445487,183.127688309466),
 .UNSPECIFIED.);
#1477=B_SPLINE_CURVE_WITH_KNOTS('',3,(#144048,#144049,#144050,#144051,#144052,
#144053,#144054,#144055),.UNSPECIFIED.,.F.,.F.,(4,1,1,1,1,4),(15.707963267949,
15.8622700343739,16.8611064843358,17.8599429342977,18.8587793842596,19.7647623411309),
 .UNSPECIFIED.);
#1478=B_SPLINE_CURVE_WITH_KNOTS('',3,(#144057,#144058,#144059,#144060,#144061,
#144062,#144063,#144064,#144065,#144066,#144067,#144068,#144069,#144070,
#144071,#144072,#144073,#144074,#144075,#144076,#144077,#144078,#144079,
#144080,#144081,#144082,#144083,#144084,#144085,#144086,#144087,#144088,
#144089,#144090,#144091,#144092,#144093,#144094,#144095,#144096,#144097,
#144098,#144099,#144100,#144101,#144102,#144103,#144104,#144105,#144106,
#144107,#144108,#144109,#144110,#144111,#144112,#144113,#144114),
 .UNSPECIFIED.,.F.,.F.,(4,3,3,3,3,3,3,3,3,3,3,3,3,3,3,3,3,3,3,4),(13.8757070305517,
13.9742335889647,14.072619844817,14.1714715622663,14.2696802945035,14.3678559192405,
14.4660280130677,14.5653794059038,14.6636894122209,14.7635614983165,14.8634335844121,
14.9606976622509,15.0578044027615,15.1548229002686,15.2517842042296,15.3487192914879,
15.4457083558909,15.5427241566488,15.6398692495935,15.707963267949),
 .UNSPECIFIED.);
#1479=B_SPLINE_CURVE_WITH_KNOTS('',3,(#144118,#144119,#144120,#144121,#144122),
 .UNSPECIFIED.,.F.,.F.,(4,1,4),(14.3986268518925,15.3974633018543,15.707963267949),
 .UNSPECIFIED.);
#1480=B_SPLINE_CURVE_WITH_KNOTS('',3,(#144123,#144124,#144125,#144126,#144127,
#144128,#144129,#144130),.UNSPECIFIED.,.F.,.F.,(4,1,1,1,1,4),(15.707963267949,
16.3962997518162,17.3951362017781,18.39397265174,19.3928091017018,19.7659327876261),
 .UNSPECIFIED.);
#1481=B_SPLINE_CURVE_WITH_KNOTS('',3,(#144136,#144137,#144138,#144139,#144140,
#144141,#144142,#144143),.UNSPECIFIED.,.F.,.F.,(4,1,1,1,1,4),(21.9911485751286,
22.854125184107,23.8529616340689,24.8517980840308,25.8506345339927,26.0493850773176),
 .UNSPECIFIED.);
#1482=B_SPLINE_CURVE_WITH_KNOTS('',3,(#144144,#144145,#144146,#144147,#144148,
#144149,#144150),.UNSPECIFIED.,.F.,.F.,(4,1,1,1,4),(19.7647623411309,19.8576158342214,
20.8564522841833,21.8552887341452,21.9911485751286),.UNSPECIFIED.);
#1483=B_SPLINE_CURVE_WITH_KNOTS('',3,(#144152,#144153,#144154,#144155,#144156,
#144157),.UNSPECIFIED.,.F.,.F.,(4,1,1,4),(19.7659327876261,20.3916455516637,
21.3904820016256,21.9911485751286),.UNSPECIFIED.);
#1484=B_SPLINE_CURVE_WITH_KNOTS('',3,(#144158,#144159,#144160,#144161,#144162,
#144163,#144164,#144165,#144166,#144167,#144168,#144169,#144170,#144171,
#144172,#144173,#144174,#144175,#144176,#144177,#144178,#144179,#144180,
#144181,#144182,#144183,#144184,#144185,#144186,#144187,#144188,#144189,
#144190,#144191,#144192,#144193,#144194,#144195,#144196,#144197,#144198,
#144199,#144200,#144201,#144202,#144203,#144204,#144205,#144206,#144207,
#144208,#144209,#144210,#144211,#144212,#144213,#144214,#144215,#144216,
#144217,#144218,#144219,#144220,#144221,#144222,#144223,#144224,#144225,
#144226,#144227,#144228,#144229,#144230,#144231,#144232,#144233,#144234,
#144235,#144236,#144237,#144238,#144239,#144240,#144241,#144242,#144243,
#144244,#144245,#144246,#144247,#144248,#144249,#144250,#144251,#144252,
#144253,#144254,#144255,#144256,#144257,#144258,#144259,#144260,#144261,
#144262,#144263,#144264,#144265,#144266,#144267,#144268,#144269,#144270,
#144271,#144272,#144273,#144274,#144275,#144276,#144277,#144278,#144279,
#144280,#144281),.UNSPECIFIED.,.F.,.F.,(4,3,3,3,3,3,3,3,3,3,3,3,3,3,3,3,
3,3,3,3,3,3,3,3,3,3,3,3,3,3,3,3,3,3,3,3,3,3,3,3,3,4),(21.9911487995816,
22.0999040743052,22.2090426220591,22.3187161819304,22.3893184515875,22.487921325434,
22.5863838904609,22.6866052668469,22.7848896533628,22.8831410679294,22.9813889867089,
23.083080465419,23.1814696653607,23.284812283455,23.3881549015493,23.4867551946089,
23.5852151974108,23.6854372166734,23.7837191063733,23.8819680542081,23.9802135397836,
24.0819079927155,24.180294868899,24.2836431102051,24.3869913515112,24.4855869800636,
24.5840422282252,24.6842654248812,24.7825423726193,24.8807863192412,24.9790267507949,
25.0807270134645,25.1791087548176,25.2824682781454,25.3858278014731,25.4844081039851,
25.5828572783489,25.6812050438807,25.779488016792,25.8777310255654,25.9759959055665,
26.0480412392441),.UNSPECIFIED.);
#1485=B_SPLINE_CURVE_WITH_KNOTS('',3,(#144287,#144288,#144289,#144290,#144291,
#144292,#144293,#144294,#144295,#144296,#144297,#144298,#144299,#144300,
#144301,#144302,#144303,#144304,#144305,#144306,#144307,#144308,#144309,
#144310,#144311,#144312,#144313,#144314,#144315,#144316,#144317,#144318,
#144319,#144320,#144321,#144322,#144323,#144324,#144325,#144326,#144327,
#144328,#144329,#144330,#144331,#144332,#144333,#144334,#144335,#144336,
#144337,#144338,#144339,#144340,#144341,#144342,#144343,#144344,#144345,
#144346,#144347,#144348,#144349,#144350,#144351,#144352,#144353,#144354,
#144355,#144356,#144357,#144358,#144359,#144360,#144361,#144362,#144363,
#144364,#144365,#144366,#144367,#144368,#144369,#144370,#144371,#144372,
#144373,#144374,#144375,#144376,#144377,#144378,#144379,#144380,#144381,
#144382,#144383,#144384,#144385,#144386,#144387,#144388,#144389,#144390,
#144391,#144392,#144393,#144394,#144395,#144396,#144397,#144398,#144399,
#144400,#144401,#144402,#144403,#144404,#144405,#144406,#144407,#144408,
#144409,#144410),.UNSPECIFIED.,.F.,.F.,(4,3,3,3,3,3,3,3,3,3,3,3,3,3,3,3,
3,3,3,3,3,3,3,3,3,3,3,3,3,3,3,3,3,3,3,3,3,3,3,3,3,4),(28.2743338823082,
28.3746245106346,28.4749734038757,28.575488632026,28.6760922702813,28.7769068624063,
28.8471438838783,28.9457420299521,29.0441998340445,29.144422396519,29.2427019760092,
29.3409485769638,29.4391916819739,29.5408888449405,29.6392732803314,29.7426268070858,
29.8459803338402,29.9445784592259,30.043036242451,30.1432588101199,30.241538368458,
30.3397849482006,30.4380280319667,30.5397252199255,30.6381096342119,30.7414632090069,
30.844816783802,30.9434149029147,31.041872679697,31.1420952489554,31.240374800478,
31.3386213732805,31.4368644499908,31.5385616459341,31.6369460529461,31.740299643355,
31.8436532337639,31.9422528703149,32.0406907036705,32.1390337581153,32.237318176998,
32.3317147986234),.UNSPECIFIED.);
#1486=B_SPLINE_CURVE_WITH_KNOTS('',3,(#144411,#144412,#144413,#144414,#144415,
#144416),.UNSPECIFIED.,.F.,.F.,(4,1,1,4),(26.0493850773176,26.8494709839545,
27.8483074339164,28.2743284148014),.UNSPECIFIED.);
#1487=B_SPLINE_CURVE_WITH_KNOTS('',3,(#144418,#144419,#144420,#144421,#144422,
#144423,#144424,#144425,#144426,#144427,#144428,#144429,#144430,#144431,
#144432,#144433,#144434,#144435,#144436,#144437,#144438,#144439,#144440,
#144441,#144442,#144443,#144444,#144445,#144446,#144447,#144448,#144449,
#144450,#144451,#144452,#144453,#144454,#144455,#144456,#144457,#144458,
#144459,#144460,#144461,#144462,#144463,#144464,#144465,#144466,#144467,
#144468,#144469,#144470,#144471,#144472,#144473,#144474,#144475,#144476,
#144477,#144478,#144479,#144480,#144481,#144482,#144483,#144484,#144485,
#144486,#144487,#144488,#144489,#144490),.UNSPECIFIED.,.F.,.F.,(4,3,3,3,
3,3,3,3,3,3,3,3,3,3,3,3,3,3,3,3,3,3,3,3,4),(26.0480412392441,26.1464094161118,
26.2448398501594,26.3434312965433,26.384664251435,26.4832625888131,26.5817205900565,
26.681943103974,26.780222893609,26.8784697091132,26.9767130328096,27.0784099499564,
27.1767946121896,27.2801476567932,27.3835007013968,27.4808124356152,27.5800026164232,
27.6770619121749,27.7740624149263,27.8710350587886,27.9718597646113,28.0689211634457,
28.1660361050485,28.2632831532614,28.2743338820794),.UNSPECIFIED.);
#1488=B_SPLINE_CURVE_WITH_KNOTS('',3,(#144491,#144492,#144493,#144494,#144495,
#144496,#144497,#144498,#144499,#144500,#144501,#144502,#144503,#144504,
#144505,#144506,#144507,#144508,#144509,#144510,#144511,#144512,#144513,
#144514,#144515,#144516,#144517,#144518,#144519,#144520,#144521,#144522,
#144523,#144524,#144525,#144526,#144527,#144528,#144529,#144530,#144531,
#144532,#144533,#144534,#144535,#144536,#144537,#144538,#144539,#144540,
#144541,#144542,#144543,#144544,#144545,#144546,#144547,#144548,#144549,
#144550,#144551,#144552,#144553,#144554,#144555,#144556,#144557,#144558,
#144559,#144560,#144561,#144562,#144563,#144564,#144565,#144566,#144567,
#144568,#144569,#144570,#144571,#144572,#144573,#144574,#144575,#144576,
#144577,#144578,#144579,#144580,#144581,#144582,#144583,#144584,#144585,
#144586,#144587,#144588,#144589,#144590,#144591,#144592,#144593,#144594,
#144595,#144596,#144597,#144598,#144599,#144600,#144601,#144602,#144603,
#144604,#144605,#144606,#144607,#144608,#144609,#144610,#144611,#144612,
#144613,#144614),.UNSPECIFIED.,.F.,.F.,(4,3,3,3,3,3,3,3,3,3,3,3,3,3,3,3,
3,3,3,3,3,3,3,3,3,3,3,3,3,3,3,3,3,3,3,3,3,3,3,3,3,4),(28.2743338823082,
28.3823371513587,28.4809354100483,28.5793933279209,28.6796158620959,28.7778955573906,
28.876142274651,28.9743854963144,29.0760825225659,29.1744670742836,29.2778203378021,
29.3811736013206,29.47977174272,29.5782295425626,29.6784521061526,29.7767316824779,
29.8749782806812,29.9732213833592,30.07491855034,30.173302984478,30.2766565178803,
30.3800100512825,30.4786081310757,30.5770658678857,30.6772884470555,30.7755679572915,
30.8738144884062,30.9720575230819,31.0737547676225,31.1721391321597,31.275492816702,
31.3788465012443,31.4774477473466,31.5759078066679,31.6742504131212,31.7725287579753,
31.8707723649116,31.9690107165623,32.0673303010146,32.1656922450024,32.2642027659188,
32.3314303507724),.UNSPECIFIED.);
#1489=B_SPLINE_CURVE_WITH_KNOTS('',3,(#144620,#144621,#144622,#144623,#144624,
#144625,#144626,#144627,#144628,#144629,#144630,#144631,#144632,#144633,
#144634,#144635,#144636,#144637,#144638,#144639,#144640,#144641,#144642,
#144643,#144644,#144645,#144646,#144647,#144648,#144649,#144650,#144651,
#144652,#144653,#144654,#144655,#144656,#144657,#144658,#144659,#144660,
#144661,#144662,#144663,#144664,#144665,#144666,#144667,#144668,#144669,
#144670,#144671,#144672,#144673,#144674,#144675,#144676,#144677,#144678,
#144679,#144680,#144681,#144682,#144683,#144684,#144685,#144686,#144687,
#144688,#144689,#144690,#144691,#144692,#144693,#144694,#144695,#144696,
#144697,#144698,#144699,#144700,#144701,#144702,#144703,#144704,#144705,
#144706,#144707,#144708,#144709,#144710,#144711,#144712,#144713,#144714,
#144715,#144716,#144717,#144718,#144719,#144720,#144721,#144722,#144723,
#144724,#144725,#144726,#144727,#144728,#144729,#144730,#144731,#144732,
#144733,#144734,#144735,#144736,#144737,#144738,#144739,#144740,#144741,
#144742,#144743),.UNSPECIFIED.,.F.,.F.,(4,3,3,3,3,3,3,3,3,3,3,3,3,3,3,3,
3,3,3,3,3,3,3,3,3,3,3,3,3,3,3,3,3,3,3,3,3,3,3,3,3,4),(34.5575191897594,
34.6782345503608,34.8009387396036,34.8401625836495,34.9387607091287,35.0372184923873,
35.1374410600403,35.2357206182623,35.333967197833,35.4322102813716,35.5339074694315,
35.6322918833522,35.7356454584818,35.8389990336114,35.9375971585481,36.0360549412581,
36.1362775090475,36.2345570667098,36.3328036457177,36.4310467286914,36.5327439174119,
36.6311283307679,36.7344819071706,36.8378354835733,36.9364336084865,37.034891391171,
37.1351139589665,37.2333935165987,37.3316400955748,37.429883178515,37.5315803672701,
37.6299647805889,37.7333183570621,37.8366719335352,37.9352415778349,38.0336830992393,
38.1320262040969,38.2303004962056,38.328562793654,38.4268127465216,38.5251372404807,
38.6142676624748),.UNSPECIFIED.);
#1490=B_SPLINE_CURVE_WITH_KNOTS('',3,(#144744,#144745,#144746,#144747,#144748,
#144749,#144750,#144751,#144752,#144753,#144754,#144755,#144756,#144757,
#144758,#144759,#144760,#144761,#144762,#144763,#144764,#144765,#144766,
#144767,#144768,#144769,#144770,#144771,#144772,#144773,#144774,#144775,
#144776,#144777,#144778,#144779,#144780,#144781,#144782,#144783,#144784,
#144785,#144786,#144787,#144788,#144789,#144790,#144791,#144792,#144793,
#144794,#144795,#144796,#144797,#144798,#144799,#144800,#144801,#144802,
#144803,#144804,#144805,#144806,#144807,#144808,#144809,#144810,#144811,
#144812,#144813,#144814,#144815,#144816),.UNSPECIFIED.,.F.,.F.,(4,3,3,3,
3,3,3,3,3,3,3,3,3,3,3,3,3,3,3,3,3,3,3,3,4),(32.3317147986234,32.4299572783543,
32.5330903796972,32.6314723034345,32.7299238260328,32.8285286780479,32.8424896837258,
32.9410878085144,33.0395455910817,33.1397681589074,33.2380477164404,33.3362942953245,
33.4345373781799,33.5362345670569,33.6346189803101,33.7379725569989,33.8413261336877,
33.93909739415,34.0367388270534,34.1342810926871,34.2317547370018,34.3292101035708,
34.426655495324,34.5241539308998,34.5575191894878),.UNSPECIFIED.);
#1491=B_SPLINE_CURVE_WITH_KNOTS('',3,(#144818,#144819,#144820,#144821,#144822,
#144823,#144824,#144825,#144826,#144827,#144828,#144829,#144830,#144831,
#144832,#144833,#144834,#144835,#144836,#144837,#144838,#144839,#144840,
#144841,#144842,#144843,#144844,#144845,#144846,#144847,#144848,#144849,
#144850,#144851,#144852,#144853,#144854,#144855,#144856,#144857,#144858,
#144859,#144860,#144861,#144862,#144863,#144864,#144865,#144866,#144867,
#144868,#144869,#144870,#144871,#144872,#144873,#144874,#144875,#144876,
#144877,#144878,#144879,#144880,#144881,#144882,#144883,#144884,#144885,
#144886,#144887),.UNSPECIFIED.,.F.,.F.,(4,3,3,3,3,3,3,3,3,3,3,3,3,3,3,3,
3,3,3,3,3,3,3,4),(32.3314303507724,32.3776829512062,32.4762810765969,32.5747388598271,
32.6749614274947,32.7732409858373,32.871487565584,32.9697306493543,33.0714278373078,
33.1698122515977,33.2731658263829,33.3765194011681,33.4751175203039,33.5735752971096,
33.6737978663622,33.7720774179092,33.8703239907363,33.9685670674716,34.0702642633862,
34.1686486704234,34.2720022607767,34.37535585113,34.5238559809678,34.5575191894878),
 .UNSPECIFIED.);
#1492=B_SPLINE_CURVE_WITH_KNOTS('',3,(#144888,#144889,#144890,#144891,#144892,
#144893,#144894,#144895),.UNSPECIFIED.,.F.,.F.,(4,1,1,1,1,4),(34.5575241471828,
35.3741923010918,36.3730287510537,37.3718652010156,38.3707016509774,38.6157831659124),
 .UNSPECIFIED.);
#1493=B_SPLINE_CURVE_WITH_KNOTS('',3,(#144901,#144902,#144903,#144904,#144905,
#144906,#144907,#144908,#144909,#144910,#144911,#144912,#144913,#144914,
#144915,#144916,#144917,#144918,#144919,#144920,#144921,#144922,#144923,
#144924,#144925,#144926,#144927,#144928,#144929,#144930,#144931,#144932,
#144933,#144934,#144935,#144936,#144937,#144938,#144939,#144940,#144941,
#144942,#144943,#144944,#144945,#144946,#144947,#144948,#144949,#144950,
#144951,#144952,#144953,#144954,#144955,#144956,#144957,#144958,#144959,
#144960,#144961,#144962,#144963,#144964,#144965,#144966,#144967,#144968,
#144969,#144970,#144971,#144972,#144973,#144974,#144975,#144976,#144977,
#144978,#144979,#144980,#144981,#144982,#144983,#144984,#144985,#144986,
#144987,#144988,#144989,#144990,#144991,#144992,#144993,#144994,#144995,
#144996,#144997,#144998,#144999,#145000,#145001,#145002,#145003,#145004,
#145005,#145006,#145007,#145008,#145009,#145010,#145011,#145012,#145013,
#145014,#145015,#145016,#145017,#145018,#145019,#145020,#145021,#145022,
#145023,#145024),.UNSPECIFIED.,.F.,.F.,(4,3,3,3,3,3,3,3,3,3,3,3,3,3,3,3,
3,3,3,3,3,3,3,3,3,3,3,3,3,3,3,3,3,3,3,3,3,3,3,3,3,4),(40.8407044969197,
40.9391705387199,41.0374964280042,41.1368115911765,41.2349607512895,41.3330774110131,
41.4311912274066,41.5313978539006,41.6296531901077,41.7308354617452,41.8320177333827,
41.9306158583837,42.0290736411578,42.1292962089311,42.2275757666566,42.3258223457272,
42.424065428763,42.5257626174084,42.6241470308244,42.7275006070845,42.8308541833445,
42.929452308347,43.0279100911226,43.1281326588956,43.2264122166225,43.3246587956946,
43.4229018787317,43.5245990673754,43.6229834807929,43.7263370570496,43.8296906333064,
43.9282887583114,44.0267465410897,44.126969108862,44.2252486665916,44.3234952456665,
44.4217383287062,44.5234355173468,44.6218199307671,44.7251735070177,44.8285270832683,
44.8983979680182),.UNSPECIFIED.);
#1494=B_SPLINE_CURVE_WITH_KNOTS('',3,(#145025,#145026,#145027,#145028,#145029,
#145030,#145031,#145032,#145033,#145034,#145035,#145036,#145037,#145038,
#145039,#145040,#145041,#145042,#145043,#145044,#145045,#145046,#145047,
#145048,#145049,#145050,#145051,#145052,#145053,#145054,#145055,#145056,
#145057,#145058,#145059,#145060,#145061,#145062,#145063,#145064,#145065,
#145066,#145067,#145068,#145069,#145070,#145071,#145072,#145073,#145074,
#145075,#145076,#145077,#145078,#145079,#145080,#145081,#145082,#145083,
#145084,#145085,#145086,#145087,#145088,#145089,#145090,#145091,#145092,
#145093,#145094,#145095,#145096,#145097),.UNSPECIFIED.,.F.,.F.,(4,3,3,3,
3,3,3,3,3,3,3,3,3,3,3,3,3,3,3,3,3,3,3,3,4),(38.6142676624748,38.7127107166971,
38.8113099318161,38.835508383497,38.9341065084864,39.0325642912487,39.132786859025,
39.2310664167387,39.3293129957976,39.4275560788218,39.5292532674811,39.6276376808857,
39.7309912571723,39.8343448334589,39.9329429584521,40.0314007412181,40.1316233089935,
40.2299028667104,40.3281494457725,40.4263925287994,40.5280897174548,40.6264741308618,
40.7298277071413,40.8331812834208,40.8407044966674),.UNSPECIFIED.);
#1495=B_SPLINE_CURVE_WITH_KNOTS('',3,(#145099,#145100,#145101,#145102,#145103,
#145104),.UNSPECIFIED.,.F.,.F.,(4,1,1,4),(38.6157831659124,39.3695381009393,
40.3683745509012,40.8407024149584),.UNSPECIFIED.);
#1496=B_SPLINE_CURVE_WITH_KNOTS('',3,(#145105,#145106,#145107,#145108,#145109,
#145110,#145111,#145112,#145113,#145114,#145115,#145116,#145117,#145118,
#145119,#145120,#145121,#145122,#145123,#145124,#145125,#145126,#145127,
#145128,#145129,#145130,#145131,#145132,#145133,#145134,#145135,#145136,
#145137,#145138,#145139,#145140,#145141,#145142,#145143,#145144,#145145,
#145146,#145147,#145148,#145149,#145150,#145151,#145152,#145153,#145154,
#145155,#145156,#145157,#145158,#145159,#145160,#145161,#145162,#145163,
#145164,#145165,#145166,#145167,#145168,#145169,#145170,#145171,#145172,
#145173,#145174,#145175,#145176,#145177,#145178,#145179,#145180,#145181,
#145182,#145183,#145184,#145185,#145186,#145187,#145188,#145189,#145190,
#145191,#145192,#145193,#145194,#145195,#145196,#145197,#145198,#145199,
#145200,#145201,#145202,#145203,#145204,#145205,#145206,#145207,#145208,
#145209,#145210,#145211,#145212,#145213,#145214,#145215,#145216,#145217,
#145218,#145219,#145220,#145221,#145222,#145223,#145224,#145225,#145226,
#145227,#145228,#145229,#145230,#145231),.UNSPECIFIED.,.F.,.F.,(4,3,3,3,
3,3,3,3,3,3,3,3,3,3,3,3,3,3,3,3,3,3,3,3,3,3,3,3,3,3,3,3,3,3,3,3,3,3,3,3,
3,3,4),(40.8407044966674,40.9425310419931,41.0487010317106,41.1508691915794,
41.2531658485544,41.3556785603232,41.3672110008631,41.4658091258525,41.5642669086152,
41.6644894763914,41.7627690341051,41.8610156131641,41.9592586961883,42.0609558848474,
42.1593402982521,42.2626938745385,42.3660474508249,42.4646455758182,42.5631033585842,
42.6633259263595,42.7616054840765,42.8598520631385,42.9580951461655,43.0597923348208,
43.1581767482279,43.2615303245073,43.3648839007868,43.4634820258002,43.5619398085867,
43.6621623763569,43.7604419340952,43.8586885131787,43.9569315962273,44.0586287848577,
44.157013198287,44.2603667745178,44.3637203507487,44.4623140220524,44.5607732131559,
44.6591152246758,44.757389474878,44.8556332863474,44.8979423039439),
 .UNSPECIFIED.);
#1497=B_SPLINE_CURVE_WITH_KNOTS('',3,(#145237,#145238,#145239,#145240,#145241,
#145242,#145243,#145244),.UNSPECIFIED.,.F.,.F.,(4,1,1,1,1,4),(47.123889803847,
47.8250364331539,48.8238728831158,49.8227093330777,50.8215457830395,51.1819114029981),
 .UNSPECIFIED.);
#1498=B_SPLINE_CURVE_WITH_KNOTS('',3,(#145245,#145246,#145247,#145248,#145249,
#145250,#145251,#145252,#145253,#145254,#145255,#145256,#145257,#145258,
#145259,#145260,#145261,#145262,#145263,#145264,#145265,#145266,#145267,
#145268,#145269,#145270,#145271,#145272,#145273,#145274,#145275,#145276,
#145277,#145278,#145279,#145280,#145281,#145282,#145283,#145284,#145285,
#145286,#145287,#145288,#145289,#145290,#145291,#145292,#145293,#145294,
#145295,#145296,#145297,#145298,#145299,#145300,#145301,#145302,#145303,
#145304,#145305,#145306,#145307,#145308,#145309,#145310,#145311,#145312,
#145313,#145314),.UNSPECIFIED.,.F.,.F.,(4,3,3,3,3,3,3,3,3,3,3,3,3,3,3,3,
3,3,3,3,3,3,3,4),(44.8983979680182,44.9968932668749,45.0952714925266,45.1935672979277,
45.2918209615386,45.3900619752629,45.4883198102566,45.5866859517105,45.6851137001938,
45.7837031754335,45.8273635332302,45.9259616582337,46.0244194410101,46.1246420087828,
46.2229215665108,46.3211681455839,46.4194112286225,46.5211084172648,46.6194928306836,
46.7228464069378,46.826199983192,46.9466622822351,47.0654828012647,47.1238896269613),
 .UNSPECIFIED.);
#1499=B_SPLINE_CURVE_WITH_KNOTS('',3,(#145316,#145317,#145318,#145319,#145320,
#145321,#145322,#145323,#145324,#145325,#145326,#145327,#145328,#145329,
#145330,#145331,#145332,#145333,#145334,#145335,#145336,#145337,#145338,
#145339,#145340,#145341,#145342,#145343,#145344,#145345,#145346,#145347,
#145348,#145349,#145350,#145351,#145352,#145353,#145354,#145355,#145356,
#145357,#145358,#145359,#145360,#145361,#145362,#145363,#145364,#145365,
#145366,#145367,#145368,#145369,#145370,#145371,#145372,#145373,#145374,
#145375,#145376,#145377,#145378,#145379,#145380,#145381,#145382,#145383,
#145384,#145385),.UNSPECIFIED.,.F.,.F.,(4,3,3,3,3,3,3,3,3,3,3,3,3,3,3,3,
3,3,3,3,3,3,3,4),(44.8979423039439,44.9961925047522,45.0945462342209,45.1929542076481,
45.2915321400895,45.3625568007106,45.4611549257133,45.5596127084887,45.6598352762617,
45.7581148339886,45.8563614130606,45.9546044960977,46.0563016847413,46.1546860981589,
46.2580396744156,46.3613932506724,46.4587199838046,46.5559210250953,46.6530274701202,
46.7500702965176,46.8471124553619,46.9441490048062,47.0412721236582,47.123889803847),
 .UNSPECIFIED.);
#1500=B_SPLINE_CURVE_WITH_KNOTS('',3,(#145386,#145387,#145388,#145389,#145390,
#145391,#145392,#145393),.UNSPECIFIED.,.F.,.F.,(4,1,1,1,1,4),(47.1238901028405,
47.3602297006343,48.3590661505962,49.3579026005581,50.3567390505199,51.180388194529),
 .UNSPECIFIED.);
#1501=B_SPLINE_CURVE_WITH_KNOTS('',3,(#145399,#145400,#145401,#145402,#145403,
#145404,#145405,#145406,#145407,#145408,#145409,#145410,#145411,#145412,
#145413,#145414,#145415,#145416,#145417,#145418,#145419,#145420,#145421,
#145422,#145423,#145424,#145425,#145426,#145427,#145428,#145429,#145430,
#145431,#145432,#145433,#145434,#145435,#145436,#145437,#145438,#145439,
#145440,#145441,#145442,#145443,#145444,#145445,#145446,#145447,#145448,
#145449,#145450,#145451,#145452,#145453,#145454,#145455,#145456,#145457,
#145458,#145459,#145460,#145461,#145462,#145463,#145464,#145465,#145466,
#145467,#145468,#145469,#145470,#145471,#145472,#145473,#145474,#145475,
#145476,#145477,#145478,#145479,#145480,#145481,#145482,#145483,#145484,
#145485,#145486,#145487,#145488,#145489,#145490,#145491,#145492,#145493,
#145494,#145495,#145496,#145497,#145498,#145499,#145500,#145501,#145502,
#145503,#145504,#145505,#145506,#145507,#145508,#145509,#145510,#145511,
#145512,#145513,#145514,#145515,#145516,#145517,#145518,#145519,#145520,
#145521,#145522),.UNSPECIFIED.,.F.,.F.,(4,3,3,3,3,3,3,3,3,3,3,3,3,3,3,3,
3,3,3,3,3,3,3,3,3,3,3,3,3,3,3,3,3,3,3,3,3,3,3,3,3,4),(53.4070755243676,
53.5149520672777,53.623163861073,53.7318758460237,53.8180551329252,53.9166532579289,
54.0151110407056,54.1153336084783,54.2136131662064,54.3118597452797,54.4101028283182,
54.5118000169604,54.6101844303791,54.7135380066331,54.816891582887,54.9154897078907,
55.0139474906675,55.1141700584402,55.2124496161683,55.3106961952417,55.4089392782802,
55.5106364669224,55.6090208803412,55.7123744565951,55.8157280328489,55.9143261578526,
56.0127839406294,56.113006508402,56.2112860661302,56.3095326452036,56.4077757282421,
56.5094729168843,56.6078573303031,56.7112109065569,56.8145644828108,56.9131452274569,
57.0115945031609,57.1099420320499,57.2082227592529,57.3064633876105,57.4047205556915,
57.4639959741701),.UNSPECIFIED.);
#1502=B_SPLINE_CURVE_WITH_KNOTS('',3,(#145523,#145524,#145525,#145526,#145527,
#145528),.UNSPECIFIED.,.F.,.F.,(4,1,1,4),(51.1819114029981,51.8203822330014,
52.8192186829633,53.4070751110266),.UNSPECIFIED.);
#1503=B_SPLINE_CURVE_WITH_KNOTS('',3,(#145530,#145531,#145532,#145533,#145534,
#145535,#145536),.UNSPECIFIED.,.F.,.F.,(4,1,1,1,4),(51.180388194529,51.3555755004818,
52.3544119504437,53.3532484004056,53.4070751110266),.UNSPECIFIED.);
#1504=B_SPLINE_CURVE_WITH_KNOTS('',3,(#145537,#145538,#145539,#145540,#145541,
#145542,#145543,#145544,#145545,#145546,#145547,#145548,#145549,#145550,
#145551,#145552,#145553,#145554,#145555,#145556,#145557,#145558,#145559,
#145560,#145561,#145562,#145563,#145564,#145565,#145566,#145567,#145568,
#145569,#145570,#145571,#145572,#145573,#145574,#145575,#145576,#145577,
#145578,#145579,#145580,#145581,#145582,#145583,#145584,#145585,#145586,
#145587,#145588,#145589,#145590,#145591,#145592,#145593,#145594,#145595,
#145596,#145597,#145598,#145599,#145600,#145601,#145602,#145603,#145604,
#145605,#145606,#145607,#145608,#145609,#145610,#145611,#145612,#145613,
#145614,#145615,#145616,#145617,#145618,#145619,#145620,#145621,#145622,
#145623,#145624,#145625,#145626,#145627,#145628,#145629,#145630,#145631,
#145632,#145633,#145634,#145635,#145636,#145637,#145638,#145639,#145640,
#145641,#145642,#145643,#145644,#145645,#145646,#145647,#145648,#145649,
#145650,#145651,#145652,#145653,#145654,#145655,#145656,#145657,#145658,
#145659,#145660,#145661,#145662,#145663),.UNSPECIFIED.,.F.,.F.,(4,3,3,3,
3,3,3,3,3,3,3,3,3,3,3,3,3,3,3,3,3,3,3,3,3,3,3,3,3,3,3,3,3,3,3,3,3,3,3,3,
3,3,4),(53.4070751110266,53.5048543854907,53.6024983707772,53.7000367768846,
53.7975186210126,53.8949743677963,53.9924344477706,54.0899931990358,54.1876041339868,
54.2853815723763,54.3520848503674,54.4506829753711,54.5491407581477,54.6493633259204,
54.7476428836485,54.8458894627219,54.9441325457602,55.0458297344025,55.1442141478213,
55.2475677240753,55.3509213003293,55.4495194253331,55.5479772081099,55.6481997758826,
55.7464793336108,55.8447259126843,55.9429689957226,56.0446661843648,56.1430505977836,
56.2464041740374,56.3497577502912,56.4483558752949,56.5468136580715,56.6470362258442,
56.7453157835723,56.8435623626457,56.9418054456841,57.0435026343264,57.1418870477452,
57.2452406239991,57.3485942002531,57.4471969425955,57.4649113880947),
 .UNSPECIFIED.);
#1505=B_SPLINE_CURVE_WITH_KNOTS('',3,(#145669,#145670,#145671,#145672,#145673,
#145674,#145675,#145676),.UNSPECIFIED.,.F.,.F.,(4,1,1,1,1,4),(59.6902604182062,
59.8110738326964,60.8099102826583,61.8087467326202,62.807583182582,63.7472418219311),
 .UNSPECIFIED.);
#1506=B_SPLINE_CURVE_WITH_KNOTS('',3,(#145677,#145678,#145679,#145680,#145681,
#145682,#145683,#145684,#145685,#145686,#145687,#145688,#145689,#145690,
#145691,#145692,#145693,#145694,#145695,#145696,#145697,#145698,#145699,
#145700,#145701,#145702,#145703,#145704,#145705,#145706,#145707,#145708,
#145709,#145710,#145711,#145712,#145713,#145714,#145715,#145716,#145717,
#145718,#145719,#145720,#145721,#145722,#145723,#145724,#145725,#145726,
#145727,#145728,#145729,#145730,#145731,#145732,#145733,#145734,#145735,
#145736,#145737,#145738,#145739,#145740,#145741,#145742,#145743,#145744,
#145745,#145746),.UNSPECIFIED.,.F.,.F.,(4,3,3,3,3,3,3,3,3,3,3,3,3,3,3,3,
3,3,3,3,3,3,3,4),(57.4639959741701,57.5623571679093,57.6607771760175,57.759361977221,
57.8134009327727,57.9119990577764,58.0104568405532,58.1106794083258,58.208958966054,
58.3072055451274,58.4054486281659,58.507145816808,58.6055302302268,58.7088838064807,
58.8122373827345,58.9094791608007,59.0070768179764,59.1040671063403,59.2009981633324,
59.2979009849176,59.3959908432397,59.4929780422904,59.5916192302483,59.6902604182062),
 .UNSPECIFIED.);
#1507=B_SPLINE_CURVE_WITH_KNOTS('',3,(#145748,#145749,#145750,#145751,#145752,
#145753,#145754,#145755,#145756,#145757,#145758,#145759,#145760,#145761,
#145762,#145763,#145764,#145765,#145766,#145767,#145768,#145769,#145770,
#145771,#145772,#145773,#145774,#145775,#145776,#145777,#145778,#145779,
#145780,#145781,#145782,#145783,#145784,#145785,#145786,#145787,#145788,
#145789,#145790,#145791,#145792,#145793,#145794,#145795,#145796,#145797,
#145798,#145799,#145800,#145801,#145802,#145803,#145804,#145805,#145806,
#145807,#145808,#145809,#145810,#145811,#145812,#145813,#145814),
 .UNSPECIFIED.,.F.,.F.,(4,3,3,3,3,3,3,3,3,3,3,3,3,3,3,3,3,3,3,3,3,3,4),
(57.4649113880947,57.563347414557,57.6616774298067,57.7599496949233,57.858193723518,
57.9564389944101,58.0547832866313,58.1531751872017,58.2517448734333,58.3474306502149,
58.4460287752185,58.544486557995,58.6447091257677,58.7429886834959,58.8412352625694,
58.9394783456078,59.0411755342501,59.1395599476689,59.2429135239229,59.3462671001768,
59.4608829140295,59.5755716660044,59.6902604179793),.UNSPECIFIED.);
#1508=B_SPLINE_CURVE_WITH_KNOTS('',3,(#145815,#145816,#145817,#145818,#145819,
#145820,#145821,#145822,#145823,#145824,#145825,#145826,#145827,#145828,
#145829,#145830,#145831,#145832,#145833,#145834,#145835,#145836,#145837,
#145838,#145839,#145840,#145841,#145842,#145843,#145844,#145845,#145846,
#145847,#145848,#145849,#145850,#145851,#145852,#145853,#145854,#145855,
#145856,#145857,#145858,#145859,#145860,#145861,#145862,#145863,#145864,
#145865,#145866,#145867,#145868,#145869,#145870,#145871,#145872,#145873,
#145874,#145875,#145876,#145877,#145878,#145879,#145880,#145881,#145882,
#145883,#145884,#145885,#145886,#145887,#145888,#145889,#145890,#145891,
#145892,#145893,#145894,#145895,#145896,#145897,#145898,#145899,#145900,
#145901,#145902,#145903,#145904,#145905,#145906,#145907,#145908,#145909,
#145910,#145911,#145912,#145913,#145914,#145915,#145916,#145917,#145918,
#145919,#145920,#145921,#145922,#145923,#145924,#145925,#145926,#145927,
#145928,#145929,#145930,#145931,#145932,#145933,#145934,#145935,#145936,
#145937,#145938),.UNSPECIFIED.,.F.,.F.,(4,3,3,3,3,3,3,3,3,3,3,3,3,3,3,3,
3,3,3,3,3,3,3,3,3,3,3,3,3,3,3,3,3,3,3,3,3,3,3,3,3,4),(59.6902604182062,
59.788634173056,59.886998581597,59.9853827919993,60.0838846667643,60.1824499292137,
60.2811933482975,60.3451035501387,60.4437016751424,60.5421594579193,60.642382025692,
60.7406615834201,60.8389081624935,60.937151245532,61.0388484341742,61.1372328475929,
61.2405864238468,61.3439400001006,61.4425381251043,61.5409959078807,61.6412184756534,
61.7394980333816,61.8377446124549,61.9359876954935,62.0376848841357,62.1360692975546,
62.2394228738085,62.3427764500624,62.4413745750661,62.5398323578427,62.6400549256154,
62.7383344833436,62.836581062417,62.9348241454553,63.0365213340976,63.1349057475164,
63.2382593237703,63.3416129000243,63.4431811256632,63.5416227665057,63.6447542845429,
63.74788580258),.UNSPECIFIED.);
#1509=B_SPLINE_CURVE_WITH_KNOTS('',3,(#145944,#145945,#145946,#145947,#145948,
#145949,#145950,#145951,#145952,#145953,#145954,#145955,#145956,#145957,
#145958,#145959,#145960,#145961,#145962,#145963,#145964,#145965,#145966,
#145967,#145968,#145969,#145970,#145971,#145972,#145973,#145974,#145975,
#145976,#145977,#145978,#145979,#145980,#145981,#145982,#145983,#145984,
#145985,#145986,#145987,#145988,#145989,#145990,#145991,#145992,#145993,
#145994,#145995,#145996,#145997,#145998,#145999,#146000,#146001,#146002,
#146003,#146004,#146005,#146006,#146007,#146008,#146009,#146010,#146011,
#146012,#146013,#146014,#146015,#146016,#146017,#146018,#146019,#146020,
#146021,#146022,#146023,#146024,#146025,#146026,#146027,#146028,#146029,
#146030,#146031,#146032,#146033,#146034,#146035,#146036,#146037,#146038,
#146039,#146040,#146041,#146042,#146043,#146044,#146045,#146046,#146047,
#146048,#146049,#146050,#146051,#146052,#146053,#146054,#146055,#146056,
#146057,#146058,#146059,#146060,#146061,#146062,#146063,#146064,#146065,
#146066,#146067,#146068,#146069,#146070),.UNSPECIFIED.,.F.,.F.,(4,3,3,3,
3,3,3,3,3,3,3,3,3,3,3,3,3,3,3,3,3,3,3,3,3,3,3,3,3,3,3,3,3,3,3,3,3,3,3,3,
3,3,4),(65.9734457253857,66.0704340596178,66.1673127975358,66.264132888756,
66.360925426791,66.4577214670338,66.5546134226801,66.6515579893415,66.7486626585398,
66.8029289824295,66.9015271074332,66.9999848902101,67.1002074579827,67.1984870157109,
67.2967335947841,67.3949766778227,67.4966738664649,67.5950582798837,67.6984118561375,
67.8017654323914,67.9003635573952,67.998821340172,68.0990439079447,68.1973234656729,
68.2955700447463,68.3938131277848,68.4955103164269,68.5938947298458,68.6972483060995,
68.8006018823533,68.899200007357,68.9976577901336,69.0978803579063,69.1961599156345,
69.2944064947079,69.3926495777464,69.4943467663886,69.5927311798073,69.6960847560612,
69.7994383323151,69.8980412657737,69.9964918402282,70.0313849530686),
 .UNSPECIFIED.);
#1510=B_SPLINE_CURVE_WITH_KNOTS('',3,(#146071,#146072,#146073,#146074,#146075,
#146076,#146077),.UNSPECIFIED.,.F.,.F.,(4,1,1,1,4),(63.7472418219311,63.8064196325439,
64.8052560825058,65.8040925324676,65.9734457253857),.UNSPECIFIED.);
#1511=B_SPLINE_CURVE_WITH_KNOTS('',3,(#146079,#146080,#146081,#146082,#146083,
#146084,#146085,#146086,#146087,#146088,#146089,#146090,#146091,#146092,
#146093,#146094,#146095,#146096,#146097,#146098,#146099,#146100,#146101,
#146102,#146103,#146104,#146105,#146106,#146107,#146108,#146109,#146110,
#146111,#146112,#146113,#146114,#146115,#146116,#146117,#146118,#146119,
#146120,#146121,#146122,#146123,#146124,#146125,#146126,#146127,#146128,
#146129,#146130,#146131,#146132,#146133,#146134,#146135,#146136,#146137,
#146138,#146139,#146140,#146141,#146142,#146143,#146144,#146145,#146146,
#146147,#146148),.UNSPECIFIED.,.F.,.F.,(4,3,3,3,3,3,3,3,3,3,3,3,3,3,3,3,
3,3,3,3,3,3,3,4),(63.74788580258,63.8461305686218,63.9443750524778,64.0433936268549,
64.1417828266295,64.2411160883078,64.3404493499862,64.4390474749899,64.5375052577665,
64.6377278255392,64.7360073832674,64.8342539623407,64.932497045379,65.0341942340213,
65.1325786474401,65.2359322236941,65.3392857999481,65.4384637976085,65.53749807745,
65.6364173808604,65.7352455972606,65.8340208922139,65.932784900221,65.9734457253857),
 .UNSPECIFIED.);
#1512=B_SPLINE_CURVE_WITH_KNOTS('',3,(#146149,#146150,#146151,#146152,#146153,
#146154,#146155,#146156,#146157,#146158,#146159,#146160,#146161,#146162,
#146163,#146164,#146165,#146166,#146167,#146168,#146169,#146170,#146171,
#146172,#146173,#146174,#146175,#146176,#146177,#146178,#146179,#146180,
#146181,#146182,#146183,#146184,#146185,#146186,#146187,#146188,#146189,
#146190,#146191,#146192,#146193,#146194,#146195,#146196,#146197,#146198,
#146199,#146200,#146201,#146202,#146203,#146204,#146205,#146206,#146207,
#146208,#146209,#146210,#146211,#146212,#146213,#146214,#146215,#146216,
#146217,#146218,#146219,#146220,#146221,#146222,#146223,#146224,#146225,
#146226,#146227,#146228,#146229,#146230,#146231,#146232,#146233,#146234,
#146235,#146236,#146237,#146238,#146239,#146240,#146241,#146242,#146243,
#146244,#146245,#146246,#146247,#146248,#146249,#146250,#146251,#146252,
#146253,#146254,#146255,#146256,#146257,#146258,#146259,#146260,#146261,
#146262,#146263,#146264,#146265,#146266,#146267,#146268,#146269,#146270,
#146271,#146272),.UNSPECIFIED.,.F.,.F.,(4,3,3,3,3,3,3,3,3,3,3,3,3,3,3,3,
3,3,3,3,3,3,3,3,3,3,3,3,3,3,3,3,3,3,3,3,3,3,3,3,3,4),(65.9734457256204,
66.0848798050736,66.1968635637033,66.3094957826818,66.3381222499099,66.4367203749136,
66.5351781576903,66.635400725463,66.7336802831912,66.8319268622646,66.930169945303,
67.0318671339452,67.130251547364,67.2336051236179,67.3369586998718,67.4355568248755,
67.5340146076523,67.634237175425,67.7325167331532,67.8307633122265,67.9290063952651,
68.0307035839073,68.1290879973261,68.2324415735799,68.3357951498337,68.4343932748374,
68.5328510576141,68.6330736253868,68.7313531831149,68.8295997621883,68.9278428452268,
69.029540033869,69.1279244472878,69.2312780235417,69.3346315997956,69.433207943647,
69.5316540255013,69.6299995615608,69.7300684022547,69.8283147727187,69.9292948485276,
70.0302749243365),.UNSPECIFIED.);
#1513=B_SPLINE_CURVE_WITH_KNOTS('',3,(#146278,#146279,#146280,#146281,#146282,
#146283,#146284,#146285),.UNSPECIFIED.,.F.,.F.,(4,1,1,1,1,4),(72.2566310325654,
72.7959476822008,73.7947841321626,74.7936205821245,75.7924570320864,76.3138574567704),
 .UNSPECIFIED.);
#1514=B_SPLINE_CURVE_WITH_KNOTS('',3,(#146286,#146287,#146288,#146289,#146290,
#146291,#146292,#146293,#146294,#146295,#146296,#146297,#146298,#146299,
#146300,#146301,#146302,#146303,#146304,#146305,#146306,#146307,#146308,
#146309,#146310,#146311,#146312,#146313,#146314,#146315,#146316,#146317,
#146318,#146319,#146320,#146321,#146322,#146323,#146324,#146325,#146326,
#146327,#146328,#146329,#146330,#146331,#146332,#146333,#146334,#146335,
#146336,#146337,#146338,#146339,#146340,#146341,#146342,#146343,#146344,
#146345,#146346,#146347,#146348,#146349,#146350,#146351,#146352,#146353,
#146354,#146355),.UNSPECIFIED.,.F.,.F.,(4,3,3,3,3,3,3,3,3,3,3,3,3,3,3,3,
3,3,3,3,3,3,3,4),(70.0313849530686,70.1297027427429,70.2279679449009,70.3262100651504,
70.4244585789561,70.522809277639,70.6212122122823,70.7197874335469,70.798274782277,
70.8968729072806,70.9953306900573,71.09555325783,71.193832815558,71.2920793946316,
71.39032247767,71.4920196663122,71.590404079731,71.6937576559849,71.7971112322389,
71.902834090551,72.0081993817376,72.1133399321502,72.2181701837246,72.2566308185778),
 .UNSPECIFIED.);
#1515=B_SPLINE_CURVE_WITH_KNOTS('',3,(#146357,#146358,#146359,#146360,#146361,
#146362,#146363,#146364,#146365,#146366,#146367,#146368,#146369,#146370,
#146371,#146372,#146373,#146374,#146375,#146376,#146377,#146378,#146379,
#146380,#146381,#146382,#146383,#146384,#146385,#146386,#146387,#146388,
#146389,#146390,#146391,#146392,#146393,#146394,#146395,#146396,#146397,
#146398,#146399,#146400,#146401,#146402,#146403,#146404,#146405,#146406,
#146407,#146408,#146409,#146410,#146411,#146412,#146413,#146414,#146415,
#146416,#146417,#146418,#146419,#146420,#146421,#146422,#146423,#146424,
#146425,#146426),.UNSPECIFIED.,.F.,.F.,(4,3,3,3,3,3,3,3,3,3,3,3,3,3,3,3,
3,3,3,3,3,3,3,4),(70.0302749243365,70.1286604525724,70.2310642511649,70.3334680497574,
70.4320661747611,70.5305239575378,70.6307465253105,70.7290260830387,70.8272726621121,
70.9255157451506,71.0272129337928,71.1255973472116,71.2289509234654,71.3323044997193,
71.4298807240688,71.527317634942,71.6246428433669,71.7219081150619,71.8191441424516,
71.9163815796695,72.013708783522,72.1110862397604,72.208614546431,72.2566310325654),
 .UNSPECIFIED.);
#1516=B_SPLINE_CURVE_WITH_KNOTS('',3,(#146427,#146428,#146429,#146430,#146431,
#146432,#146433,#146434),.UNSPECIFIED.,.F.,.F.,(4,1,1,1,1,4),(72.2566310325654,
72.3311409496812,73.3299773996431,74.3288138496049,75.3276502995668,76.3138964141676),
 .UNSPECIFIED.);
#1517=B_SPLINE_CURVE_WITH_KNOTS('',3,(#146440,#146441,#146442,#146443,#146444,
#146445,#146446,#146447,#146448,#146449,#146450,#146451,#146452,#146453,
#146454,#146455,#146456,#146457,#146458,#146459,#146460,#146461,#146462,
#146463,#146464,#146465,#146466,#146467,#146468,#146469,#146470,#146471,
#146472,#146473,#146474,#146475,#146476,#146477,#146478,#146479,#146480,
#146481,#146482,#146483,#146484,#146485,#146486,#146487,#146488,#146489,
#146490,#146491,#146492,#146493,#146494,#146495,#146496,#146497,#146498,
#146499,#146500,#146501,#146502,#146503,#146504,#146505,#146506,#146507,
#146508,#146509,#146510,#146511,#146512,#146513,#146514,#146515,#146516,
#146517,#146518,#146519,#146520,#146521,#146522,#146523,#146524,#146525,
#146526,#146527,#146528,#146529,#146530,#146531,#146532,#146533,#146534,
#146535,#146536,#146537,#146538,#146539,#146540,#146541,#146542,#146543,
#146544,#146545,#146546,#146547,#146548,#146549,#146550,#146551,#146552,
#146553,#146554,#146555,#146556,#146557,#146558,#146559,#146560,#146561,
#146562,#146563),.UNSPECIFIED.,.F.,.F.,(4,3,3,3,3,3,3,3,3,3,3,3,3,3,3,3,
3,3,3,3,3,3,3,3,3,3,3,3,3,3,3,3,3,3,3,3,3,3,3,3,3,4),(78.5398164398193,
78.6677108218625,78.788966381972,78.8875645069757,78.9860222897523,79.086244857525,
79.1845244152531,79.2827709943265,79.3810140773651,79.4827112660073,79.5810956794261,
79.68444925568,79.7878028319339,79.8864009569376,79.9848587397144,80.085081307487,
80.1833608652152,80.2816074442886,80.379850527327,80.4815477159692,80.579932129388,
80.6832857056419,80.7866392818958,80.8852374068995,80.9836951896763,81.0839177574489,
81.1821973151771,81.2804438942505,81.378686977289,81.4803841659311,81.5787685793499,
81.6821221556038,81.7854757318576,81.8868624838438,81.9852993428627,82.0836395040165,
82.1819125660622,82.2801480557045,82.3784063416034,82.4766798080588,82.5750348031723,
82.5965697477472),.UNSPECIFIED.);
#1518=B_SPLINE_CURVE_WITH_KNOTS('',3,(#146564,#146565,#146566,#146567,#146568,
#146569),.UNSPECIFIED.,.F.,.F.,(4,1,1,4),(76.3138574567704,76.7912934820483,
77.7901299320101,78.539816339745),.UNSPECIFIED.);
#1519=B_SPLINE_CURVE_WITH_KNOTS('',3,(#146571,#146572,#146573,#146574,#146575,
#146576,#146577),.UNSPECIFIED.,.F.,.F.,(4,1,1,1,4),(76.3138964141676,76.3264867495287,
77.3253231994906,78.3241596494524,78.539816339745),.UNSPECIFIED.);
#1520=B_SPLINE_CURVE_WITH_KNOTS('',3,(#146578,#146579,#146580,#146581,#146582,
#146583,#146584,#146585,#146586,#146587,#146588,#146589,#146590,#146591,
#146592,#146593,#146594,#146595,#146596,#146597,#146598,#146599,#146600,
#146601,#146602,#146603,#146604,#146605,#146606,#146607,#146608,#146609,
#146610,#146611,#146612,#146613,#146614,#146615,#146616,#146617,#146618,
#146619,#146620,#146621,#146622,#146623,#146624,#146625,#146626,#146627,
#146628,#146629,#146630,#146631,#146632,#146633,#146634,#146635,#146636,
#146637,#146638,#146639,#146640,#146641,#146642,#146643,#146644,#146645,
#146646,#146647,#146648,#146649,#146650,#146651,#146652,#146653,#146654,
#146655,#146656,#146657,#146658,#146659,#146660,#146661,#146662,#146663,
#146664,#146665,#146666,#146667,#146668,#146669,#146670,#146671,#146672,
#146673,#146674,#146675,#146676,#146677,#146678,#146679,#146680,#146681,
#146682,#146683,#146684,#146685,#146686,#146687,#146688,#146689,#146690,
#146691,#146692,#146693,#146694,#146695,#146696,#146697,#146698,#146699,
#146700,#146701),.UNSPECIFIED.,.F.,.F.,(4,3,3,3,3,3,3,3,3,3,3,3,3,3,3,3,
3,3,3,3,3,3,3,3,3,3,3,3,3,3,3,3,3,3,3,3,3,3,3,3,3,4),(78.539816339745,78.6377138097037,
78.7346673304386,78.8315786913981,78.9284788661295,79.0271081744507,79.1241353185129,
79.2235657089636,79.3229960994143,79.421594224418,79.5200520071949,79.6202745749676,
79.7185541326958,79.8168007117692,79.9150437948077,80.0167409834498,80.1151253968686,
80.2184789731224,80.3218325493762,80.4204306743798,80.5188884571566,80.6191110249293,
80.7173905826574,80.8156371617309,80.9138802447695,81.0155774334116,81.1139618468305,
81.2173154230843,81.3206689993381,81.4192671243418,81.5177249071187,81.6179474748913,
81.7162270326194,81.8144736116928,81.9127166947312,82.0144138833734,82.1127982967921,
82.216151873046,82.3195054492999,82.4180964129948,82.5165362141343,82.5977152891205),
 .UNSPECIFIED.);
#1521=B_SPLINE_CURVE_WITH_KNOTS('',3,(#146707,#146708,#146709,#146710,#146711,
#146712,#146713,#146714),.UNSPECIFIED.,.F.,.F.,(4,1,1,1,1,4),(84.8230070319842,
85.7808215317051,86.779657981667,87.7784944316289,88.7773308815908,88.8809435690823),
 .UNSPECIFIED.);
#1522=B_SPLINE_CURVE_WITH_KNOTS('',3,(#146715,#146716,#146717,#146718,#146719,
#146720,#146721,#146722,#146723,#146724,#146725,#146726,#146727,#146728,
#146729,#146730,#146731,#146732,#146733,#146734,#146735,#146736,#146737,
#146738,#146739,#146740,#146741,#146742,#146743,#146744,#146745,#146746,
#146747,#146748,#146749,#146750,#146751,#146752,#146753,#146754,#146755,
#146756,#146757,#146758,#146759,#146760,#146761,#146762,#146763,#146764,
#146765,#146766,#146767,#146768,#146769,#146770,#146771,#146772,#146773,
#146774,#146775,#146776,#146777,#146778,#146779,#146780,#146781,#146782,
#146783,#146784),.UNSPECIFIED.,.F.,.F.,(4,3,3,3,3,3,3,3,3,3,3,3,3,3,3,3,
3,3,3,3,3,3,3,4),(82.5965697477472,82.6951414136759,82.7843121818195,82.8829103068232,
82.9813680895999,83.0815906573726,83.1798702151008,83.2781167941742,83.3763598772127,
83.4780570658548,83.5764414792737,83.6797950555275,83.7831486317814,83.8817467567851,
83.9802045395618,84.0804271073345,84.1787066650627,84.2769532441361,84.3751963271746,
84.4768935158168,84.5752779292356,84.6786315054894,84.7819850817433,84.8230016469246),
 .UNSPECIFIED.);
#1523=B_SPLINE_CURVE_WITH_KNOTS('',3,(#146786,#146787,#146788,#146789,#146790,
#146791,#146792,#146793,#146794,#146795,#146796,#146797,#146798,#146799,
#146800,#146801,#146802,#146803,#146804,#146805,#146806,#146807,#146808,
#146809,#146810,#146811,#146812,#146813,#146814,#146815,#146816,#146817,
#146818,#146819,#146820,#146821,#146822,#146823,#146824,#146825,#146826,
#146827,#146828,#146829,#146830,#146831,#146832,#146833,#146834,#146835,
#146836,#146837,#146838,#146839,#146840,#146841,#146842,#146843,#146844,
#146845,#146846,#146847,#146848,#146849,#146850,#146851,#146852,#146853,
#146854,#146855),.UNSPECIFIED.,.F.,.F.,(4,3,3,3,3,3,3,3,3,3,3,3,3,3,3,3,
3,3,3,3,3,3,3,4),(82.5977152891205,82.6960046600494,82.7942553301755,82.892496787616,
82.9907585028357,83.0891304591162,83.1875671116892,83.2861621786639,83.3183418992618,
83.4169400242656,83.5153978070425,83.6156203748151,83.7138999325432,83.8121465116165,
83.9103895946547,84.012086783297,84.1104711967157,84.2138247729697,84.3171783492237,
84.4205578302506,84.5236543867486,84.626583481318,84.7292989065995,84.8230016469246),
 .UNSPECIFIED.);
#1524=B_SPLINE_CURVE_WITH_KNOTS('',3,(#146856,#146857,#146858,#146859,#146860,
#146861,#146862,#146863,#146864,#146865,#146866,#146867,#146868,#146869,
#146870,#146871,#146872,#146873,#146874,#146875,#146876,#146877,#146878,
#146879,#146880,#146881,#146882,#146883,#146884,#146885,#146886,#146887,
#146888,#146889,#146890,#146891,#146892,#146893,#146894,#146895,#146896,
#146897,#146898,#146899,#146900,#146901,#146902,#146903,#146904,#146905,
#146906,#146907,#146908,#146909,#146910,#146911,#146912,#146913,#146914,
#146915,#146916,#146917,#146918,#146919,#146920,#146921,#146922,#146923,
#146924,#146925,#146926,#146927,#146928,#146929,#146930,#146931,#146932,
#146933,#146934,#146935,#146936,#146937,#146938,#146939,#146940,#146941,
#146942,#146943,#146944,#146945,#146946,#146947,#146948,#146949,#146950,
#146951,#146952,#146953,#146954,#146955,#146956,#146957,#146958,#146959,
#146960,#146961,#146962,#146963,#146964,#146965,#146966,#146967,#146968,
#146969,#146970,#146971,#146972,#146973,#146974,#146975,#146976,#146977,
#146978,#146979),.UNSPECIFIED.,.F.,.F.,(4,3,3,3,3,3,3,3,3,3,3,3,3,3,3,3,
3,3,3,3,3,3,3,3,3,3,3,3,3,3,3,3,3,3,3,3,3,3,3,3,3,4),(84.8230016472006,
84.9261861619504,85.0296647966981,85.1332945907092,85.2372126194224,85.3160147991856,
85.4146129241893,85.513070706966,85.6132932747387,85.7115728324668,85.8098194115402,
85.9080624945787,86.0097596832209,86.1081440966397,86.2114976728935,86.3148512491474,
86.4134493741511,86.5119071569279,86.6121297247006,86.7104092824287,86.8086558615021,
86.9068989445406,87.0085961331828,87.1069805466016,87.2103341228554,87.3136876991093,
87.412285824113,87.5107436068898,87.6109661746625,87.7092457323906,87.807492311464,
87.9057353945025,88.0074325831447,88.1058169965635,88.2091705728174,88.3125241490712,
88.4111137865017,88.5095698168558,88.6079122101848,88.7061871882861,88.8044419893967,
88.8801389646388),.UNSPECIFIED.);
#1525=B_SPLINE_CURVE_WITH_KNOTS('',3,(#146985,#146986,#146987,#146988,#146989,
#146990,#146991,#146992,#146993,#146994,#146995,#146996,#146997,#146998,
#146999,#147000,#147001,#147002,#147003,#147004,#147005,#147006,#147007,
#147008,#147009,#147010,#147011,#147012,#147013,#147014,#147015,#147016,
#147017,#147018,#147019,#147020,#147021,#147022,#147023,#147024,#147025,
#147026,#147027,#147028,#147029,#147030,#147031,#147032,#147033,#147034,
#147035,#147036,#147037,#147038,#147039,#147040,#147041,#147042,#147043,
#147044,#147045,#147046,#147047,#147048,#147049,#147050,#147051,#147052,
#147053,#147054,#147055,#147056,#147057,#147058,#147059,#147060,#147061,
#147062,#147063,#147064,#147065,#147066,#147067,#147068,#147069,#147070,
#147071,#147072,#147073,#147074,#147075,#147076,#147077,#147078,#147079,
#147080,#147081,#147082,#147083,#147084,#147085,#147086,#147087,#147088,
#147089,#147090,#147091,#147092,#147093,#147094,#147095,#147096,#147097,
#147098,#147099,#147100,#147101,#147102,#147103,#147104,#147105,#147106,
#147107,#147108),.UNSPECIFIED.,.F.,.F.,(4,3,3,3,3,3,3,3,3,3,3,3,3,3,3,3,
3,3,3,3,3,3,3,3,3,3,3,3,3,3,3,3,3,3,3,3,3,3,3,3,3,4),(91.1061869541041,
91.204341964477,91.3024795334307,91.4006291648839,91.4988897541856,91.5972075103077,
91.6957053368613,91.7738402314764,91.8724383564801,91.9708961392568,92.0711187070295,
92.1693982647576,92.2676448438311,92.3658879268694,92.4675851155116,92.5659695289304,
92.6693231051843,92.7726766814383,92.871274806442,92.9697325892187,93.0699551569914,
93.1682347147195,93.2664812937929,93.3647243768313,93.4664215654735,93.5648059788923,
93.6681595551462,93.7715131314001,93.8701112564038,93.9685690391807,94.0687916069534,
94.1670711646815,94.2653177437549,94.3635608267937,94.4652580154358,94.5636424288545,
94.6669960051083,94.770349581362,94.8689185475027,94.9673651079972,95.065708303045,
95.1638473516788),.UNSPECIFIED.);
#1526=B_SPLINE_CURVE_WITH_KNOTS('',3,(#147109,#147110,#147111,#147112,#147113,
#147114),.UNSPECIFIED.,.F.,.F.,(4,1,1,4),(88.8809435690823,89.7761673315526,
90.7750037815145,91.1061798190633),.UNSPECIFIED.);
#1527=B_SPLINE_CURVE_WITH_KNOTS('',3,(#147116,#147117,#147118,#147119,#147120,
#147121,#147122,#147123,#147124,#147125,#147126,#147127,#147128,#147129,
#147130,#147131,#147132,#147133,#147134,#147135,#147136,#147137,#147138,
#147139,#147140,#147141,#147142,#147143,#147144,#147145,#147146,#147147,
#147148,#147149,#147150,#147151,#147152,#147153,#147154,#147155,#147156,
#147157,#147158,#147159,#147160,#147161,#147162,#147163,#147164,#147165,
#147166,#147167,#147168,#147169,#147170,#147171,#147172,#147173,#147174,
#147175,#147176,#147177,#147178,#147179,#147180,#147181,#147182,#147183,
#147184,#147185,#147186,#147187,#147188),.UNSPECIFIED.,.F.,.F.,(4,3,3,3,
3,3,3,3,3,3,3,3,3,3,3,3,3,3,3,3,3,3,3,3,4),(88.8801389646388,88.9783988089623,
89.0767679915452,89.1752004205634,89.2737928081253,89.3113605990331,89.4099587240368,
89.5084165068136,89.6086390745863,89.7069186323145,89.8051652113879,89.9034082944264,
90.0051054830685,90.1034898964873,90.2068434727411,90.3101970489949,90.409695787095,
90.5067185530535,90.6036495481491,90.7005198981799,90.801936662084,90.8988156754797,
90.9957205549586,91.0927209416412,91.1061869537961),.UNSPECIFIED.);
#1528=B_SPLINE_CURVE_WITH_KNOTS('',3,(#147189,#147190,#147191,#147192,#147193,
#147194,#147195,#147196,#147197,#147198,#147199,#147200,#147201,#147202,
#147203,#147204,#147205,#147206,#147207,#147208,#147209,#147210,#147211,
#147212,#147213,#147214,#147215,#147216,#147217,#147218,#147219,#147220,
#147221,#147222,#147223,#147224,#147225,#147226,#147227,#147228,#147229,
#147230,#147231,#147232,#147233,#147234,#147235,#147236,#147237,#147238,
#147239,#147240,#147241,#147242,#147243,#147244,#147245,#147246,#147247,
#147248,#147249,#147250,#147251,#147252,#147253,#147254,#147255,#147256,
#147257,#147258,#147259,#147260,#147261,#147262,#147263,#147264,#147265,
#147266,#147267,#147268,#147269,#147270,#147271,#147272,#147273,#147274,
#147275,#147276,#147277,#147278,#147279,#147280,#147281,#147282,#147283,
#147284,#147285,#147286,#147287,#147288,#147289,#147290,#147291,#147292,
#147293,#147294,#147295,#147296,#147297,#147298,#147299,#147300,#147301,
#147302,#147303,#147304,#147305,#147306,#147307,#147308,#147309,#147310,
#147311,#147312),.UNSPECIFIED.,.F.,.F.,(4,3,3,3,3,3,3,3,3,3,3,3,3,3,3,3,
3,3,3,3,3,3,3,3,3,3,3,3,3,3,3,3,3,3,3,3,3,3,3,3,3,4),(91.1061869541041,
91.246503559673,91.3090334989568,91.4076316239605,91.5060894067373,91.6063119745099,
91.7045915322381,91.8028381113116,91.9010811943501,92.0027783829923,92.101162796411,
92.2045163726649,92.3078699489187,92.4064680739224,92.5049258566991,92.6051484244718,
92.7034279822,92.8016745612733,92.8999176443118,93.001614832954,93.0999992463728,
93.2033528226267,93.3067063988806,93.4053045238843,93.5037623066611,93.6039848744337,
93.7022644321619,93.8005110112352,93.8987540942737,94.0004512829159,94.0988356963347,
94.2021892725885,94.3055428488424,94.4041508037231,94.5025891903028,94.6009312472701,
94.6992065724882,94.7974446925385,94.8957159603378,94.9940021459977,95.0923959722068,
95.1629909686178),.UNSPECIFIED.);
#1529=B_SPLINE_CURVE_WITH_KNOTS('',3,(#147318,#147319,#147320,#147321,#147322,
#147323,#147324,#147325),.UNSPECIFIED.,.F.,.F.,(4,1,1,1,1,4),(97.3893797695142,
97.7668589312476,98.7656953812095,99.7645318311714,100.763368281133,101.445902003198),
 .UNSPECIFIED.);
#1530=B_SPLINE_CURVE_WITH_KNOTS('',3,(#147326,#147327,#147328,#147329,#147330,
#147331,#147332,#147333,#147334,#147335,#147336,#147337,#147338,#147339,
#147340,#147341,#147342,#147343,#147344,#147345,#147346,#147347,#147348,
#147349,#147350,#147351,#147352,#147353,#147354,#147355,#147356,#147357,
#147358,#147359,#147360,#147361,#147362,#147363,#147364,#147365,#147366,
#147367,#147368,#147369,#147370,#147371,#147372,#147373,#147374,#147375,
#147376,#147377,#147378,#147379,#147380,#147381,#147382,#147383,#147384,
#147385,#147386,#147387,#147388,#147389,#147390,#147391,#147392,#147393,
#147394,#147395,#147396,#147397,#147398),.UNSPECIFIED.,.F.,.F.,(4,3,3,3,
3,3,3,3,3,3,3,3,3,3,3,3,3,3,3,3,3,3,3,3,4),(95.1638473516788,95.2620943195394,
95.3603371734009,95.4625493878816,95.5609329012682,95.6593867584473,95.7579931908366,
95.7691860313239,95.8677841563275,95.9662419391037,96.0664645068765,96.1647440646045,
96.2629906436779,96.361233726716,96.4629309153584,96.5613153287773,96.6646689050316,
96.7680224812858,96.8674993725788,96.9668292609825,97.0660403563896,97.1651524247991,
97.2642075332237,97.3632407686266,97.3893722612837),.UNSPECIFIED.);
#1531=B_SPLINE_CURVE_WITH_KNOTS('',3,(#147400,#147401,#147402,#147403,#147404,
#147405,#147406,#147407,#147408,#147409,#147410,#147411,#147412,#147413,
#147414,#147415,#147416,#147417,#147418,#147419,#147420,#147421,#147422,
#147423,#147424,#147425,#147426,#147427,#147428,#147429,#147430,#147431,
#147432,#147433,#147434,#147435,#147436,#147437,#147438,#147439,#147440,
#147441,#147442,#147443,#147444,#147445,#147446,#147447,#147448,#147449,
#147450,#147451,#147452,#147453,#147454,#147455,#147456,#147457,#147458,
#147459,#147460,#147461,#147462,#147463,#147464,#147465,#147466,#147467,
#147468,#147469),.UNSPECIFIED.,.F.,.F.,(4,3,3,3,3,3,3,3,3,3,3,3,3,3,3,3,
3,3,3,3,3,3,3,4),(95.1629909686178,95.2615808482906,95.3043792988043,95.402977423808,
95.5014352065848,95.6016577743574,95.6999373320856,95.7981839111589,95.8964269941975,
95.9981241828397,96.0965085962585,96.1998621725123,96.3032157487662,96.4018138737699,
96.5002716565466,96.6004942243193,96.6987737820475,96.7970203611208,96.8952634441593,
96.9969606328015,97.0953450462203,97.1986986224741,97.302052198728,97.3893722612837),
 .UNSPECIFIED.);
#1532=B_SPLINE_CURVE_WITH_KNOTS('',3,(#147470,#147471,#147472,#147473,#147474,
#147475,#147476,#147477),.UNSPECIFIED.,.F.,.F.,(4,1,1,1,1,4),(97.3893809712563,
98.3008886486899,99.2997250986518,100.298561548614,101.297397998576,101.447496664675),
 .UNSPECIFIED.);
#1533=B_SPLINE_CURVE_WITH_KNOTS('',3,(#147483,#147484,#147485,#147486,#147487,
#147488,#147489,#147490,#147491,#147492,#147493,#147494,#147495,#147496,
#147497,#147498,#147499,#147500,#147501,#147502,#147503,#147504,#147505,
#147506,#147507,#147508,#147509,#147510,#147511,#147512,#147513,#147514,
#147515,#147516,#147517,#147518,#147519,#147520,#147521,#147522,#147523,
#147524,#147525,#147526,#147527,#147528,#147529,#147530,#147531,#147532,
#147533,#147534,#147535,#147536,#147537,#147538,#147539,#147540,#147541,
#147542,#147543,#147544,#147545,#147546,#147547,#147548,#147549,#147550,
#147551,#147552,#147553,#147554,#147555,#147556,#147557,#147558,#147559,
#147560,#147561,#147562,#147563,#147564,#147565,#147566,#147567,#147568,
#147569,#147570,#147571,#147572,#147573,#147574,#147575,#147576,#147577,
#147578,#147579,#147580,#147581,#147582,#147583,#147584,#147585,#147586,
#147587,#147588,#147589,#147590,#147591,#147592,#147593,#147594,#147595,
#147596,#147597,#147598,#147599,#147600,#147601,#147602,#147603,#147604,
#147605,#147606),.UNSPECIFIED.,.F.,.F.,(4,3,3,3,3,3,3,3,3,3,3,3,3,3,3,3,
3,3,3,3,3,3,3,3,3,3,3,3,3,3,3,3,3,3,3,3,3,3,3,3,3,4),(103.672557568463,
103.759877631019,103.858475756023,103.9569335388,104.057156106572,104.1554356643,
104.253682243374,104.351925326412,104.453622515054,104.552006928473,104.655360504727,
104.758714080981,104.857312205985,104.955769988762,105.055992556534,105.154272114262,
105.252518693336,105.350761776374,105.452458965017,105.550843378435,105.654196954689,
105.757550530943,105.856148655947,105.954606438723,106.054829006496,106.153108564224,
106.251355143298,106.349598226336,106.451295414978,106.549679828397,106.653033404651,
106.756386980905,106.854986798947,106.953445809627,107.05178876834,107.150068003063,
107.248313037023,107.346553353057,107.444881222508,107.543251670465,107.641785788185,
107.729756570279),.UNSPECIFIED.);
#1534=B_SPLINE_CURVE_WITH_KNOTS('',3,(#147607,#147608,#147609,#147610,#147611,
#147612),.UNSPECIFIED.,.F.,.F.,(4,1,1,4),(101.445902003198,101.762204731095,
102.761041181057,103.672548858943),.UNSPECIFIED.);
#1535=B_SPLINE_CURVE_WITH_KNOTS('',3,(#147614,#147615,#147616,#147617,#147618,
#147619),.UNSPECIFIED.,.F.,.F.,(4,1,1,4),(101.447496664675,102.296234448537,
103.295070898499,103.672550060648),.UNSPECIFIED.);
#1536=B_SPLINE_CURVE_WITH_KNOTS('',3,(#147620,#147621,#147622,#147623,#147624,
#147625,#147626,#147627,#147628,#147629,#147630,#147631,#147632,#147633,
#147634,#147635,#147636,#147637,#147638,#147639,#147640,#147641,#147642,
#147643,#147644,#147645,#147646,#147647,#147648,#147649,#147650,#147651,
#147652,#147653,#147654,#147655,#147656,#147657,#147658,#147659,#147660,
#147661,#147662,#147663,#147664,#147665,#147666,#147667,#147668,#147669,
#147670,#147671,#147672,#147673,#147674,#147675,#147676,#147677,#147678,
#147679,#147680,#147681,#147682,#147683,#147684,#147685,#147686,#147687,
#147688,#147689,#147690,#147691,#147692,#147693,#147694,#147695,#147696,
#147697,#147698,#147699,#147700,#147701,#147702,#147703,#147704,#147705,
#147706,#147707,#147708,#147709,#147710,#147711,#147712,#147713,#147714,
#147715,#147716,#147717,#147718,#147719,#147720,#147721,#147722,#147723,
#147724,#147725,#147726,#147727,#147728,#147729,#147730,#147731,#147732,
#147733,#147734,#147735,#147736,#147737,#147738,#147739,#147740,#147741,
#147742,#147743,#147744,#147745,#147746),.UNSPECIFIED.,.F.,.F.,(4,3,3,3,
3,3,3,3,3,3,3,3,3,3,3,3,3,3,3,3,3,3,3,3,3,3,3,3,3,3,3,3,3,3,3,3,3,3,3,3,
3,3,4),(103.672557568463,103.771601702603,103.870660322484,103.96976131202,
104.06899945985,104.168318657834,104.267812431338,104.293907348461,104.392505473465,
104.490963256242,104.591185824014,104.689465381742,104.787711960816,104.885955043854,
104.987652232497,105.086036645915,105.189390222169,105.292743798423,105.391341923427,
105.489799706203,105.590022273976,105.688301831704,105.786548410778,105.884791493816,
105.986488682458,106.084873095877,106.188226672131,106.291580248385,106.390178373389,
106.488636156165,106.588858723938,106.687138281666,106.78538486074,106.883627943778,
106.98532513242,107.083709545839,107.187063122093,107.290416698347,107.389023062569,
107.487464394918,107.585810440421,107.684086111431,107.730086441502),
 .UNSPECIFIED.);
#1537=B_SPLINE_CURVE_WITH_KNOTS('',3,(#147752,#147753,#147754,#147755,#147756,
#147757,#147758,#147759,#147760,#147761,#147762,#147763,#147764,#147765,
#147766,#147767,#147768,#147769,#147770,#147771,#147772,#147773,#147774,
#147775,#147776,#147777,#147778,#147779,#147780,#147781,#147782,#147783,
#147784,#147785,#147786,#147787,#147788,#147789,#147790,#147791,#147792,
#147793,#147794,#147795,#147796,#147797,#147798,#147799,#147800,#147801,
#147802,#147803,#147804,#147805,#147806,#147807,#147808,#147809,#147810,
#147811,#147812,#147813,#147814,#147815,#147816,#147817,#147818,#147819,
#147820,#147821,#147822,#147823,#147824,#147825,#147826,#147827,#147828,
#147829,#147830,#147831,#147832,#147833,#147834,#147835,#147836,#147837,
#147838,#147839,#147840,#147841,#147842,#147843,#147844,#147845,#147846,
#147847,#147848,#147849,#147850,#147851,#147852,#147853,#147854,#147855,
#147856,#147857,#147858,#147859,#147860,#147861,#147862,#147863,#147864,
#147865,#147866,#147867,#147868,#147869,#147870,#147871,#147872,#147873,
#147874,#147875,#147876,#147877,#147878),.UNSPECIFIED.,.F.,.F.,(4,3,3,3,
3,3,3,3,3,3,3,3,3,3,3,3,3,3,3,3,3,3,3,3,3,3,3,3,3,3,3,3,3,3,3,3,3,3,3,3,
3,3,4),(109.955742875951,110.055241614051,110.152151423466,110.249014842069,
110.345862894414,110.447330365999,110.544300028994,110.641334438529,110.738518045248,
110.751732780752,110.850330905756,110.948788688533,111.049011256305,111.147290814033,
111.245537393107,111.343780476145,111.445477664787,111.543862078206,111.64721565446,
111.750569230714,111.849167355718,111.947625138494,112.047847706267,112.146127263995,
112.244373843069,112.342616926107,112.44431411475,112.542698528168,112.646052104422,
112.749405680676,112.84800380568,112.946461588456,113.046684156229,113.144963713957,
113.243210293031,113.341453376069,113.443150564711,113.54153497813,113.644888554384,
113.748242130638,113.846836224881,113.945278284699,114.013656826298),
 .UNSPECIFIED.);
#1538=B_SPLINE_CURVE_WITH_KNOTS('',3,(#147879,#147880,#147881,#147882,#147883,
#147884,#147885,#147886,#147887,#147888,#147889,#147890,#147891,#147892,
#147893,#147894,#147895,#147896,#147897,#147898,#147899,#147900,#147901,
#147902,#147903,#147904,#147905,#147906,#147907,#147908,#147909,#147910,
#147911,#147912,#147913,#147914,#147915,#147916,#147917,#147918,#147919,
#147920,#147921,#147922,#147923,#147924,#147925,#147926,#147927,#147928,
#147929,#147930,#147931,#147932,#147933,#147934,#147935,#147936,#147937,
#147938,#147939,#147940,#147941,#147942,#147943,#147944,#147945,#147946,
#147947,#147948),.UNSPECIFIED.,.F.,.F.,(4,3,3,3,3,3,3,3,3,3,3,3,3,3,3,3,
3,3,3,3,3,3,3,4),(107.729756570279,107.755223430866,107.85382155587,107.952279338646,
108.052501906419,108.150781464147,108.24902804322,108.347271126259,108.448968314901,
108.54735272832,108.650706304574,108.754059880828,108.852658005832,108.951115788608,
109.051338356381,109.149617914109,109.247864493183,109.346107576221,109.447804764863,
109.546189178282,109.649542754536,109.75289633079,109.893212936346,109.955742875643),
 .UNSPECIFIED.);
#1539=B_SPLINE_CURVE_WITH_KNOTS('',3,(#147950,#147951,#147952,#147953,#147954,
#147955,#147956,#147957,#147958,#147959,#147960,#147961,#147962,#147963,
#147964,#147965,#147966,#147967,#147968,#147969,#147970,#147971,#147972,
#147973,#147974,#147975,#147976,#147977,#147978,#147979,#147980,#147981,
#147982,#147983,#147984,#147985,#147986,#147987,#147988,#147989,#147990,
#147991,#147992,#147993,#147994,#147995,#147996,#147997,#147998,#147999,
#148000,#148001,#148002,#148003,#148004,#148005,#148006,#148007,#148008,
#148009,#148010,#148011,#148012,#148013,#148014,#148015,#148016,#148017,
#148018,#148019),.UNSPECIFIED.,.F.,.F.,(4,3,3,3,3,3,3,3,3,3,3,3,3,3,3,3,
3,3,3,3,3,3,3,4),(107.730086441502,107.828327805401,107.926578904311,108.024934190854,
108.123344715731,108.221924060079,108.289253148309,108.387851273313,108.486309056089,
108.586531623862,108.68481118159,108.783057760664,108.881300843702,108.982998032344,
109.081382445763,109.184736022017,109.288089598271,109.386591328535,109.484956309732,
109.583214317041,109.681399820023,109.779540599733,109.877698313764,109.955742875643),
 .UNSPECIFIED.);
#1540=B_SPLINE_CURVE_WITH_KNOTS('',3,(#148020,#148021,#148022,#148023,#148024,
#148025,#148026,#148027),.UNSPECIFIED.,.F.,.F.,(4,1,1,1,1,4),(109.955750010146,
110.286926048232,111.285762498194,112.284598948156,113.283435398118,114.01218696335),
 .UNSPECIFIED.);
#1541=B_SPLINE_CURVE_WITH_KNOTS('',3,(#148033,#148034,#148035,#148036,#148037,
#148038,#148039,#148040,#148041,#148042,#148043,#148044,#148045,#148046,
#148047,#148048,#148049,#148050,#148051,#148052,#148053,#148054,#148055,
#148056,#148057,#148058,#148059,#148060,#148061,#148062,#148063,#148064,
#148065,#148066,#148067,#148068,#148069,#148070,#148071,#148072,#148073,
#148074,#148075,#148076,#148077,#148078,#148079,#148080,#148081,#148082,
#148083,#148084,#148085,#148086,#148087,#148088,#148089,#148090,#148091,
#148092,#148093,#148094,#148095,#148096,#148097,#148098,#148099,#148100,
#148101,#148102,#148103,#148104,#148105,#148106,#148107,#148108,#148109,
#148110,#148111,#148112,#148113,#148114,#148115,#148116,#148117,#148118,
#148119,#148120,#148121,#148122,#148123,#148124,#148125,#148126,#148127,
#148128,#148129,#148130,#148131,#148132,#148133,#148134,#148135,#148136,
#148137,#148138,#148139,#148140,#148141,#148142,#148143,#148144,#148145,
#148146,#148147,#148148,#148149,#148150,#148151,#148152,#148153,#148154,
#148155,#148156),.UNSPECIFIED.,.F.,.F.,(4,3,3,3,3,3,3,3,3,3,3,3,3,3,3,3,
3,3,3,3,3,3,3,3,3,3,3,3,3,3,3,3,3,3,3,3,3,3,3,3,3,4),(116.238928182823,
116.341566510357,116.44447107289,116.547509821617,116.650828963887,116.744751480523,
116.843349605527,116.941807388303,117.042029956076,117.140309513804,117.238556092877,
117.336799175916,117.438496364558,117.536880777977,117.640234354231,117.743587930485,
117.842186055489,117.940643838265,118.040866406038,118.139145963766,118.23739254284,
118.335635625878,118.437332814521,118.535717227939,118.639070804193,118.742424380447,
118.841022505451,118.939480288228,119.039702856,119.137982413728,119.236228992802,
119.33447207584,119.436169264482,119.534553677901,119.637907254155,119.741260830409,
119.839851983056,119.938309194702,120.036651331111,120.134925920019,120.233176074199,
120.296103415561),.UNSPECIFIED.);
#1542=B_SPLINE_CURVE_WITH_KNOTS('',3,(#148157,#148158,#148159,#148160,#148161,
#148162,#148163,#148164,#148165,#148166,#148167,#148168,#148169,#148170,
#148171,#148172,#148173,#148174,#148175,#148176,#148177,#148178,#148179,
#148180,#148181,#148182,#148183,#148184,#148185,#148186,#148187,#148188,
#148189,#148190,#148191,#148192,#148193,#148194,#148195,#148196,#148197,
#148198,#148199,#148200,#148201,#148202,#148203,#148204,#148205,#148206,
#148207,#148208,#148209,#148210,#148211,#148212,#148213,#148214,#148215,
#148216,#148217,#148218,#148219,#148220,#148221,#148222,#148223,#148224,
#148225,#148226),.UNSPECIFIED.,.F.,.F.,(4,3,3,3,3,3,3,3,3,3,3,3,3,3,3,3,
3,3,3,3,3,3,3,4),(114.013656826298,114.111953403897,114.210207440612,114.308448428809,
114.406705839748,114.505071330138,114.60349806933,114.702086924788,114.747078580599,
114.845676705603,114.944134488379,115.044357056152,115.14263661388,115.240883192953,
115.339126275991,115.440823464634,115.539207878053,115.642561454307,115.745915030561,
115.849888759331,115.953561696348,116.057054365164,116.160309146371,116.238928182547),
 .UNSPECIFIED.);
#1543=B_SPLINE_CURVE_WITH_KNOTS('',3,(#148228,#148229,#148230,#148231,#148232,
#148233),.UNSPECIFIED.,.F.,.F.,(4,1,1,4),(114.01218696335,114.28227184808,
115.281108298042,116.238922797526),.UNSPECIFIED.);
#1544=B_SPLINE_CURVE_WITH_KNOTS('',3,(#148234,#148235,#148236,#148237,#148238,
#148239,#148240,#148241,#148242,#148243,#148244,#148245,#148246,#148247,
#148248,#148249,#148250,#148251,#148252,#148253,#148254,#148255,#148256,
#148257,#148258,#148259,#148260,#148261,#148262,#148263,#148264,#148265,
#148266,#148267,#148268,#148269,#148270,#148271,#148272,#148273,#148274,
#148275,#148276,#148277,#148278,#148279,#148280,#148281,#148282,#148283,
#148284,#148285,#148286,#148287,#148288,#148289,#148290,#148291,#148292,
#148293,#148294,#148295,#148296,#148297,#148298,#148299,#148300,#148301,
#148302,#148303,#148304,#148305,#148306,#148307,#148308,#148309,#148310,
#148311,#148312,#148313,#148314,#148315,#148316,#148317,#148318,#148319,
#148320,#148321,#148322,#148323,#148324,#148325,#148326,#148327,#148328,
#148329,#148330,#148331,#148332,#148333,#148334,#148335,#148336,#148337,
#148338,#148339,#148340,#148341,#148342,#148343,#148344,#148345,#148346,
#148347,#148348,#148349,#148350,#148351,#148352,#148353,#148354,#148355,
#148356,#148357,#148358,#148359,#148360),.UNSPECIFIED.,.F.,.F.,(4,3,3,3,
3,3,3,3,3,3,3,3,3,3,3,3,3,3,3,3,3,3,3,3,3,3,3,3,3,3,3,3,3,3,3,3,3,3,3,3,
3,3,4),(116.238928182823,116.279944748004,116.378542873008,116.477000655784,
116.577223223557,116.675502781285,116.773749360358,116.871992443397,116.973689632039,
117.072074045458,117.175427621712,117.278781197966,117.37737932297,117.475837105746,
117.576059673519,117.674339231247,117.77258581032,117.870828893359,117.972526082001,
118.07091049542,118.174264071673,118.277617647927,118.376215772931,118.474673555707,
118.57489612348,118.673175681208,118.771422260281,118.86966534332,118.971362531962,
119.069746945381,119.173100521635,119.276454097889,119.375052222893,119.47351000567,
119.573732573442,119.67201213117,119.770258710244,119.868501793282,119.970198981925,
120.068583395343,120.171936971597,120.275290547851,120.296396934293),
 .UNSPECIFIED.);
#1545=B_SPLINE_CURVE_WITH_KNOTS('',3,(#148366,#148367,#148368,#148369,#148370,
#148371,#148372,#148373),.UNSPECIFIED.,.F.,.F.,(4,1,1,1,1,4),(122.522113490002,
122.737770180294,123.736606630256,124.735443080218,125.73427953018,126.57866683563),
 .UNSPECIFIED.);
#1546=B_SPLINE_CURVE_WITH_KNOTS('',3,(#148374,#148375,#148376,#148377,#148378,
#148379,#148380,#148381,#148382,#148383,#148384,#148385,#148386,#148387,
#148388,#148389,#148390,#148391,#148392,#148393,#148394,#148395,#148396,
#148397,#148398,#148399,#148400,#148401,#148402,#148403,#148404,#148405,
#148406,#148407,#148408,#148409,#148410,#148411,#148412,#148413,#148414,
#148415,#148416,#148417,#148418,#148419,#148420,#148421,#148422,#148423,
#148424,#148425,#148426,#148427,#148428,#148429,#148430,#148431,#148432,
#148433,#148434,#148435,#148436,#148437,#148438,#148439,#148440,#148441,
#148442,#148443),.UNSPECIFIED.,.F.,.F.,(4,3,3,3,3,3,3,3,3,3,3,3,3,3,3,3,
3,3,3,3,3,3,3,4),(120.296103415561,120.394359169329,120.492722080471,120.59114479427,
120.689731208205,120.740097280371,120.838695405375,120.937153188151,121.037375755924,
121.135655313652,121.233901892726,121.332144975764,121.433842164406,121.532226577825,
121.635580154079,121.738933730333,121.836831200292,121.933909156543,122.030894120917,
122.127817176647,122.226391254986,122.323316910845,122.422715200424,122.522113490002),
 .UNSPECIFIED.);
#1547=B_SPLINE_CURVE_WITH_KNOTS('',3,(#148445,#148446,#148447,#148448,#148449,
#148450,#148451,#148452,#148453,#148454,#148455,#148456,#148457,#148458,
#148459,#148460,#148461,#148462,#148463,#148464,#148465,#148466,#148467,
#148468,#148469,#148470,#148471,#148472,#148473,#148474,#148475,#148476,
#148477,#148478,#148479,#148480,#148481,#148482,#148483,#148484,#148485,
#148486,#148487,#148488,#148489,#148490,#148491,#148492,#148493,#148494,
#148495,#148496,#148497,#148498,#148499,#148500,#148501,#148502,#148503,
#148504,#148505,#148506,#148507,#148508,#148509,#148510,#148511),
 .UNSPECIFIED.,.F.,.F.,(4,3,3,3,3,3,3,3,3,3,3,3,3,3,3,3,3,3,3,3,3,3,4),
(120.296396934293,120.394962268417,120.493394294901,120.59172185699,120.689992675083,
120.788236261167,120.886482093345,120.984827570553,121.083221557777,121.181792244442,
121.274126997813,121.372725122817,121.471182905593,121.571405473366,121.669685031094,
121.767931610168,121.866174693206,121.967871881848,122.066256295267,122.169609871521,
122.272963447775,122.400857829821,122.52211338997),.UNSPECIFIED.);
#1548=B_SPLINE_CURVE_WITH_KNOTS('',3,(#148512,#148513,#148514,#148515,#148516,
#148517,#148518,#148519),.UNSPECIFIED.,.F.,.F.,(4,1,1,1,1,4),(122.522113490002,
123.271799897737,124.270636347699,125.269472797661,126.268309247622,126.58028576884),
 .UNSPECIFIED.);
#1549=B_SPLINE_CURVE_WITH_KNOTS('',3,(#148525,#148526,#148527,#148528,#148529,
#148530,#148531,#148532,#148533,#148534,#148535,#148536,#148537,#148538,
#148539,#148540,#148541,#148542,#148543,#148544,#148545,#148546,#148547,
#148548,#148549,#148550,#148551,#148552,#148553,#148554,#148555,#148556,
#148557,#148558,#148559,#148560,#148561,#148562,#148563,#148564,#148565,
#148566,#148567,#148568,#148569,#148570,#148571,#148572,#148573,#148574,
#148575,#148576,#148577,#148578,#148579,#148580,#148581,#148582,#148583,
#148584,#148585,#148586,#148587,#148588,#148589,#148590,#148591,#148592,
#148593,#148594,#148595,#148596,#148597,#148598,#148599,#148600,#148601,
#148602,#148603,#148604,#148605,#148606,#148607,#148608,#148609,#148610,
#148611,#148612,#148613,#148614,#148615,#148616,#148617,#148618,#148619,
#148620,#148621,#148622,#148623,#148624,#148625,#148626,#148627,#148628,
#148629,#148630,#148631,#148632,#148633,#148634,#148635,#148636,#148637,
#148638,#148639,#148640,#148641,#148642,#148643,#148644,#148645,#148646,
#148647,#148648,#148649,#148650,#148651),.UNSPECIFIED.,.F.,.F.,(4,3,3,3,
3,3,3,3,3,3,3,3,3,3,3,3,3,3,3,3,3,3,3,3,3,3,3,3,3,3,3,3,3,3,3,3,3,3,3,3,
3,3,4),(128.805298797182,128.902840431273,129.000250613517,129.097560812666,
129.194818343698,129.292053887497,129.389298094495,129.486642967568,129.584044330746,
129.68160592498,129.729625330028,129.828223455032,129.926681237808,130.026903805581,
130.125183363309,130.223429942382,130.321673025421,130.423370214063,130.521754627482,
130.625108203735,130.728461779989,130.827059904993,130.92551768777,131.025740255542,
131.12401981327,131.222266392344,131.320509475382,131.422206664024,131.520591077443,
131.623944653697,131.727298229951,131.825896354955,131.924354137731,132.024576705504,
132.122856263232,132.221102842306,132.319345925344,132.421043113987,132.519427527405,
132.622781103659,132.726134679913,132.8247266372,132.863178388799),
 .UNSPECIFIED.);
#1550=B_SPLINE_CURVE_WITH_KNOTS('',3,(#148652,#148653,#148654,#148655,#148656,
#148657,#148658),.UNSPECIFIED.,.F.,.F.,(4,1,1,1,4),(126.57866683563,126.733115980142,
127.731952430104,128.730788880066,128.805298797182),.UNSPECIFIED.);
#1551=B_SPLINE_CURVE_WITH_KNOTS('',3,(#148660,#148661,#148662,#148663,#148664,
#148665),.UNSPECIFIED.,.F.,.F.,(4,1,1,4),(126.58028576884,127.267145697584,
128.265982147546,128.805298797182),.UNSPECIFIED.);
#1552=B_SPLINE_CURVE_WITH_KNOTS('',3,(#148666,#148667,#148668,#148669,#148670,
#148671,#148672,#148673,#148674,#148675,#148676,#148677,#148678,#148679,
#148680,#148681,#148682,#148683,#148684,#148685,#148686,#148687,#148688,
#148689,#148690,#148691,#148692,#148693,#148694,#148695,#148696,#148697,
#148698,#148699,#148700,#148701,#148702,#148703,#148704,#148705,#148706,
#148707,#148708,#148709,#148710,#148711,#148712,#148713,#148714,#148715,
#148716,#148717,#148718,#148719,#148720,#148721,#148722,#148723,#148724,
#148725,#148726,#148727,#148728,#148729,#148730,#148731,#148732,#148733,
#148734,#148735,#148736,#148737,#148738,#148739,#148740,#148741,#148742,
#148743,#148744,#148745,#148746,#148747,#148748,#148749,#148750,#148751,
#148752,#148753,#148754,#148755,#148756,#148757,#148758,#148759,#148760,
#148761,#148762,#148763,#148764,#148765,#148766,#148767,#148768,#148769,
#148770,#148771,#148772,#148773,#148774,#148775,#148776,#148777,#148778,
#148779,#148780,#148781,#148782,#148783,#148784,#148785,#148786,#148787,
#148788,#148789),.UNSPECIFIED.,.F.,.F.,(4,3,3,3,3,3,3,3,3,3,3,3,3,3,3,3,
3,3,3,3,3,3,3,3,3,3,3,3,3,3,3,3,3,3,3,3,3,3,3,3,3,4),(128.80529901116,128.910085619871,
129.015255759151,129.120630109632,129.226318351047,129.264818597508,129.363416722512,
129.461874505288,129.562097073061,129.660376630789,129.758623209863,129.856866292901,
129.958563481543,130.056947894962,130.160301471216,130.26365504747,130.362253172474,
130.46071095525,130.560933523023,130.659213080751,130.757459659825,130.855702742863,
130.957399931505,131.055784344924,131.159137921178,131.262491497432,131.361089622436,
131.459547405213,131.559769972985,131.658049530713,131.756296109787,131.854539192825,
131.956236381468,132.054620794886,132.15797437114,132.261327947394,132.359913784698,
132.458366887933,132.559360491667,132.657635694893,132.75998849888,132.862341302868),
 .UNSPECIFIED.);
#1553=B_SPLINE_CURVE_WITH_KNOTS('',3,(#148795,#148796,#148797,#148798,#148799,
#148800,#148801,#148802,#148803,#148804,#148805,#148806,#148807,#148808,
#148809,#148810,#148811,#148812,#148813,#148814,#148815,#148816,#148817,
#148818,#148819,#148820,#148821,#148822,#148823,#148824,#148825,#148826,
#148827,#148828,#148829,#148830,#148831,#148832,#148833,#148834,#148835,
#148836,#148837,#148838,#148839,#148840,#148841,#148842,#148843,#148844,
#148845,#148846,#148847,#148848,#148849,#148850,#148851,#148852,#148853,
#148854,#148855,#148856,#148857,#148858,#148859,#148860,#148861,#148862,
#148863,#148864,#148865,#148866,#148867,#148868,#148869,#148870,#148871,
#148872,#148873,#148874,#148875,#148876,#148877,#148878,#148879,#148880,
#148881,#148882,#148883,#148884,#148885,#148886,#148887,#148888,#148889,
#148890,#148891,#148892,#148893,#148894,#148895,#148896,#148897,#148898,
#148899,#148900,#148901,#148902,#148903,#148904,#148905,#148906,#148907,
#148908,#148909,#148910,#148911,#148912,#148913,#148914,#148915,#148916,
#148917,#148918,#148919,#148920,#148921),.UNSPECIFIED.,.F.,.F.,(4,3,3,3,
3,3,3,3,3,3,3,3,3,3,3,3,3,3,3,3,3,3,3,3,3,3,3,3,3,3,3,3,3,3,3,3,3,3,3,3,
3,3,4),(135.088484104361,135.187254556185,135.286029876603,135.384838499173,
135.483776463585,135.582788468008,135.681976179006,135.722644029799,135.821242154803,
135.919699937579,136.019922505352,136.11820206308,136.216448642154,136.314691725192,
136.416388913834,136.514773327253,136.618126903507,136.721480479761,136.820078604765,
136.918536387541,137.018758955314,137.117038513042,137.215285092115,137.313528175154,
137.415225363796,137.513609777215,137.616963353469,137.720316929723,137.818915054727,
137.917372837503,138.017595405276,138.115874963004,138.214121542077,138.312364625116,
138.414061813758,138.512446227177,138.61579980343,138.719153379684,138.817761602492,
138.916204188038,139.014551352302,139.112826031212,139.14605062869),
 .UNSPECIFIED.);
#1554=B_SPLINE_CURVE_WITH_KNOTS('',3,(#148922,#148923,#148924,#148925,#148926,
#148927,#148928,#148929,#148930,#148931,#148932,#148933,#148934,#148935,
#148936,#148937,#148938,#148939,#148940,#148941,#148942,#148943,#148944,
#148945,#148946,#148947,#148948,#148949,#148950,#148951,#148952,#148953,
#148954,#148955,#148956,#148957,#148958,#148959,#148960,#148961,#148962,
#148963,#148964,#148965,#148966,#148967,#148968,#148969,#148970,#148971,
#148972,#148973,#148974,#148975,#148976,#148977,#148978,#148979,#148980,
#148981,#148982,#148983,#148984,#148985,#148986,#148987,#148988,#148989,
#148990,#148991),.UNSPECIFIED.,.F.,.F.,(4,3,3,3,3,3,3,3,3,3,3,3,3,3,3,3,
3,3,3,3,3,3,3,4),(132.863178388799,132.961590306302,133.059905711635,133.158169582967,
133.256411424373,133.354660710732,133.453012816327,133.551418102536,133.649994575943,
133.724971129875,133.823569254879,133.922027037656,134.022249605428,134.120529163156,
134.21877574223,134.317018825268,134.41871601391,134.517100427329,134.620454003583,
134.723807579837,134.8363385207,134.948409000641,135.059693750753,135.088484104126),
 .UNSPECIFIED.);
#1555=B_SPLINE_CURVE_WITH_KNOTS('',3,(#148993,#148994,#148995,#148996,#148997,
#148998,#148999,#149000,#149001,#149002,#149003,#149004,#149005,#149006,
#149007,#149008,#149009,#149010,#149011,#149012,#149013,#149014,#149015,
#149016,#149017,#149018,#149019,#149020,#149021,#149022,#149023,#149024,
#149025,#149026,#149027,#149028,#149029,#149030,#149031,#149032,#149033,
#149034,#149035,#149036,#149037,#149038,#149039,#149040,#149041,#149042,
#149043,#149044,#149045,#149046,#149047,#149048,#149049,#149050,#149051,
#149052,#149053,#149054,#149055,#149056,#149057,#149058,#149059,#149060,
#149061,#149062),.UNSPECIFIED.,.F.,.F.,(4,3,3,3,3,3,3,3,3,3,3,3,3,3,3,3,
3,3,3,3,3,3,3,4),(132.862341302868,132.96179707649,133.060185482975,133.160174940165,
133.260164397356,133.35876252236,133.457220305136,133.557442872909,133.655722430637,
133.75396900971,133.852212092749,133.953909281391,134.05229369481,134.155647271063,
134.259000847317,134.356128675186,134.453094160804,134.549968416922,134.646782617699,
134.743567858737,134.840399971759,134.937256811785,135.034231214224,135.088484104361),
 .UNSPECIFIED.);
#1556=B_SPLINE_CURVE_WITH_KNOTS('',3,(#149063,#149064,#149065,#149066,#149067,
#149068,#149069,#149070),.UNSPECIFIED.,.F.,.F.,(4,1,1,1,1,4),(135.088484104361,
135.257837297279,136.256673747241,137.255510197203,138.254346647165,139.145213405918),
 .UNSPECIFIED.);
#1557=B_SPLINE_CURVE_WITH_KNOTS('',3,(#149076,#149077,#149078,#149079,#149080,
#149081,#149082,#149083,#149084,#149085,#149086,#149087,#149088,#149089,
#149090,#149091,#149092,#149093,#149094,#149095,#149096,#149097,#149098,
#149099,#149100,#149101,#149102,#149103,#149104,#149105,#149106,#149107,
#149108,#149109,#149110,#149111,#149112,#149113,#149114,#149115,#149116,
#149117,#149118,#149119,#149120,#149121,#149122,#149123,#149124,#149125,
#149126,#149127,#149128,#149129,#149130,#149131,#149132,#149133,#149134,
#149135,#149136,#149137,#149138,#149139,#149140,#149141,#149142,#149143,
#149144,#149145,#149146,#149147,#149148,#149149,#149150,#149151,#149152,
#149153,#149154,#149155,#149156,#149157,#149158,#149159,#149160,#149161,
#149162,#149163,#149164,#149165,#149166,#149167,#149168,#149169,#149170,
#149171,#149172,#149173,#149174,#149175,#149176,#149177,#149178,#149179,
#149180,#149181,#149182,#149183,#149184,#149185,#149186,#149187,#149188,
#149189,#149190,#149191,#149192,#149193,#149194,#149195,#149196,#149197,
#149198,#149199),.UNSPECIFIED.,.F.,.F.,(4,3,3,3,3,3,3,3,3,3,3,3,3,3,3,3,
3,3,3,3,3,3,3,3,3,3,3,3,3,3,3,3,3,3,3,3,3,3,3,3,3,4),(141.371669411768,
141.485016004534,141.600339367052,141.71566272957,141.814260854574,141.91271863735,
142.012941205123,142.111220762851,142.209467341925,142.307710424963,142.409407613605,
142.507792027024,142.611145603278,142.714499179532,142.813097304536,142.911555087312,
143.011777655085,143.110057212813,143.208303791887,143.306546874925,143.408244063567,
143.506628476986,143.60998205324,143.713335629494,143.811933754498,143.910391537274,
144.010614105047,144.108893662775,144.207140241849,144.305383324887,144.407080513529,
144.505464926948,144.608818503202,144.712172079456,144.81074660183,144.909191401417,
145.007536191857,145.105810581995,145.204060790383,145.302298022116,145.400579631087,
145.428467348202),.UNSPECIFIED.);
#1558=B_SPLINE_CURVE_WITH_KNOTS('',3,(#149200,#149201,#149202,#149203,#149204,
#149205,#149206,#149207,#149208,#149209,#149210,#149211,#149212,#149213,
#149214,#149215,#149216,#149217,#149218,#149219,#149220,#149221,#149222,
#149223,#149224,#149225,#149226,#149227,#149228,#149229,#149230,#149231,
#149232,#149233,#149234,#149235,#149236,#149237,#149238,#149239,#149240,
#149241,#149242,#149243,#149244,#149245,#149246,#149247,#149248,#149249,
#149250,#149251,#149252,#149253,#149254,#149255,#149256,#149257,#149258,
#149259,#149260,#149261,#149262,#149263,#149264,#149265,#149266,#149267,
#149268,#149269),.UNSPECIFIED.,.F.,.F.,(4,3,3,3,3,3,3,3,3,3,3,3,3,3,3,3,
3,3,3,3,3,3,3,4),(139.14605062869,139.244292891595,139.342541058438,139.440891113436,
139.539292964499,139.637867616823,139.717989829646,139.81658795465,139.915045737426,
140.015268305199,140.113547862927,140.211794442001,140.310037525039,140.411734713681,
140.5101191271,140.613472703354,140.716826279608,140.815569227393,140.914173010821,
141.012667061738,141.11108183093,141.209449097701,141.307822396311,141.371669411541),
 .UNSPECIFIED.);
#1559=B_SPLINE_CURVE_WITH_KNOTS('',3,(#149271,#149272,#149273,#149274,#149275,
#149276,#149277),.UNSPECIFIED.,.F.,.F.,(4,1,1,1,4),(139.145213405918,139.253183097127,
140.252019547089,141.250855997051,141.371669411541),.UNSPECIFIED.);
#1560=B_SPLINE_CURVE_WITH_KNOTS('',3,(#149278,#149279,#149280,#149281,#149282,
#149283,#149284,#149285,#149286,#149287,#149288,#149289,#149290,#149291,
#149292,#149293,#149294,#149295,#149296,#149297,#149298,#149299,#149300,
#149301,#149302,#149303,#149304,#149305,#149306,#149307,#149308,#149309,
#149310,#149311,#149312,#149313,#149314,#149315,#149316,#149317,#149318,
#149319,#149320,#149321,#149322,#149323,#149324,#149325,#149326,#149327,
#149328,#149329,#149330,#149331,#149332,#149333,#149334,#149335,#149336,
#149337,#149338,#149339,#149340,#149341,#149342,#149343,#149344,#149345,
#149346,#149347,#149348,#149349,#149350,#149351,#149352,#149353,#149354,
#149355,#149356,#149357,#149358,#149359,#149360,#149361,#149362,#149363,
#149364,#149365,#149366,#149367,#149368,#149369,#149370,#149371,#149372,
#149373,#149374,#149375,#149376,#149377,#149378,#149379,#149380,#149381,
#149382,#149383,#149384,#149385,#149386,#149387,#149388,#149389,#149390,
#149391,#149392,#149393,#149394,#149395,#149396,#149397,#149398,#149399,
#149400,#149401),.UNSPECIFIED.,.F.,.F.,(4,3,3,3,3,3,3,3,3,3,3,3,3,3,3,3,
3,3,3,3,3,3,3,3,3,3,3,3,3,3,3,3,3,3,3,3,3,3,3,3,3,4),(141.371669411541,
141.468831254161,141.566438903267,141.66339620349,141.760311911022,141.857216996242,
141.955335858934,142.052368429038,142.151030438025,142.249692447012,142.348290572016,
142.446748354792,142.546970922565,142.645250480293,142.743497059366,142.841740142405,
142.943437331047,143.041821744466,143.14517532072,143.248528896974,143.347127021978,
143.445584804755,143.545807372527,143.644086930255,143.742333509329,143.840576592367,
143.942273781009,144.040658194428,144.144011770682,144.247365346936,144.34596347194,
144.444421254716,144.544643822489,144.642923380217,144.74116995929,144.839413042329,
144.941110230971,145.03949464439,145.142848220644,145.246201796898,145.344774861151,
145.429604694147),.UNSPECIFIED.);
#1561=B_SPLINE_CURVE_WITH_KNOTS('',3,(#149407,#149408,#149409,#149410,#149411,
#149412,#149413,#149414,#149415),.UNSPECIFIED.,.F.,.F.,(4,1,1,1,1,1,4),
(147.65485471872,147.708681429341,148.707517879303,149.706354329265,150.705190779227,
151.704027229189,151.712252778999),.UNSPECIFIED.);
#1562=B_SPLINE_CURVE_WITH_KNOTS('',3,(#149416,#149417,#149418,#149419,#149420,
#149421,#149422,#149423,#149424,#149425,#149426,#149427,#149428,#149429,
#149430,#149431,#149432,#149433,#149434,#149435,#149436,#149437,#149438,
#149439,#149440,#149441,#149442,#149443,#149444,#149445,#149446,#149447,
#149448,#149449,#149450,#149451,#149452,#149453,#149454,#149455,#149456,
#149457,#149458,#149459,#149460,#149461,#149462,#149463,#149464,#149465,
#149466,#149467,#149468,#149469,#149470,#149471,#149472,#149473,#149474,
#149475,#149476,#149477,#149478,#149479,#149480,#149481,#149482,#149483,
#149484,#149485),.UNSPECIFIED.,.F.,.F.,(4,3,3,3,3,3,3,3,3,3,3,3,3,3,3,3,
3,3,3,3,3,3,3,4),(145.428467348202,145.52686564106,145.625438462383,145.711008529418,
145.809606654422,145.908064437198,146.008287004971,146.106566562699,146.204813141772,
146.303056224811,146.404753413453,146.503137826872,146.606491403125,146.709844979379,
146.807643480436,146.905302408374,147.002849316603,147.100335701354,147.197792033696,
147.295248746519,147.3927980835,147.490396206244,147.588155506493,147.65485471872),
 .UNSPECIFIED.);
#1563=B_SPLINE_CURVE_WITH_KNOTS('',3,(#149487,#149488,#149489,#149490,#149491,
#149492,#149493,#149494,#149495,#149496,#149497,#149498,#149499,#149500,
#149501,#149502,#149503,#149504,#149505,#149506,#149507,#149508,#149509,
#149510,#149511,#149512,#149513,#149514,#149515,#149516,#149517,#149518,
#149519,#149520,#149521,#149522,#149523,#149524,#149525,#149526,#149527,
#149528,#149529,#149530,#149531,#149532,#149533,#149534,#149535,#149536,
#149537,#149538,#149539,#149540,#149541,#149542,#149543,#149544,#149545,
#149546,#149547,#149548,#149549,#149550,#149551,#149552,#149553,#149554,
#149555,#149556),.UNSPECIFIED.,.F.,.F.,(4,3,3,3,3,3,3,3,3,3,3,3,3,3,3,3,
3,3,3,3,3,3,3,4),(145.429604694147,145.531533888236,145.629819464068,145.728068476452,
145.826310411335,145.924574738934,146.022950488803,146.121392854414,146.219991618488,
146.24503824686,146.343636371864,146.442094154641,146.542316722413,146.640596280141,
146.738842859215,146.837085942253,146.938783130895,147.037167544314,147.140521120568,
147.243874696822,147.352569174392,147.460952550046,147.568802109382,147.654854305399),
 .UNSPECIFIED.);
#1564=B_SPLINE_CURVE_WITH_KNOTS('',3,(#149557,#149558,#149559,#149560,#149561,
#149562,#149563,#149564),.UNSPECIFIED.,.F.,.F.,(4,1,1,1,1,4),(147.65485471872,
148.242711146784,149.241547596746,150.240384046707,151.239220496669,151.712342700426),
 .UNSPECIFIED.);
#1565=B_SPLINE_CURVE_WITH_KNOTS('',3,(#149570,#149571,#149572,#149573,#149574,
#149575,#149576,#149577,#149578,#149579,#149580,#149581,#149582,#149583,
#149584,#149585,#149586,#149587,#149588,#149589,#149590,#149591,#149592,
#149593,#149594,#149595,#149596,#149597,#149598,#149599,#149600,#149601,
#149602,#149603,#149604,#149605,#149606,#149607,#149608,#149609,#149610,
#149611,#149612,#149613,#149614,#149615,#149616,#149617,#149618,#149619,
#149620,#149621,#149622,#149623,#149624,#149625,#149626,#149627,#149628,
#149629,#149630,#149631,#149632,#149633,#149634,#149635,#149636,#149637,
#149638,#149639,#149640,#149641,#149642,#149643,#149644,#149645,#149646,
#149647,#149648,#149649,#149650,#149651,#149652,#149653,#149654,#149655,
#149656,#149657,#149658,#149659,#149660,#149661,#149662,#149663,#149664,
#149665,#149666,#149667,#149668,#149669,#149670,#149671,#149672,#149673,
#149674,#149675,#149676,#149677,#149678,#149679,#149680,#149681,#149682,
#149683,#149684,#149685,#149686,#149687,#149688,#149689,#149690,#149691,
#149692,#149693),.UNSPECIFIED.,.F.,.F.,(4,3,3,3,3,3,3,3,3,3,3,3,3,3,3,3,
3,3,3,3,3,3,3,3,3,3,3,3,3,3,3,3,3,3,3,3,3,3,3,3,3,4),(153.9380400259,154.035163898234,
154.132222574363,154.229246955324,154.326267897773,154.423381488606,154.520541056366,
154.617870832504,154.700536579074,154.799134704076,154.897592486852,154.997815054625,
155.096094612352,155.194341191424,155.292584274461,155.394281463105,155.492665876523,
155.596019452779,155.699373029036,155.797971154037,155.896428936811,155.996651504585,
156.09493106231,156.193177641381,156.291420724416,156.393117913062,156.491502326478,
156.594855902738,156.698209478998,156.796807604012,156.895265386799,156.995487954569,
157.093767512308,157.192014091392,157.29025717444,157.39195436307,157.490338776499,
157.59369235273,157.69704592896,157.795632129848,157.895770619144,157.995909108439),
 .UNSPECIFIED.);
#1566=B_SPLINE_CURVE_WITH_KNOTS('',3,(#149694,#149695,#149696,#149697,#149698,
#149699),.UNSPECIFIED.,.F.,.F.,(4,1,1,4),(151.712252778999,152.702863679151,
153.701700129113,153.938039726298),.UNSPECIFIED.);
#1567=B_SPLINE_CURVE_WITH_KNOTS('',3,(#149701,#149702,#149703,#149704,#149705,
#149706),.UNSPECIFIED.,.F.,.F.,(4,1,1,4),(151.712342700426,152.238056946631,
153.236893396593,153.9380400259),.UNSPECIFIED.);
#1568=B_SPLINE_CURVE_WITH_KNOTS('',3,(#149707,#149708,#149709,#149710,#149711,
#149712,#149713,#149714,#149715,#149716,#149717,#149718,#149719,#149720,
#149721,#149722,#149723,#149724,#149725,#149726,#149727,#149728,#149729,
#149730,#149731,#149732,#149733,#149734,#149735,#149736,#149737,#149738,
#149739,#149740,#149741,#149742,#149743,#149744,#149745,#149746,#149747,
#149748,#149749,#149750,#149751,#149752,#149753,#149754,#149755,#149756,
#149757,#149758,#149759,#149760,#149761,#149762,#149763,#149764,#149765,
#149766,#149767,#149768,#149769,#149770,#149771,#149772,#149773,#149774,
#149775,#149776,#149777,#149778,#149779,#149780,#149781,#149782,#149783,
#149784,#149785,#149786,#149787,#149788,#149789,#149790,#149791,#149792,
#149793,#149794,#149795,#149796,#149797,#149798,#149799,#149800,#149801,
#149802,#149803,#149804,#149805,#149806,#149807,#149808,#149809,#149810,
#149811,#149812,#149813,#149814,#149815,#149816,#149817,#149818,#149819,
#149820,#149821,#149822,#149823,#149824,#149825,#149826,#149827,#149828,
#149829,#149830),.UNSPECIFIED.,.F.,.F.,(4,3,3,3,3,3,3,3,3,3,3,3,3,3,3,3,
3,3,3,3,3,3,3,3,3,3,3,3,3,3,3,3,3,3,3,3,3,3,3,3,3,4),(153.938040202766,
154.056659980235,154.176963650991,154.235729846555,154.334327971559,154.432785754335,
154.533008322108,154.631287879836,154.729534458909,154.827777541948,154.92947473059,
155.027859144009,155.131212720263,155.234566296517,155.33316442152,155.431622204297,
155.531844772069,155.630124329797,155.72837090887,155.826613991908,155.928311180551,
156.026695593969,156.130049170224,156.233402746479,156.332000871484,156.430458654262,
156.530681222035,156.628960779764,156.727207358839,156.825450441879,156.927147630519,
157.025532043939,157.12888562019,157.232239196441,157.330809964381,157.429252216959,
157.527595662268,157.625869905303,157.724128943532,157.822375482215,157.920688283613,
157.994794053202),.UNSPECIFIED.);
#1569=B_SPLINE_CURVE_WITH_KNOTS('',3,(#149836,#149837,#149838,#149839,#149840,
#149841,#149842,#149843),.UNSPECIFIED.,.F.,.F.,(4,1,1,1,1,4),(160.221227414878,
160.693555278846,161.692391728808,162.691228178769,163.690064628731,164.278110100501),
 .UNSPECIFIED.);
#1570=B_SPLINE_CURVE_WITH_KNOTS('',3,(#149844,#149845,#149846,#149847,#149848,
#149849,#149850,#149851,#149852,#149853,#149854,#149855,#149856,#149857,
#149858,#149859,#149860,#149861,#149862,#149863,#149864,#149865,#149866,
#149867,#149868,#149869,#149870,#149871,#149872,#149873,#149874,#149875,
#149876,#149877,#149878,#149879,#149880,#149881,#149882,#149883,#149884,
#149885,#149886,#149887,#149888,#149889,#149890,#149891,#149892,#149893,
#149894,#149895,#149896,#149897,#149898,#149899,#149900,#149901,#149902,
#149903,#149904,#149905,#149906,#149907,#149908,#149909,#149910,#149911,
#149912,#149913),.UNSPECIFIED.,.F.,.F.,(4,3,3,3,3,3,3,3,3,3,3,3,3,3,3,3,
3,3,3,3,3,3,3,4),(157.995909108439,158.094187900561,158.192434189533,158.290677457562,
158.391978687902,158.490363797708,158.593123088315,158.695882378922,158.794480503912,
158.892938286675,158.993160854451,159.091440412165,159.189686991224,159.287930074248,
159.389627262907,159.488011676311,159.591365252598,159.694718828884,159.797216560019,
159.903218753284,160.005303397592,160.107256278837,160.209067828956,160.22122533308),
 .UNSPECIFIED.);
#1571=B_SPLINE_CURVE_WITH_KNOTS('',3,(#149915,#149916,#149917,#149918,#149919,
#149920,#149921,#149922,#149923,#149924,#149925,#149926,#149927,#149928,
#149929,#149930,#149931,#149932,#149933,#149934,#149935,#149936,#149937,
#149938,#149939,#149940,#149941,#149942,#149943,#149944,#149945,#149946,
#149947,#149948,#149949,#149950,#149951,#149952,#149953,#149954,#149955,
#149956,#149957,#149958,#149959,#149960,#149961,#149962,#149963,#149964,
#149965,#149966,#149967,#149968,#149969,#149970,#149971,#149972,#149973,
#149974,#149975,#149976,#149977,#149978,#149979,#149980,#149981,#149982,
#149983,#149984),.UNSPECIFIED.,.F.,.F.,(4,3,3,3,3,3,3,3,3,3,3,3,3,3,3,3,
3,3,3,3,3,3,3,4),(157.994794053202,158.093225172905,158.191816739594,158.231075646402,
158.329673771403,158.428131554177,158.528354121951,158.626633679676,158.724880258747,
158.823123341783,158.924820530428,159.023204943844,159.126558520104,159.229912096364,
159.328378576654,159.426704810661,159.526019875932,159.624169149678,159.722285836342,
159.820399593048,159.920606027993,160.018861091251,160.120043212039,160.221225332828),
 .UNSPECIFIED.);
#1572=B_SPLINE_CURVE_WITH_KNOTS('',3,(#149985,#149986,#149987,#149988,#149989,
#149990,#149991,#149992,#149993,#149994,#149995,#149996,#149997,#149998,
#149999,#150000,#150001,#150002,#150003,#150004,#150005,#150006,#150007,
#150008,#150009,#150010,#150011,#150012,#150013,#150014,#150015,#150016,
#150017,#150018,#150019,#150020,#150021,#150022,#150023,#150024,#150025,
#150026,#150027,#150028,#150029,#150030,#150031,#150032,#150033,#150034,
#150035,#150036,#150037,#150038,#150039,#150040,#150041,#150042,#150043,
#150044,#150045,#150046,#150047,#150048,#150049,#150050,#150051,#150052,
#150053,#150054,#150055,#150056,#150057,#150058,#150059,#150060,#150061,
#150062,#150063,#150064,#150065,#150066,#150067,#150068,#150069,#150070,
#150071,#150072,#150073,#150074,#150075,#150076,#150077,#150078,#150079,
#150080,#150081,#150082,#150083,#150084,#150085,#150086,#150087,#150088,
#150089,#150090,#150091,#150092,#150093,#150094,#150095,#150096,#150097,
#150098,#150099,#150100,#150101,#150102,#150103,#150104,#150105,#150106,
#150107,#150108,#150109,#150110,#150111),.UNSPECIFIED.,.F.,.F.,(4,3,3,3,
3,3,3,3,3,3,3,3,3,3,3,3,3,3,3,3,3,3,3,3,3,3,3,3,3,3,3,3,3,3,3,3,3,3,3,3,
3,3,4),(160.22122533308,160.228748546326,160.327346671318,160.425804454083,
160.526027021859,160.624306579575,160.722553158637,160.820796241665,160.92249343032,
161.020877843728,161.124231420008,161.227584996288,161.326183121278,161.424640904041,
161.524863471817,161.623143029531,161.72138960859,161.819632691615,161.921329880273,
162.019714293678,162.123067869964,162.22642144625,162.325019571326,162.423477354175,
162.52369992193,162.62197947973,162.720226058876,162.818469141986,162.920166330542,
163.018550744032,163.121904320122,163.225257896212,163.323856021116,163.422313803793,
163.522536371591,163.620815929221,163.719062508197,163.817305591139,163.919002779898,
164.017387193223,164.120740769699,164.224094346174,164.278857765994),
 .UNSPECIFIED.);
#1573=B_SPLINE_CURVE_WITH_KNOTS('',3,(#150117,#150118,#150119,#150120,#150121,
#150122,#150123,#150124,#150125,#150126,#150127,#150128,#150129,#150130,
#150131,#150132,#150133,#150134,#150135,#150136,#150137,#150138,#150139,
#150140,#150141,#150142,#150143,#150144,#150145,#150146,#150147,#150148,
#150149,#150150,#150151,#150152,#150153,#150154,#150155,#150156,#150157,
#150158,#150159,#150160,#150161,#150162,#150163,#150164,#150165,#150166,
#150167,#150168,#150169,#150170,#150171,#150172,#150173,#150174,#150175,
#150176,#150177,#150178,#150179,#150180,#150181,#150182,#150183,#150184,
#150185,#150186,#150187,#150188,#150189,#150190,#150191,#150192,#150193,
#150194,#150195,#150196,#150197,#150198,#150199,#150200,#150201,#150202,
#150203,#150204,#150205,#150206,#150207,#150208,#150209,#150210,#150211,
#150212,#150213,#150214,#150215,#150216,#150217,#150218,#150219,#150220,
#150221,#150222,#150223,#150224,#150225,#150226,#150227,#150228,#150229,
#150230,#150231,#150232,#150233,#150234,#150235,#150236,#150237,#150238,
#150239,#150240),.UNSPECIFIED.,.F.,.F.,(4,3,3,3,3,3,3,3,3,3,3,3,3,3,3,3,
3,3,3,3,3,3,3,3,3,3,3,3,3,3,3,3,3,3,3,3,3,3,3,3,3,4),(166.504410640259,
166.652910770227,166.686573978617,166.785172097216,166.883629873594,166.983852442967,
167.082131994355,167.180378567125,167.278621643903,167.380318840072,167.478703247402,
167.58205683799,167.685410428579,167.784008554554,167.882466338243,167.98268890578,
168.080968464272,168.179215044053,168.277458127742,168.379155315442,168.477539729364,
168.580893303952,168.684246878541,168.782845025293,168.881302829919,168.981525392242,
169.079804971909,169.178051572908,169.276294677829,169.377991840497,169.476376275469,
169.579729801986,169.683083328503,169.781689727945,169.880127484649,169.978469449795,
170.076745219903,170.174984320903,170.273261950043,170.371554712591,170.469968413607,
170.561255441754),.UNSPECIFIED.);
#1574=B_SPLINE_CURVE_WITH_KNOTS('',3,(#150241,#150242,#150243,#150244,#150245,
#150246),.UNSPECIFIED.,.F.,.F.,(4,1,1,4),(164.278110100501,164.688901078693,
165.687737528655,166.504405683232),.UNSPECIFIED.);
#1575=B_SPLINE_CURVE_WITH_KNOTS('',3,(#150248,#150249,#150250,#150251,#150252,
#150253,#150254,#150255,#150256,#150257,#150258,#150259,#150260,#150261,
#150262,#150263,#150264,#150265,#150266,#150267,#150268,#150269,#150270,
#150271,#150272,#150273,#150274,#150275,#150276,#150277,#150278,#150279,
#150280,#150281,#150282,#150283,#150284,#150285,#150286,#150287,#150288,
#150289,#150290,#150291,#150292,#150293,#150294,#150295,#150296,#150297,
#150298,#150299,#150300,#150301,#150302,#150303,#150304,#150305,#150306,
#150307,#150308,#150309,#150310,#150311,#150312,#150313,#150314,#150315,
#150316,#150317),.UNSPECIFIED.,.F.,.F.,(4,3,3,3,3,3,3,3,3,3,3,3,3,3,3,3,
3,3,3,3,3,3,3,4),(164.278857765994,164.377373907485,164.475767948866,164.574072822073,
164.672331029923,164.770572069846,164.868825414456,164.967184460474,165.065601054055,
165.164183854236,165.222930796136,165.321528921635,165.419986704909,165.520209272558,
165.618488830783,165.716735410353,165.814978493886,165.916675681939,166.015060095843,
166.11841367097,166.221767246097,166.34459987441,166.465474953157,166.504410639987),
 .UNSPECIFIED.);
#1576=B_SPLINE_CURVE_WITH_KNOTS('',3,(#150318,#150319,#150320,#150321,#150322,
#150323,#150324,#150325,#150326,#150327,#150328,#150329,#150330,#150331,
#150332,#150333,#150334,#150335,#150336,#150337,#150338,#150339,#150340,
#150341,#150342,#150343,#150344,#150345,#150346,#150347,#150348,#150349,
#150350,#150351,#150352,#150353,#150354,#150355,#150356,#150357,#150358,
#150359,#150360,#150361,#150362,#150363,#150364,#150365,#150366,#150367,
#150368,#150369,#150370,#150371,#150372,#150373,#150374,#150375,#150376,
#150377,#150378,#150379,#150380,#150381,#150382,#150383,#150384,#150385,
#150386,#150387,#150388,#150389,#150390,#150391,#150392,#150393,#150394,
#150395,#150396,#150397,#150398,#150399,#150400,#150401,#150402,#150403,
#150404,#150405,#150406,#150407,#150408,#150409,#150410,#150411,#150412,
#150413,#150414,#150415,#150416,#150417,#150418,#150419,#150420,#150421,
#150422,#150423,#150424,#150425,#150426,#150427,#150428,#150429,#150430,
#150431,#150432,#150433,#150434,#150435,#150436,#150437,#150438,#150439,
#150440,#150441,#150442,#150443,#150444),.UNSPECIFIED.,.F.,.F.,(4,3,3,3,
3,3,3,3,3,3,3,3,3,3,3,3,3,3,3,3,3,3,3,3,3,3,3,3,3,3,3,3,3,3,3,3,3,3,3,3,
3,3,4),(166.504410640259,166.6019131263,166.699371433809,166.79681599036,
166.894277201724,166.991846173228,167.089478292237,167.187269535439,167.220603696059,
167.319201820915,167.417659603535,167.517882171346,167.616161728898,167.714408307788,
167.812651390637,167.914348579483,168.012732992698,168.116086569359,168.219440146021,
168.318038274346,168.416496060457,168.516718627398,168.614998188467,168.713244770876,
168.811487857242,168.913185041927,169.011569458616,169.1149230273,169.218276595983,
169.316874714607,169.415332491011,169.515555060377,169.613834611791,169.712081184585,
169.810324261387,169.912021457527,170.01040586488,170.113759455413,170.217113045945,
170.315689889885,170.414143809233,170.512486666531,170.562190678317),
 .UNSPECIFIED.);
#1577=B_SPLINE_CURVE_WITH_KNOTS('',3,(#150450,#150451,#150452,#150453,#150454,
#150455,#150456,#150457,#150458,#150459,#150460,#150461,#150462,#150463,
#150464,#150465,#150466,#150467,#150468,#150469,#150470,#150471,#150472,
#150473,#150474,#150475,#150476,#150477,#150478,#150479,#150480,#150481,
#150482,#150483,#150484,#150485,#150486,#150487,#150488,#150489,#150490,
#150491,#150492,#150493,#150494,#150495,#150496,#150497,#150498,#150499,
#150500,#150501,#150502,#150503,#150504,#150505,#150506,#150507,#150508,
#150509,#150510,#150511,#150512,#150513,#150514,#150515,#150516,#150517,
#150518,#150519,#150520,#150521,#150522,#150523,#150524,#150525,#150526,
#150527,#150528,#150529,#150530,#150531,#150532,#150533,#150534,#150535,
#150536,#150537,#150538,#150539,#150540,#150541,#150542,#150543,#150544,
#150545,#150546,#150547,#150548,#150549,#150550,#150551,#150552,#150553,
#150554,#150555,#150556,#150557,#150558,#150559,#150560,#150561,#150562,
#150563,#150564,#150565,#150566,#150567,#150568,#150569,#150570,#150571,
#150572,#150573,#150574,#150575,#150576),.UNSPECIFIED.,.F.,.F.,(4,3,3,3,
3,3,3,3,3,3,3,3,3,3,3,3,3,3,3,3,3,3,3,3,3,3,3,3,3,3,3,3,3,3,3,3,3,3,3,3,
3,3,4),(172.787595947668,172.884841558603,172.984040004821,173.081071836984,
173.178059268517,173.275033212281,173.375882191298,173.472980624789,173.57014496826,
173.66745840562,173.67842912835,173.777027506535,173.875485539983,173.975708044774,
174.073987845308,174.172234663756,174.270477982445,174.372174881412,174.470559518906,
174.573912548609,174.677265578312,174.77586453171,174.874323148858,174.974545508785,
175.072825909421,175.171073332739,175.26931726024,175.371013452249,175.469398702017,
175.572750365145,175.676102028274,175.774697485907,175.873152598171,175.973375833179,
176.071652731782,176.169896661679,176.2681371089,176.369837451234,176.468219288705,
176.57157888347,176.674938478236,176.773518528063,176.845520771701),
 .UNSPECIFIED.);
#1578=B_SPLINE_CURVE_WITH_KNOTS('',3,(#150577,#150578,#150579,#150580,#150581,
#150582,#150583,#150584,#150585,#150586,#150587,#150588,#150589,#150590,
#150591,#150592,#150593,#150594,#150595,#150596,#150597,#150598,#150599,
#150600,#150601,#150602,#150603,#150604,#150605,#150606,#150607,#150608,
#150609,#150610,#150611,#150612,#150613,#150614,#150615,#150616,#150617,
#150618,#150619,#150620,#150621,#150622,#150623,#150624,#150625,#150626,
#150627,#150628,#150629,#150630,#150631,#150632,#150633,#150634,#150635,
#150636,#150637,#150638,#150639,#150640,#150641,#150642,#150643,#150644,
#150645,#150646),.UNSPECIFIED.,.F.,.F.,(4,3,3,3,3,3,3,3,3,3,3,3,3,3,3,3,
3,3,3,3,3,3,3,4),(170.561255441754,170.659855757029,170.681919778464,170.780517924866,
170.878975728651,170.979198291123,171.077477868768,171.17572446731,171.273967569349,
171.375664734118,171.474049165187,171.577402696807,171.680756228426,171.779354490553,
171.877812411242,171.978034944635,172.076314641203,172.17456135916,172.272804580942,
172.374501605303,172.472886155702,172.576239417045,172.679592678388,172.787595947439),
 .UNSPECIFIED.);
#1579=B_SPLINE_CURVE_WITH_KNOTS('',3,(#150648,#150649,#150650,#150651,#150652,
#150653,#150654,#150655,#150656,#150657,#150658,#150659,#150660,#150661,
#150662,#150663,#150664,#150665,#150666,#150667,#150668,#150669,#150670,
#150671,#150672,#150673,#150674,#150675,#150676,#150677,#150678,#150679,
#150680,#150681,#150682,#150683,#150684,#150685,#150686,#150687,#150688,
#150689,#150690,#150691,#150692,#150693,#150694,#150695,#150696,#150697,
#150698,#150699,#150700,#150701,#150702,#150703,#150704,#150705,#150706,
#150707,#150708,#150709,#150710,#150711,#150712,#150713,#150714,#150715,
#150716,#150717),.UNSPECIFIED.,.F.,.F.,(4,3,3,3,3,3,3,3,3,3,3,3,3,3,3,3,
3,3,3,3,3,3,3,4),(170.562190678317,170.660450514926,170.758691713403,170.856943746971,
170.955300618973,171.053713717861,171.152294511815,171.215949495907,171.314547642568,
171.413005447104,171.51322800945,171.611507589026,171.709754189934,171.807997294764,
171.90969445754,172.008078892422,172.111432419146,172.214785945869,172.315617765325,
172.416285943672,172.516781875576,172.617176498836,172.717484580328,172.787595947439),
 .UNSPECIFIED.);
#1580=B_SPLINE_CURVE_WITH_KNOTS('',3,(#150718,#150719,#150720,#150721,#150722,
#150723,#150724,#150725),.UNSPECIFIED.,.F.,.F.,(4,1,1,1,1,4),(172.787601414694,
173.21362239583,174.212458845792,175.211295295754,176.210131745716,176.844282077012),
 .UNSPECIFIED.);
#1581=B_SPLINE_CURVE_WITH_KNOTS('',3,(#150731,#150732,#150733,#150734,#150735,
#150736,#150737,#150738),.UNSPECIFIED.,.F.,.F.,(4,1,1,1,1,4),(179.070781254618,
179.671447828121,180.670284278083,181.669120728045,182.667957178007,183.128402568106),
 .UNSPECIFIED.);
#1582=B_SPLINE_CURVE_WITH_KNOTS('',3,(#150739,#150740,#150741,#150742,#150743,
#150744,#150745,#150746,#150747,#150748,#150749,#150750,#150751,#150752,
#150753,#150754,#150755,#150756,#150757,#150758,#150759,#150760,#150761,
#150762,#150763,#150764,#150765,#150766,#150767,#150768,#150769,#150770,
#150771,#150772,#150773,#150774,#150775,#150776,#150777,#150778,#150779,
#150780,#150781,#150782,#150783,#150784,#150785,#150786,#150787,#150788,
#150789,#150790,#150791,#150792,#150793,#150794,#150795,#150796,#150797,
#150798,#150799,#150800,#150801,#150802,#150803,#150804,#150805,#150806,
#150807,#150808),.UNSPECIFIED.,.F.,.F.,(4,3,3,3,3,3,3,3,3,3,3,3,3,3,3,3,
3,3,3,3,3,3,3,4),(176.845520771701,176.949052541263,177.047346590345,177.145600683284,
177.243844306548,177.342106927815,177.440479043576,177.538914719441,177.637509918042,
177.673774928198,177.772377764499,177.870840302866,177.971061687278,178.069346073991,
178.167597498754,178.265845437705,178.367536922818,178.465926167544,178.569268772851,
178.672611378159,178.782250111505,178.891545462336,179.000249339659,179.070781030153),
 .UNSPECIFIED.);
#1583=B_SPLINE_CURVE_WITH_KNOTS('',3,(#150810,#150811,#150812,#150813,#150814,
#150815),.UNSPECIFIED.,.F.,.F.,(4,1,1,4),(176.844282077012,177.208968195678,
178.20780464564,179.070781254618),.UNSPECIFIED.);
#1584=B_SPLINE_CURVE_WITH_KNOTS('',3,(#150816,#150817,#150818,#150819,#150820,
#150821,#150822,#150823),.UNSPECIFIED.,.F.,.F.,(4,1,1,1,1,4),(179.070781254618,
179.206641095602,180.205477545564,181.204313995525,182.203150445487,183.127688302604),
 .UNSPECIFIED.);
#1585=B_SPLINE_CURVE_WITH_KNOTS('',3,(#150829,#150830,#150831,#150832,#150833,
#150834,#150835,#150836),.UNSPECIFIED.,.F.,.F.,(4,1,1,1,1,4),(15.707963267949,
15.8622700343739,16.8611064843358,17.8599429342977,18.8587793842596,19.7647622867482),
 .UNSPECIFIED.);
#1586=B_SPLINE_CURVE_WITH_KNOTS('',3,(#150838,#150839,#150840,#150841,#150842,
#150843,#150844,#150845,#150846,#150847,#150848,#150849,#150850,#150851,
#150852,#150853,#150854,#150855,#150856,#150857,#150858,#150859,#150860,
#150861,#150862,#150863,#150864,#150865,#150866,#150867,#150868,#150869,
#150870,#150871,#150872,#150873,#150874,#150875,#150876,#150877,#150878,
#150879,#150880,#150881,#150882,#150883,#150884,#150885,#150886,#150887,
#150888,#150889,#150890,#150891,#150892,#150893,#150894,#150895),
 .UNSPECIFIED.,.F.,.F.,(4,3,3,3,3,3,3,3,3,3,3,3,3,3,3,3,3,3,3,4),(13.8757070305535,
13.9742334885845,14.0726196430263,14.1714713856996,14.2696800147309,14.3678555358064,
14.4660275256487,14.5653790403396,14.6636889428954,14.7635612636538,14.8634335844121,
14.9606976643214,15.0578044061946,15.154822904629,15.2517842090804,15.3487192963901,
15.4457083601634,15.5427241599104,15.6398692512359,15.707963267949),
 .UNSPECIFIED.);
#1587=B_SPLINE_CURVE_WITH_KNOTS('',3,(#150899,#150900,#150901,#150902,#150903),
 .UNSPECIFIED.,.F.,.F.,(4,1,4),(14.3986268518925,15.3974633018543,15.707963267949),
 .UNSPECIFIED.);
#1588=B_SPLINE_CURVE_WITH_KNOTS('',3,(#150904,#150905,#150906,#150907,#150908,
#150909,#150910,#150911),.UNSPECIFIED.,.F.,.F.,(4,1,1,1,1,4),(15.707963267949,
16.3962997518162,17.3951362017781,18.39397265174,19.3928091017018,19.7659327146509),
 .UNSPECIFIED.);
#1589=B_SPLINE_CURVE_WITH_KNOTS('',3,(#150917,#150918,#150919,#150920,#150921,
#150922,#150923,#150924),.UNSPECIFIED.,.F.,.F.,(4,1,1,1,1,4),(21.9911485751286,
22.854125184107,23.8529616340689,24.8517980840308,25.8506345339927,26.0493850218968),
 .UNSPECIFIED.);
#1590=B_SPLINE_CURVE_WITH_KNOTS('',3,(#150925,#150926,#150927,#150928,#150929,
#150930,#150931),.UNSPECIFIED.,.F.,.F.,(4,1,1,1,4),(19.7647622867482,19.8576158342214,
20.8564522841833,21.8552887341452,21.9911485751286),.UNSPECIFIED.);
#1591=B_SPLINE_CURVE_WITH_KNOTS('',3,(#150933,#150934,#150935,#150936,#150937,
#150938),.UNSPECIFIED.,.F.,.F.,(4,1,1,4),(19.7659327146509,20.3916455516637,
21.3904820016256,21.9911485751286),.UNSPECIFIED.);
#1592=B_SPLINE_CURVE_WITH_KNOTS('',3,(#150939,#150940,#150941,#150942,#150943,
#150944,#150945,#150946,#150947,#150948,#150949,#150950,#150951,#150952,
#150953,#150954,#150955,#150956,#150957,#150958,#150959,#150960,#150961,
#150962,#150963,#150964,#150965,#150966,#150967,#150968,#150969,#150970,
#150971,#150972,#150973,#150974,#150975,#150976,#150977,#150978,#150979,
#150980,#150981,#150982,#150983,#150984,#150985,#150986,#150987,#150988,
#150989,#150990,#150991,#150992,#150993,#150994,#150995,#150996,#150997,
#150998,#150999,#151000,#151001,#151002,#151003,#151004,#151005,#151006,
#151007,#151008,#151009,#151010,#151011,#151012,#151013,#151014,#151015,
#151016,#151017,#151018,#151019,#151020,#151021,#151022,#151023,#151024,
#151025,#151026,#151027,#151028,#151029,#151030,#151031,#151032,#151033,
#151034,#151035,#151036,#151037,#151038,#151039,#151040,#151041,#151042,
#151043,#151044,#151045,#151046,#151047,#151048,#151049,#151050,#151051,
#151052,#151053,#151054,#151055,#151056,#151057,#151058,#151059,#151060,
#151061,#151062),.UNSPECIFIED.,.F.,.F.,(4,3,3,3,3,3,3,3,3,3,3,3,3,3,3,3,
3,3,3,3,3,3,3,3,3,3,3,3,3,3,3,3,3,3,3,3,3,3,3,3,3,4),(21.9911487995909,
22.0999040367044,22.2090425458686,22.3187160667875,22.3893184515875,22.487921335874,
22.5863839114419,22.6866052852053,22.7848896824335,22.883141107753,22.9813890373116,
23.0830805033711,23.1814697140479,23.2848123077986,23.3881549015493,23.4867551965745,
23.5852152014032,23.6854372201667,23.78371911203,23.8819680620747,23.9802135499039,
24.0819080003058,24.1802948788303,24.2836431151707,24.3869913515112,24.4855869755136,
24.5840422190559,24.6842654168581,24.7825423598393,24.8807863016633,24.9790267283841,
25.0807269966564,25.1791087331383,25.2824682673057,25.3858278014731,25.4844081060613,
25.5828572825197,25.6812050501617,25.7794880251905,25.8777310360909,25.9759959181972,
26.0480411834147),.UNSPECIFIED.);
#1593=B_SPLINE_CURVE_WITH_KNOTS('',3,(#151068,#151069,#151070,#151071,#151072,
#151073,#151074,#151075,#151076,#151077,#151078,#151079,#151080,#151081,
#151082,#151083,#151084,#151085,#151086,#151087,#151088,#151089,#151090,
#151091,#151092,#151093,#151094,#151095,#151096,#151097,#151098,#151099,
#151100,#151101,#151102,#151103,#151104,#151105,#151106,#151107,#151108,
#151109,#151110,#151111,#151112,#151113,#151114,#151115,#151116,#151117,
#151118,#151119,#151120,#151121,#151122,#151123,#151124,#151125,#151126,
#151127,#151128,#151129,#151130,#151131,#151132,#151133,#151134,#151135,
#151136,#151137,#151138,#151139,#151140,#151141,#151142,#151143,#151144,
#151145,#151146,#151147,#151148,#151149,#151150,#151151,#151152,#151153,
#151154,#151155,#151156,#151157,#151158,#151159,#151160,#151161,#151162,
#151163,#151164,#151165,#151166,#151167,#151168,#151169,#151170,#151171,
#151172,#151173,#151174,#151175,#151176,#151177,#151178,#151179,#151180,
#151181,#151182,#151183,#151184,#151185,#151186,#151187,#151188,#151189,
#151190,#151191),.UNSPECIFIED.,.F.,.F.,(4,3,3,3,3,3,3,3,3,3,3,3,3,3,3,3,
3,3,3,3,3,3,3,3,3,3,3,3,3,3,3,3,3,3,3,3,3,3,3,3,3,4),(28.2743338823082,
28.3746245107026,28.4749734040128,28.5754886322331,28.6760922705589,28.7769068627545,
28.8471438838783,28.9457420299255,29.0441998339908,29.144422396472,29.2427019759347,
29.3409485768614,29.4391916818436,29.5408888448427,29.6392732802058,29.742626807023,
29.8459803338402,29.9445784592274,30.043036242454,30.1432588101225,30.241538368462,
30.3397849482058,30.4380280319734,30.5397252199305,30.638109634218,30.74146320901,
30.844816783802,30.9434149029218,31.0418726797114,31.142095248968,31.2403748004981,
31.3386213733082,31.4368644500261,31.5385616459606,31.6369460529803,31.7402996433721,
31.8436532337639,31.9422528703178,32.0406907036715,32.1390337581138,32.2373181769772,
32.331714743168),.UNSPECIFIED.);
#1594=B_SPLINE_CURVE_WITH_KNOTS('',3,(#151192,#151193,#151194,#151195,#151196,
#151197),.UNSPECIFIED.,.F.,.F.,(4,1,1,4),(26.0493850218968,26.8494709839545,
27.8483074339164,28.2743284148783),.UNSPECIFIED.);
#1595=B_SPLINE_CURVE_WITH_KNOTS('',3,(#151199,#151200,#151201,#151202,#151203,
#151204,#151205,#151206,#151207,#151208,#151209,#151210,#151211,#151212,
#151213,#151214,#151215,#151216,#151217,#151218,#151219,#151220,#151221,
#151222,#151223,#151224,#151225,#151226,#151227,#151228,#151229,#151230,
#151231,#151232,#151233,#151234,#151235,#151236,#151237,#151238,#151239,
#151240,#151241,#151242,#151243,#151244,#151245,#151246,#151247,#151248,
#151249,#151250,#151251,#151252,#151253,#151254,#151255,#151256,#151257,
#151258,#151259,#151260,#151261,#151262,#151263,#151264,#151265,#151266,
#151267,#151268,#151269,#151270,#151271),.UNSPECIFIED.,.F.,.F.,(4,3,3,3,
3,3,3,3,3,3,3,3,3,3,3,3,3,3,3,3,3,3,3,3,4),(26.0480411834147,26.1464093623878,
26.244839798522,26.3434312469923,26.384664251435,26.4832625890263,26.5817205904922,
26.6819431043553,26.7802228942346,26.8784697099906,26.976713033946,27.0784099508087,
27.1767946133168,27.2801476573568,27.3835007013968,27.4808124349029,27.5800026158,
27.6770619108145,27.7740624128206,27.8710350559302,27.9718597624675,28.0689211605358,
28.1660361013683,28.2632831488084,28.2743338820795),.UNSPECIFIED.);
#1596=B_SPLINE_CURVE_WITH_KNOTS('',3,(#151272,#151273,#151274,#151275,#151276,
#151277,#151278,#151279,#151280,#151281,#151282,#151283,#151284,#151285,
#151286,#151287,#151288,#151289,#151290,#151291,#151292,#151293,#151294,
#151295,#151296,#151297,#151298,#151299,#151300,#151301,#151302,#151303,
#151304,#151305,#151306,#151307,#151308,#151309,#151310,#151311,#151312,
#151313,#151314,#151315,#151316,#151317,#151318,#151319,#151320,#151321,
#151322,#151323,#151324,#151325,#151326,#151327,#151328,#151329,#151330,
#151331,#151332,#151333,#151334,#151335,#151336,#151337,#151338,#151339,
#151340,#151341,#151342,#151343,#151344,#151345,#151346,#151347,#151348,
#151349,#151350,#151351,#151352,#151353,#151354,#151355,#151356,#151357,
#151358,#151359,#151360,#151361,#151362,#151363,#151364,#151365,#151366,
#151367,#151368,#151369,#151370,#151371,#151372,#151373,#151374,#151375,
#151376,#151377,#151378,#151379,#151380,#151381,#151382,#151383,#151384,
#151385,#151386,#151387,#151388,#151389,#151390,#151391,#151392,#151393,
#151394,#151395),.UNSPECIFIED.,.F.,.F.,(4,3,3,3,3,3,3,3,3,3,3,3,3,3,3,3,
3,3,3,3,3,3,3,3,3,3,3,3,3,3,3,3,3,3,3,3,3,3,3,3,3,4),(28.2743338823082,
28.3823371513587,28.4809354104368,28.5793933287022,28.6796158627795,28.7778955584748,
28.8761422761379,28.9743854982056,29.0760825239843,29.1744670761058,29.2778203387132,
29.3811736013206,29.4797717427275,29.5782295425788,29.6784521061668,29.7767316825037,
29.8749782807199,29.9732213834117,30.0749185503794,30.1733029845339,30.2766565179082,
30.3800100512825,30.4786081309532,30.5770658676386,30.6772884468394,30.7755679569466,
30.8738144879313,30.9720575224759,31.073754767168,31.1721391315728,31.2754928164085,
31.3788465012443,31.47744774742,31.5759078068145,31.6742504133382,31.772528758262,
31.8707723652669,31.969010716985,32.0673303014884,32.1656922455267,32.264202766454,
32.3314302948912),.UNSPECIFIED.);
#1597=B_SPLINE_CURVE_WITH_KNOTS('',3,(#151401,#151402,#151403,#151404,#151405,
#151406,#151407,#151408,#151409,#151410,#151411,#151412,#151413,#151414,
#151415,#151416,#151417,#151418,#151419,#151420,#151421,#151422,#151423,
#151424,#151425,#151426,#151427,#151428,#151429,#151430,#151431,#151432,
#151433,#151434,#151435,#151436,#151437,#151438,#151439,#151440,#151441,
#151442,#151443,#151444,#151445,#151446,#151447,#151448,#151449,#151450,
#151451,#151452,#151453,#151454,#151455,#151456,#151457,#151458,#151459,
#151460,#151461,#151462,#151463,#151464,#151465,#151466,#151467,#151468,
#151469,#151470,#151471,#151472,#151473,#151474,#151475,#151476,#151477,
#151478,#151479,#151480,#151481,#151482,#151483,#151484,#151485,#151486,
#151487,#151488,#151489,#151490,#151491,#151492,#151493,#151494,#151495,
#151496,#151497,#151498,#151499,#151500,#151501,#151502,#151503,#151504,
#151505,#151506,#151507,#151508,#151509,#151510,#151511,#151512,#151513,
#151514,#151515,#151516,#151517,#151518,#151519,#151520,#151521,#151522,
#151523,#151524),.UNSPECIFIED.,.F.,.F.,(4,3,3,3,3,3,3,3,3,3,3,3,3,3,3,3,
3,3,3,3,3,3,3,3,3,3,3,3,3,3,3,3,3,3,3,3,3,3,3,3,3,4),(34.5575191897594,
34.6782345503652,34.8009387396128,34.8401625836495,34.938760709128,35.0372184923859,
35.1374410600391,35.2357206182604,35.3339671978303,35.432210281368,35.5339074694289,
35.6322918833488,35.7356454584801,35.8389990336114,35.9375971585483,36.0360549412584,
36.1362775090477,36.2345570667101,36.3328036457183,36.431046728692,36.5327439174123,
36.6311283307686,36.7344819071709,36.8378354835733,36.9364336084867,37.0348913911713,
37.1351139589668,37.2333935165991,37.3316400955754,37.4298831785158,37.5315803672706,
37.6299647805896,37.7333183570624,37.8366719335352,37.9352415778389,38.0336830992457,
38.1320262041044,38.2303004962127,38.3285627936486,38.4268127465031,38.5251372404174,
38.6142676068576),.UNSPECIFIED.);
#1598=B_SPLINE_CURVE_WITH_KNOTS('',3,(#151525,#151526,#151527,#151528,#151529,
#151530,#151531,#151532,#151533,#151534,#151535,#151536,#151537,#151538,
#151539,#151540,#151541,#151542,#151543,#151544,#151545,#151546,#151547,
#151548,#151549,#151550,#151551,#151552,#151553,#151554,#151555,#151556,
#151557,#151558,#151559,#151560,#151561,#151562,#151563,#151564,#151565,
#151566,#151567,#151568,#151569,#151570,#151571,#151572,#151573,#151574,
#151575,#151576,#151577,#151578,#151579,#151580,#151581,#151582,#151583,
#151584,#151585,#151586,#151587,#151588,#151589,#151590,#151591,#151592,
#151593,#151594,#151595,#151596,#151597),.UNSPECIFIED.,.F.,.F.,(4,3,3,3,
3,3,3,3,3,3,3,3,3,3,3,3,3,3,3,3,3,3,3,3,4),(32.331714743168,32.4299572228888,
32.533090338098,32.6314722618068,32.7299237843655,32.8285286363519,32.8424896837258,
32.941087808515,33.039545591083,33.1397681589086,33.2380477164422,33.3362942953269,
33.434537378183,33.5362345670592,33.634618980313,33.7379725570004,33.8413261336877,
33.9390973941506,34.0367388270547,34.1342810926888,34.2317547370042,34.3292101035739,
34.4266554953284,34.5241539309046,34.5575191894878),.UNSPECIFIED.);
#1599=B_SPLINE_CURVE_WITH_KNOTS('',3,(#151599,#151600,#151601,#151602,#151603,
#151604,#151605,#151606,#151607,#151608,#151609,#151610,#151611,#151612,
#151613,#151614,#151615,#151616,#151617,#151618,#151619,#151620,#151621,
#151622,#151623,#151624,#151625,#151626,#151627,#151628,#151629,#151630,
#151631,#151632,#151633,#151634,#151635,#151636,#151637,#151638,#151639,
#151640,#151641,#151642,#151643,#151644,#151645,#151646,#151647,#151648,
#151649,#151650,#151651,#151652,#151653,#151654,#151655,#151656,#151657,
#151658,#151659,#151660,#151661,#151662,#151663,#151664,#151665,#151666,
#151667,#151668),.UNSPECIFIED.,.F.,.F.,(4,3,3,3,3,3,3,3,3,3,3,3,3,3,3,3,
3,3,3,3,3,3,3,4),(32.3314302948912,32.3776829512062,32.4762810765929,32.5747388598192,
32.6749614274878,32.7732409858268,32.8714875655702,32.9697306493372,33.0714278372949,
33.169812251582,33.273165826375,33.3765194011681,33.4751175202855,33.5735752970726,
33.6737978663298,33.7720774178574,33.8703239906649,33.9685670673804,34.0702642633178,
34.1686486703349,34.2720022607324,34.37535585113,34.5238559810743,34.5575191894878),
 .UNSPECIFIED.);
#1600=B_SPLINE_CURVE_WITH_KNOTS('',3,(#151669,#151670,#151671,#151672,#151673,
#151674,#151675,#151676),.UNSPECIFIED.,.F.,.F.,(4,1,1,1,1,4),(34.5575241466493,
35.3741923010918,36.3730287510537,37.3718652010156,38.3707016509774,38.6157831097427),
 .UNSPECIFIED.);
#1601=B_SPLINE_CURVE_WITH_KNOTS('',3,(#151682,#151683,#151684,#151685,#151686,
#151687,#151688,#151689,#151690,#151691,#151692,#151693,#151694,#151695,
#151696,#151697,#151698,#151699,#151700,#151701,#151702,#151703,#151704,
#151705,#151706,#151707,#151708,#151709,#151710,#151711,#151712,#151713,
#151714,#151715,#151716,#151717,#151718,#151719,#151720,#151721,#151722,
#151723,#151724,#151725,#151726,#151727,#151728,#151729,#151730,#151731,
#151732,#151733,#151734,#151735,#151736,#151737,#151738,#151739,#151740,
#151741,#151742,#151743,#151744,#151745,#151746,#151747,#151748,#151749,
#151750,#151751,#151752,#151753,#151754,#151755,#151756,#151757,#151758,
#151759,#151760,#151761,#151762,#151763,#151764,#151765,#151766,#151767,
#151768,#151769,#151770,#151771,#151772,#151773,#151774,#151775,#151776,
#151777,#151778,#151779,#151780,#151781,#151782,#151783,#151784,#151785,
#151786,#151787,#151788,#151789,#151790,#151791,#151792,#151793,#151794,
#151795,#151796,#151797,#151798,#151799,#151800,#151801,#151802,#151803,
#151804,#151805),.UNSPECIFIED.,.F.,.F.,(4,3,3,3,3,3,3,3,3,3,3,3,3,3,3,3,
3,3,3,3,3,3,3,3,3,3,3,3,3,3,3,3,3,3,3,3,3,3,3,3,3,4),(40.8407044969197,
40.9391705387198,41.037496428004,41.1368115911763,41.2349607512892,41.3330774110127,
41.4311912274061,41.5313978539003,41.6296531901072,41.730835461745,41.8320177333827,
41.9306158583838,42.029073641158,42.1292962089313,42.2275757666567,42.3258223457274,
42.4240654287631,42.5257626174084,42.6241470308245,42.7275006070845,42.8308541833445,
42.9294523083471,43.0279100911227,43.1281326588956,43.2264122166225,43.3246587956947,
43.4229018787317,43.5245990673754,43.6229834807929,43.7263370570496,43.8296906333064,
43.9282887583115,44.0267465410895,44.1269691088619,44.2252486665914,44.3234952456661,
44.421738328706,44.5234355173466,44.6218199307668,44.7251735070175,44.8285270832683,
44.898397912177),.UNSPECIFIED.);
#1602=B_SPLINE_CURVE_WITH_KNOTS('',3,(#151806,#151807,#151808,#151809,#151810,
#151811,#151812,#151813,#151814,#151815,#151816,#151817,#151818,#151819,
#151820,#151821,#151822,#151823,#151824,#151825,#151826,#151827,#151828,
#151829,#151830,#151831,#151832,#151833,#151834,#151835,#151836,#151837,
#151838,#151839,#151840,#151841,#151842,#151843,#151844,#151845,#151846,
#151847,#151848,#151849,#151850,#151851,#151852,#151853,#151854,#151855,
#151856,#151857,#151858,#151859,#151860,#151861,#151862,#151863,#151864,
#151865,#151866,#151867,#151868,#151869,#151870,#151871,#151872,#151873,
#151874,#151875,#151876,#151877,#151878),.UNSPECIFIED.,.F.,.F.,(4,3,3,3,
3,3,3,3,3,3,3,3,3,3,3,3,3,3,3,3,3,3,3,3,4),(38.6142676068576,38.7127106610344,
38.8113098761237,38.835508383497,38.9341065084864,39.0325642912489,39.1327868590251,
39.2310664167389,39.3293129957979,39.4275560788221,39.5292532674813,39.627637680886,
39.7309912571724,39.8343448334589,39.9329429584521,40.0314007412181,40.1316233089934,
40.2299028667104,40.3281494457725,40.4263925287995,40.5280897174548,40.6264741308619,
40.7298277071414,40.8331812834208,40.8407044966674),.UNSPECIFIED.);
#1603=B_SPLINE_CURVE_WITH_KNOTS('',3,(#151880,#151881,#151882,#151883,#151884,
#151885),.UNSPECIFIED.,.F.,.F.,(4,1,1,4),(38.6157831097427,39.3695381009393,
40.3683745509012,40.8407024148877),.UNSPECIFIED.);
#1604=B_SPLINE_CURVE_WITH_KNOTS('',3,(#151886,#151887,#151888,#151889,#151890,
#151891,#151892,#151893,#151894,#151895,#151896,#151897,#151898,#151899,
#151900,#151901,#151902,#151903,#151904,#151905,#151906,#151907,#151908,
#151909,#151910,#151911,#151912,#151913,#151914,#151915,#151916,#151917,
#151918,#151919,#151920,#151921,#151922,#151923,#151924,#151925,#151926,
#151927,#151928,#151929,#151930,#151931,#151932,#151933,#151934,#151935,
#151936,#151937,#151938,#151939,#151940,#151941,#151942,#151943,#151944,
#151945,#151946,#151947,#151948,#151949,#151950,#151951,#151952,#151953,
#151954,#151955,#151956,#151957,#151958,#151959,#151960,#151961,#151962,
#151963,#151964,#151965,#151966,#151967,#151968,#151969,#151970,#151971,
#151972,#151973,#151974,#151975,#151976,#151977,#151978,#151979,#151980,
#151981,#151982,#151983,#151984,#151985,#151986,#151987,#151988,#151989,
#151990,#151991,#151992,#151993,#151994,#151995,#151996,#151997,#151998,
#151999,#152000,#152001,#152002,#152003,#152004,#152005,#152006,#152007,
#152008,#152009,#152010,#152011,#152012),.UNSPECIFIED.,.F.,.F.,(4,3,3,3,
3,3,3,3,3,3,3,3,3,3,3,3,3,3,3,3,3,3,3,3,3,3,3,3,3,3,3,3,3,3,3,3,3,3,3,3,
3,3,4),(40.8407044966674,40.9425310419933,41.0487010317108,41.1508691915798,
41.2531658485548,41.3556785603237,41.3672110008631,41.4658091258525,41.5642669086149,
41.6644894763911,41.7627690341048,41.8610156131638,41.959258696188,42.0609558848473,
42.1593402982519,42.2626938745384,42.3660474508249,42.4646455758181,42.5631033585842,
42.6633259263595,42.7616054840764,42.8598520631386,42.9580951461657,43.0597923348209,
43.1581767482281,43.2615303245074,43.3648839007868,43.4634820258002,43.5619398085866,
43.6621623763569,43.7604419340952,43.858688513179,43.956931596228,44.0586287848581,
44.1570131982874,44.260366774518,44.3637203507487,44.4623140220593,44.5607732131683,
44.6591152246882,44.7573894748901,44.8556332863445,44.8979422484848),
 .UNSPECIFIED.);
#1605=B_SPLINE_CURVE_WITH_KNOTS('',3,(#152018,#152019,#152020,#152021,#152022,
#152023,#152024,#152025),.UNSPECIFIED.,.F.,.F.,(4,1,1,1,1,4),(47.123889803847,
47.8250364331539,48.8238728831158,49.8227093330777,50.8215457830395,51.1819113477222),
 .UNSPECIFIED.);
#1606=B_SPLINE_CURVE_WITH_KNOTS('',3,(#152026,#152027,#152028,#152029,#152030,
#152031,#152032,#152033,#152034,#152035,#152036,#152037,#152038,#152039,
#152040,#152041,#152042,#152043,#152044,#152045,#152046,#152047,#152048,
#152049,#152050,#152051,#152052,#152053,#152054,#152055,#152056,#152057,
#152058,#152059,#152060,#152061,#152062,#152063,#152064,#152065,#152066,
#152067,#152068,#152069,#152070,#152071,#152072,#152073,#152074,#152075,
#152076,#152077,#152078,#152079,#152080,#152081,#152082,#152083,#152084,
#152085,#152086,#152087,#152088,#152089,#152090,#152091,#152092,#152093,
#152094,#152095),.UNSPECIFIED.,.F.,.F.,(4,3,3,3,3,3,3,3,3,3,3,3,3,3,3,3,
3,3,3,3,3,3,3,4),(44.898397912177,44.996893211109,45.0952714368175,45.1935672422509,
45.2918209058777,45.3900619196009,45.4883197545766,45.5866858960032,45.6851136444438,
45.7837031196575,45.8273635332302,45.9259616582338,46.0244194410105,46.1246420087832,
46.2229215665111,46.3211681455844,46.4194112286225,46.5211084172649,46.6194928306835,
46.7228464069377,46.826199983192,46.9466622822341,47.0654828012636,47.1238896269672),
 .UNSPECIFIED.);
#1607=B_SPLINE_CURVE_WITH_KNOTS('',3,(#152097,#152098,#152099,#152100,#152101,
#152102,#152103,#152104,#152105,#152106,#152107,#152108,#152109,#152110,
#152111,#152112,#152113,#152114,#152115,#152116,#152117,#152118,#152119,
#152120,#152121,#152122,#152123,#152124,#152125,#152126,#152127,#152128,
#152129,#152130,#152131,#152132,#152133,#152134,#152135,#152136,#152137,
#152138,#152139,#152140,#152141,#152142,#152143,#152144,#152145,#152146,
#152147,#152148,#152149,#152150,#152151,#152152,#152153,#152154,#152155,
#152156,#152157,#152158,#152159,#152160,#152161,#152162,#152163,#152164,
#152165,#152166),.UNSPECIFIED.,.F.,.F.,(4,3,3,3,3,3,3,3,3,3,3,3,3,3,3,3,
3,3,3,3,3,3,3,4),(44.8979422484848,44.9961924492798,45.0945461787255,45.1929541521146,
45.2915320845352,45.3625568007106,45.4611549257132,45.5596127084889,45.6598352762619,
45.7581148339888,45.856361413061,45.9546044960982,46.0563016847417,46.1546860981591,
46.2580396744158,46.3613932506724,46.4587199838046,46.5559210250952,46.6530274701203,
46.7500702965179,46.8471124553621,46.9441490048064,47.0412721236584,47.123889803847),
 .UNSPECIFIED.);
#1608=B_SPLINE_CURVE_WITH_KNOTS('',3,(#152167,#152168,#152169,#152170,#152171,
#152172,#152173,#152174),.UNSPECIFIED.,.F.,.F.,(4,1,1,1,1,4),(47.1238901033263,
47.3602297006343,48.3590661505962,49.3579026005581,50.3567390505199,51.1803881393169),
 .UNSPECIFIED.);
#1609=B_SPLINE_CURVE_WITH_KNOTS('',3,(#152180,#152181,#152182,#152183,#152184,
#152185,#152186,#152187,#152188,#152189,#152190,#152191,#152192,#152193,
#152194,#152195,#152196,#152197,#152198,#152199,#152200,#152201,#152202,
#152203,#152204,#152205,#152206,#152207,#152208,#152209,#152210,#152211,
#152212,#152213,#152214,#152215,#152216,#152217,#152218,#152219,#152220,
#152221,#152222,#152223,#152224,#152225,#152226,#152227,#152228,#152229,
#152230,#152231,#152232,#152233,#152234,#152235,#152236,#152237,#152238,
#152239,#152240,#152241,#152242,#152243,#152244,#152245,#152246,#152247,
#152248,#152249,#152250,#152251,#152252,#152253,#152254,#152255,#152256,
#152257,#152258,#152259,#152260,#152261,#152262,#152263,#152264,#152265,
#152266,#152267,#152268,#152269,#152270,#152271,#152272,#152273,#152274,
#152275,#152276,#152277,#152278,#152279,#152280,#152281,#152282,#152283,
#152284,#152285,#152286,#152287,#152288,#152289,#152290,#152291,#152292,
#152293,#152294,#152295,#152296,#152297,#152298,#152299,#152300,#152301,
#152302,#152303),.UNSPECIFIED.,.F.,.F.,(4,3,3,3,3,3,3,3,3,3,3,3,3,3,3,3,
3,3,3,3,3,3,3,3,3,3,3,3,3,3,3,3,3,3,3,3,3,3,3,3,3,4),(53.4070755243615,
53.5149520672712,53.6231638610662,53.7318758460164,53.8180551329252,53.9166532579289,
54.0151110407057,54.1153336084784,54.2136131662065,54.3118597452799,54.4101028283183,
54.5118000169605,54.6101844303793,54.7135380066332,54.816891582887,54.9154897078907,
55.0139474906675,55.1141700584402,55.2124496161683,55.3106961952417,55.4089392782802,
55.5106364669224,55.6090208803412,55.7123744565951,55.8157280328489,55.9143261578526,
56.0127839406294,56.113006508402,56.2112860661302,56.3095326452036,56.4077757282421,
56.5094729168843,56.6078573303031,56.7112109065569,56.8145644828108,56.9131452274625,
57.0115945031705,57.1099420320622,57.2082227592595,57.3064633876106,57.4047205556631,
57.4639959186668),.UNSPECIFIED.);
#1610=B_SPLINE_CURVE_WITH_KNOTS('',3,(#152304,#152305,#152306,#152307,#152308,
#152309),.UNSPECIFIED.,.F.,.F.,(4,1,1,4),(51.1819113477222,51.8203822330014,
52.8192186829633,53.4070751110266),.UNSPECIFIED.);
#1611=B_SPLINE_CURVE_WITH_KNOTS('',3,(#152311,#152312,#152313,#152314,#152315,
#152316,#152317),.UNSPECIFIED.,.F.,.F.,(4,1,1,1,4),(51.1803881393169,51.3555755004818,
52.3544119504437,53.3532484004056,53.4070751110266),.UNSPECIFIED.);
#1612=B_SPLINE_CURVE_WITH_KNOTS('',3,(#152318,#152319,#152320,#152321,#152322,
#152323,#152324,#152325,#152326,#152327,#152328,#152329,#152330,#152331,
#152332,#152333,#152334,#152335,#152336,#152337,#152338,#152339,#152340,
#152341,#152342,#152343,#152344,#152345,#152346,#152347,#152348,#152349,
#152350,#152351,#152352,#152353,#152354,#152355,#152356,#152357,#152358,
#152359,#152360,#152361,#152362,#152363,#152364,#152365,#152366,#152367,
#152368,#152369,#152370,#152371,#152372,#152373,#152374,#152375,#152376,
#152377,#152378,#152379,#152380,#152381,#152382,#152383,#152384,#152385,
#152386,#152387,#152388,#152389,#152390,#152391,#152392,#152393,#152394,
#152395,#152396,#152397,#152398,#152399,#152400,#152401,#152402,#152403,
#152404,#152405,#152406,#152407,#152408,#152409,#152410,#152411,#152412,
#152413,#152414,#152415,#152416,#152417,#152418,#152419,#152420,#152421,
#152422,#152423,#152424,#152425,#152426,#152427,#152428,#152429,#152430,
#152431,#152432,#152433,#152434,#152435,#152436,#152437,#152438,#152439,
#152440,#152441,#152442,#152443,#152444),.UNSPECIFIED.,.F.,.F.,(4,3,3,3,
3,3,3,3,3,3,3,3,3,3,3,3,3,3,3,3,3,3,3,3,3,3,3,3,3,3,3,3,3,3,3,3,3,3,3,3,
3,3,4),(53.4070751110266,53.5048543854907,53.6024983707769,53.7000367768843,
53.7975186210124,53.8949743677959,53.9924344477701,54.0899931990353,54.1876041339863,
54.2853815723758,54.3520848503674,54.4506829753712,54.549140758148,54.6493633259207,
54.7476428836488,54.8458894627222,54.9441325457608,55.0458297344029,55.1442141478217,
55.2475677240755,55.3509213003293,55.449519425333,55.5479772081097,55.6481997758824,
55.7464793336105,55.8447259126839,55.9429689957224,56.0446661843646,56.1430505977834,
56.2464041740373,56.3497577502912,56.4483558752948,56.5468136580714,56.6470362258441,
56.7453157835723,56.8435623626456,56.9418054456843,57.0435026343265,57.1418870477453,
57.2452406239992,57.3485942002531,57.4471969426278,57.4649113323326),
 .UNSPECIFIED.);
#1613=B_SPLINE_CURVE_WITH_KNOTS('',3,(#152450,#152451,#152452,#152453,#152454,
#152455,#152456,#152457),.UNSPECIFIED.,.F.,.F.,(4,1,1,1,1,4),(59.6902604182062,
59.8110738326964,60.8099102826583,61.8087467326202,62.807583182582,63.7472417658755),
 .UNSPECIFIED.);
#1614=B_SPLINE_CURVE_WITH_KNOTS('',3,(#152458,#152459,#152460,#152461,#152462,
#152463,#152464,#152465,#152466,#152467,#152468,#152469,#152470,#152471,
#152472,#152473,#152474,#152475,#152476,#152477,#152478,#152479,#152480,
#152481,#152482,#152483,#152484,#152485,#152486,#152487,#152488,#152489,
#152490,#152491,#152492,#152493,#152494,#152495,#152496,#152497,#152498,
#152499,#152500,#152501,#152502,#152503,#152504,#152505,#152506,#152507,
#152508,#152509,#152510,#152511,#152512,#152513,#152514,#152515,#152516,
#152517,#152518,#152519,#152520,#152521,#152522,#152523,#152524,#152525,
#152526,#152527),.UNSPECIFIED.,.F.,.F.,(4,3,3,3,3,3,3,3,3,3,3,3,3,3,3,3,
3,3,3,3,3,3,3,4),(57.4639959186668,57.5623571123803,57.6607771204479,57.7593619216273,
57.8134009327727,57.9119990577764,58.010456840553,58.1106794083257,58.2089589660538,
58.3072055451272,58.4054486281658,58.507145816808,58.6055302302267,58.7088838064806,
58.8122373827345,58.9094791608007,59.0070768179764,59.1040671063403,59.2009981633323,
59.2979009849174,59.3959908432396,59.4929780422902,59.5916192302482,59.6902604182062),
 .UNSPECIFIED.);
#1615=B_SPLINE_CURVE_WITH_KNOTS('',3,(#152529,#152530,#152531,#152532,#152533,
#152534,#152535,#152536,#152537,#152538,#152539,#152540,#152541,#152542,
#152543,#152544,#152545,#152546,#152547,#152548,#152549,#152550,#152551,
#152552,#152553,#152554,#152555,#152556,#152557,#152558,#152559,#152560,
#152561,#152562,#152563,#152564,#152565,#152566,#152567,#152568,#152569,
#152570,#152571,#152572,#152573,#152574,#152575,#152576,#152577,#152578,
#152579,#152580,#152581,#152582,#152583,#152584,#152585,#152586,#152587,
#152588,#152589,#152590,#152591,#152592,#152593,#152594,#152595),
 .UNSPECIFIED.,.F.,.F.,(4,3,3,3,3,3,3,3,3,3,3,3,3,3,3,3,3,3,3,3,3,3,4),
(57.4649113323326,57.5633473588617,57.6616773741524,57.7599496392934,57.8581936678956,
57.9564389387784,58.0547832309801,58.1531751315162,58.2517448177315,58.3474306502149,
58.4460287752186,58.5444865579952,58.6447091257679,58.742988683496,58.8412352625694,
58.9394783456079,59.0411755342501,59.139559947669,59.2429135239229,59.3462671001768,
59.4608829140306,59.5755716660049,59.6902604179793),.UNSPECIFIED.);
#1616=B_SPLINE_CURVE_WITH_KNOTS('',3,(#152596,#152597,#152598,#152599,#152600,
#152601,#152602,#152603,#152604,#152605,#152606,#152607,#152608,#152609,
#152610,#152611,#152612,#152613,#152614,#152615,#152616,#152617,#152618,
#152619,#152620,#152621,#152622,#152623,#152624,#152625,#152626,#152627,
#152628,#152629,#152630,#152631,#152632,#152633,#152634,#152635,#152636,
#152637,#152638,#152639,#152640,#152641,#152642,#152643,#152644,#152645,
#152646,#152647,#152648,#152649,#152650,#152651,#152652,#152653,#152654,
#152655,#152656,#152657,#152658,#152659,#152660,#152661,#152662,#152663,
#152664,#152665,#152666,#152667,#152668,#152669,#152670,#152671,#152672,
#152673,#152674,#152675,#152676,#152677,#152678,#152679,#152680,#152681,
#152682,#152683,#152684,#152685,#152686,#152687,#152688,#152689,#152690,
#152691,#152692,#152693,#152694,#152695,#152696,#152697,#152698,#152699,
#152700,#152701,#152702,#152703,#152704,#152705,#152706,#152707,#152708,
#152709,#152710,#152711,#152712,#152713,#152714,#152715,#152716,#152717,
#152718,#152719),.UNSPECIFIED.,.F.,.F.,(4,3,3,3,3,3,3,3,3,3,3,3,3,3,3,3,
3,3,3,3,3,3,3,3,3,3,3,3,3,3,3,3,3,3,3,3,3,3,3,3,3,4),(59.6902604182062,
59.788634173056,59.8869985815969,59.9853827919993,60.0838846667642,60.1824499292134,
60.2811933482972,60.3451035501387,60.4437016751424,60.5421594579191,60.6423820256918,
60.7406615834199,60.8389081624934,60.937151245532,61.0388484341741,61.1372328475929,
61.2405864238468,61.3439400001006,61.4425381251044,61.5409959078813,61.641218475654,
61.7394980333821,61.8377446124555,61.935987695494,62.0376848841361,62.1360692975549,
62.2394228738086,62.3427764500624,62.4413745750661,62.5398323578429,62.6400549256156,
62.7383344833437,62.836581062417,62.9348241454556,63.0365213340978,63.1349057475167,
63.2382593237705,63.3416129000243,63.4431811117946,63.5416227526594,63.6447542498824,
63.7478857471053),.UNSPECIFIED.);
#1617=B_SPLINE_CURVE_WITH_KNOTS('',3,(#152725,#152726,#152727,#152728,#152729,
#152730,#152731,#152732,#152733,#152734,#152735,#152736,#152737,#152738,
#152739,#152740,#152741,#152742,#152743,#152744,#152745,#152746,#152747,
#152748,#152749,#152750,#152751,#152752,#152753,#152754,#152755,#152756,
#152757,#152758,#152759,#152760,#152761,#152762,#152763,#152764,#152765,
#152766,#152767,#152768,#152769,#152770,#152771,#152772,#152773,#152774,
#152775,#152776,#152777,#152778,#152779,#152780,#152781,#152782,#152783,
#152784,#152785,#152786,#152787,#152788,#152789,#152790,#152791,#152792,
#152793,#152794,#152795,#152796,#152797,#152798,#152799,#152800,#152801,
#152802,#152803,#152804,#152805,#152806,#152807,#152808,#152809,#152810,
#152811,#152812,#152813,#152814,#152815,#152816,#152817,#152818,#152819,
#152820,#152821,#152822,#152823,#152824,#152825,#152826,#152827,#152828,
#152829,#152830,#152831,#152832,#152833,#152834,#152835,#152836,#152837,
#152838,#152839,#152840,#152841,#152842,#152843,#152844,#152845,#152846,
#152847,#152848,#152849,#152850,#152851),.UNSPECIFIED.,.F.,.F.,(4,3,3,3,
3,3,3,3,3,3,3,3,3,3,3,3,3,3,3,3,3,3,3,3,3,3,3,3,3,3,3,3,3,3,3,3,3,3,3,3,
3,3,4),(65.9734457253857,66.0704340596178,66.1673127975358,66.264132888756,
66.360925426791,66.4577214670338,66.5546134226801,66.6515579893416,66.7486626585399,
66.8029289824295,66.9015271074332,66.99998489021,67.1002074579826,67.1984870157108,
67.2967335947843,67.3949766778228,67.4966738664649,67.5950582798837,67.6984118561376,
67.8017654323914,67.900363557395,67.9988213401718,68.0990439079444,68.1973234656726,
68.295570044746,68.3938131277846,68.4955103164268,68.5938947298455,68.6972483060994,
68.8006018823533,68.8992000073569,68.9976577901338,69.0978803579064,69.1961599156346,
69.294406494708,69.3926495777466,69.4943467663888,69.5927311798075,69.6960847560613,
69.7994383323151,69.8980412657884,69.9964918402605,70.0313848974635),
 .UNSPECIFIED.);
#1618=B_SPLINE_CURVE_WITH_KNOTS('',3,(#152852,#152853,#152854,#152855,#152856,
#152857,#152858),.UNSPECIFIED.,.F.,.F.,(4,1,1,1,4),(63.7472417658755,63.8064196325439,
64.8052560825058,65.8040925324676,65.9734457253857),.UNSPECIFIED.);
#1619=B_SPLINE_CURVE_WITH_KNOTS('',3,(#152860,#152861,#152862,#152863,#152864,
#152865,#152866,#152867,#152868,#152869,#152870,#152871,#152872,#152873,
#152874,#152875,#152876,#152877,#152878,#152879,#152880,#152881,#152882,
#152883,#152884,#152885,#152886,#152887,#152888,#152889,#152890,#152891,
#152892,#152893,#152894,#152895,#152896,#152897,#152898,#152899,#152900,
#152901,#152902,#152903,#152904,#152905,#152906,#152907,#152908,#152909,
#152910,#152911,#152912,#152913,#152914,#152915,#152916,#152917,#152918,
#152919,#152920,#152921,#152922,#152923,#152924,#152925,#152926,#152927,
#152928,#152929),.UNSPECIFIED.,.F.,.F.,(4,3,3,3,3,3,3,3,3,3,3,3,3,3,3,3,
3,3,3,3,3,3,3,4),(63.7478857471053,63.8461305131556,63.9443749970032,64.0433935852489,
64.1417827849983,64.2411160674923,64.3404493499862,64.4390474749898,64.5375052577667,
64.6377278255393,64.7360073832674,64.8342539623408,64.9324970453792,65.0341942340214,
65.1325786474401,65.2359322236941,65.3392857999481,65.4384637976084,65.5374980774502,
65.6364173808603,65.7352455972603,65.8340208922133,65.9327849002203,65.9734457253857),
 .UNSPECIFIED.);
#1620=B_SPLINE_CURVE_WITH_KNOTS('',3,(#152930,#152931,#152932,#152933,#152934,
#152935,#152936,#152937,#152938,#152939,#152940,#152941,#152942,#152943,
#152944,#152945,#152946,#152947,#152948,#152949,#152950,#152951,#152952,
#152953,#152954,#152955,#152956,#152957,#152958,#152959,#152960,#152961,
#152962,#152963,#152964,#152965,#152966,#152967,#152968,#152969,#152970,
#152971,#152972,#152973,#152974,#152975,#152976,#152977,#152978,#152979,
#152980,#152981,#152982,#152983,#152984,#152985,#152986,#152987,#152988,
#152989,#152990,#152991,#152992,#152993,#152994,#152995,#152996,#152997,
#152998,#152999,#153000,#153001,#153002,#153003,#153004,#153005,#153006,
#153007,#153008,#153009,#153010,#153011,#153012,#153013,#153014,#153015,
#153016,#153017,#153018,#153019,#153020,#153021,#153022,#153023,#153024,
#153025,#153026,#153027,#153028,#153029,#153030,#153031,#153032,#153033,
#153034,#153035,#153036,#153037,#153038,#153039,#153040,#153041,#153042,
#153043,#153044,#153045,#153046,#153047,#153048,#153049,#153050,#153051,
#153052,#153053),.UNSPECIFIED.,.F.,.F.,(4,3,3,3,3,3,3,3,3,3,3,3,3,3,3,3,
3,3,3,3,3,3,3,3,3,3,3,3,3,3,3,3,3,3,3,3,3,3,3,3,3,4),(65.9734457256204,
66.084879805074,66.1968635637049,66.3094957826842,66.3381222499099,66.4367203749136,
66.5351781576905,66.6354007254632,66.7336802831913,66.8319268622647,66.9301699453032,
67.0318671339454,67.1302515473642,67.233605123618,67.3369586998718,67.4355568248755,
67.5340146076523,67.634237175425,67.7325167331532,67.8307633122266,67.9290063952651,
68.0307035839072,68.1290879973261,68.2324415735799,68.3357951498337,68.4343932748374,
68.5328510576142,68.6330736253868,68.731353183115,68.8295997621883,68.9278428452268,
69.029540033869,69.1279244472878,69.2312780235417,69.3346315997956,69.433207943652,
69.5316540255099,69.6299995615715,69.7300683883787,69.8283147588378,69.9292948138189,
70.0302748688001),.UNSPECIFIED.);
#1621=B_SPLINE_CURVE_WITH_KNOTS('',3,(#153059,#153060,#153061,#153062,#153063,
#153064,#153065,#153066),.UNSPECIFIED.,.F.,.F.,(4,1,1,1,1,4),(72.2566310325654,
72.7959476822008,73.7947841321626,74.7936205821245,75.7924570320864,76.3138574014144),
 .UNSPECIFIED.);
#1622=B_SPLINE_CURVE_WITH_KNOTS('',3,(#153067,#153068,#153069,#153070,#153071,
#153072,#153073,#153074,#153075,#153076,#153077,#153078,#153079,#153080,
#153081,#153082,#153083,#153084,#153085,#153086,#153087,#153088,#153089,
#153090,#153091,#153092,#153093,#153094,#153095,#153096,#153097,#153098,
#153099,#153100,#153101,#153102,#153103,#153104,#153105,#153106,#153107,
#153108,#153109,#153110,#153111,#153112,#153113,#153114,#153115,#153116,
#153117,#153118,#153119,#153120,#153121,#153122,#153123,#153124,#153125,
#153126,#153127,#153128,#153129,#153130,#153131,#153132,#153133,#153134,
#153135,#153136),.UNSPECIFIED.,.F.,.F.,(4,3,3,3,3,3,3,3,3,3,3,3,3,3,3,3,
3,3,3,3,3,3,3,4),(70.0313848974635,70.1297026871758,70.2279678893552,70.3262100096092,
70.4244585234034,70.5228092220642,70.6212121566704,70.7197873779156,70.798274782277,
70.8968729072808,70.9953306900579,71.0955532578305,71.1938328155586,71.2920793946318,
71.3903224776704,71.4920196663125,71.5904040797314,71.6937576559851,71.7971112322389,
71.9028340905518,72.0081993817383,72.1133399321502,72.2181701837247,72.2566308185806),
 .UNSPECIFIED.);
#1623=B_SPLINE_CURVE_WITH_KNOTS('',3,(#153138,#153139,#153140,#153141,#153142,
#153143,#153144,#153145,#153146,#153147,#153148,#153149,#153150,#153151,
#153152,#153153,#153154,#153155,#153156,#153157,#153158,#153159,#153160,
#153161,#153162,#153163,#153164,#153165,#153166,#153167,#153168,#153169,
#153170,#153171,#153172,#153173,#153174,#153175,#153176,#153177,#153178,
#153179,#153180,#153181,#153182,#153183,#153184,#153185,#153186,#153187,
#153188,#153189,#153190,#153191,#153192,#153193,#153194,#153195,#153196,
#153197,#153198,#153199,#153200,#153201,#153202,#153203,#153204,#153205,
#153206,#153207),.UNSPECIFIED.,.F.,.F.,(4,3,3,3,3,3,3,3,3,3,3,3,3,3,3,3,
3,3,3,3,3,3,3,4),(70.0302748688001,70.1286603970033,70.2310642233803,70.3334680497574,
70.4320661747611,70.5305239575378,70.6307465253105,70.7290260830386,70.827272662112,
70.9255157451506,71.0272129337928,71.1255973472115,71.2289509234654,71.3323044997193,
71.4298807240689,71.5273176349422,71.6246428433671,71.7219081150621,71.8191441424517,
71.9163815796695,72.013708783522,72.1110862397604,72.2086145464311,72.2566310325654),
 .UNSPECIFIED.);
#1624=B_SPLINE_CURVE_WITH_KNOTS('',3,(#153208,#153209,#153210,#153211,#153212,
#153213,#153214,#153215),.UNSPECIFIED.,.F.,.F.,(4,1,1,1,1,4),(72.2566310325654,
72.3311409496812,73.3299773996431,74.3288138496049,75.3276502995668,76.3138963582499),
 .UNSPECIFIED.);
#1625=B_SPLINE_CURVE_WITH_KNOTS('',3,(#153221,#153222,#153223,#153224,#153225,
#153226,#153227,#153228,#153229,#153230,#153231,#153232,#153233,#153234,
#153235,#153236,#153237,#153238,#153239,#153240,#153241,#153242,#153243,
#153244,#153245,#153246,#153247,#153248,#153249,#153250,#153251,#153252,
#153253,#153254,#153255,#153256,#153257,#153258,#153259,#153260,#153261,
#153262,#153263,#153264,#153265,#153266,#153267,#153268,#153269,#153270,
#153271,#153272,#153273,#153274,#153275,#153276,#153277,#153278,#153279,
#153280,#153281,#153282,#153283,#153284,#153285,#153286,#153287,#153288,
#153289,#153290,#153291,#153292,#153293,#153294,#153295,#153296,#153297,
#153298,#153299,#153300,#153301,#153302,#153303,#153304,#153305,#153306,
#153307,#153308,#153309,#153310,#153311,#153312,#153313,#153314,#153315,
#153316,#153317,#153318,#153319,#153320,#153321,#153322,#153323,#153324,
#153325,#153326,#153327,#153328,#153329,#153330,#153331,#153332,#153333,
#153334,#153335,#153336,#153337,#153338,#153339,#153340,#153341,#153342,
#153343,#153344),.UNSPECIFIED.,.F.,.F.,(4,3,3,3,3,3,3,3,3,3,3,3,3,3,3,3,
3,3,3,3,3,3,3,3,3,3,3,3,3,3,3,3,3,3,3,3,3,3,3,3,3,4),(78.5398164398063,
78.6677108218491,78.788966381972,78.8875645069757,78.9860222897523,79.086244857525,
79.1845244152532,79.2827709943266,79.3810140773651,79.4827112660073,79.5810956794261,
79.68444925568,79.7878028319339,79.8864009569376,79.9848587397144,80.0850813074871,
80.1833608652152,80.2816074442886,80.3798505273271,80.4815477159693,80.5799321293881,
80.6832857056419,80.7866392818958,80.8852374068995,80.9836951896763,81.0839177574489,
81.1821973151771,81.2804438942504,81.3786869772889,81.4803841659311,81.5787685793499,
81.6821221556038,81.7854757318576,81.8868624768865,81.9852993359155,82.0836394970758,
82.1819125591245,82.2801480487663,82.3784063346505,82.4766798010887,82.5750347961583,
82.5965696920888),.UNSPECIFIED.);
#1626=B_SPLINE_CURVE_WITH_KNOTS('',3,(#153345,#153346,#153347,#153348,#153349,
#153350),.UNSPECIFIED.,.F.,.F.,(4,1,1,4),(76.3138574014144,76.7912934820483,
77.7901299320101,78.539816339745),.UNSPECIFIED.);
#1627=B_SPLINE_CURVE_WITH_KNOTS('',3,(#153352,#153353,#153354,#153355,#153356,
#153357,#153358),.UNSPECIFIED.,.F.,.F.,(4,1,1,1,4),(76.3138963582499,76.3264867495287,
77.3253231994906,78.3241596494524,78.539816339745),.UNSPECIFIED.);
#1628=B_SPLINE_CURVE_WITH_KNOTS('',3,(#153359,#153360,#153361,#153362,#153363,
#153364,#153365,#153366,#153367,#153368,#153369,#153370,#153371,#153372,
#153373,#153374,#153375,#153376,#153377,#153378,#153379,#153380,#153381,
#153382,#153383,#153384,#153385,#153386,#153387,#153388,#153389,#153390,
#153391,#153392,#153393,#153394,#153395,#153396,#153397,#153398,#153399,
#153400,#153401,#153402,#153403,#153404,#153405,#153406,#153407,#153408,
#153409,#153410,#153411,#153412,#153413,#153414,#153415,#153416,#153417,
#153418,#153419,#153420,#153421,#153422,#153423,#153424,#153425,#153426,
#153427,#153428,#153429,#153430,#153431,#153432,#153433,#153434,#153435,
#153436,#153437,#153438,#153439,#153440,#153441,#153442,#153443,#153444,
#153445,#153446,#153447,#153448,#153449,#153450,#153451,#153452,#153453,
#153454,#153455,#153456,#153457,#153458,#153459,#153460,#153461,#153462,
#153463,#153464,#153465,#153466,#153467,#153468,#153469,#153470,#153471,
#153472,#153473,#153474,#153475,#153476,#153477,#153478,#153479,#153480,
#153481,#153482),.UNSPECIFIED.,.F.,.F.,(4,3,3,3,3,3,3,3,3,3,3,3,3,3,3,3,
3,3,3,3,3,3,3,3,3,3,3,3,3,3,3,3,3,3,3,3,3,3,3,3,3,4),(78.539816339745,78.6377138097037,
78.7346673304386,78.8315786913982,78.9284788661298,79.0271081744509,79.1241353185132,
79.2235657089638,79.3229960994143,79.421594224418,79.5200520071948,79.6202745749675,
79.7185541326956,79.8168007117689,79.9150437948075,80.0167409834497,80.1151253968685,
80.2184789731223,80.3218325493762,80.4204306743799,80.5188884571567,80.6191110249294,
80.7173905826575,80.8156371617309,80.9138802447694,81.0155774334116,81.1139618468304,
81.2173154230842,81.3206689993381,81.4192671243418,81.5177249071184,81.6179474748911,
81.7162270326193,81.8144736116927,81.9127166947311,82.0144138833733,82.1127982967921,
82.216151873046,82.3195054492999,82.4180964130078,82.5165362141558,82.5977152335624),
 .UNSPECIFIED.);
#1629=B_SPLINE_CURVE_WITH_KNOTS('',3,(#153488,#153489,#153490,#153491,#153492,
#153493,#153494,#153495),.UNSPECIFIED.,.F.,.F.,(4,1,1,1,1,4),(84.8230070320566,
85.7808215317051,86.779657981667,87.7784944316289,88.7773308815908,88.8809435133539),
 .UNSPECIFIED.);
#1630=B_SPLINE_CURVE_WITH_KNOTS('',3,(#153496,#153497,#153498,#153499,#153500,
#153501,#153502,#153503,#153504,#153505,#153506,#153507,#153508,#153509,
#153510,#153511,#153512,#153513,#153514,#153515,#153516,#153517,#153518,
#153519,#153520,#153521,#153522,#153523,#153524,#153525,#153526,#153527,
#153528,#153529,#153530,#153531,#153532,#153533,#153534,#153535,#153536,
#153537,#153538,#153539,#153540,#153541,#153542,#153543,#153544,#153545,
#153546,#153547,#153548,#153549,#153550,#153551,#153552,#153553,#153554,
#153555,#153556,#153557,#153558,#153559,#153560,#153561,#153562,#153563,
#153564,#153565),.UNSPECIFIED.,.F.,.F.,(4,3,3,3,3,3,3,3,3,3,3,3,3,3,3,3,
3,3,3,3,3,3,3,4),(82.5965696920888,82.695141358,82.7843121818195,82.8829103068232,
82.9813680895999,83.0815906573726,83.1798702151008,83.2781167941742,83.3763598772127,
83.4780570658548,83.5764414792737,83.6797950555275,83.7831486317814,83.8817467567851,
83.9802045395617,84.0804271073344,84.1787066650625,84.2769532441359,84.3751963271743,
84.4768935158166,84.5752779292353,84.6786315054893,84.7819850817433,84.8230016469246),
 .UNSPECIFIED.);
#1631=B_SPLINE_CURVE_WITH_KNOTS('',3,(#153567,#153568,#153569,#153570,#153571,
#153572,#153573,#153574,#153575,#153576,#153577,#153578,#153579,#153580,
#153581,#153582,#153583,#153584,#153585,#153586,#153587,#153588,#153589,
#153590,#153591,#153592,#153593,#153594,#153595,#153596,#153597,#153598,
#153599,#153600,#153601,#153602,#153603,#153604,#153605,#153606,#153607,
#153608,#153609,#153610,#153611,#153612,#153613,#153614,#153615,#153616,
#153617,#153618,#153619,#153620,#153621,#153622,#153623,#153624,#153625,
#153626,#153627,#153628,#153629,#153630,#153631,#153632,#153633,#153634,
#153635,#153636),.UNSPECIFIED.,.F.,.F.,(4,3,3,3,3,3,3,3,3,3,3,3,3,3,3,3,
3,3,3,3,3,3,3,4),(82.5977152335624,82.6960046045216,82.7942552746611,82.8924967320984,
82.9907584472983,83.0891304035499,83.1875670560788,83.2861621230254,83.3183418992618,
83.4169400242655,83.5153978070419,83.6156203748146,83.7138999325428,83.8121465116162,
83.9103895946549,84.0120867832971,84.1104711967159,84.2138247729698,84.3171783492237,
84.4205578302504,84.5236543867486,84.6265834813177,84.7292989065991,84.8230016469246),
 .UNSPECIFIED.);
#1632=B_SPLINE_CURVE_WITH_KNOTS('',3,(#153637,#153638,#153639,#153640,#153641,
#153642,#153643,#153644,#153645,#153646,#153647,#153648,#153649,#153650,
#153651,#153652,#153653,#153654,#153655,#153656,#153657,#153658,#153659,
#153660,#153661,#153662,#153663,#153664,#153665,#153666,#153667,#153668,
#153669,#153670,#153671,#153672,#153673,#153674,#153675,#153676,#153677,
#153678,#153679,#153680,#153681,#153682,#153683,#153684,#153685,#153686,
#153687,#153688,#153689,#153690,#153691,#153692,#153693,#153694,#153695,
#153696,#153697,#153698,#153699,#153700,#153701,#153702,#153703,#153704,
#153705,#153706,#153707,#153708,#153709,#153710,#153711,#153712,#153713,
#153714,#153715,#153716,#153717,#153718,#153719,#153720,#153721,#153722,
#153723,#153724,#153725,#153726,#153727,#153728,#153729,#153730,#153731,
#153732,#153733,#153734,#153735,#153736,#153737,#153738,#153739,#153740,
#153741,#153742,#153743,#153744,#153745,#153746,#153747,#153748,#153749,
#153750,#153751,#153752,#153753,#153754,#153755,#153756,#153757,#153758,
#153759,#153760),.UNSPECIFIED.,.F.,.F.,(4,3,3,3,3,3,3,3,3,3,3,3,3,3,3,3,
3,3,3,3,3,3,3,3,3,3,3,3,3,3,3,3,3,3,3,3,3,3,3,3,3,4),(84.8230016472006,
84.9261861619506,85.0296647966982,85.1332945907094,85.2372126194226,85.3160147991856,
85.4146129241893,85.5130707069661,85.6132932747388,85.7115728324669,85.8098194115403,
85.9080624945788,86.0097596832209,86.1081440966397,86.2114976728936,86.3148512491474,
86.4134493741511,86.5119071569279,86.6121297247006,86.7104092824287,86.8086558615021,
86.9068989445406,87.0085961331827,87.1069805466016,87.2103341228554,87.3136876991093,
87.412285824113,87.5107436068898,87.6109661746624,87.7092457323906,87.807492311464,
87.9057353945025,88.0074325831446,88.1058169965635,88.2091705728173,88.3125241490712,
88.4111137865082,88.5095698168674,88.6079122101949,88.7061871882943,88.8044419893836,
88.8801389091725),.UNSPECIFIED.);
#1633=B_SPLINE_CURVE_WITH_KNOTS('',3,(#153766,#153767,#153768,#153769,#153770,
#153771,#153772,#153773,#153774,#153775,#153776,#153777,#153778,#153779,
#153780,#153781,#153782,#153783,#153784,#153785,#153786,#153787,#153788,
#153789,#153790,#153791,#153792,#153793,#153794,#153795,#153796,#153797,
#153798,#153799,#153800,#153801,#153802,#153803,#153804,#153805,#153806,
#153807,#153808,#153809,#153810,#153811,#153812,#153813,#153814,#153815,
#153816,#153817,#153818,#153819,#153820,#153821,#153822,#153823,#153824,
#153825,#153826,#153827,#153828,#153829,#153830,#153831,#153832,#153833,
#153834,#153835,#153836,#153837,#153838,#153839,#153840,#153841,#153842,
#153843,#153844,#153845,#153846,#153847,#153848,#153849,#153850,#153851,
#153852,#153853,#153854,#153855,#153856,#153857,#153858,#153859,#153860,
#153861,#153862,#153863,#153864,#153865,#153866,#153867,#153868,#153869,
#153870,#153871,#153872,#153873,#153874,#153875,#153876,#153877,#153878,
#153879,#153880,#153881,#153882,#153883,#153884,#153885,#153886,#153887,
#153888,#153889),.UNSPECIFIED.,.F.,.F.,(4,3,3,3,3,3,3,3,3,3,3,3,3,3,3,3,
3,3,3,3,3,3,3,3,3,3,3,3,3,3,3,3,3,3,3,3,3,3,3,3,3,4),(91.1061869541041,
91.204341964477,91.3024795334308,91.400629164884,91.4988897541857,91.5972075103079,
91.6957053368615,91.7738402314764,91.8724383564801,91.9708961392568,92.0711187070295,
92.1693982647576,92.267644843831,92.3658879268695,92.4675851155117,92.5659695289306,
92.6693231051844,92.7726766814383,92.871274806442,92.9697325892188,93.0699551569915,
93.1682347147196,93.2664812937929,93.3647243768313,93.4664215654735,93.5648059788923,
93.6681595551462,93.7715131314001,93.8701112564038,93.9685690391805,94.0687916069532,
94.1670711646814,94.2653177437547,94.3635608267932,94.4652580154354,94.5636424288543,
94.6669960051081,94.770349581362,94.8689185475107,94.9673651080125,95.0657083030554,
95.1638472961989),.UNSPECIFIED.);
#1634=B_SPLINE_CURVE_WITH_KNOTS('',3,(#153890,#153891,#153892,#153893,#153894,
#153895),.UNSPECIFIED.,.F.,.F.,(4,1,1,4),(88.8809435133539,89.7761673315526,
90.7750037815145,91.1061798192275),.UNSPECIFIED.);
#1635=B_SPLINE_CURVE_WITH_KNOTS('',3,(#153897,#153898,#153899,#153900,#153901,
#153902,#153903,#153904,#153905,#153906,#153907,#153908,#153909,#153910,
#153911,#153912,#153913,#153914,#153915,#153916,#153917,#153918,#153919,
#153920,#153921,#153922,#153923,#153924,#153925,#153926,#153927,#153928,
#153929,#153930,#153931,#153932,#153933,#153934,#153935,#153936,#153937,
#153938,#153939,#153940,#153941,#153942,#153943,#153944,#153945,#153946,
#153947,#153948,#153949,#153950,#153951,#153952,#153953,#153954,#153955,
#153956,#153957,#153958,#153959,#153960,#153961,#153962,#153963,#153964,
#153965,#153966,#153967,#153968,#153969),.UNSPECIFIED.,.F.,.F.,(4,3,3,3,
3,3,3,3,3,3,3,3,3,3,3,3,3,3,3,3,3,3,3,3,4),(88.8801389091725,88.9783987534772,
89.0767679360319,89.1752003650069,89.2737927525417,89.3113605990331,89.4099587240368,
89.5084165068135,89.6086390745862,89.7069186323143,89.8051652113877,89.9034082944262,
90.0051054830683,90.1034898964871,90.206843472741,90.3101970489949,90.409695787095,
90.5067185530535,90.6036495481491,90.7005198981798,90.8019366620839,90.8988156754796,
90.9957205549586,91.0927209416411,91.1061869537961),.UNSPECIFIED.);
#1636=B_SPLINE_CURVE_WITH_KNOTS('',3,(#153970,#153971,#153972,#153973,#153974,
#153975,#153976,#153977,#153978,#153979,#153980,#153981,#153982,#153983,
#153984,#153985,#153986,#153987,#153988,#153989,#153990,#153991,#153992,
#153993,#153994,#153995,#153996,#153997,#153998,#153999,#154000,#154001,
#154002,#154003,#154004,#154005,#154006,#154007,#154008,#154009,#154010,
#154011,#154012,#154013,#154014,#154015,#154016,#154017,#154018,#154019,
#154020,#154021,#154022,#154023,#154024,#154025,#154026,#154027,#154028,
#154029,#154030,#154031,#154032,#154033,#154034,#154035,#154036,#154037,
#154038,#154039,#154040,#154041,#154042,#154043,#154044,#154045,#154046,
#154047,#154048,#154049,#154050,#154051,#154052,#154053,#154054,#154055,
#154056,#154057,#154058,#154059,#154060,#154061,#154062,#154063,#154064,
#154065,#154066,#154067,#154068,#154069,#154070,#154071,#154072,#154073,
#154074,#154075,#154076,#154077,#154078,#154079,#154080,#154081,#154082,
#154083,#154084,#154085,#154086,#154087,#154088,#154089,#154090,#154091,
#154092,#154093),.UNSPECIFIED.,.F.,.F.,(4,3,3,3,3,3,3,3,3,3,3,3,3,3,3,3,
3,3,3,3,3,3,3,3,3,3,3,3,3,3,3,3,3,3,3,3,3,3,3,3,3,4),(91.1061869541041,
91.2465035596771,91.3090334989568,91.4076316239605,91.5060894067374,91.60631197451,
91.7045915322382,91.8028381113116,91.9010811943501,92.0027783829923,92.101162796411,
92.2045163726649,92.3078699489187,92.4064680739224,92.5049258566991,92.6051484244718,
92.7034279822,92.8016745612733,92.8999176443118,93.001614832954,93.0999992463728,
93.2033528226267,93.3067063988806,93.4053045238843,93.5037623066611,93.6039848744337,
93.7022644321619,93.8005110112353,93.8987540942738,94.0004512829159,94.0988356963347,
94.2021892725886,94.3055428488424,94.4041508037272,94.5025891903085,94.6009312472761,
94.6992065724929,94.7974446925405,94.895715960323,94.9940021459656,95.0923959721231,
95.1629909128946),.UNSPECIFIED.);
#1637=B_SPLINE_CURVE_WITH_KNOTS('',3,(#154099,#154100,#154101,#154102,#154103,
#154104,#154105,#154106),.UNSPECIFIED.,.F.,.F.,(4,1,1,1,1,4),(97.3893797693875,
97.7668589312476,98.7656953812095,99.7645318311714,100.763368281133,101.445901947532),
 .UNSPECIFIED.);
#1638=B_SPLINE_CURVE_WITH_KNOTS('',3,(#154107,#154108,#154109,#154110,#154111,
#154112,#154113,#154114,#154115,#154116,#154117,#154118,#154119,#154120,
#154121,#154122,#154123,#154124,#154125,#154126,#154127,#154128,#154129,
#154130,#154131,#154132,#154133,#154134,#154135,#154136,#154137,#154138,
#154139,#154140,#154141,#154142,#154143,#154144,#154145,#154146,#154147,
#154148,#154149,#154150,#154151,#154152,#154153,#154154,#154155,#154156,
#154157,#154158,#154159,#154160,#154161,#154162,#154163,#154164,#154165,
#154166,#154167,#154168,#154169,#154170,#154171,#154172,#154173,#154174,
#154175,#154176,#154177,#154178,#154179),.UNSPECIFIED.,.F.,.F.,(4,3,3,3,
3,3,3,3,3,3,3,3,3,3,3,3,3,3,3,3,3,3,3,3,4),(95.1638472961989,95.2620942640701,
95.3603371179254,95.4625493462751,95.5609328596376,95.659386716781,95.7579931491462,
95.7691860313239,95.8677841563277,95.9662419391048,96.0664645068774,96.1647440646056,
96.262990643679,96.3612337267176,96.4629309153596,96.5613153287785,96.6646689050321,
96.7680224812858,96.8674993725789,96.9668292609827,97.0660403563899,97.1651524247994,
97.2642075332238,97.3632407686269,97.3893722612837),.UNSPECIFIED.);
#1639=B_SPLINE_CURVE_WITH_KNOTS('',3,(#154181,#154182,#154183,#154184,#154185,
#154186,#154187,#154188,#154189,#154190,#154191,#154192,#154193,#154194,
#154195,#154196,#154197,#154198,#154199,#154200,#154201,#154202,#154203,
#154204,#154205,#154206,#154207,#154208,#154209,#154210,#154211,#154212,
#154213,#154214,#154215,#154216,#154217,#154218,#154219,#154220,#154221,
#154222,#154223,#154224,#154225,#154226,#154227,#154228,#154229,#154230,
#154231,#154232,#154233,#154234,#154235,#154236,#154237,#154238,#154239,
#154240,#154241,#154242,#154243,#154244,#154245,#154246,#154247,#154248,
#154249,#154250),.UNSPECIFIED.,.F.,.F.,(4,3,3,3,3,3,3,3,3,3,3,3,3,3,3,3,
3,3,3,3,3,3,3,4),(95.1629909128946,95.2615807925411,95.3043792988043,95.402977423808,
95.5014352065848,95.6016577743575,95.6999373320856,95.798183911159,95.8964269941974,
95.9981241828396,96.0965085962584,96.1998621725123,96.3032157487662,96.4018138737699,
96.5002716565467,96.6004942243194,96.6987737820475,96.7970203611209,96.8952634441594,
96.9969606328015,97.0953450462203,97.1986986224742,97.302052198728,97.3893722612837),
 .UNSPECIFIED.);
#1640=B_SPLINE_CURVE_WITH_KNOTS('',3,(#154251,#154252,#154253,#154254,#154255,
#154256,#154257,#154258),.UNSPECIFIED.,.F.,.F.,(4,1,1,1,1,4),(97.3893809708947,
98.3008886486899,99.2997250986518,100.298561548614,101.297397998576,101.447496608354),
 .UNSPECIFIED.);
#1641=B_SPLINE_CURVE_WITH_KNOTS('',3,(#154264,#154265,#154266,#154267,#154268,
#154269,#154270,#154271,#154272,#154273,#154274,#154275,#154276,#154277,
#154278,#154279,#154280,#154281,#154282,#154283,#154284,#154285,#154286,
#154287,#154288,#154289,#154290,#154291,#154292,#154293,#154294,#154295,
#154296,#154297,#154298,#154299,#154300,#154301,#154302,#154303,#154304,
#154305,#154306,#154307,#154308,#154309,#154310,#154311,#154312,#154313,
#154314,#154315,#154316,#154317,#154318,#154319,#154320,#154321,#154322,
#154323,#154324,#154325,#154326,#154327,#154328,#154329,#154330,#154331,
#154332,#154333,#154334,#154335,#154336,#154337,#154338,#154339,#154340,
#154341,#154342,#154343,#154344,#154345,#154346,#154347,#154348,#154349,
#154350,#154351,#154352,#154353,#154354,#154355,#154356,#154357,#154358,
#154359,#154360,#154361,#154362,#154363,#154364,#154365,#154366,#154367,
#154368,#154369,#154370,#154371,#154372,#154373,#154374,#154375,#154376,
#154377,#154378,#154379,#154380,#154381,#154382,#154383,#154384,#154385,
#154386,#154387),.UNSPECIFIED.,.F.,.F.,(4,3,3,3,3,3,3,3,3,3,3,3,3,3,3,3,
3,3,3,3,3,3,3,3,3,3,3,3,3,3,3,3,3,3,3,3,3,3,3,3,3,4),(103.672557568463,
103.759877631019,103.858475756023,103.956933538799,104.057156106572,104.1554356643,
104.253682243374,104.351925326412,104.453622515054,104.552006928473,104.655360504727,
104.758714080981,104.857312205985,104.955769988762,105.055992556534,105.154272114262,
105.252518693336,105.350761776374,105.452458965017,105.550843378435,105.654196954689,
105.757550530943,105.856148655947,105.954606438723,106.054829006496,106.153108564224,
106.251355143298,106.349598226336,106.451295414978,106.549679828397,106.653033404651,
106.756386980905,106.854986798951,106.953445809633,107.051788768345,107.150068003066,
107.248313037022,107.34655335305,107.444881222478,107.543251670412,107.641785788067,
107.729756514353),.UNSPECIFIED.);
#1642=B_SPLINE_CURVE_WITH_KNOTS('',3,(#154388,#154389,#154390,#154391,#154392,
#154393),.UNSPECIFIED.,.F.,.F.,(4,1,1,4),(101.445901947532,101.762204731095,
102.761041181057,103.672548858805),.UNSPECIFIED.);
#1643=B_SPLINE_CURVE_WITH_KNOTS('',3,(#154395,#154396,#154397,#154398,#154399,
#154400),.UNSPECIFIED.,.F.,.F.,(4,1,1,4),(101.447496608354,102.296234448537,
103.295070898499,103.672550060316),.UNSPECIFIED.);
#1644=B_SPLINE_CURVE_WITH_KNOTS('',3,(#154401,#154402,#154403,#154404,#154405,
#154406,#154407,#154408,#154409,#154410,#154411,#154412,#154413,#154414,
#154415,#154416,#154417,#154418,#154419,#154420,#154421,#154422,#154423,
#154424,#154425,#154426,#154427,#154428,#154429,#154430,#154431,#154432,
#154433,#154434,#154435,#154436,#154437,#154438,#154439,#154440,#154441,
#154442,#154443,#154444,#154445,#154446,#154447,#154448,#154449,#154450,
#154451,#154452,#154453,#154454,#154455,#154456,#154457,#154458,#154459,
#154460,#154461,#154462,#154463,#154464,#154465,#154466,#154467,#154468,
#154469,#154470,#154471,#154472,#154473,#154474,#154475,#154476,#154477,
#154478,#154479,#154480,#154481,#154482,#154483,#154484,#154485,#154486,
#154487,#154488,#154489,#154490,#154491,#154492,#154493,#154494,#154495,
#154496,#154497,#154498,#154499,#154500,#154501,#154502,#154503,#154504,
#154505,#154506,#154507,#154508,#154509,#154510,#154511,#154512,#154513,
#154514,#154515,#154516,#154517,#154518,#154519,#154520,#154521,#154522,
#154523,#154524,#154525,#154526,#154527),.UNSPECIFIED.,.F.,.F.,(4,3,3,3,
3,3,3,3,3,3,3,3,3,3,3,3,3,3,3,3,3,3,3,3,3,3,3,3,3,3,3,3,3,3,3,3,3,3,3,3,
3,3,4),(103.672557568463,103.771601702603,103.870660322484,103.96976131202,
104.06899945985,104.168318657834,104.267812431338,104.293907348461,104.392505473465,
104.490963256242,104.591185824014,104.689465381742,104.787711960816,104.885955043854,
104.987652232497,105.086036645915,105.189390222169,105.292743798423,105.391341923427,
105.489799706204,105.590022273976,105.688301831705,105.786548410778,105.884791493817,
105.986488682459,106.084873095877,106.188226672131,106.291580248385,106.390178373389,
106.488636156165,106.588858723938,106.687138281666,106.78538486074,106.883627943778,
106.98532513242,107.083709545839,107.187063122093,107.290416698347,107.389023062577,
107.487464394931,107.585810440439,107.684086111444,107.730086386038),
 .UNSPECIFIED.);
#1645=B_SPLINE_CURVE_WITH_KNOTS('',3,(#154533,#154534,#154535,#154536,#154537,
#154538,#154539,#154540,#154541,#154542,#154543,#154544,#154545,#154546,
#154547,#154548,#154549,#154550,#154551,#154552,#154553,#154554,#154555,
#154556,#154557,#154558,#154559,#154560,#154561,#154562,#154563,#154564,
#154565,#154566,#154567,#154568,#154569,#154570,#154571,#154572,#154573,
#154574,#154575,#154576,#154577,#154578,#154579,#154580,#154581,#154582,
#154583,#154584,#154585,#154586,#154587,#154588,#154589,#154590,#154591,
#154592,#154593,#154594,#154595,#154596,#154597,#154598,#154599,#154600,
#154601,#154602,#154603,#154604,#154605,#154606,#154607,#154608,#154609,
#154610,#154611,#154612,#154613,#154614,#154615,#154616,#154617,#154618,
#154619,#154620,#154621,#154622,#154623,#154624,#154625,#154626,#154627,
#154628,#154629,#154630,#154631,#154632,#154633,#154634,#154635,#154636,
#154637,#154638,#154639,#154640,#154641,#154642,#154643,#154644,#154645,
#154646,#154647,#154648,#154649,#154650,#154651,#154652,#154653,#154654,
#154655,#154656,#154657,#154658,#154659),.UNSPECIFIED.,.F.,.F.,(4,3,3,3,
3,3,3,3,3,3,3,3,3,3,3,3,3,3,3,3,3,3,3,3,3,3,3,3,3,3,3,3,3,3,3,3,3,3,3,3,
3,3,4),(109.955742875951,110.055241614051,110.152151423466,110.249014842069,
110.345862894414,110.447330365998,110.544300028994,110.641334438528,110.738518045248,
110.751732780752,110.850330905756,110.948788688532,111.049011256305,111.147290814033,
111.245537393107,111.343780476145,111.445477664787,111.543862078206,111.64721565446,
111.750569230714,111.849167355718,111.947625138494,112.047847706267,112.146127263995,
112.244373843069,112.342616926107,112.444314114749,112.542698528168,112.646052104422,
112.749405680676,112.84800380568,112.946461588456,113.046684156229,113.144963713957,
113.243210293031,113.341453376069,113.443150564711,113.54153497813,113.644888554384,
113.748242130638,113.846836224895,113.945278284723,114.013656770728),
 .UNSPECIFIED.);
#1646=B_SPLINE_CURVE_WITH_KNOTS('',3,(#154660,#154661,#154662,#154663,#154664,
#154665,#154666,#154667,#154668,#154669,#154670,#154671,#154672,#154673,
#154674,#154675,#154676,#154677,#154678,#154679,#154680,#154681,#154682,
#154683,#154684,#154685,#154686,#154687,#154688,#154689,#154690,#154691,
#154692,#154693,#154694,#154695,#154696,#154697,#154698,#154699,#154700,
#154701,#154702,#154703,#154704,#154705,#154706,#154707,#154708,#154709,
#154710,#154711,#154712,#154713,#154714,#154715,#154716,#154717,#154718,
#154719,#154720,#154721,#154722,#154723,#154724,#154725,#154726,#154727,
#154728,#154729),.UNSPECIFIED.,.F.,.F.,(4,3,3,3,3,3,3,3,3,3,3,3,3,3,3,3,
3,3,3,3,3,3,3,4),(107.729756514353,107.755223430866,107.85382155587,107.952279338646,
108.052501906419,108.150781464147,108.24902804322,108.347271126259,108.448968314901,
108.54735272832,108.650706304574,108.754059880828,108.852658005832,108.951115788609,
109.051338356381,109.149617914109,109.247864493183,109.346107576221,109.447804764864,
109.546189178282,109.649542754536,109.75289633079,109.893212936346,109.955742875643),
 .UNSPECIFIED.);
#1647=B_SPLINE_CURVE_WITH_KNOTS('',3,(#154731,#154732,#154733,#154734,#154735,
#154736,#154737,#154738,#154739,#154740,#154741,#154742,#154743,#154744,
#154745,#154746,#154747,#154748,#154749,#154750,#154751,#154752,#154753,
#154754,#154755,#154756,#154757,#154758,#154759,#154760,#154761,#154762,
#154763,#154764,#154765,#154766,#154767,#154768,#154769,#154770,#154771,
#154772,#154773,#154774,#154775,#154776,#154777,#154778,#154779,#154780,
#154781,#154782,#154783,#154784,#154785,#154786,#154787,#154788,#154789,
#154790,#154791,#154792,#154793,#154794,#154795,#154796,#154797,#154798,
#154799,#154800),.UNSPECIFIED.,.F.,.F.,(4,3,3,3,3,3,3,3,3,3,3,3,3,3,3,3,
3,3,3,3,3,3,3,4),(107.730086386038,107.82832774994,107.926578848836,108.024934135355,
108.123344660194,108.22192400452,108.289253148309,108.387851273313,108.48630905609,
108.586531623862,108.68481118159,108.783057760664,108.881300843702,108.982998032344,
109.081382445763,109.184736022017,109.288089598271,109.386591328536,109.484956309732,
109.583214317042,109.681399820024,109.779540599734,109.877698313765,109.955742875643),
 .UNSPECIFIED.);
#1648=B_SPLINE_CURVE_WITH_KNOTS('',3,(#154801,#154802,#154803,#154804,#154805,
#154806,#154807,#154808),.UNSPECIFIED.,.F.,.F.,(4,1,1,1,1,4),(109.955750010575,
110.286926048232,111.285762498194,112.284598948156,113.283435398118,114.012186908316),
 .UNSPECIFIED.);
#1649=B_SPLINE_CURVE_WITH_KNOTS('',3,(#154814,#154815,#154816,#154817,#154818,
#154819,#154820,#154821,#154822,#154823,#154824,#154825,#154826,#154827,
#154828,#154829,#154830,#154831,#154832,#154833,#154834,#154835,#154836,
#154837,#154838,#154839,#154840,#154841,#154842,#154843,#154844,#154845,
#154846,#154847,#154848,#154849,#154850,#154851,#154852,#154853,#154854,
#154855,#154856,#154857,#154858,#154859,#154860,#154861,#154862,#154863,
#154864,#154865,#154866,#154867,#154868,#154869,#154870,#154871,#154872,
#154873,#154874,#154875,#154876,#154877,#154878,#154879,#154880,#154881,
#154882,#154883,#154884,#154885,#154886,#154887,#154888,#154889,#154890,
#154891,#154892,#154893,#154894,#154895,#154896,#154897,#154898,#154899,
#154900,#154901,#154902,#154903,#154904,#154905,#154906,#154907,#154908,
#154909,#154910,#154911,#154912,#154913,#154914,#154915,#154916,#154917,
#154918,#154919,#154920,#154921,#154922,#154923,#154924,#154925,#154926,
#154927,#154928,#154929,#154930,#154931,#154932,#154933,#154934,#154935,
#154936,#154937),.UNSPECIFIED.,.F.,.F.,(4,3,3,3,3,3,3,3,3,3,3,3,3,3,3,3,
3,3,3,3,3,3,3,3,3,3,3,3,3,3,3,3,3,3,3,3,3,3,3,3,3,4),(116.238928182823,
116.341566510357,116.44447107289,116.547509821617,116.650828963887,116.744751480523,
116.843349605527,116.941807388303,117.042029956076,117.140309513804,117.238556092877,
117.336799175916,117.438496364558,117.536880777977,117.640234354231,117.743587930485,
117.842186055489,117.940643838266,118.040866406038,118.139145963766,118.23739254284,
118.335635625878,118.437332814521,118.53571722794,118.639070804193,118.742424380447,
118.841022505451,118.939480288227,119.039702856,119.137982413728,119.236228992802,
119.33447207584,119.436169264482,119.534553677901,119.637907254155,119.741260830409,
119.839851983063,119.938309194714,120.036651331122,120.134925920028,120.233176074189,
120.296103360098),.UNSPECIFIED.);
#1650=B_SPLINE_CURVE_WITH_KNOTS('',3,(#154938,#154939,#154940,#154941,#154942,
#154943,#154944,#154945,#154946,#154947,#154948,#154949,#154950,#154951,
#154952,#154953,#154954,#154955,#154956,#154957,#154958,#154959,#154960,
#154961,#154962,#154963,#154964,#154965,#154966,#154967,#154968,#154969,
#154970,#154971,#154972,#154973,#154974,#154975,#154976,#154977,#154978,
#154979,#154980,#154981,#154982,#154983,#154984,#154985,#154986,#154987,
#154988,#154989,#154990,#154991,#154992,#154993,#154994,#154995,#154996,
#154997,#154998,#154999,#155000,#155001,#155002,#155003,#155004,#155005,
#155006,#155007),.UNSPECIFIED.,.F.,.F.,(4,3,3,3,3,3,3,3,3,3,3,3,3,3,3,3,
3,3,3,3,3,3,3,4),(114.013656770728,114.111953348359,114.21020738509,114.308448373286,
114.406705784207,114.50507127457,114.60349801372,114.702086869152,114.747078580599,
114.845676705603,114.944134488379,115.044357056152,115.14263661388,115.240883192953,
115.339126275992,115.440823464634,115.539207878053,115.642561454307,115.745915030561,
115.84988875933,115.953561696348,116.057054365165,116.160309146372,116.238928182547),
 .UNSPECIFIED.);
#1651=B_SPLINE_CURVE_WITH_KNOTS('',3,(#155009,#155010,#155011,#155012,#155013,
#155014),.UNSPECIFIED.,.F.,.F.,(4,1,1,4),(114.012186908316,114.28227184808,
115.281108298042,116.238922797716),.UNSPECIFIED.);
#1652=B_SPLINE_CURVE_WITH_KNOTS('',3,(#155015,#155016,#155017,#155018,#155019,
#155020,#155021,#155022,#155023,#155024,#155025,#155026,#155027,#155028,
#155029,#155030,#155031,#155032,#155033,#155034,#155035,#155036,#155037,
#155038,#155039,#155040,#155041,#155042,#155043,#155044,#155045,#155046,
#155047,#155048,#155049,#155050,#155051,#155052,#155053,#155054,#155055,
#155056,#155057,#155058,#155059,#155060,#155061,#155062,#155063,#155064,
#155065,#155066,#155067,#155068,#155069,#155070,#155071,#155072,#155073,
#155074,#155075,#155076,#155077,#155078,#155079,#155080,#155081,#155082,
#155083,#155084,#155085,#155086,#155087,#155088,#155089,#155090,#155091,
#155092,#155093,#155094,#155095,#155096,#155097,#155098,#155099,#155100,
#155101,#155102,#155103,#155104,#155105,#155106,#155107,#155108,#155109,
#155110,#155111,#155112,#155113,#155114,#155115,#155116,#155117,#155118,
#155119,#155120,#155121,#155122,#155123,#155124,#155125,#155126,#155127,
#155128,#155129,#155130,#155131,#155132,#155133,#155134,#155135,#155136,
#155137,#155138,#155139,#155140,#155141),.UNSPECIFIED.,.F.,.F.,(4,3,3,3,
3,3,3,3,3,3,3,3,3,3,3,3,3,3,3,3,3,3,3,3,3,3,3,3,3,3,3,3,3,3,3,3,3,3,3,3,
3,3,4),(116.238928182823,116.279944748004,116.378542873008,116.477000655784,
116.577223223557,116.675502781285,116.773749360358,116.871992443397,116.973689632039,
117.072074045458,117.175427621712,117.278781197966,117.37737932297,117.475837105746,
117.576059673519,117.674339231247,117.77258581032,117.870828893359,117.972526082001,
118.07091049542,118.174264071673,118.277617647927,118.376215772931,118.474673555707,
118.57489612348,118.673175681208,118.771422260282,118.86966534332,118.971362531962,
119.069746945381,119.173100521635,119.276454097889,119.375052222893,119.47351000567,
119.573732573442,119.67201213117,119.770258710244,119.868501793282,119.970198981924,
120.068583395343,120.171936971597,120.275290547851,120.296396878359),
 .UNSPECIFIED.);
#1653=B_SPLINE_CURVE_WITH_KNOTS('',3,(#155147,#155148,#155149,#155150,#155151,
#155152,#155153,#155154),.UNSPECIFIED.,.F.,.F.,(4,1,1,1,1,4),(122.522113490002,
122.737770180294,123.736606630256,124.735443080218,125.73427953018,126.578666779634),
 .UNSPECIFIED.);
#1654=B_SPLINE_CURVE_WITH_KNOTS('',3,(#155155,#155156,#155157,#155158,#155159,
#155160,#155161,#155162,#155163,#155164,#155165,#155166,#155167,#155168,
#155169,#155170,#155171,#155172,#155173,#155174,#155175,#155176,#155177,
#155178,#155179,#155180,#155181,#155182,#155183,#155184,#155185,#155186,
#155187,#155188,#155189,#155190,#155191,#155192,#155193,#155194,#155195,
#155196,#155197,#155198,#155199,#155200,#155201,#155202,#155203,#155204,
#155205,#155206,#155207,#155208,#155209,#155210,#155211,#155212,#155213,
#155214,#155215,#155216,#155217,#155218,#155219,#155220,#155221,#155222,
#155223,#155224),.UNSPECIFIED.,.F.,.F.,(4,3,3,3,3,3,3,3,3,3,3,3,3,3,3,3,
3,3,3,3,3,3,3,4),(120.296103360098,120.394359113849,120.492722024964,120.591144738723,
120.689731152633,120.740097280371,120.838695405375,120.937153188151,121.037375755924,
121.135655313652,121.233901892726,121.332144975764,121.433842164407,121.532226577825,
121.635580154079,121.738933730333,121.836831200292,121.933909156543,122.030894120917,
122.127817176648,122.226391254986,122.323316910845,122.422715200424,122.522113490002),
 .UNSPECIFIED.);
#1655=B_SPLINE_CURVE_WITH_KNOTS('',3,(#155226,#155227,#155228,#155229,#155230,
#155231,#155232,#155233,#155234,#155235,#155236,#155237,#155238,#155239,
#155240,#155241,#155242,#155243,#155244,#155245,#155246,#155247,#155248,
#155249,#155250,#155251,#155252,#155253,#155254,#155255,#155256,#155257,
#155258,#155259,#155260,#155261,#155262,#155263,#155264,#155265,#155266,
#155267,#155268,#155269,#155270,#155271,#155272,#155273,#155274,#155275,
#155276,#155277,#155278,#155279,#155280,#155281,#155282,#155283,#155284,
#155285,#155286,#155287,#155288,#155289,#155290,#155291,#155292),
 .UNSPECIFIED.,.F.,.F.,(4,3,3,3,3,3,3,3,3,3,3,3,3,3,3,3,3,3,3,3,3,3,4),
(120.296396878359,120.394962212568,120.493394239118,120.591721801248,120.689992619365,
120.788236205456,120.886482037624,120.984827514811,121.083221502001,121.181792188648,
121.274126997813,121.372725122817,121.471182905593,121.571405473366,121.669685031094,
121.767931610168,121.866174693206,121.967871881848,122.066256295267,122.169609871521,
122.272963447775,122.400857829824,122.522113389936),.UNSPECIFIED.);
#1656=B_SPLINE_CURVE_WITH_KNOTS('',3,(#155293,#155294,#155295,#155296,#155297,
#155298,#155299,#155300),.UNSPECIFIED.,.F.,.F.,(4,1,1,1,1,4),(122.522113490002,
123.271799897737,124.270636347699,125.269472797661,126.268309247622,126.580285712868),
 .UNSPECIFIED.);
#1657=B_SPLINE_CURVE_WITH_KNOTS('',3,(#155306,#155307,#155308,#155309,#155310,
#155311,#155312,#155313,#155314,#155315,#155316,#155317,#155318,#155319,
#155320,#155321,#155322,#155323,#155324,#155325,#155326,#155327,#155328,
#155329,#155330,#155331,#155332,#155333,#155334,#155335,#155336,#155337,
#155338,#155339,#155340,#155341,#155342,#155343,#155344,#155345,#155346,
#155347,#155348,#155349,#155350,#155351,#155352,#155353,#155354,#155355,
#155356,#155357,#155358,#155359,#155360,#155361,#155362,#155363,#155364,
#155365,#155366,#155367,#155368,#155369,#155370,#155371,#155372,#155373,
#155374,#155375,#155376,#155377,#155378,#155379,#155380,#155381,#155382,
#155383,#155384,#155385,#155386,#155387,#155388,#155389,#155390,#155391,
#155392,#155393,#155394,#155395,#155396,#155397,#155398,#155399,#155400,
#155401,#155402,#155403,#155404,#155405,#155406,#155407,#155408,#155409,
#155410,#155411,#155412,#155413,#155414,#155415,#155416,#155417,#155418,
#155419,#155420,#155421,#155422,#155423,#155424,#155425,#155426,#155427,
#155428,#155429,#155430,#155431,#155432),.UNSPECIFIED.,.F.,.F.,(4,3,3,3,
3,3,3,3,3,3,3,3,3,3,3,3,3,3,3,3,3,3,3,3,3,3,3,3,3,3,3,3,3,3,3,3,3,3,3,3,
3,3,4),(128.805298797182,128.902840431273,129.000250613517,129.097560812666,
129.194818343698,129.292053887498,129.389298094495,129.486642967569,129.584044330746,
129.681605924981,129.729625330028,129.828223455032,129.926681237808,130.026903805581,
130.125183363309,130.223429942382,130.321673025421,130.423370214063,130.521754627482,
130.625108203735,130.728461779989,130.827059904993,130.925517687769,131.025740255542,
131.12401981327,131.222266392343,131.320509475382,131.422206664024,131.520591077443,
131.623944653697,131.727298229951,131.825896354955,131.924354137731,132.024576705504,
132.122856263232,132.221102842306,132.319345925344,132.421043113987,132.519427527405,
132.622781103659,132.726134679913,132.824726637228,132.863178333069),
 .UNSPECIFIED.);
#1658=B_SPLINE_CURVE_WITH_KNOTS('',3,(#155433,#155434,#155435,#155436,#155437,
#155438,#155439),.UNSPECIFIED.,.F.,.F.,(4,1,1,1,4),(126.578666779634,126.733115980142,
127.731952430104,128.730788880066,128.805298797182),.UNSPECIFIED.);
#1659=B_SPLINE_CURVE_WITH_KNOTS('',3,(#155441,#155442,#155443,#155444,#155445,
#155446),.UNSPECIFIED.,.F.,.F.,(4,1,1,4),(126.580285712868,127.267145697584,
128.265982147546,128.805298797182),.UNSPECIFIED.);
#1660=B_SPLINE_CURVE_WITH_KNOTS('',3,(#155447,#155448,#155449,#155450,#155451,
#155452,#155453,#155454,#155455,#155456,#155457,#155458,#155459,#155460,
#155461,#155462,#155463,#155464,#155465,#155466,#155467,#155468,#155469,
#155470,#155471,#155472,#155473,#155474,#155475,#155476,#155477,#155478,
#155479,#155480,#155481,#155482,#155483,#155484,#155485,#155486,#155487,
#155488,#155489,#155490,#155491,#155492,#155493,#155494,#155495,#155496,
#155497,#155498,#155499,#155500,#155501,#155502,#155503,#155504,#155505,
#155506,#155507,#155508,#155509,#155510,#155511,#155512,#155513,#155514,
#155515,#155516,#155517,#155518,#155519,#155520,#155521,#155522,#155523,
#155524,#155525,#155526,#155527,#155528,#155529,#155530,#155531,#155532,
#155533,#155534,#155535,#155536,#155537,#155538,#155539,#155540,#155541,
#155542,#155543,#155544,#155545,#155546,#155547,#155548,#155549,#155550,
#155551,#155552,#155553,#155554,#155555,#155556,#155557,#155558,#155559,
#155560,#155561,#155562,#155563,#155564,#155565,#155566,#155567,#155568,
#155569,#155570),.UNSPECIFIED.,.F.,.F.,(4,3,3,3,3,3,3,3,3,3,3,3,3,3,3,3,
3,3,3,3,3,3,3,3,3,3,3,3,3,3,3,3,3,3,3,3,3,3,3,3,3,4),(128.805299011168,
128.910085619878,129.015255759158,129.12063010964,129.226318351055,129.264818597508,
129.363416722512,129.461874505288,129.562097073061,129.660376630789,129.758623209863,
129.856866292901,129.958563481543,130.056947894962,130.160301471216,130.26365504747,
130.362253172474,130.46071095525,130.560933523023,130.659213080751,130.757459659825,
130.855702742863,130.957399931505,131.055784344924,131.159137921178,131.262491497432,
131.361089622436,131.459547405213,131.559769972985,131.658049530713,131.756296109787,
131.854539192826,131.956236381468,132.054620794887,132.15797437114,132.261327947394,
132.359913784705,132.458366887944,132.559360477805,132.657635681036,132.759988464213,
132.86234124739),.UNSPECIFIED.);
#1661=B_SPLINE_CURVE_WITH_KNOTS('',3,(#155576,#155577,#155578,#155579,#155580,
#155581,#155582,#155583,#155584,#155585,#155586,#155587,#155588,#155589,
#155590,#155591,#155592,#155593,#155594,#155595,#155596,#155597,#155598,
#155599,#155600,#155601,#155602,#155603,#155604,#155605,#155606,#155607,
#155608,#155609,#155610,#155611,#155612,#155613,#155614,#155615,#155616,
#155617,#155618,#155619,#155620,#155621,#155622,#155623,#155624,#155625,
#155626,#155627,#155628,#155629,#155630,#155631,#155632,#155633,#155634,
#155635,#155636,#155637,#155638,#155639,#155640,#155641,#155642,#155643,
#155644,#155645,#155646,#155647,#155648,#155649,#155650,#155651,#155652,
#155653,#155654,#155655,#155656,#155657,#155658,#155659,#155660,#155661,
#155662,#155663,#155664,#155665,#155666,#155667,#155668,#155669,#155670,
#155671,#155672,#155673,#155674,#155675,#155676,#155677,#155678,#155679,
#155680,#155681,#155682,#155683,#155684,#155685,#155686,#155687,#155688,
#155689,#155690,#155691,#155692,#155693,#155694,#155695,#155696,#155697,
#155698,#155699,#155700,#155701,#155702),.UNSPECIFIED.,.F.,.F.,(4,3,3,3,
3,3,3,3,3,3,3,3,3,3,3,3,3,3,3,3,3,3,3,3,3,3,3,3,3,3,3,3,3,3,3,3,3,3,3,3,
3,3,4),(135.088484104361,135.187254556185,135.286029876603,135.384838499173,
135.483776463585,135.582788468007,135.681976179005,135.722644029799,135.821242154803,
135.91969993758,136.019922505352,136.11820206308,136.216448642154,136.314691725192,
136.416388913834,136.514773327253,136.618126903507,136.721480479761,136.820078604765,
136.918536387541,137.018758955314,137.117038513042,137.215285092116,137.313528175154,
137.415225363796,137.513609777215,137.616963353469,137.720316929723,137.818915054727,
137.917372837503,138.017595405276,138.115874963004,138.214121542077,138.312364625116,
138.414061813758,138.512446227176,138.61579980343,138.719153379684,138.8177616025,
138.916204188052,139.014551352321,139.112826031228,139.146050573222),
 .UNSPECIFIED.);
#1662=B_SPLINE_CURVE_WITH_KNOTS('',3,(#155703,#155704,#155705,#155706,#155707,
#155708,#155709,#155710,#155711,#155712,#155713,#155714,#155715,#155716,
#155717,#155718,#155719,#155720,#155721,#155722,#155723,#155724,#155725,
#155726,#155727,#155728,#155729,#155730,#155731,#155732,#155733,#155734,
#155735,#155736,#155737,#155738,#155739,#155740,#155741,#155742,#155743,
#155744,#155745,#155746,#155747,#155748,#155749,#155750,#155751,#155752,
#155753,#155754,#155755,#155756,#155757,#155758,#155759,#155760,#155761,
#155762,#155763,#155764,#155765,#155766,#155767,#155768,#155769,#155770,
#155771,#155772),.UNSPECIFIED.,.F.,.F.,(4,3,3,3,3,3,3,3,3,3,3,3,3,3,3,3,
3,3,3,3,3,3,3,4),(132.863178333069,132.961590250635,133.059905656005,133.158169527358,
133.256411368768,133.354660655115,133.453012760686,133.551418046858,133.649994520245,
133.724971129875,133.823569254879,133.922027037655,134.022249605428,134.120529163156,
134.218775742229,134.317018825268,134.41871601391,134.517100427329,134.620454003583,
134.723807579837,134.836338520701,134.948409000642,135.059693750752,135.088484104126),
 .UNSPECIFIED.);
#1663=B_SPLINE_CURVE_WITH_KNOTS('',3,(#155774,#155775,#155776,#155777,#155778,
#155779,#155780,#155781,#155782,#155783,#155784,#155785,#155786,#155787,
#155788,#155789,#155790,#155791,#155792,#155793,#155794,#155795,#155796,
#155797,#155798,#155799,#155800,#155801,#155802,#155803,#155804,#155805,
#155806,#155807,#155808,#155809,#155810,#155811,#155812,#155813,#155814,
#155815,#155816,#155817,#155818,#155819,#155820,#155821,#155822,#155823,
#155824,#155825,#155826,#155827,#155828,#155829,#155830,#155831,#155832,
#155833,#155834,#155835,#155836,#155837,#155838,#155839,#155840,#155841,
#155842,#155843),.UNSPECIFIED.,.F.,.F.,(4,3,3,3,3,3,3,3,3,3,3,3,3,3,3,3,
3,3,3,3,3,3,3,4),(132.86234124739,132.961797034881,133.060185441341,133.160174919349,
133.260164397356,133.35876252236,133.457220305136,133.557442872909,133.655722430637,
133.75396900971,133.852212092749,133.953909281391,134.05229369481,134.155647271063,
134.259000847317,134.356128675186,134.453094160804,134.549968416923,134.646782617699,
134.743567858738,134.84039997176,134.937256811786,135.034231214225,135.088484104361),
 .UNSPECIFIED.);
#1664=B_SPLINE_CURVE_WITH_KNOTS('',3,(#155844,#155845,#155846,#155847,#155848,
#155849,#155850,#155851),.UNSPECIFIED.,.F.,.F.,(4,1,1,1,1,4),(135.088484104361,
135.257837297279,136.256673747241,137.255510197203,138.254346647165,139.145213350467),
 .UNSPECIFIED.);
#1665=B_SPLINE_CURVE_WITH_KNOTS('',3,(#155857,#155858,#155859,#155860,#155861,
#155862,#155863,#155864,#155865,#155866,#155867,#155868,#155869,#155870,
#155871,#155872,#155873,#155874,#155875,#155876,#155877,#155878,#155879,
#155880,#155881,#155882,#155883,#155884,#155885,#155886,#155887,#155888,
#155889,#155890,#155891,#155892,#155893,#155894,#155895,#155896,#155897,
#155898,#155899,#155900,#155901,#155902,#155903,#155904,#155905,#155906,
#155907,#155908,#155909,#155910,#155911,#155912,#155913,#155914,#155915,
#155916,#155917,#155918,#155919,#155920,#155921,#155922,#155923,#155924,
#155925,#155926,#155927,#155928,#155929,#155930,#155931,#155932,#155933,
#155934,#155935,#155936,#155937,#155938,#155939,#155940,#155941,#155942,
#155943,#155944,#155945,#155946,#155947,#155948,#155949,#155950,#155951,
#155952,#155953,#155954,#155955,#155956,#155957,#155958,#155959,#155960,
#155961,#155962,#155963,#155964,#155965,#155966,#155967,#155968,#155969,
#155970,#155971,#155972,#155973,#155974,#155975,#155976,#155977,#155978,
#155979,#155980),.UNSPECIFIED.,.F.,.F.,(4,3,3,3,3,3,3,3,3,3,3,3,3,3,3,3,
3,3,3,3,3,3,3,3,3,3,3,3,3,3,3,3,3,3,3,3,3,3,3,3,3,4),(141.371669411768,
141.485016004535,141.600339367052,141.71566272957,141.814260854574,141.912718637351,
142.012941205123,142.111220762851,142.209467341925,142.307710424963,142.409407613606,
142.507792027024,142.611145603278,142.714499179532,142.813097304536,142.911555087312,
143.011777655085,143.110057212813,143.208303791887,143.306546874925,143.408244063567,
143.506628476986,143.60998205324,143.713335629494,143.811933754498,143.910391537274,
144.010614105047,144.108893662775,144.207140241849,144.305383324887,144.40708051353,
144.505464926948,144.608818503202,144.712172079456,144.810746601835,144.909191401425,
145.007536191867,145.105810582005,145.204060790384,145.302298022107,145.400579631044,
145.428467292648),.UNSPECIFIED.);
#1666=B_SPLINE_CURVE_WITH_KNOTS('',3,(#155981,#155982,#155983,#155984,#155985,
#155986,#155987,#155988,#155989,#155990,#155991,#155992,#155993,#155994,
#155995,#155996,#155997,#155998,#155999,#156000,#156001,#156002,#156003,
#156004,#156005,#156006,#156007,#156008,#156009,#156010,#156011,#156012,
#156013,#156014,#156015,#156016,#156017,#156018,#156019,#156020,#156021,
#156022,#156023,#156024,#156025,#156026,#156027,#156028,#156029,#156030,
#156031,#156032,#156033,#156034,#156035,#156036,#156037,#156038,#156039,
#156040,#156041,#156042,#156043,#156044,#156045,#156046,#156047,#156048,
#156049,#156050),.UNSPECIFIED.,.F.,.F.,(4,3,3,3,3,3,3,3,3,3,3,3,3,3,3,3,
3,3,3,3,3,3,3,4),(139.146050573222,139.244292836133,139.342541002963,139.440891057939,
139.539292908966,139.637867561271,139.717989829646,139.81658795465,139.915045737426,
140.015268305199,140.113547862927,140.211794442001,140.31003752504,140.411734713682,
140.510119127101,140.613472703354,140.716826279608,140.815569227393,140.914173010821,
141.012667061739,141.111081830931,141.209449097701,141.307822396311,141.371669411541),
 .UNSPECIFIED.);
#1667=B_SPLINE_CURVE_WITH_KNOTS('',3,(#156052,#156053,#156054,#156055,#156056,
#156057,#156058),.UNSPECIFIED.,.F.,.F.,(4,1,1,1,4),(139.145213350467,139.253183097127,
140.252019547089,141.250855997051,141.371669411541),.UNSPECIFIED.);
#1668=B_SPLINE_CURVE_WITH_KNOTS('',3,(#156059,#156060,#156061,#156062,#156063,
#156064,#156065,#156066,#156067,#156068,#156069,#156070,#156071,#156072,
#156073,#156074,#156075,#156076,#156077,#156078,#156079,#156080,#156081,
#156082,#156083,#156084,#156085,#156086,#156087,#156088,#156089,#156090,
#156091,#156092,#156093,#156094,#156095,#156096,#156097,#156098,#156099,
#156100,#156101,#156102,#156103,#156104,#156105,#156106,#156107,#156108,
#156109,#156110,#156111,#156112,#156113,#156114,#156115,#156116,#156117,
#156118,#156119,#156120,#156121,#156122,#156123,#156124,#156125,#156126,
#156127,#156128,#156129,#156130,#156131,#156132,#156133,#156134,#156135,
#156136,#156137,#156138,#156139,#156140,#156141,#156142,#156143,#156144,
#156145,#156146,#156147,#156148,#156149,#156150,#156151,#156152,#156153,
#156154,#156155,#156156,#156157,#156158,#156159,#156160,#156161,#156162,
#156163,#156164,#156165,#156166,#156167,#156168,#156169,#156170,#156171,
#156172,#156173,#156174,#156175,#156176,#156177,#156178,#156179,#156180,
#156181,#156182),.UNSPECIFIED.,.F.,.F.,(4,3,3,3,3,3,3,3,3,3,3,3,3,3,3,3,
3,3,3,3,3,3,3,3,3,3,3,3,3,3,3,3,3,3,3,3,3,3,3,3,3,4),(141.371669411541,
141.46883125416,141.566438903267,141.66339620349,141.760311911022,141.857216996242,
141.955335858935,142.052368429038,142.151030438025,142.249692447012,142.348290572016,
142.446748354793,142.546970922565,142.645250480293,142.743497059367,142.841740142405,
142.943437331048,143.041821744466,143.14517532072,143.248528896974,143.347127021978,
143.445584804754,143.545807372527,143.644086930255,143.742333509329,143.840576592367,
143.94227378101,144.040658194428,144.144011770682,144.247365346936,144.34596347194,
144.444421254716,144.544643822489,144.642923380217,144.741169959291,144.839413042329,
144.941110230971,145.03949464439,145.142848220644,145.246201796898,145.344774861169,
145.429604638483),.UNSPECIFIED.);
#1669=B_SPLINE_CURVE_WITH_KNOTS('',3,(#156188,#156189,#156190,#156191,#156192,
#156193,#156194,#156195,#156196),.UNSPECIFIED.,.F.,.F.,(4,1,1,1,1,1,4),
(147.65485471872,147.708681429341,148.707517879303,149.706354329265,150.705190779227,
151.704027229189,151.71225272303),.UNSPECIFIED.);
#1670=B_SPLINE_CURVE_WITH_KNOTS('',3,(#156197,#156198,#156199,#156200,#156201,
#156202,#156203,#156204,#156205,#156206,#156207,#156208,#156209,#156210,
#156211,#156212,#156213,#156214,#156215,#156216,#156217,#156218,#156219,
#156220,#156221,#156222,#156223,#156224,#156225,#156226,#156227,#156228,
#156229,#156230,#156231,#156232,#156233,#156234,#156235,#156236,#156237,
#156238,#156239,#156240,#156241,#156242,#156243,#156244,#156245,#156246,
#156247,#156248,#156249,#156250,#156251,#156252,#156253,#156254,#156255,
#156256,#156257,#156258,#156259,#156260,#156261,#156262,#156263,#156264,
#156265,#156266),.UNSPECIFIED.,.F.,.F.,(4,3,3,3,3,3,3,3,3,3,3,3,3,3,3,3,
3,3,3,3,3,3,3,4),(145.428467292648,145.52686558547,145.625438406774,145.711008529418,
145.809606654422,145.908064437198,146.008287004971,146.106566562699,146.204813141772,
146.303056224811,146.404753413453,146.503137826872,146.606491403125,146.709844979379,
146.807643480436,146.905302408374,147.002849316603,147.100335701354,147.197792033696,
147.295248746519,147.3927980835,147.490396206244,147.588155506493,147.65485471872),
 .UNSPECIFIED.);
#1671=B_SPLINE_CURVE_WITH_KNOTS('',3,(#156268,#156269,#156270,#156271,#156272,
#156273,#156274,#156275,#156276,#156277,#156278,#156279,#156280,#156281,
#156282,#156283,#156284,#156285,#156286,#156287,#156288,#156289,#156290,
#156291,#156292,#156293,#156294,#156295,#156296,#156297,#156298,#156299,
#156300,#156301,#156302,#156303,#156304,#156305,#156306,#156307,#156308,
#156309,#156310,#156311,#156312,#156313,#156314,#156315,#156316,#156317,
#156318,#156319,#156320,#156321,#156322,#156323,#156324,#156325,#156326,
#156327,#156328,#156329,#156330,#156331,#156332,#156333,#156334,#156335,
#156336,#156337),.UNSPECIFIED.,.F.,.F.,(4,3,3,3,3,3,3,3,3,3,3,3,3,3,3,3,
3,3,3,3,3,3,3,4),(145.429604638483,145.53153383953,145.629819415388,145.728068427782,
145.826310362661,145.924574690241,146.022950440083,146.121392805655,146.219991569703,
146.24503824686,146.343636371864,146.44209415464,146.542316722413,146.640596280141,
146.738842859215,146.837085942253,146.938783130895,147.037167544314,147.140521120568,
147.243874696822,147.352569174392,147.460952550046,147.568802109382,147.654854305383),
 .UNSPECIFIED.);
#1672=B_SPLINE_CURVE_WITH_KNOTS('',3,(#156338,#156339,#156340,#156341,#156342,
#156343,#156344,#156345),.UNSPECIFIED.,.F.,.F.,(4,1,1,1,1,4),(147.65485471872,
148.242711146784,149.241547596746,150.240384046707,151.239220496669,151.712342645016),
 .UNSPECIFIED.);
#1673=B_SPLINE_CURVE_WITH_KNOTS('',3,(#156351,#156352,#156353,#156354,#156355,
#156356,#156357,#156358,#156359,#156360,#156361,#156362,#156363,#156364,
#156365,#156366,#156367,#156368,#156369,#156370,#156371,#156372,#156373,
#156374,#156375,#156376,#156377,#156378,#156379,#156380,#156381,#156382,
#156383,#156384,#156385,#156386,#156387,#156388,#156389,#156390,#156391,
#156392,#156393,#156394,#156395,#156396,#156397,#156398,#156399,#156400,
#156401,#156402,#156403,#156404,#156405,#156406,#156407,#156408,#156409,
#156410,#156411,#156412,#156413,#156414,#156415,#156416,#156417,#156418,
#156419,#156420,#156421,#156422,#156423,#156424,#156425,#156426,#156427,
#156428,#156429,#156430,#156431,#156432,#156433,#156434,#156435,#156436,
#156437,#156438,#156439,#156440,#156441,#156442,#156443,#156444,#156445,
#156446,#156447,#156448,#156449,#156450,#156451,#156452,#156453,#156454,
#156455,#156456,#156457,#156458,#156459,#156460,#156461,#156462,#156463,
#156464,#156465,#156466,#156467,#156468,#156469,#156470,#156471,#156472,
#156473,#156474),.UNSPECIFIED.,.F.,.F.,(4,3,3,3,3,3,3,3,3,3,3,3,3,3,3,3,
3,3,3,3,3,3,3,3,3,3,3,3,3,3,3,3,3,3,3,3,3,3,3,3,3,4),(153.9380400259,154.035163898234,
154.132222574362,154.229246955324,154.326267897773,154.423381488606,154.520541056366,
154.617870832504,154.700536579074,154.799134704076,154.897592486852,154.997815054625,
155.096094612352,155.194341191424,155.292584274461,155.394281463105,155.492665876523,
155.596019452779,155.699373029036,155.797971154037,155.896428936811,155.996651504585,
156.09493106231,156.193177641381,156.291420724417,156.393117913062,156.491502326478,
156.594855902738,156.698209478998,156.796807604012,156.895265386799,156.995487954569,
157.093767512308,157.192014091391,157.29025717444,157.39195436307,157.490338776499,
157.593692352729,157.69704592896,157.795632129861,157.89577059138,157.995909052899),
 .UNSPECIFIED.);
#1674=B_SPLINE_CURVE_WITH_KNOTS('',3,(#156475,#156476,#156477,#156478,#156479,
#156480),.UNSPECIFIED.,.F.,.F.,(4,1,1,4),(151.71225272303,152.702863679151,
153.701700129113,153.938039726484),.UNSPECIFIED.);
#1675=B_SPLINE_CURVE_WITH_KNOTS('',3,(#156482,#156483,#156484,#156485,#156486,
#156487),.UNSPECIFIED.,.F.,.F.,(4,1,1,4),(151.712342645016,152.238056946631,
153.236893396593,153.9380400259),.UNSPECIFIED.);
#1676=B_SPLINE_CURVE_WITH_KNOTS('',3,(#156488,#156489,#156490,#156491,#156492,
#156493,#156494,#156495,#156496,#156497,#156498,#156499,#156500,#156501,
#156502,#156503,#156504,#156505,#156506,#156507,#156508,#156509,#156510,
#156511,#156512,#156513,#156514,#156515,#156516,#156517,#156518,#156519,
#156520,#156521,#156522,#156523,#156524,#156525,#156526,#156527,#156528,
#156529,#156530,#156531,#156532,#156533,#156534,#156535,#156536,#156537,
#156538,#156539,#156540,#156541,#156542,#156543,#156544,#156545,#156546,
#156547,#156548,#156549,#156550,#156551,#156552,#156553,#156554,#156555,
#156556,#156557,#156558,#156559,#156560,#156561,#156562,#156563,#156564,
#156565,#156566,#156567,#156568,#156569,#156570,#156571,#156572,#156573,
#156574,#156575,#156576,#156577,#156578,#156579,#156580,#156581,#156582,
#156583,#156584,#156585,#156586,#156587,#156588,#156589,#156590,#156591,
#156592,#156593,#156594,#156595,#156596,#156597,#156598,#156599,#156600,
#156601,#156602,#156603,#156604,#156605,#156606,#156607,#156608,#156609,
#156610,#156611),.UNSPECIFIED.,.F.,.F.,(4,3,3,3,3,3,3,3,3,3,3,3,3,3,3,3,
3,3,3,3,3,3,3,3,3,3,3,3,3,3,3,3,3,3,3,3,3,3,3,3,3,4),(153.938040202782,
154.056659980249,154.176963651006,154.235729846555,154.334327971559,154.432785754335,
154.533008322108,154.631287879836,154.729534458909,154.827777541948,154.92947473059,
155.027859144009,155.131212720263,155.234566296517,155.33316442152,155.431622204297,
155.531844772069,155.630124329797,155.72837090887,155.826613991908,155.928311180551,
156.026695593969,156.130049170224,156.233402746479,156.332000871484,156.430458654262,
156.530681222035,156.628960779764,156.727207358839,156.825450441879,156.927147630519,
157.02553204394,157.12888562019,157.232239196441,157.330809964386,157.429252216966,
157.527595662276,157.625869905311,157.724128943529,157.822375482199,157.920688283555,
157.994793997602),.UNSPECIFIED.);
#1677=B_SPLINE_CURVE_WITH_KNOTS('',3,(#156617,#156618,#156619,#156620,#156621,
#156622,#156623,#156624),.UNSPECIFIED.,.F.,.F.,(4,1,1,1,1,4),(160.221227414851,
160.693555278846,161.692391728808,162.691228178769,163.690064628731,164.278110045036),
 .UNSPECIFIED.);
#1678=B_SPLINE_CURVE_WITH_KNOTS('',3,(#156625,#156626,#156627,#156628,#156629,
#156630,#156631,#156632,#156633,#156634,#156635,#156636,#156637,#156638,
#156639,#156640,#156641,#156642,#156643,#156644,#156645,#156646,#156647,
#156648,#156649,#156650,#156651,#156652,#156653,#156654,#156655,#156656,
#156657,#156658,#156659,#156660,#156661,#156662,#156663,#156664,#156665,
#156666,#156667,#156668,#156669,#156670,#156671,#156672,#156673,#156674,
#156675,#156676,#156677,#156678,#156679,#156680,#156681,#156682,#156683,
#156684,#156685,#156686,#156687,#156688,#156689,#156690,#156691,#156692,
#156693,#156694),.UNSPECIFIED.,.F.,.F.,(4,3,3,3,3,3,3,3,3,3,3,3,3,3,3,3,
3,3,3,3,3,3,3,4),(157.995909052899,158.094187845048,158.192434134029,158.290677402052,
158.39197864627,158.490363756051,158.593123067487,158.695882378922,158.794480503912,
158.892938286674,158.993160854451,159.091440412165,159.189686991223,159.287930074248,
159.389627262907,159.488011676311,159.591365252598,159.694718828884,159.797216560019,
159.903218753284,160.005303397592,160.107256278838,160.209067828957,160.22122533308),
 .UNSPECIFIED.);
#1679=B_SPLINE_CURVE_WITH_KNOTS('',3,(#156696,#156697,#156698,#156699,#156700,
#156701,#156702,#156703,#156704,#156705,#156706,#156707,#156708,#156709,
#156710,#156711,#156712,#156713,#156714,#156715,#156716,#156717,#156718,
#156719,#156720,#156721,#156722,#156723,#156724,#156725,#156726,#156727,
#156728,#156729,#156730,#156731,#156732,#156733,#156734,#156735,#156736,
#156737,#156738,#156739,#156740,#156741,#156742,#156743,#156744,#156745,
#156746,#156747,#156748,#156749,#156750,#156751,#156752,#156753,#156754,
#156755,#156756,#156757,#156758,#156759,#156760,#156761,#156762,#156763,
#156764,#156765),.UNSPECIFIED.,.F.,.F.,(4,3,3,3,3,3,3,3,3,3,3,3,3,3,3,3,
3,3,3,3,3,3,3,4),(157.994793997602,158.093225117261,158.191816683924,158.231075646402,
158.329673771403,158.428131554177,158.52835412195,158.626633679676,158.724880258747,
158.823123341782,158.924820530428,159.023204943844,159.126558520104,159.229912096364,
159.328378576654,159.426704810661,159.526019875932,159.624169149678,159.722285836342,
159.820399593048,159.920606027993,160.018861091251,160.120043212039,160.221225332828),
 .UNSPECIFIED.);
#1680=B_SPLINE_CURVE_WITH_KNOTS('',3,(#156766,#156767,#156768,#156769,#156770,
#156771,#156772,#156773,#156774,#156775,#156776,#156777,#156778,#156779,
#156780,#156781,#156782,#156783,#156784,#156785,#156786,#156787,#156788,
#156789,#156790,#156791,#156792,#156793,#156794,#156795,#156796,#156797,
#156798,#156799,#156800,#156801,#156802,#156803,#156804,#156805,#156806,
#156807,#156808,#156809,#156810,#156811,#156812,#156813,#156814,#156815,
#156816,#156817,#156818,#156819,#156820,#156821,#156822,#156823,#156824,
#156825,#156826,#156827,#156828,#156829,#156830,#156831,#156832,#156833,
#156834,#156835,#156836,#156837,#156838,#156839,#156840,#156841,#156842,
#156843,#156844,#156845,#156846,#156847,#156848,#156849,#156850,#156851,
#156852,#156853,#156854,#156855,#156856,#156857,#156858,#156859,#156860,
#156861,#156862,#156863,#156864,#156865,#156866,#156867,#156868,#156869,
#156870,#156871,#156872,#156873,#156874,#156875,#156876,#156877,#156878,
#156879,#156880,#156881,#156882,#156883,#156884,#156885,#156886,#156887,
#156888,#156889,#156890,#156891,#156892),.UNSPECIFIED.,.F.,.F.,(4,3,3,3,
3,3,3,3,3,3,3,3,3,3,3,3,3,3,3,3,3,3,3,3,3,3,3,3,3,3,3,3,3,3,3,3,3,3,3,3,
3,3,4),(160.22122533308,160.228748546326,160.327346671318,160.425804454083,
160.526027021859,160.624306579575,160.722553158637,160.820796241664,160.92249343032,
161.020877843728,161.124231420008,161.227584996288,161.326183121278,161.424640904041,
161.524863471817,161.623143029531,161.72138960859,161.819632691614,161.921329880273,
162.019714293677,162.123067869964,162.22642144625,162.325019571326,162.423477354176,
162.52369992193,162.621979479731,162.720226058877,162.818469141987,162.920166330544,
163.018550744033,163.121904320123,163.225257896212,163.323856021116,163.422313803792,
163.52253637159,163.62081592922,163.719062508196,163.817305591137,163.919002779896,
164.017387193222,164.120740769698,164.224094346174,164.278857710125),
 .UNSPECIFIED.);
#1681=B_SPLINE_CURVE_WITH_KNOTS('',3,(#156898,#156899,#156900,#156901,#156902,
#156903,#156904,#156905,#156906,#156907,#156908,#156909,#156910,#156911,
#156912,#156913,#156914,#156915,#156916,#156917,#156918,#156919,#156920,
#156921,#156922,#156923,#156924,#156925,#156926,#156927,#156928,#156929,
#156930,#156931,#156932,#156933,#156934,#156935,#156936,#156937,#156938,
#156939,#156940,#156941,#156942,#156943,#156944,#156945,#156946,#156947,
#156948,#156949,#156950,#156951,#156952,#156953,#156954,#156955,#156956,
#156957,#156958,#156959,#156960,#156961,#156962,#156963,#156964,#156965,
#156966,#156967,#156968,#156969,#156970,#156971,#156972,#156973,#156974,
#156975,#156976,#156977,#156978,#156979,#156980,#156981,#156982,#156983,
#156984,#156985,#156986,#156987,#156988,#156989,#156990,#156991,#156992,
#156993,#156994,#156995,#156996,#156997,#156998,#156999,#157000,#157001,
#157002,#157003,#157004,#157005,#157006,#157007,#157008,#157009,#157010,
#157011,#157012,#157013,#157014,#157015,#157016,#157017,#157018,#157019,
#157020,#157021),.UNSPECIFIED.,.F.,.F.,(4,3,3,3,3,3,3,3,3,3,3,3,3,3,3,3,
3,3,3,3,3,3,3,3,3,3,3,3,3,3,3,3,3,3,3,3,3,3,3,3,3,4),(166.504410640259,
166.65291077017,166.686573978617,166.785172097224,166.883629873609,166.983852442981,
167.082131994377,167.180378567154,167.278621643939,167.380318840099,167.478703247436,
167.582056838008,167.685410428579,167.784008554555,167.882466338245,167.982688905782,
168.080968464275,168.179215044057,168.277458127747,168.379155315446,168.477539729369,
168.580893303955,168.684246878541,168.782845025265,168.881302829864,168.981525392194,
169.079804971833,169.178051572804,169.276294677697,169.377991840398,169.476376275343,
169.579729801923,169.683083328503,169.781689728,169.880127484756,169.978469449952,
170.076745220109,170.174984321157,170.273261950328,170.371554712907,170.469968413916,
170.561255386023),.UNSPECIFIED.);
#1682=B_SPLINE_CURVE_WITH_KNOTS('',3,(#157022,#157023,#157024,#157025,#157026,
#157027),.UNSPECIFIED.,.F.,.F.,(4,1,1,4),(164.278110045036,164.688901078693,
165.687737528655,166.504405683028),.UNSPECIFIED.);
#1683=B_SPLINE_CURVE_WITH_KNOTS('',3,(#157029,#157030,#157031,#157032,#157033,
#157034,#157035,#157036,#157037,#157038,#157039,#157040,#157041,#157042,
#157043,#157044,#157045,#157046,#157047,#157048,#157049,#157050,#157051,
#157052,#157053,#157054,#157055,#157056,#157057,#157058,#157059,#157060,
#157061,#157062,#157063,#157064,#157065,#157066,#157067,#157068,#157069,
#157070,#157071,#157072,#157073,#157074,#157075,#157076,#157077,#157078,
#157079,#157080,#157081,#157082,#157083,#157084,#157085,#157086,#157087,
#157088,#157089,#157090,#157091,#157092,#157093,#157094,#157095,#157096,
#157097,#157098),.UNSPECIFIED.,.F.,.F.,(4,3,3,3,3,3,3,3,3,3,3,3,3,3,3,3,
3,3,3,3,3,3,3,4),(164.278857710125,164.377373851694,164.475767893135,164.574072766376,
164.672330974244,164.770572014167,164.868825358762,164.967184404754,165.065600998296,
165.164183798452,165.222930796136,165.321528921637,165.419986704913,165.520209272561,
165.618488830789,165.71673541036,165.814978493895,165.916675681946,166.015060095852,
166.118413670974,166.221767246097,166.344599874398,166.465474953135,166.504410639987),
 .UNSPECIFIED.);
#1684=B_SPLINE_CURVE_WITH_KNOTS('',3,(#157099,#157100,#157101,#157102,#157103,
#157104,#157105,#157106,#157107,#157108,#157109,#157110,#157111,#157112,
#157113,#157114,#157115,#157116,#157117,#157118,#157119,#157120,#157121,
#157122,#157123,#157124,#157125,#157126,#157127,#157128,#157129,#157130,
#157131,#157132,#157133,#157134,#157135,#157136,#157137,#157138,#157139,
#157140,#157141,#157142,#157143,#157144,#157145,#157146,#157147,#157148,
#157149,#157150,#157151,#157152,#157153,#157154,#157155,#157156,#157157,
#157158,#157159,#157160,#157161,#157162,#157163,#157164,#157165,#157166,
#157167,#157168,#157169,#157170,#157171,#157172,#157173,#157174,#157175,
#157176,#157177,#157178,#157179,#157180,#157181,#157182,#157183,#157184,
#157185,#157186,#157187,#157188,#157189,#157190,#157191,#157192,#157193,
#157194,#157195,#157196,#157197,#157198,#157199,#157200,#157201,#157202,
#157203,#157204,#157205,#157206,#157207,#157208,#157209,#157210,#157211,
#157212,#157213,#157214,#157215,#157216,#157217,#157218,#157219,#157220,
#157221,#157222,#157223,#157224,#157225),.UNSPECIFIED.,.F.,.F.,(4,3,3,3,
3,3,3,3,3,3,3,3,3,3,3,3,3,3,3,3,3,3,3,3,3,3,3,3,3,3,3,3,3,3,3,3,3,3,3,3,
3,3,4),(166.504410640259,166.601913126298,166.699371433805,166.796815990355,
166.894277201717,166.99184617322,167.089478292227,167.187269535427,167.220603696059,
167.319201820913,167.417659603532,167.517882171343,167.616161728894,167.714408307783,
167.81265139063,167.914348579478,168.012732992691,168.116086569356,168.219440146021,
168.318038274359,168.416496060482,168.516718627419,168.614998188501,168.713244770923,
168.811487857301,168.913185041971,169.011569458673,169.114923027328,169.218276595983,
169.316874714587,169.41533249097,169.515555060342,169.613834611735,169.71208118451,
169.810324261293,169.912021457456,170.010405864791,170.113759455368,170.217113045945,
170.315689889892,170.414143809247,170.512486666546,170.562190622809),
 .UNSPECIFIED.);
#1685=B_SPLINE_CURVE_WITH_KNOTS('',3,(#157231,#157232,#157233,#157234,#157235,
#157236,#157237,#157238,#157239,#157240,#157241,#157242,#157243,#157244,
#157245,#157246,#157247,#157248,#157249,#157250,#157251,#157252,#157253,
#157254,#157255,#157256,#157257,#157258,#157259,#157260,#157261,#157262,
#157263,#157264,#157265,#157266,#157267,#157268,#157269,#157270,#157271,
#157272,#157273,#157274,#157275,#157276,#157277,#157278,#157279,#157280,
#157281,#157282,#157283,#157284,#157285,#157286,#157287,#157288,#157289,
#157290,#157291,#157292,#157293,#157294,#157295,#157296,#157297,#157298,
#157299,#157300,#157301,#157302,#157303,#157304,#157305,#157306,#157307,
#157308,#157309,#157310,#157311,#157312,#157313,#157314,#157315,#157316,
#157317,#157318,#157319,#157320,#157321,#157322,#157323,#157324,#157325,
#157326,#157327,#157328,#157329,#157330,#157331,#157332,#157333,#157334,
#157335,#157336,#157337,#157338,#157339,#157340,#157341,#157342,#157343,
#157344,#157345,#157346,#157347,#157348,#157349,#157350,#157351,#157352,
#157353,#157354,#157355,#157356,#157357),.UNSPECIFIED.,.F.,.F.,(4,3,3,3,
3,3,3,3,3,3,3,3,3,3,3,3,3,3,3,3,3,3,3,3,3,3,3,3,3,3,3,3,3,3,3,3,3,3,3,3,
3,3,4),(172.787595947668,172.884841558898,172.98404000508,173.081071837534,
173.178059269357,173.275033213409,173.375882192145,173.472980625916,173.570144969666,
173.667458407301,173.67842912835,173.777027506426,173.875485539767,173.975708044585,
174.073987845019,174.172234663368,174.270477981962,174.372174881049,174.470559518455,
174.573912548384,174.677265578312,174.775864530901,174.874323147236,174.974545507366,
175.072825907183,175.171073329681,175.269317256364,175.371013449341,175.469398698301,
175.572750363288,175.676102028274,175.774697487766,175.873152601892,175.973375836435,
176.07165273689,176.169896668633,176.268137117691,176.369837457827,176.468219297092,
176.571578887664,176.674938478236,176.773518527172,176.845520716454),
 .UNSPECIFIED.);
#1686=B_SPLINE_CURVE_WITH_KNOTS('',3,(#157358,#157359,#157360,#157361,#157362,
#157363,#157364,#157365,#157366,#157367,#157368,#157369,#157370,#157371,
#157372,#157373,#157374,#157375,#157376,#157377,#157378,#157379,#157380,
#157381,#157382,#157383,#157384,#157385,#157386,#157387,#157388,#157389,
#157390,#157391,#157392,#157393,#157394,#157395,#157396,#157397,#157398,
#157399,#157400,#157401,#157402,#157403,#157404,#157405,#157406,#157407,
#157408,#157409,#157410,#157411,#157412,#157413,#157414,#157415,#157416,
#157417,#157418,#157419,#157420,#157421,#157422,#157423,#157424,#157425,
#157426,#157427),.UNSPECIFIED.,.F.,.F.,(4,3,3,3,3,3,3,3,3,3,3,3,3,3,3,3,
3,3,3,3,3,3,3,4),(170.561255386023,170.659855701315,170.681919778464,170.780517924859,
170.878975728637,170.979198291111,171.07747786875,171.175724467288,171.273967569322,
171.375664734098,171.474049165163,171.577402696795,171.680756228426,171.7793544904,
171.877812410935,171.978034944366,172.07631464078,172.174561358581,172.272804580209,
172.374501604754,172.472886155,172.576239416694,172.679592678388,172.787595947439),
 .UNSPECIFIED.);
#1687=B_SPLINE_CURVE_WITH_KNOTS('',3,(#157429,#157430,#157431,#157432,#157433,
#157434,#157435,#157436,#157437,#157438,#157439,#157440,#157441,#157442,
#157443,#157444,#157445,#157446,#157447,#157448,#157449,#157450,#157451,
#157452,#157453,#157454,#157455,#157456,#157457,#157458,#157459,#157460,
#157461,#157462,#157463,#157464,#157465,#157466,#157467,#157468,#157469,
#157470,#157471,#157472,#157473,#157474,#157475,#157476,#157477,#157478,
#157479,#157480,#157481,#157482,#157483,#157484,#157485,#157486,#157487,
#157488,#157489,#157490,#157491,#157492,#157493,#157494,#157495,#157496,
#157497,#157498),.UNSPECIFIED.,.F.,.F.,(4,3,3,3,3,3,3,3,3,3,3,3,3,3,3,3,
3,3,3,3,3,3,3,4),(170.562190622809,170.660450459433,170.758691657909,170.85694369146,
170.955300563434,171.053713662279,171.152294456207,171.215949495907,171.314547642641,
171.413005447249,171.513228009576,171.611507589225,171.709754190205,171.807997295108,
171.909694457798,172.008078892752,172.11143241931,172.214785945869,172.315617765141,
172.416285943305,172.516781875028,172.617176498107,172.717484579422,172.787595947439),
 .UNSPECIFIED.);
#1688=B_SPLINE_CURVE_WITH_KNOTS('',3,(#157499,#157500,#157501,#157502,#157503,
#157504,#157505,#157506),.UNSPECIFIED.,.F.,.F.,(4,1,1,1,1,4),(172.787601414895,
173.21362239583,174.212458845792,175.211295295754,176.210131745716,176.84428202222),
 .UNSPECIFIED.);
#1689=B_SPLINE_CURVE_WITH_KNOTS('',3,(#157512,#157513,#157514,#157515,#157516,
#157517,#157518,#157519),.UNSPECIFIED.,.F.,.F.,(4,1,1,1,1,4),(179.070781254618,
179.671447828121,180.670284278083,181.669120728045,182.667957178007,183.128402505335),
 .UNSPECIFIED.);
#1690=B_SPLINE_CURVE_WITH_KNOTS('',3,(#157520,#157521,#157522,#157523,#157524,
#157525,#157526,#157527,#157528,#157529,#157530,#157531,#157532,#157533,
#157534,#157535,#157536,#157537,#157538,#157539,#157540,#157541,#157542,
#157543,#157544,#157545,#157546,#157547,#157548,#157549,#157550,#157551,
#157552,#157553,#157554,#157555,#157556,#157557,#157558,#157559,#157560,
#157561,#157562,#157563,#157564,#157565,#157566,#157567,#157568,#157569,
#157570,#157571,#157572,#157573,#157574,#157575,#157576,#157577,#157578,
#157579,#157580,#157581,#157582,#157583,#157584,#157585,#157586,#157587,
#157588,#157589),.UNSPECIFIED.,.F.,.F.,(4,3,3,3,3,3,3,3,3,3,3,3,3,3,3,3,
3,3,3,3,3,3,3,4),(176.845520716454,176.949052492922,177.047346541156,177.145600633247,
177.243844255663,177.342106876084,177.440478991019,177.538914666061,177.637509863883,
177.673774928198,177.772377760441,177.870840294725,177.971061680154,178.069346062747,
178.167597483387,178.265845418215,178.367536908201,178.465926148849,178.569268763504,
178.672611378159,178.782250126366,178.891545491967,179.000249383586,179.070781030157),
 .UNSPECIFIED.);
#1691=B_SPLINE_CURVE_WITH_KNOTS('',3,(#157591,#157592,#157593,#157594,#157595,
#157596),.UNSPECIFIED.,.F.,.F.,(4,1,1,4),(176.84428202222,177.208968195678,
178.20780464564,179.070781254618),.UNSPECIFIED.);
#1692=B_SPLINE_CURVE_WITH_KNOTS('',3,(#157597,#157598,#157599,#157600,#157601,
#157602,#157603,#157604),.UNSPECIFIED.,.F.,.F.,(4,1,1,1,1,4),(179.070781254618,
179.206641095602,180.205477545564,181.204313995525,182.203150445487,183.127688252684),
 .UNSPECIFIED.);
#1693=B_SPLINE_CURVE_WITH_KNOTS('',3,(#157610,#157611,#157612,#157613,#157614,
#157615,#157616,#157617,#157618,#157619,#157620,#157621,#157622,#157623,
#157624,#157625),.UNSPECIFIED.,.F.,.F.,(4,2,2,2,2,2,2,4),(-3.36796875566957,
-3.29693602662566,-3.22761043814152,-3.1044360662705,-3.02217397688405,
-2.85177102547367,-2.77989462151021,-2.68789784099922),.UNSPECIFIED.);
#1694=B_SPLINE_CURVE_WITH_KNOTS('',3,(#157631,#157632,#157633,#157634,#157635,
#157636,#157637,#157638,#157639,#157640,#157641,#157642,#157643,#157644,
#157645,#157646,#157647,#157648,#157649,#157650,#157651,#157652,#157653,
#157654,#157655,#157656,#157657,#157658,#157659,#157660,#157661,#157662,
#157663,#157664,#157665,#157666,#157667,#157668,#157669,#157670,#157671,
#157672,#157673,#157674,#157675,#157676,#157677,#157678,#157679,#157680,
#157681,#157682,#157683,#157684),.UNSPECIFIED.,.F.,.F.,(4,2,2,2,2,2,2,2,
2,2,2,2,2,2,2,2,2,2,2,2,2,2,2,2,2,2,4),(-2.68789784099922,-2.65408837964258,
-2.57621411781424,-2.4966237333734,-2.32905307278914,-2.2450929033377,-2.17225677845503,
-2.05508950305336,-1.97375003241058,-1.85231723560798,-1.68441649845486,
-1.51608522360846,-1.44252219577298,-1.30207940119469,-1.21379664641263,
-1.12981832981553,-0.980005758162937,-0.912771512159761,-0.811790608062358,
-0.6822244712479,-0.609196859613438,-0.468499066483631,-0.385607510180293,
-0.301727696250491,-0.150758602094993,-0.0760649568285229,-0.000831943578446319),
 .UNSPECIFIED.);
#1695=B_SPLINE_CURVE_WITH_KNOTS('',3,(#157687,#157688,#157689,#157690,#157691,
#157692,#157693,#157694,#157695,#157696,#157697,#157698,#157699,#157700,
#157701,#157702,#157703,#157704,#157705,#157706,#157707,#157708,#157709,
#157710,#157711,#157712,#157713,#157714,#157715,#157716,#157717,#157718,
#157719,#157720,#157721,#157722,#157723,#157724,#157725,#157726,#157727,
#157728,#157729,#157730,#157731,#157732,#157733,#157734,#157735,#157736,
#157737,#157738),.UNSPECIFIED.,.F.,.F.,(4,2,2,2,2,2,2,2,2,2,2,2,2,2,2,2,
2,2,2,2,2,2,2,2,2,4),(2.08290412127981E-5,0.148616879989859,0.210346499036526,
0.277678159472066,0.445327467469216,0.529291339569611,0.612068174123259,
0.726650632271939,0.806873057478271,0.925431469321915,1.00702977628667,
1.12919268297785,1.21136628889785,1.38178661778949,1.45314215401029,1.57770656729397,
1.65588321631932,1.73550058497634,1.9026016001689,1.98657761141511,2.07050498841144,
2.21332407327658,2.28618427846037,2.41365321730892,2.49217571148828,2.63428973736591),
 .UNSPECIFIED.);
#1696=B_SPLINE_CURVE_WITH_KNOTS('',3,(#157743,#157744,#157745,#157746,#157747,
#157748,#157749,#157750,#157751,#157752,#157753,#157754,#157755,#157756,
#157757,#157758,#157759,#157760,#157761,#157762,#157763,#157764,#157765,
#157766,#157767,#157768,#157769,#157770,#157771,#157772,#157773,#157774,
#157775,#157776,#157777,#157778,#157779,#157780,#157781,#157782,#157783,
#157784,#157785,#157786,#157787,#157788,#157789,#157790,#157791,#157792,
#157793,#157794,#157795,#157796,#157797,#157798,#157799,#157800,#157801,
#157802,#157803,#157804,#157805,#157806,#157807,#157808,#157809,#157810,
#157811,#157812,#157813,#157814,#157815,#157816,#157817,#157818,#157819,
#157820,#157821,#157822,#157823,#157824,#157825,#157826,#157827,#157828,
#157829,#157830,#157831,#157832,#157833,#157834,#157835,#157836,#157837,
#157838,#157839,#157840,#157841,#157842,#157843,#157844,#157845,#157846,
#157847,#157848,#157849,#157850,#157851,#157852,#157853,#157854,#157855,
#157856,#157857,#157858,#157859,#157860,#157861,#157862,#157863,#157864,
#157865,#157866,#157867,#157868,#157869,#157870,#157871,#157872,#157873,
#157874,#157875,#157876,#157877,#157878,#157879,#157880,#157881,#157882,
#157883,#157884,#157885,#157886,#157887,#157888,#157889,#157890,#157891,
#157892,#157893,#157894,#157895,#157896,#157897,#157898,#157899,#157900,
#157901,#157902,#157903,#157904,#157905,#157906,#157907,#157908,#157909,
#157910,#157911,#157912,#157913,#157914,#157915,#157916,#157917,#157918,
#157919,#157920,#157921,#157922,#157923,#157924,#157925,#157926,#157927,
#157928,#157929,#157930,#157931,#157932,#157933,#157934,#157935,#157936,
#157937,#157938,#157939,#157940,#157941,#157942,#157943,#157944,#157945,
#157946,#157947,#157948,#157949,#157950,#157951,#157952,#157953,#157954,
#157955,#157956,#157957,#157958,#157959,#157960,#157961,#157962),
 .UNSPECIFIED.,.F.,.F.,(4,3,3,3,3,3,3,3,3,3,3,3,3,3,3,3,3,3,3,3,3,3,3,3,
3,3,3,3,3,3,3,3,3,3,3,3,3,3,3,3,3,3,3,3,3,3,3,3,3,3,3,3,3,3,3,3,3,3,3,3,
3,3,3,3,3,3,3,3,3,3,3,3,3,4),(-16.4213910178811,-16.3286432460334,-16.2359126775523,
-16.1431937736906,-16.0824674261131,-15.9941326347525,-15.9058201280992,
-15.81748971347,-15.7291508902718,-15.6407545361228,-15.5951199283521,-15.4994686331016,
-15.401544582474,-15.3059685045778,-15.2068704675844,-15.1077724305911,
-15.0193184286812,-14.9308670580831,-14.8423692825813,-14.7538469094734,
-14.6652436972666,-14.6204249328301,-14.5321659959703,-14.4439802741915,
-14.3558480516816,-14.2670832873849,-14.1789810556079,-14.0908703594027,
-14.0027333871464,-13.9134825246869,-13.8251922454331,-13.7354610913706,
-13.6457299373081,-13.5603980691463,-13.4751819518284,-13.3900578392207,
-13.3050021057494,-13.2199819233987,-13.134977242644,-13.0499668163815,
-12.9649293941461,-12.8797915746879,-12.7945965012499,-12.7092654850702,
-12.6710349417861,-12.5825725222911,-12.4942230261398,-12.405966583943,
-12.3172632542332,-12.2291343186378,-12.1410336270666,-12.0529433623445,
-11.9637925083244,-11.8756388741685,-11.7859894102163,-11.6963399462641,
-11.6077342332092,-11.5191955002859,-11.4307068279097,-11.342248612659,
-11.2537923358304,-11.2089924485031,-11.1135915257343,-11.0156048819863,
-10.9199968256523,-10.8208208881972,-10.7216449507421,-10.6332474245461,
-10.5448987428145,-10.4565720082927,-10.3682595889264,-10.2799238818341,
-10.2342974529811,-10.1382057107015),.UNSPECIFIED.);
#1697=B_SPLINE_CURVE_WITH_KNOTS('',3,(#157963,#157964,#157965,#157966,#157967,
#157968,#157969,#157970,#157971,#157972,#157973,#157974,#157975,#157976,
#157977,#157978,#157979,#157980,#157981,#157982,#157983,#157984,#157985,
#157986,#157987,#157988,#157989,#157990,#157991,#157992,#157993,#157994,
#157995,#157996,#157997,#157998,#157999,#158000,#158001,#158002,#158003,
#158004,#158005,#158006,#158007,#158008,#158009,#158010,#158011,#158012,
#158013,#158014,#158015,#158016,#158017,#158018,#158019,#158020,#158021,
#158022,#158023,#158024,#158025,#158026),.UNSPECIFIED.,.F.,.F.,(4,2,2,2,
2,2,2,2,2,2,2,2,2,2,2,2,2,2,2,2,2,2,2,2,2,2,2,2,2,2,2,4),(2.63428973736591,
2.66088030343492,2.74224037341081,2.8234354530902,2.94015318077752,3.00738558007736,
3.13228271568951,3.20336580092265,3.37373005819757,3.45586954025754,3.57847978926214,
3.66000380813647,3.77621516884977,3.85553026353794,3.97452927204004,4.0648220573991,
4.1729444122466,4.24437363486414,4.40914497732687,4.49070881257043,4.62100573148373,
4.68806932974065,4.80426761483173,4.96307722778861,4.99098169170844,5.01472046629936,
5.08915323440459,5.15916500631349,5.18798383976303,5.21418265554997,5.25339267367173,
5.32107893380752),.UNSPECIFIED.);
#1698=B_SPLINE_CURVE_WITH_KNOTS('',3,(#158031,#158032,#158033,#158034,#158035,
#158036,#158037,#158038,#158039,#158040,#158041,#158042,#158043,#158044,
#158045,#158046,#158047,#158048,#158049,#158050,#158051,#158052,#158053,
#158054,#158055,#158056,#158057,#158058,#158059,#158060,#158061,#158062,
#158063,#158064,#158065,#158066,#158067,#158068,#158069,#158070,#158071,
#158072,#158073,#158074,#158075,#158076,#158077,#158078,#158079,#158080,
#158081,#158082,#158083,#158084,#158085,#158086),.UNSPECIFIED.,.F.,.F.,
(4,2,2,2,2,2,2,2,2,2,2,2,2,2,2,2,2,2,2,2,2,2,2,2,2,2,2,4),(1.64869401953039,
1.65982716497674,1.79037275571469,1.89090356673503,1.95818813039972,2.0409203859265,
2.16786929391265,2.30166199712435,2.38022082935311,2.50764971042287,2.58040208492111,
2.72361472000731,2.80826242758488,2.89225516964731,3.05897279728656,3.13861342395075,
3.22546685407399,3.30946904726711,3.4761010374434,3.55574189436597,3.63441392828252,
3.75681848930802,3.82840234120101,3.99886928816814,4.08084321955354,4.19285213499667,
4.26394696517578,4.33610062123442),.UNSPECIFIED.);
#1699=B_SPLINE_CURVE_WITH_KNOTS('',3,(#158087,#158088,#158089,#158090,#158091,
#158092,#158093,#158094,#158095,#158096,#158097,#158098,#158099,#158100,
#158101,#158102,#158103,#158104,#158105,#158106,#158107,#158108,#158109,
#158110,#158111,#158112,#158113,#158114,#158115,#158116,#158117,#158118,
#158119,#158120,#158121,#158122,#158123,#158124,#158125,#158126,#158127,
#158128,#158129,#158130,#158131,#158132,#158133,#158134,#158135,#158136,
#158137,#158138,#158139,#158140,#158141,#158142,#158143,#158144,#158145,
#158146,#158147,#158148,#158149,#158150,#158151,#158152,#158153,#158154,
#158155,#158156,#158157,#158158,#158159,#158160,#158161,#158162,#158163,
#158164,#158165,#158166,#158167,#158168,#158169,#158170,#158171,#158172,
#158173,#158174,#158175,#158176,#158177,#158178,#158179,#158180,#158181,
#158182,#158183,#158184,#158185,#158186,#158187,#158188,#158189,#158190,
#158191,#158192,#158193,#158194,#158195,#158196,#158197,#158198,#158199,
#158200,#158201,#158202,#158203,#158204,#158205,#158206,#158207,#158208,
#158209,#158210,#158211,#158212,#158213,#158214,#158215,#158216,#158217,
#158218,#158219,#158220,#158221,#158222,#158223,#158224,#158225,#158226,
#158227,#158228,#158229,#158230,#158231,#158232,#158233,#158234,#158235,
#158236,#158237,#158238,#158239,#158240,#158241,#158242,#158243,#158244,
#158245,#158246,#158247,#158248,#158249,#158250,#158251,#158252,#158253,
#158254,#158255,#158256,#158257,#158258,#158259,#158260,#158261,#158262,
#158263,#158264,#158265,#158266,#158267,#158268,#158269,#158270,#158271,
#158272,#158273,#158274,#158275,#158276,#158277,#158278,#158279,#158280,
#158281,#158282,#158283,#158284,#158285,#158286,#158287,#158288,#158289,
#158290,#158291,#158292,#158293,#158294,#158295,#158296,#158297,#158298,
#158299,#158300,#158301,#158302,#158303,#158304,#158305,#158306,#158307,
#158308,#158309,#158310,#158311,#158312),.UNSPECIFIED.,.F.,.F.,(4,3,3,3,
3,3,3,3,3,3,3,3,3,3,3,3,3,3,3,3,3,3,3,3,3,3,3,3,3,3,3,3,3,3,3,3,3,3,3,3,
3,3,3,3,3,3,3,3,3,3,3,3,3,3,3,3,3,3,3,3,3,3,3,3,3,3,3,3,3,3,3,3,3,3,3,4),
(7.59153924858055,7.6845224783778,7.77753299194077,7.79755996417604,7.88864771831868,
7.97971760835622,8.07079089443809,8.16186028956199,8.2529495047339,8.28490746193705,
8.37600661966196,8.46708750385086,8.55817107950977,8.64925032934122,8.74034868496834,
8.77225495969805,8.86358446014535,8.95489727790249,9.04621272797726,9.13752315628156,
9.22884970421161,9.25960245745905,9.35004563389331,9.44046838421938,9.53089683726842,
9.62132426183796,9.71178086513476,9.74694995522005,9.83977082466953,9.93258020493847,
10.0253815422507,10.1181658427925,10.2109349487687,10.2342974529811,10.3226340982603,
10.4109484628818,10.4992807310775,10.5876214045936,10.6760195929041,10.7216449507421,
10.8172935625052,10.9152182840046,11.0107916985716,11.1098920735374,11.2089924485031,
11.2974475293379,11.3858999834853,11.4743988429813,11.5629222999095,11.6515265886469,
11.6963399462641,11.7845988436236,11.8727845281299,11.96091671564,12.0496814939083,
12.1377836965724,12.2258943659517,12.3140313137176,12.4032822207347,12.4915724815489,
12.5813037116675,12.6710349417861,12.7563666072233,12.8415825207838,12.9267064287632,
13.0117619568872,13.0967819333776,13.1817864079043,13.2667966276969,13.3518338433476,
13.4369714570383,13.5221663247904,13.6074971372277,13.6457299373081,13.7757706988632,
13.8747245557601),.UNSPECIFIED.);
#1700=B_SPLINE_CURVE_WITH_KNOTS('',3,(#158318,#158319,#158320,#158321,#158322,
#158323,#158324,#158325,#158326,#158327,#158328,#158329,#158330,#158331,
#158332),.UNSPECIFIED.,.F.,.F.,(4,1,1,1,1,1,1,1,1,1,1,1,4),(2.0217817672715,
2.43673748880501,2.92408498656602,3.41143248432702,3.89877998208802,4.38612747984903,
4.87347497761003,5.36082247537103,5.84816997313203,6.33551747089303,6.82286496865404,
7.31021246641504,7.59153924858053),.UNSPECIFIED.);
#1701=B_SPLINE_CURVE_WITH_KNOTS('',3,(#158335,#158336,#158337,#158338,#158339,
#158340,#158341,#158342,#158343,#158344,#158345,#158346,#158347,#158348,
#158349,#158350,#158351,#158352,#158353,#158354,#158355,#158356,#158357,
#158358,#158359,#158360,#158361,#158362,#158363,#158364,#158365,#158366,
#158367,#158368),.UNSPECIFIED.,.F.,.F.,(4,2,2,2,2,2,2,2,2,2,2,2,2,2,2,2,
4),(2.0822795579724E-5,0.091991742256264,0.179274456734732,0.298803049019205,
0.380584217944318,0.503956148693981,0.586127319892338,0.756537131127894,
0.827746482729973,0.952032398654662,1.0317636690925,1.111360273655,1.23017564205823,
1.31025989550073,1.44909386849414,1.58459957318183,1.64862342708563),
 .UNSPECIFIED.);
#1702=B_SPLINE_CURVE_WITH_KNOTS('',3,(#158373,#158374,#158375,#158376,#158377,
#158378,#158379,#158380,#158381,#158382,#158383,#158384,#158385,#158386,
#158387,#158388,#158389,#158390,#158391,#158392,#158393,#158394,#158395,
#158396,#158397,#158398,#158399,#158400,#158401,#158402,#158403,#158404,
#158405,#158406,#158407,#158408,#158409,#158410,#158411,#158412,#158413,
#158414,#158415,#158416,#158417,#158418,#158419,#158420,#158421,#158422,
#158423,#158424,#158425,#158426,#158427,#158428,#158429,#158430,#158431,
#158432,#158433,#158434,#158435,#158436,#158437,#158438,#158439,#158440,
#158441,#158442,#158443,#158444,#158445,#158446,#158447,#158448,#158449,
#158450,#158451,#158452,#158453,#158454,#158455,#158456,#158457,#158458,
#158459,#158460,#158461,#158462,#158463,#158464,#158465,#158466,#158467,
#158468,#158469,#158470,#158471,#158472,#158473,#158474,#158475,#158476,
#158477,#158478,#158479,#158480,#158481,#158482,#158483,#158484,#158485,
#158486,#158487,#158488,#158489,#158490,#158491,#158492,#158493,#158494,
#158495,#158496,#158497,#158498,#158499,#158500,#158501,#158502,#158503,
#158504,#158505,#158506,#158507,#158508,#158509,#158510,#158511,#158512,
#158513,#158514,#158515,#158516,#158517,#158518,#158519,#158520,#158521,
#158522,#158523,#158524,#158525,#158526,#158527,#158528,#158529,#158530,
#158531,#158532,#158533,#158534,#158535,#158536,#158537,#158538,#158539,
#158540,#158541,#158542,#158543,#158544,#158545,#158546,#158547,#158548,
#158549,#158550,#158551,#158552,#158553,#158554,#158555,#158556,#158557,
#158558,#158559,#158560,#158561,#158562,#158563,#158564,#158565,#158566,
#158567,#158568,#158569,#158570,#158571,#158572,#158573,#158574,#158575,
#158576,#158577,#158578,#158579,#158580,#158581,#158582,#158583,#158584,
#158585,#158586,#158587,#158588,#158589,#158590,#158591,#158592,#158593,
#158594,#158595,#158596,#158597,#158598),.UNSPECIFIED.,.F.,.F.,(4,3,3,3,
3,3,3,3,3,3,3,3,3,3,3,3,3,3,3,3,3,3,3,3,3,3,3,3,3,3,3,3,3,3,3,3,3,3,3,3,
3,3,3,3,3,3,3,3,3,3,3,3,3,3,3,3,3,3,3,3,3,3,3,3,3,3,3,3,3,3,3,3,3,3,3,4),
(7.59153924858053,7.68452254538593,7.77753312315871,7.79755996417604,7.88864761488148,
7.97971740157217,8.07079058546456,8.16185987934358,8.25294899549126,8.28490746193705,
8.37600652726715,8.46708731777341,8.55817079881157,8.6492499537383,8.74034821484695,
8.77225495969805,8.86358513560277,8.9548986330717,9.04621476194116,9.1375258664909,
9.22885308111593,9.25960245745905,9.35004385837792,9.44046482582385,9.53089150074111,
9.62131715354628,9.7117720080883,9.74694995522006,9.83977478998513,9.93258815792015,
10.025393459506,10.1181816912061,10.2109546401573,10.2342974529811,10.3226295283866,
10.410939313145,10.4992670123095,10.5876031247876,10.6759967918602,10.7216449507421,
10.8173001765085,10.9152232445072,11.0108032234786,11.1098978359908,11.2089924485031,
11.2974448715171,11.3858946564481,11.4743908456245,11.562911632656,11.6515132694445,
11.6963399462641,11.7845989400825,11.872784715549,11.9609169884106,12.0496817325825,
12.1377840060822,12.22589474066,12.31403174787,12.403282546349,12.4915728517076,
12.5813038967469,12.6710349417861,12.7563671078331,12.8415835245525,12.9267079378408,
13.011763973049,13.0967844578901,13.1817894416759,13.2668001713248,13.3518378971159,
13.4369760189292,13.5221713946028,13.6075027101629,13.6457299373081,13.775760012771,
13.8747245557601),.UNSPECIFIED.);
#1703=B_SPLINE_CURVE_WITH_KNOTS('',3,(#158599,#158600,#158601,#158602,#158603,
#158604,#158605,#158606,#158607,#158608,#158609,#158610,#158611,#158612,
#158613,#158614,#158615,#158616,#158617,#158618,#158619,#158620,#158621,
#158622,#158623,#158624,#158625,#158626,#158627,#158628,#158629,#158630,
#158631,#158632,#158633,#158634,#158635,#158636,#158637,#158638,#158639,
#158640,#158641,#158642,#158643,#158644,#158645,#158646,#158647,#158648,
#158649,#158650,#158651,#158652,#158653,#158654),.UNSPECIFIED.,.F.,.F.,
(4,2,2,2,2,2,2,2,2,2,2,2,2,2,2,2,2,2,2,2,2,2,2,2,2,2,2,4),(1.64862342708563,
1.65975747808592,1.7902957319901,1.89082544682229,1.95810743753247,2.04083689546831,
2.16778132685088,2.3015693448455,2.38012496633507,2.5075505762483,2.58030073732943,
2.72350721335624,2.80814921045046,2.89213912604029,3.05885293405854,3.13849080231745,
3.22533403256793,3.30933341472838,3.47596438146038,3.55560238516295,3.63426033790054,
3.7566778859009,3.82826608880163,3.99872817063951,4.08070038166504,4.19269628700354,
4.26378911976537,4.33594015439032),.UNSPECIFIED.);
#1704=B_SPLINE_CURVE_WITH_KNOTS('',3,(#158659,#158660,#158661,#158662,#158663,
#158664,#158665,#158666,#158667,#158668,#158669,#158670,#158671,#158672,
#158673,#158674,#158675,#158676,#158677,#158678,#158679,#158680,#158681,
#158682,#158683,#158684,#158685,#158686,#158687,#158688,#158689,#158690,
#158691,#158692,#158693,#158694,#158695,#158696,#158697,#158698,#158699,
#158700,#158701,#158702,#158703,#158704,#158705,#158706,#158707,#158708,
#158709,#158710,#158711,#158712,#158713,#158714,#158715,#158716,#158717,
#158718,#158719,#158720,#158721,#158722,#158723,#158724),.UNSPECIFIED.,
 .F.,.F.,(4,2,2,2,2,2,2,2,2,2,2,2,2,2,2,2,2,2,2,2,2,2,2,2,2,2,2,2,2,2,2,
2,4),(2.63429014437239,2.66088071416629,2.74224077834121,2.82343586597364,
2.94015381581752,3.00738688395098,3.13228218594895,3.20336250272686,3.37372653651136,
3.45586556153257,3.57847340338257,3.65999611372759,3.77619619405356,3.85543902504589,
3.97445736545625,4.06450248924364,4.17267568339614,4.24357042392699,4.40856429324298,
4.49003136565494,4.5999968004622,4.66211636333309,4.76327748018164,4.897186414341,
4.97452871563384,4.99842278741062,5.02879770385687,5.11926810911955,5.16652795741294,
5.19356119390082,5.22090478708735,5.26966811136063,5.32075006326628),
 .UNSPECIFIED.);
#1705=B_SPLINE_CURVE_WITH_KNOTS('',3,(#158725,#158726,#158727,#158728,#158729,
#158730,#158731,#158732,#158733,#158734,#158735,#158736,#158737,#158738,
#158739,#158740,#158741,#158742,#158743,#158744,#158745,#158746,#158747,
#158748,#158749,#158750,#158751,#158752,#158753,#158754,#158755,#158756,
#158757,#158758,#158759,#158760,#158761,#158762,#158763,#158764,#158765,
#158766,#158767,#158768,#158769,#158770,#158771,#158772,#158773,#158774,
#158775,#158776,#158777,#158778,#158779,#158780,#158781,#158782,#158783,
#158784,#158785,#158786,#158787,#158788,#158789,#158790,#158791,#158792,
#158793,#158794,#158795,#158796,#158797,#158798,#158799,#158800,#158801,
#158802,#158803,#158804,#158805,#158806,#158807,#158808,#158809,#158810,
#158811,#158812,#158813,#158814,#158815,#158816,#158817,#158818,#158819,
#158820,#158821,#158822,#158823,#158824,#158825,#158826,#158827,#158828,
#158829,#158830,#158831,#158832,#158833,#158834,#158835,#158836,#158837,
#158838,#158839,#158840,#158841,#158842,#158843,#158844,#158845,#158846,
#158847,#158848,#158849,#158850,#158851,#158852,#158853,#158854,#158855,
#158856,#158857,#158858,#158859,#158860,#158861,#158862,#158863,#158864,
#158865,#158866,#158867,#158868,#158869,#158870,#158871,#158872,#158873,
#158874,#158875,#158876,#158877,#158878,#158879,#158880,#158881,#158882,
#158883,#158884,#158885,#158886,#158887,#158888,#158889,#158890,#158891,
#158892,#158893,#158894,#158895,#158896,#158897,#158898,#158899,#158900,
#158901,#158902,#158903,#158904,#158905,#158906,#158907,#158908,#158909,
#158910,#158911,#158912,#158913,#158914,#158915,#158916,#158917,#158918,
#158919,#158920,#158921,#158922,#158923,#158924,#158925,#158926,#158927,
#158928,#158929,#158930,#158931,#158932,#158933,#158934,#158935,#158936,
#158937,#158938,#158939,#158940,#158941,#158942,#158943,#158944),
 .UNSPECIFIED.,.F.,.F.,(4,3,3,3,3,3,3,3,3,3,3,3,3,3,3,3,3,3,3,3,3,3,3,3,
3,3,3,3,3,3,3,3,3,3,3,3,3,3,3,3,3,3,3,3,3,3,3,3,3,3,3,3,3,3,3,3,3,3,3,3,
3,3,3,3,3,3,3,3,3,3,3,3,3,4),(-16.4213910178811,-16.3286400772641,-16.2359063591921,
-16.1431843748859,-16.0824674261131,-15.9941362568266,-15.9058273801709,
-15.8175005869686,-15.7291653788733,-15.6407726083022,-15.5951199283521,
-15.4994633914501,-15.4015406512354,-15.3059593709262,-15.2068659007586,
-15.1077724305911,-15.0193205338912,-14.9308712775328,-14.84237561715,-14.7538553588308,
-14.6652542472042,-14.6204249328301,-14.5321659202474,-14.4439801271102,
-14.3558478376921,-14.2670831001441,-14.1789808129682,-14.0908700658319,
-14.0027330472036,-13.9134822697297,-13.8251919559008,-13.7354609466044,
-13.6457299373081,-13.5603976716426,-13.4751811547976,-13.390056640956,
-13.3050005048409,-13.2199799188415,-13.1349748337167,-13.0499640026098,
-12.9649261753039,-12.8797879523774,-12.7945924756304,-12.7092610599517,
-12.6710349417861,-12.5825724970548,-12.4942229702032,-12.4059664919653,
-12.3172631737526,-12.2291341894402,-12.1410334445326,-12.0529431219476,
-11.9637923280267,-11.8756386254687,-11.7859892858664,-11.6963399462641,
-11.6077363315675,-11.5191997074042,-11.430713147944,-11.3422570464542,
-11.253802873335,-11.2089924485031,-11.1135865925285,-11.0156011820819,
-10.9199878797786,-10.8208164152604,-10.7216449507421,-10.633251005582,
-10.5449059290958,-10.4565828165548,-10.3682740267808,-10.2799419404527,
-10.2342974529811,-10.1382057107015),.UNSPECIFIED.);
#1706=B_SPLINE_CURVE_WITH_KNOTS('',3,(#158951,#158952,#158953,#158954,#158955,
#158956,#158957,#158958,#158959,#158960,#158961,#158962,#158963,#158964,
#158965,#158966,#158967,#158968,#158969,#158970,#158971,#158972,#158973,
#158974,#158975,#158976,#158977,#158978,#158979,#158980,#158981,#158982,
#158983,#158984,#158985,#158986,#158987,#158988,#158989,#158990,#158991,
#158992,#158993,#158994,#158995,#158996,#158997,#158998,#158999,#159000,
#159001,#159002),.UNSPECIFIED.,.F.,.F.,(4,2,2,2,2,2,2,2,2,2,2,2,2,2,2,2,
2,2,2,2,2,2,2,2,2,4),(2.08238338275598E-5,0.148644181152497,0.210319588588462,
0.2776422993658,0.445271649608167,0.529235565856092,0.612053706044955,0.726635154445241,
0.806859868487811,0.92542411935065,1.00702343966239,1.12918939140297,1.21136341657824,
1.38178387358329,1.45314145090535,1.57771255755794,1.65588566918239,1.73550298209199,
1.9026055656601,1.98658157752837,2.07050619976682,2.21332409776297,2.28618452567342,
2.41365385153232,2.49217608938517,2.63429014437239),.UNSPECIFIED.);
#1707=B_SPLINE_CURVE_WITH_KNOTS('',3,(#159003,#159004,#159005,#159006,#159007,
#159008,#159009,#159010,#159011,#159012,#159013,#159014,#159015,#159016,
#159017,#159018,#159019,#159020,#159021,#159022,#159023,#159024,#159025,
#159026,#159027,#159028,#159029,#159030,#159031,#159032,#159033,#159034,
#159035,#159036,#159037,#159038,#159039,#159040,#159041,#159042,#159043,
#159044,#159045,#159046,#159047,#159048,#159049,#159050,#159051,#159052,
#159053,#159054,#159055,#159056),.UNSPECIFIED.,.F.,.F.,(4,2,2,2,2,2,2,2,
2,2,2,2,2,2,2,2,2,2,2,2,2,2,2,2,2,2,4),(-2.68789745416103,-2.65408891563111,
-2.57621233738422,-2.49662198266966,-2.32905050023497,-2.24509032345514,
-2.17225591620052,-2.0550889100482,-1.97374945158346,-1.85231675710463,
-1.68441600725825,-1.51608472119004,-1.44252169241835,-1.30207874924859,
-1.21379570613023,-1.12981739078958,-0.980009160723121,-0.912778914788848,
-0.811762682087948,-0.682239388614031,-0.609249910766953,-0.468421195864385,
-0.38529873131632,-0.301417960888188,-0.150653053921509,-0.0760139026597096,
-0.000831891555311156),.UNSPECIFIED.);
#1708=B_SPLINE_CURVE_WITH_KNOTS('',3,(#159062,#159063,#159064,#159065,#159066,
#159067,#159068,#159069,#159070,#159071),.UNSPECIFIED.,.F.,.F.,(4,3,3,4),
(7.59252172359162,7.7065020665742,7.82442144880896,7.94234083104372),
 .UNSPECIFIED.);
#1709=B_SPLINE_CURVE_WITH_KNOTS('',3,(#159073,#159074,#159075,#159076,#159077,
#159078,#159079,#159080,#159081,#159082,#159083,#159084,#159085,#159086,
#159087,#159088,#159089,#159090,#159091,#159092,#159093,#159094,#159095,
#159096,#159097,#159098,#159099,#159100,#159101,#159102,#159103,#159104,
#159105,#159106,#159107,#159108,#159109,#159110,#159111,#159112,#159113,
#159114,#159115,#159116,#159117,#159118,#159119,#159120,#159121,#159122,
#159123,#159124,#159125,#159126,#159127,#159128,#159129,#159130,#159131,
#159132,#159133,#159134,#159135,#159136,#159137,#159138,#159139,#159140,
#159141,#159142,#159143,#159144,#159145,#159146,#159147,#159148,#159149,
#159150,#159151,#159152,#159153,#159154,#159155,#159156,#159157,#159158,
#159159,#159160,#159161,#159162,#159163,#159164,#159165,#159166,#159167,
#159168,#159169,#159170,#159171,#159172,#159173,#159174,#159175,#159176,
#159177,#159178,#159179,#159180,#159181,#159182,#159183,#159184,#159185,
#159186,#159187,#159188,#159189,#159190,#159191,#159192,#159193,#159194,
#159195,#159196,#159197,#159198,#159199,#159200,#159201,#159202,#159203,
#159204,#159205,#159206,#159207,#159208,#159209,#159210,#159211,#159212,
#159213,#159214,#159215,#159216,#159217,#159218,#159219,#159220,#159221,
#159222,#159223,#159224,#159225,#159226,#159227,#159228,#159229,#159230,
#159231,#159232,#159233,#159234,#159235,#159236,#159237,#159238,#159239,
#159240,#159241),.UNSPECIFIED.,.F.,.F.,(4,3,3,3,3,3,3,3,3,3,3,3,3,3,3,3,
3,3,3,3,3,3,3,3,3,3,3,3,3,3,3,3,3,3,3,3,3,3,3,3,3,3,3,3,3,3,3,3,3,3,3,3,
3,3,3,3,4),(2.00878451684803,2.11210413325299,2.21527034106239,2.31831513543185,
2.42129472868236,2.5242432661129,2.62719484999983,2.73025123525852,2.8333646167449,
2.93665426095938,2.99650934988562,3.1000823486418,3.20350565405811,3.30681236784354,
3.41005649077507,3.5132717780959,3.61649194455095,3.7198211439703,3.82320814715697,
3.92677824242682,3.9953457998475,4.09860802522564,4.2017148865668,4.30469822083937,
4.40761486436262,4.51049905109399,4.61338497056927,4.71637738346397,4.81942565840243,
4.92265765147002,4.99418224980938,5.09760362616701,5.20087164810082,5.30401837089651,
5.40709969299362,5.51014961192928,5.61320208205137,5.71636116106689,5.81957642889854,
5.92297408622033,5.99301869977125,6.09643424801845,6.19969680809051,6.30283864671347,
6.4059154433207,6.50896120312501,6.61200988851895,6.71516579043373,6.81837821646041,
6.92177360855697,6.99185514973313,7.09670696673363,7.20139077180048,7.30591382970463,
7.41034205932222,7.51471157544563,7.59252172323623),.UNSPECIFIED.);
#1710=B_SPLINE_CURVE_WITH_KNOTS('',3,(#159245,#159246,#159247,#159248,#159249,
#159250,#159251,#159252,#159253,#159254,#159255,#159256,#159257,#159258,
#159259,#159260,#159261,#159262,#159263,#159264,#159265,#159266,#159267,
#159268,#159269,#159270,#159271,#159272,#159273,#159274,#159275,#159276,
#159277,#159278,#159279,#159280,#159281,#159282,#159283,#159284,#159285,
#159286,#159287,#159288,#159289,#159290,#159291,#159292,#159293,#159294,
#159295,#159296,#159297,#159298,#159299,#159300,#159301,#159302,#159303,
#159304,#159305,#159306,#159307,#159308,#159309,#159310,#159311,#159312,
#159313,#159314,#159315,#159316,#159317,#159318,#159319,#159320,#159321,
#159322,#159323,#159324,#159325,#159326,#159327,#159328,#159329,#159330,
#159331,#159332,#159333,#159334,#159335,#159336,#159337,#159338,#159339,
#159340,#159341,#159342,#159343,#159344,#159345,#159346,#159347,#159348,
#159349,#159350,#159351,#159352,#159353,#159354,#159355,#159356,#159357,
#159358,#159359,#159360,#159361,#159362),.UNSPECIFIED.,.F.,.F.,(4,3,3,3,
3,3,3,3,3,3,3,3,3,3,3,3,3,3,3,3,3,3,3,3,3,3,3,3,3,3,3,3,3,3,3,3,3,3,3,4),
(-3.84103903298818,-3.73547282260036,-3.63371534234889,-3.53202565145685,
-3.4303680185594,-3.32870676083673,-3.22694496855287,-3.12512265123955,
-3.0231391421579,-2.99650934988562,-2.89298815672398,-2.78961796441274,
-2.68636610744672,-2.58317789200701,-2.48001949625454,-2.37685713986037,
-2.27358681231212,-2.17025936584276,-2.0667493147523,-1.99767289992375,
-1.8953694703404,-1.79322009387015,-1.69118812153633,-1.58921885584019,
-1.48727693124249,-1.38532702267508,-1.28325476444039,-1.1811195089167,
-1.07877855598727,-0.998836449961877,-0.892562814926303,-0.780992463060515,
-0.675072152100643,-0.569251436963408,-0.463502577326272,-0.357797922575414,
-0.252080134297595,-0.146357262849723,-0.0405614307760777,0.),
 .UNSPECIFIED.);
#1711=B_SPLINE_CURVE_WITH_KNOTS('',3,(#159363,#159364,#159365,#159366,#159367,
#159368,#159369,#159370,#159371,#159372,#159373,#159374,#159375,#159376,
#159377,#159378,#159379,#159380,#159381,#159382,#159383,#159384,#159385,
#159386,#159387,#159388),.UNSPECIFIED.,.F.,.F.,(4,2,2,2,2,2,2,2,2,2,2,2,
4),(0.000655563710817076,0.0215326330434009,0.0285520766491148,0.0303960653396223,
0.0316335621891305,0.0326484304910992,0.0337175099689998,0.035063400016696,
0.0377854527867724,0.0559548979009775,0.0616383509433211,0.073938246871362,
0.074757351053836),.UNSPECIFIED.);
#1712=B_SPLINE_CURVE_WITH_KNOTS('',3,(#159394,#159395,#159396,#159397,#159398,
#159399,#159400,#159401,#159402,#159403,#159404,#159405,#159406,#159407,
#159408,#159409,#159410,#159411,#159412,#159413,#159414,#159415,#159416,
#159417),.UNSPECIFIED.,.F.,.F.,(4,2,2,2,2,2,2,2,2,2,2,4),(2.59380941840705,
2.61949833194367,2.62782998250212,2.64083525297948,2.64309079252698,2.64448016828688,
2.64555519787246,2.6465640106262,2.6477771754924,2.64956358113838,2.65529879757913,
2.6679672673912),.UNSPECIFIED.);
#1713=B_SPLINE_CURVE_WITH_KNOTS('',3,(#159418,#159419,#159420,#159421,#159422,
#159423,#159424,#159425,#159426,#159427,#159428,#159429,#159430,#159431,
#159432,#159433,#159434,#159435,#159436,#159437,#159438,#159439,#159440,
#159441,#159442,#159443,#159444,#159445,#159446,#159447,#159448,#159449,
#159450,#159451,#159452,#159453,#159454,#159455,#159456,#159457,#159458,
#159459,#159460,#159461,#159462,#159463,#159464,#159465,#159466,#159467,
#159468,#159469,#159470,#159471,#159472,#159473,#159474,#159475,#159476,
#159477,#159478,#159479,#159480,#159481,#159482,#159483,#159484,#159485,
#159486,#159487,#159488,#159489,#159490,#159491,#159492,#159493,#159494,
#159495,#159496,#159497,#159498,#159499,#159500,#159501,#159502,#159503,
#159504,#159505,#159506,#159507,#159508,#159509,#159510,#159511,#159512,
#159513,#159514,#159515,#159516,#159517,#159518,#159519,#159520,#159521,
#159522,#159523,#159524,#159525,#159526,#159527,#159528,#159529,#159530,
#159531,#159532,#159533,#159534,#159535,#159536,#159537,#159538,#159539,
#159540,#159541,#159542,#159543,#159544,#159545,#159546,#159547,#159548,
#159549,#159550,#159551,#159552,#159553,#159554,#159555,#159556,#159557,
#159558,#159559,#159560,#159561,#159562,#159563,#159564,#159565,#159566,
#159567,#159568,#159569,#159570,#159571,#159572,#159573,#159574,#159575,
#159576,#159577,#159578,#159579,#159580,#159581,#159582,#159583,#159584,
#159585,#159586,#159587,#159588,#159589,#159590,#159591,#159592,#159593,
#159594,#159595,#159596,#159597,#159598),.UNSPECIFIED.,.F.,.F.,(4,3,3,3,
3,3,3,3,3,3,3,3,3,3,3,3,3,3,3,3,3,3,3,3,3,3,3,3,3,3,3,3,3,3,3,3,3,3,3,3,
3,3,3,3,3,3,3,3,3,3,3,3,3,3,3,3,3,3,3,3,4),(7.94234083104372,7.99069159969501,
8.0940913275558,8.19733763713527,8.30046266003865,8.40352230159087,8.50655059164692,
8.60958151690829,8.7127193321595,8.81591346077179,8.91929041688598,8.98952804965688,
9.09292506229385,9.19616867712089,9.29929104945922,9.40234806908498,9.5053737698128,
9.60840214233485,9.71153747947761,9.81472916791518,9.91810377272564,9.98836449961875,
10.0917566139964,10.1949952315025,10.2981124825157,10.4011643071107,10.5041847466055,
10.6072077991242,10.7103377621749,10.8135240379095,10.9168932275747,10.9872009495806,
11.0905965473409,11.1938386983577,11.2969595406341,11.4000149901819,11.5030390830394,
11.6060658120829,11.7091994619474,11.8123894359749,11.9157623013739,11.9860373995425,
12.0894323595201,12.1926738712652,12.2957940752146,12.3988488873555,12.5018723446726,
12.6048984409897,12.7080314669147,12.811220820953,12.9145930796965,12.9848738495044,
13.0869196145448,13.1887917815621,13.2905669727719,13.3922809390561,13.4939693462706,
13.5957283236005,13.6975219982505,13.7994743367661,13.8757070301447),
 .UNSPECIFIED.);
#1714=B_SPLINE_CURVE_WITH_KNOTS('',3,(#159599,#159600,#159601,#159602,#159603,
#159604,#159605,#159606,#159607,#159608,#159609,#159610,#159611,#159612,
#159613,#159614,#159615,#159616,#159617,#159618,#159619,#159620,#159621,
#159622,#159623,#159624,#159625,#159626,#159627,#159628,#159629,#159630,
#159631,#159632,#159633,#159634,#159635,#159636,#159637,#159638,#159639,
#159640,#159641,#159642,#159643,#159644,#159645,#159646,#159647,#159648,
#159649,#159650,#159651,#159652,#159653,#159654,#159655,#159656,#159657,
#159658,#159659,#159660,#159661,#159662,#159663,#159664,#159665,#159666,
#159667,#159668,#159669,#159670,#159671,#159672,#159673,#159674,#159675,
#159676,#159677,#159678,#159679,#159680,#159681,#159682,#159683,#159684,
#159685,#159686,#159687,#159688,#159689,#159690,#159691,#159692,#159693,
#159694,#159695,#159696,#159697,#159698,#159699,#159700,#159701,#159702,
#159703,#159704,#159705,#159706,#159707,#159708,#159709,#159710,#159711,
#159712,#159713,#159714,#159715,#159716,#159717,#159718,#159719,#159720,
#159721,#159722,#159723,#159724,#159725,#159726,#159727,#159728,#159729,
#159730,#159731,#159732,#159733,#159734,#159735,#159736,#159737,#159738,
#159739,#159740,#159741,#159742,#159743,#159744,#159745,#159746,#159747,
#159748,#159749,#159750,#159751,#159752,#159753,#159754,#159755,#159756,
#159757,#159758,#159759,#159760,#159761,#159762,#159763,#159764,#159765,
#159766,#159767,#159768,#159769,#159770,#159771,#159772,#159773,#159774,
#159775,#159776,#159777,#159778,#159779,#159780,#159781,#159782,#159783,
#159784,#159785,#159786,#159787,#159788,#159789,#159790,#159791,#159792,
#159793,#159794,#159795,#159796,#159797,#159798,#159799,#159800,#159801,
#159802,#159803,#159804,#159805,#159806,#159807,#159808,#159809,#159810,
#159811,#159812,#159813,#159814,#159815,#159816,#159817,#159818,#159819,
#159820,#159821,#159822,#159823,#159824),.UNSPECIFIED.,.F.,.F.,(4,2,2,2,
2,2,2,2,2,2,2,2,2,2,2,2,2,2,2,2,2,2,2,2,2,2,2,2,2,2,2,2,2,2,2,2,2,2,2,2,
2,2,2,2,2,2,2,2,2,2,2,2,2,2,2,2,2,2,2,2,2,2,2,2,2,2,2,2,2,2,2,2,2,2,2,2,
2,2,2,2,2,2,2,2,2,2,2,2,2,2,2,2,2,2,2,2,2,2,2,2,2,2,2,2,2,2,2,2,2,2,2,2,
4),(0.074757351053836,0.0845186006271381,0.106384720369821,0.122977204701593,
0.133286118471798,0.136520268752298,0.13858070105593,0.140506700555815,
0.14302476099034,0.147271566494101,0.192337918981624,0.220918010067583,
0.234451219159256,0.241869149971209,0.24384153295974,0.244851249473479,
0.245918287764432,0.247244906105232,0.249294243898364,0.258883319395038,
0.3185052212326,0.335297135910069,0.345718964687879,0.348985015376971,0.351065311525898,
0.353009687999067,0.355551683841704,0.359839378056905,0.394232083271677,
0.443433526167964,0.453286919760675,0.455474619338454,0.456715624008577,
0.457791888078883,0.45917051636006,0.462028237367567,0.484798677090485,
0.527329496551497,0.545904454581738,0.557102081967094,0.560449586097021,
0.56254524789876,0.564478990190647,0.56697181951992,0.571099362687016,0.598278838588343,
0.640350242366268,0.656908819361003,0.665449689147922,0.667534971515463,
0.668750089568529,0.669826541244136,0.671211292004528,0.673503748486762,
0.687289037325189,0.698622663609266,0.737950132216815,0.76449239524729,
0.7706604151559,0.773322046300717,0.775273867550828,0.777074383184398,0.779989388965879,
0.787184927175935,0.833861216483231,0.856214070304714,0.870037768760637,
0.875062851503067,0.878645349335746,0.880154639072828,0.88124607318625,
0.882271358494309,0.884011337224492,0.888723725450285,0.929075723453271,
0.977359055648121,0.982966790681687,0.985530047890678,0.987467724308793,
0.989297591964075,0.99185020792562,0.99855740676454,1.05366048101905,1.07817666552133,
1.0891211768874,1.09137327690968,1.09262569462842,1.09369779571862,1.09505198513576,
1.09779132550046,1.11614970864161,1.16514966527817,1.18898300462541,1.19480672617711,
1.19740893234859,1.19935222315296,1.20117008089484,1.20367844172205,1.21011171035855,
1.26784056735071,1.290703056673,1.30119586194948,1.30341928478801,1.30466495396065,
1.30573723518031,1.3070991638523,1.30978754870971,1.32763512700414,1.33373204601547,
1.37574265174544,1.40292854550757,1.40705404758681,1.40817977855291),
 .UNSPECIFIED.);
#1715=B_SPLINE_CURVE_WITH_KNOTS('',3,(#159829,#159830,#159831,#159832,#159833,
#159834,#159835,#159836,#159837,#159838,#159839,#159840,#159841,#159842,
#159843,#159844,#159845,#159846,#159847,#159848,#159849,#159850,#159851,
#159852,#159853,#159854,#159855,#159856,#159857,#159858,#159859,#159860,
#159861,#159862,#159863,#159864,#159865,#159866,#159867,#159868,#159869,
#159870,#159871,#159872,#159873,#159874,#159875,#159876,#159877,#159878,
#159879,#159880,#159881,#159882,#159883,#159884,#159885,#159886,#159887,
#159888,#159889,#159890,#159891,#159892,#159893,#159894,#159895,#159896,
#159897,#159898,#159899,#159900,#159901,#159902,#159903,#159904,#159905,
#159906,#159907,#159908,#159909,#159910,#159911,#159912,#159913,#159914,
#159915,#159916,#159917,#159918,#159919,#159920,#159921,#159922,#159923,
#159924,#159925,#159926,#159927,#159928,#159929,#159930,#159931,#159932,
#159933,#159934,#159935,#159936,#159937,#159938,#159939,#159940,#159941,
#159942,#159943,#159944,#159945,#159946,#159947,#159948,#159949,#159950,
#159951,#159952,#159953,#159954,#159955,#159956,#159957,#159958,#159959,
#159960,#159961,#159962,#159963,#159964,#159965,#159966,#159967,#159968,
#159969,#159970,#159971,#159972,#159973,#159974,#159975,#159976,#159977,
#159978,#159979,#159980,#159981,#159982,#159983,#159984,#159985,#159986,
#159987,#159988,#159989,#159990,#159991,#159992,#159993,#159994,#159995,
#159996,#159997,#159998,#159999,#160000,#160001,#160002,#160003,#160004,
#160005,#160006,#160007,#160008,#160009,#160010,#160011,#160012,#160013,
#160014,#160015,#160016,#160017,#160018,#160019,#160020,#160021,#160022,
#160023,#160024,#160025,#160026,#160027,#160028,#160029,#160030,#160031,
#160032,#160033,#160034,#160035,#160036,#160037,#160038,#160039,#160040,
#160041,#160042,#160043,#160044,#160045,#160046,#160047,#160048,#160049,
#160050,#160051,#160052,#160053,#160054,#160055,#160056,#160057,#160058,
#160059,#160060,#160061,#160062,#160063,#160064,#160065,#160066,#160067,
#160068),.UNSPECIFIED.,.F.,.F.,(4,2,2,2,2,2,2,2,2,2,2,2,2,2,2,2,2,2,2,2,
2,2,2,2,2,2,2,2,2,2,2,2,2,2,2,2,2,2,2,2,2,2,2,2,2,2,2,2,2,2,2,2,2,2,2,2,
2,2,2,2,2,2,2,2,2,2,2,2,2,2,2,2,2,2,2,2,2,2,2,2,2,2,2,2,2,2,2,2,2,2,2,2,
2,2,2,2,2,2,2,2,2,2,2,2,2,2,2,2,2,2,2,2,2,2,2,2,2,2,2,4),(1.2600599106657,
1.26288912535391,1.26546672182187,1.26740659099323,1.2692321791735,1.27176863481297,
1.2783722939111,1.33461433894213,1.35356859569969,1.36857213176709,1.37092236730132,
1.37232497219055,1.37340466478055,1.37461133465257,1.37665672191293,1.38470193621912,
1.39984346049816,1.43954686638813,1.4708057047285,1.4750324770183,1.47755426186251,
1.47949234347171,1.48157483792521,1.48486313000707,1.49551763572174,1.51284659152949,
1.55313561931878,1.58013059772863,1.58303313425721,1.58441975480281,1.58549471901526,
1.58672467901592,1.58887517585962,1.59827196371131,1.64751324121126,1.68273421234887,
1.68703164173585,1.6895739237452,1.69151526139603,1.69358910344686,1.69683824331718,
1.70714740115669,1.7237054019932,1.75659509515038,1.77015013463504,1.77746533608878,
1.78181876712263,1.79298904519116,1.7951431604594,1.79650197108491,1.79757435442588,
1.79882307623579,1.80105931569587,1.81175029489963,1.83532213563743,1.8919015926996,
1.89846487221822,1.90099476188535,1.90281852965995,1.90475915087935,1.90734233483733,
1.91305921724745,1.93608540191422,1.9691538244237,1.99055890719327,2.00472993237957,
2.00704303828902,2.0084346488703,2.00951273409787,2.01072527727021,2.01279764212641,
2.02117128946334,2.03724274418735,2.07957429992307,2.10704942593072,2.11118323019587,
2.11367758936683,2.11561117618825,2.11770532539845,2.12104748652128,2.13219934534976,
2.15066840242999,2.1966441165456,2.21638857299317,2.21917013134654,2.22053281879586,
2.22160543750744,2.22285120126972,2.22507416361126,2.23555385409372,2.25836439253159,
2.31613632519638,2.32256110393637,2.32506828750695,2.32688602427336,2.32882987004577,
2.33143399807762,2.33726698227413,2.36116976346223,2.39067207230513,2.42835862256573,
2.43118386681462,2.43255516416355,2.43362846043887,2.43484317647371,2.43695337153951,
2.43956179473568,2.44500433206508,2.46056097646302,2.50211803345605,2.51357722963294,
2.53186992066977,2.53558058707372,2.5379739042411,2.53989032669438,2.54206276619736,
2.54575859597035,2.56078603352987,2.58950540908657,2.59380941840705),
 .UNSPECIFIED.);
#1716=B_SPLINE_CURVE_WITH_KNOTS('',3,(#160070,#160071,#160072,#160073,#160074,
#160075,#160076,#160077,#160078,#160079,#160080,#160081,#160082,#160083,
#160084,#160085,#160086,#160087,#160088,#160089,#160090,#160091,#160092,
#160093,#160094,#160095,#160096,#160097,#160098,#160099,#160100,#160101,
#160102,#160103,#160104,#160105,#160106,#160107,#160108,#160109,#160110,
#160111,#160112,#160113,#160114,#160115,#160116,#160117,#160118,#160119,
#160120,#160121,#160122,#160123,#160124,#160125,#160126,#160127,#160128,
#160129,#160130,#160131,#160132,#160133,#160134,#160135,#160136,#160137,
#160138,#160139,#160140,#160141,#160142,#160143,#160144,#160145,#160146,
#160147,#160148,#160149,#160150,#160151,#160152,#160153,#160154,#160155,
#160156,#160157,#160158,#160159,#160160,#160161,#160162,#160163,#160164,
#160165,#160166,#160167,#160168,#160169,#160170,#160171,#160172,#160173,
#160174,#160175,#160176,#160177,#160178,#160179,#160180,#160181,#160182,
#160183,#160184,#160185,#160186,#160187,#160188,#160189,#160190,#160191,
#160192,#160193,#160194,#160195,#160196,#160197,#160198,#160199,#160200,
#160201,#160202,#160203,#160204,#160205,#160206,#160207,#160208,#160209,
#160210,#160211,#160212,#160213,#160214,#160215,#160216,#160217,#160218,
#160219,#160220,#160221,#160222,#160223,#160224,#160225,#160226,#160227,
#160228,#160229,#160230,#160231,#160232,#160233,#160234,#160235,#160236,
#160237,#160238,#160239,#160240,#160241,#160242,#160243,#160244,#160245,
#160246,#160247,#160248,#160249,#160250,#160251,#160252,#160253,#160254,
#160255,#160256,#160257,#160258,#160259,#160260,#160261,#160262,#160263,
#160264,#160265,#160266,#160267,#160268,#160269,#160270,#160271,#160272,
#160273,#160274,#160275,#160276,#160277,#160278,#160279),.UNSPECIFIED.,
 .F.,.F.,(4,2,2,2,2,2,2,2,2,2,2,2,2,2,2,2,2,2,2,2,2,2,2,2,2,2,2,2,2,2,2,
2,2,2,2,2,2,2,2,2,2,2,2,2,2,2,2,2,2,2,2,2,2,2,2,2,2,2,2,2,2,2,2,2,2,2,2,
2,2,2,2,2,2,2,2,2,2,2,2,2,2,2,2,2,2,2,2,2,2,2,2,2,2,2,2,2,2,2,2,2,2,2,2,
2,4),(1.40817977855291,1.40954560774862,1.41147833506768,1.41357286092246,
1.41691845439741,1.4281081550461,1.44666702024889,1.49069794755451,1.49656825849803,
1.51244823923978,1.51506158494816,1.51640744724944,1.51747862028056,1.51873640342676,
1.52101503627392,1.53242870530449,1.55875529228532,1.61123422194255,1.61816336074522,
1.62103577801428,1.62282984191506,1.62479053342678,1.62749310835263,1.63388990777096,
1.68179592775418,1.72137458067039,1.72610766369619,1.72785087794966,1.72887686407961,
1.72996902851074,1.73147804058059,1.73505270627621,1.77423000471657,1.82298217096951,
1.83011257534725,1.83301838131916,1.83481850841655,1.83677410191252,1.83944843119071,
1.84568035406849,1.87272167021881,1.91344481746139,1.93614292237264,1.93899640814411,
1.94037316759951,1.94144684594556,1.94268250749392,1.9448600448532,1.95465124329529,
2.00353490506446,2.03864076811217,2.04293545333154,2.04547651168061,2.04741714484553,
2.04949045706281,2.05273923143588,2.06305113699394,2.07961724078901,2.11250757355492,
2.12707356620539,2.13238380146595,2.14842375962974,2.15104510417974,2.15239272485768,
2.15346399684019,2.15472036241686,2.15699278370449,2.16830033571824,2.19420980535604,
2.24727808148534,2.25416218722088,2.25702698438639,2.25881950642072,2.26078109800886,
2.26348965088267,2.26992299273335,2.29863021547031,2.34984370580904,2.360880822129,
2.36302633640549,2.36438233186787,2.3654542289635,2.36670437704547,2.36894815971249,
2.37977009097098,2.40382815546894,2.45963793744676,2.46627614938373,2.46881749744398,
2.47064395100252,2.47252001071295,2.47500421270246,2.47774234321234,2.48229405495379,
2.49162484745556,2.54226102660567,2.57203624611155,2.57495061686113,2.57633922955457,
2.57741405239469,2.57864196533992,2.58078446075229,2.59007763691164,2.60891631395619,
2.66742168200086),.UNSPECIFIED.);
#1717=B_SPLINE_CURVE_WITH_KNOTS('',3,(#160280,#160281,#160282,#160283),
 .UNSPECIFIED.,.F.,.F.,(4,4),(-16.7565929213048,-16.4074096477818),
 .UNSPECIFIED.);
#1718=B_SPLINE_CURVE_WITH_KNOTS('',3,(#160289,#160290,#160291,#160292,#160293,
#160294,#160295,#160296,#160297,#160298,#160299,#160300,#160301,#160302,
#160303,#160304),.UNSPECIFIED.,.F.,.F.,(4,2,2,2,2,2,2,4),(2.60093440570636,
2.65621612731345,2.66440519623879,2.66748629392595,2.66932347326792,2.67117334794446,
2.67347254279515,2.67554350108758),.UNSPECIFIED.);
#1719=B_SPLINE_CURVE_WITH_KNOTS('',3,(#160305,#160306,#160307,#160308,#160309,
#160310,#160311,#160312,#160313,#160314,#160315,#160316,#160317,#160318,
#160319,#160320,#160321,#160322,#160323,#160324,#160325,#160326,#160327,
#160328,#160329,#160330,#160331,#160332,#160333,#160334,#160335,#160336,
#160337,#160338,#160339,#160340,#160341,#160342,#160343,#160344,#160345,
#160346,#160347,#160348,#160349,#160350,#160351,#160352,#160353,#160354,
#160355,#160356,#160357,#160358,#160359,#160360,#160361,#160362,#160363,
#160364,#160365,#160366,#160367,#160368,#160369,#160370,#160371,#160372,
#160373,#160374,#160375,#160376,#160377,#160378,#160379,#160380,#160381,
#160382,#160383,#160384,#160385,#160386,#160387,#160388,#160389,#160390,
#160391,#160392,#160393,#160394,#160395,#160396,#160397,#160398,#160399,
#160400,#160401,#160402,#160403,#160404,#160405,#160406,#160407,#160408,
#160409,#160410,#160411,#160412,#160413,#160414,#160415,#160416,#160417,
#160418,#160419,#160420,#160421,#160422,#160423,#160424,#160425,#160426,
#160427,#160428,#160429,#160430,#160431,#160432,#160433,#160434,#160435,
#160436,#160437,#160438,#160439,#160440,#160441,#160442,#160443,#160444,
#160445,#160446,#160447,#160448,#160449,#160450,#160451,#160452,#160453,
#160454,#160455,#160456,#160457,#160458,#160459,#160460,#160461,#160462,
#160463,#160464,#160465,#160466,#160467,#160468,#160469,#160470,#160471,
#160472,#160473,#160474,#160475,#160476,#160477,#160478,#160479,#160480,
#160481,#160482,#160483,#160484,#160485,#160486,#160487,#160488,#160489,
#160490,#160491,#160492,#160493,#160494,#160495,#160496,#160497,#160498,
#160499,#160500,#160501,#160502,#160503,#160504,#160505,#160506,#160507,
#160508,#160509,#160510,#160511,#160512,#160513,#160514,#160515,#160516,
#160517,#160518,#160519,#160520,#160521,#160522,#160523,#160524,#160525,
#160526,#160527,#160528,#160529,#160530,#160531,#160532,#160533,#160534,
#160535,#160536,#160537,#160538,#160539,#160540,#160541,#160542,#160543,
#160544,#160545,#160546,#160547,#160548,#160549,#160550,#160551,#160552,
#160553,#160554,#160555,#160556),.UNSPECIFIED.,.F.,.F.,(4,2,2,2,2,2,2,2,
2,2,2,2,2,2,2,2,2,2,2,2,2,2,2,2,2,2,2,2,2,2,2,2,2,2,2,2,2,2,2,2,2,2,2,2,
2,2,2,2,2,2,2,2,2,2,2,2,2,2,2,2,2,2,2,2,2,2,2,2,2,2,2,2,2,2,2,2,2,2,2,2,
2,2,2,2,2,2,2,2,2,2,2,2,2,2,2,2,2,2,2,2,2,2,2,2,2,2,2,2,2,2,2,2,2,2,2,2,
2,2,2,2,2,2,2,2,2,4),(0.000823831819623115,0.00401800839811174,0.0104924304194195,
0.0605869953018769,0.0859355292913153,0.0970980150654373,0.0993620175889886,
0.10061653242929,0.101687951053084,0.1030379450659,0.105670338168074,0.121948896835917,
0.172208828757248,0.190225336365632,0.20118167184012,0.203640691931348,
0.205924449585136,0.205939156587538,0.205954465836589,0.205970417579372,
0.205987055811404,0.206004428922813,0.206022590221724,0.20604159843857,
0.206061518650619,0.206082423055476,0.206104392100308,0.206127515721166,
0.20615189484137,0.206177643148387,0.206204889295696,0.20623377954482,0.206264481016142,
0.206297185733427,0.206332115692975,0.208204369316481,0.210580155753786,
0.214996727511496,0.240374125406916,0.284126697672046,0.300798382684377,
0.309377389810547,0.31146587329223,0.312681813631161,0.313758847935915,
0.315143836398988,0.317435001369859,0.331166304045355,0.332819697931548,
0.33712537014045,0.353432760491326,0.386321840025734,0.402920312468902,
0.413247881169353,0.416498451223915,0.418572163273139,0.420512647622365,
0.42305275830711,0.427344188489171,0.462475421859073,0.511405738160027,
0.521174752265968,0.523350854337974,0.524586228623091,0.52565999932951,
0.527037317024668,0.529893490512413,0.566048497467635,0.598719807973166,
0.621173215863973,0.626812880026451,0.629381690192194,0.631319865414483,
0.633147475528139,0.63569254512669,0.642353070409631,0.698011138240209,
0.722204159617916,0.733062373940504,0.735308617144993,0.736559414429266,
0.737631420146538,0.738986973908385,0.741733085117442,0.760301425460177,
0.77499048799126,0.777696345221885,0.810492717848545,0.833138515677649,
0.838804483371501,0.841378282182323,0.843317379454756,0.845143771971418,
0.847683797876563,0.854311170321881,0.910310110498169,0.934284976020168,
0.945084794477429,0.94732765831116,0.948577795322991,0.949649988534673,
0.9510067460488,0.953154191892558,0.964217252849379,1.01536489706998,1.04409104779892,
1.05052796189061,1.05323756827982,1.05519976166513,1.05699272657523,1.05985798688195,
1.06674190988961,1.11989087671858,1.14579192987643,1.15709805182436,1.15937088844298,
1.16062756331162,1.16169916403531,1.16304726993864,1.16566973867728,1.18171851092261,
1.18583066515089,1.20152335318015,1.23441379642287,1.25720344504392,1.2600599106657),
 .UNSPECIFIED.);
#1720=B_SPLINE_CURVE_WITH_KNOTS('',3,(#160558,#160559,#160560,#160561,#160562,
#160563,#160564,#160565,#160566,#160567),.UNSPECIFIED.,.F.,.F.,(4,1,1,1,
1,1,1,4),(-22.6905949549614,-21.9744018991612,-20.9755654491994,-19.9767289992375,
-18.9778925492756,-17.9790560993137,-16.9802196493519,-16.7565929213048),
 .UNSPECIFIED.);
#1721=B_SPLINE_CURVE_WITH_KNOTS('',3,(#160568,#160569,#160570,#160571,#160572,
#160573,#160574,#160575,#160576,#160577,#160578,#160579,#160580,#160581,
#160582,#160583,#160584,#160585),.UNSPECIFIED.,.F.,.F.,(4,2,2,2,2,2,2,2,
4),(0.000629331620540443,0.0475078168467217,0.0567255773861956,0.0588625698839201,
0.060089245776326,0.0611642454588925,0.0625547407310968,0.06481439862756,
0.0747558145485526),.UNSPECIFIED.);
#1722=B_SPLINE_CURVE_WITH_KNOTS('',3,(#160590,#160591,#160592,#160593,#160594,
#160595,#160596,#160597,#160598,#160599,#160600,#160601,#160602,#160603,
#160604,#160605,#160606,#160607,#160608,#160609,#160610,#160611,#160612,
#160613,#160614,#160615,#160616,#160617,#160618,#160619,#160620,#160621,
#160622,#160623,#160624,#160625,#160626,#160627,#160628,#160629,#160630,
#160631,#160632,#160633,#160634,#160635,#160636,#160637,#160638,#160639,
#160640,#160641,#160642,#160643,#160644,#160645,#160646,#160647,#160648,
#160649,#160650,#160651,#160652,#160653,#160654,#160655,#160656,#160657,
#160658,#160659,#160660,#160661,#160662,#160663,#160664,#160665,#160666,
#160667,#160668,#160669,#160670,#160671,#160672,#160673,#160674,#160675,
#160676,#160677,#160678,#160679,#160680,#160681,#160682,#160683,#160684,
#160685,#160686,#160687,#160688,#160689,#160690,#160691,#160692,#160693,
#160694,#160695,#160696,#160697,#160698,#160699,#160700,#160701,#160702,
#160703,#160704,#160705,#160706,#160707,#160708,#160709,#160710,#160711,
#160712,#160713,#160714,#160715,#160716,#160717,#160718,#160719,#160720,
#160721,#160722,#160723,#160724,#160725,#160726,#160727,#160728,#160729,
#160730,#160731,#160732,#160733,#160734,#160735,#160736,#160737,#160738,
#160739,#160740,#160741,#160742,#160743,#160744,#160745,#160746,#160747,
#160748,#160749,#160750,#160751,#160752,#160753,#160754,#160755,#160756,
#160757,#160758,#160759,#160760,#160761,#160762,#160763,#160764,#160765,
#160766,#160767,#160768,#160769,#160770,#160771,#160772,#160773,#160774,
#160775,#160776,#160777,#160778,#160779,#160780,#160781,#160782,#160783,
#160784,#160785,#160786,#160787,#160788,#160789,#160790,#160791,#160792,
#160793,#160794,#160795,#160796,#160797,#160798,#160799,#160800,#160801,
#160802,#160803,#160804,#160805,#160806,#160807,#160808,#160809,#160810,
#160811,#160812,#160813,#160814,#160815,#160816,#160817,#160818,#160819,
#160820,#160821,#160822,#160823,#160824,#160825,#160826,#160827,#160828,
#160829,#160830,#160831),.UNSPECIFIED.,.F.,.F.,(4,2,2,2,2,2,2,2,2,2,2,2,
2,2,2,2,2,2,2,2,2,2,2,2,2,2,2,2,2,2,2,2,2,2,2,2,2,2,2,2,2,2,2,2,2,2,2,2,
2,2,2,2,2,2,2,2,2,2,2,2,2,2,2,2,2,2,2,2,2,2,2,2,2,2,2,2,2,2,2,2,2,2,2,2,
2,2,2,2,2,2,2,2,2,2,2,2,2,2,2,2,2,2,2,2,2,2,2,2,2,2,2,2,2,2,2,2,2,2,2,2,
4),(1.26320710672139,1.28140414234432,1.28500138353877,1.28651711084254,
1.28761306789754,1.28864171356143,1.29038764403513,1.29511760263283,1.33565551298413,
1.33755091949281,1.38151516558556,1.38876004482394,1.39169055907568,1.39349930084687,
1.39545899299493,1.39812949461983,1.40430979044002,1.43085974961406,1.46989942006753,
1.47806737419444,1.49539616576754,1.49807318164083,1.49943531608537,1.50051080902851,
1.50176370969853,1.50400882264022,1.51476846237791,1.53854565703878,1.56600522890494,
1.59803832250086,1.60229132438091,1.60482450173032,1.60676886200393,1.60885567636036,
1.61214565537418,1.62276072883805,1.63998156816887,1.68585974467617,1.69266243201266,
1.70814828222705,1.71052335679931,1.71193530537155,1.71301888120648,1.71422622885667,
1.71626478862146,1.72418361242935,1.73895518628867,1.76807925458489,1.81059592893948,
1.81490262956325,1.81745143083311,1.81939834275103,1.82147871760401,1.82473929995121,
1.8350949481432,1.85173731670276,1.8847536489348,1.90082106962562,1.90452585779774,
1.920728118739,1.92336197728496,1.92471486669975,1.92578970689773,1.92704953480292,
1.92932642430623,1.9406196402055,1.9664132761091,2.01994414452875,2.02682825603955,
2.02969870608222,2.03149640617639,2.0334649855724,2.03618561413902,2.04265916874073,
2.07162167809736,2.12175094590221,2.13377890667838,2.13598737190434,2.13736477749226,
2.13844157309132,2.13968378436968,2.14187999043465,2.15187508517746,2.20077284354723,
2.23592774949268,2.24024341448053,2.24279474285378,2.24474198657402,2.24682116726395,
2.25007664697864,2.26038889830554,2.27693571456329,2.30987152969426,2.31640056354918,
2.34567293588195,2.34859595355489,2.34998889435175,2.35106716279007,2.35229911889678,
2.35444892062684,2.36377767365169,2.38269482948208,2.39296685265398,2.44514301688019,
2.45212081150089,2.45500959828721,2.45681058500777,2.45873684234103,2.46136102539072,
2.46429298621507,2.4854012479541,2.54037683814402,2.55864646498026,2.56135594357227,
2.56272500282369,2.5638010622619,2.56504902496354,2.56727149592393,2.57766883742916,
2.6001440379358,2.60093440570636),.UNSPECIFIED.);
#1723=B_SPLINE_CURVE_WITH_KNOTS('',3,(#160832,#160833,#160834,#160835,#160836,
#160837,#160838,#160839,#160840,#160841,#160842,#160843,#160844,#160845,
#160846,#160847,#160848,#160849,#160850,#160851,#160852,#160853,#160854,
#160855,#160856,#160857,#160858,#160859,#160860,#160861,#160862,#160863,
#160864,#160865,#160866,#160867,#160868,#160869,#160870,#160871,#160872,
#160873,#160874,#160875,#160876,#160877,#160878,#160879,#160880,#160881,
#160882,#160883,#160884,#160885,#160886,#160887,#160888,#160889,#160890,
#160891,#160892,#160893,#160894,#160895,#160896,#160897,#160898,#160899,
#160900,#160901,#160902,#160903,#160904,#160905,#160906,#160907,#160908,
#160909,#160910,#160911,#160912,#160913,#160914,#160915,#160916,#160917,
#160918,#160919,#160920,#160921,#160922,#160923,#160924,#160925,#160926,
#160927,#160928,#160929,#160930,#160931,#160932,#160933,#160934,#160935,
#160936,#160937,#160938,#160939,#160940,#160941,#160942,#160943,#160944,
#160945,#160946,#160947,#160948,#160949,#160950,#160951,#160952,#160953,
#160954,#160955,#160956,#160957,#160958,#160959,#160960,#160961,#160962,
#160963,#160964,#160965,#160966,#160967,#160968,#160969,#160970,#160971,
#160972,#160973,#160974,#160975,#160976,#160977,#160978,#160979,#160980,
#160981,#160982,#160983,#160984,#160985,#160986,#160987,#160988,#160989,
#160990,#160991,#160992,#160993,#160994,#160995,#160996,#160997,#160998,
#160999,#161000,#161001,#161002,#161003,#161004,#161005,#161006,#161007,
#161008,#161009,#161010,#161011,#161012,#161013,#161014,#161015,#161016,
#161017,#161018,#161019,#161020,#161021,#161022,#161023,#161024,#161025,
#161026,#161027,#161028,#161029,#161030,#161031,#161032,#161033,#161034,
#161035,#161036,#161037,#161038,#161039,#161040,#161041,#161042,#161043,
#161044,#161045,#161046,#161047,#161048,#161049,#161050,#161051,#161052,
#161053,#161054,#161055,#161056,#161057),.UNSPECIFIED.,.F.,.F.,(4,2,2,2,
2,2,2,2,2,2,2,2,2,2,2,2,2,2,2,2,2,2,2,2,2,2,2,2,2,2,2,2,2,2,2,2,2,2,2,2,
2,2,2,2,2,2,2,2,2,2,2,2,2,2,2,2,2,2,2,2,2,2,2,2,2,2,2,2,2,2,2,2,2,2,2,2,
2,2,2,2,2,2,2,2,2,2,2,2,2,2,2,2,2,2,2,2,2,2,2,2,2,2,2,2,2,2,2,2,2,2,2,2,
4),(0.0747558145485526,0.0779070904825867,0.120249644631008,0.145989993525991,
0.159965461628393,0.163505020842006,0.165684550070463,0.167599659799729,
0.169981431001474,0.173655430061543,0.191378664380046,0.19828890932858,
0.24295086429607,0.260025988150294,0.268741768545356,0.270841011506001,
0.272059362216972,0.273135947487221,0.274517035470703,0.276794899791266,
0.290252290912955,0.292360162179196,0.299136038197401,0.344049382673289,
0.361735742077373,0.372547926332288,0.375852888847452,0.377938563445688,
0.379874516979267,0.382386317486921,0.38658052038385,0.416415903625031,
0.457671852824752,0.472771237092085,0.480799656046433,0.482843161564643,
0.484049150480445,0.485128537416682,0.486531128281553,0.48888214920247,
0.503919283598053,0.511373094173349,0.524871568033967,0.557728188154391,
0.57428627654557,0.584595735868982,0.58784433778009,0.58991769076366,0.591858468787986,
0.594399872264172,0.598695522196392,0.633840746724231,0.682831924910063,
0.692532698189676,0.694704196495929,0.695938599229324,0.69701257859874,
0.698391542028116,0.701255880442206,0.737184343239716,0.791377344542833,
0.797845270892868,0.800559854167596,0.802522732508193,0.804314319922441,
0.807173032372063,0.814018747570061,0.8676263920037,0.893200794242408,0.90442244267948,
0.906690155055799,0.907945601780378,0.909017131748506,0.910366393328177,
0.912994780488261,0.929123567550305,0.929621525660078,0.973962052568461,
1.00333240209617,1.00984521440323,1.01256740304457,1.01453174461314,1.01632190637789,
1.01917237674873,1.02596775389844,1.08017868508287,1.10534321348777,1.11645879487501,
1.11872039385959,1.11997454835422,1.12104625245535,1.12239736356506,1.12503417777243,
1.14146547420592,1.19205473798027,1.20976653569563,1.22059034191823,1.22389689679959,
1.22598312505857,1.22791928177783,1.23043090597563,1.23462384918071,1.26436858768193,
1.30531332236539,1.32779341565066,1.33045688873952,1.33179575230525,1.33276374710846,
1.33398738364706,1.33610994526848,1.34512883071186,1.36311432695761,1.4083236437572),
 .UNSPECIFIED.);
#1724=B_SPLINE_CURVE_WITH_KNOTS('',3,(#161063,#161064,#161065,#161066,#161067,
#161068),.UNSPECIFIED.,.F.,.F.,(4,2,4),(2.59382545345877,2.60858976740298,
2.66828105520032),.UNSPECIFIED.);
#1725=B_SPLINE_CURVE_WITH_KNOTS('',3,(#161069,#161070,#161071,#161072,#161073,
#161074,#161075,#161076,#161077,#161078,#161079,#161080,#161081,#161082,
#161083,#161084,#161085,#161086,#161087,#161088,#161089,#161090,#161091,
#161092,#161093,#161094,#161095,#161096,#161097,#161098,#161099,#161100,
#161101,#161102,#161103,#161104,#161105,#161106,#161107,#161108,#161109,
#161110,#161111,#161112,#161113,#161114,#161115,#161116,#161117,#161118,
#161119,#161120,#161121,#161122,#161123,#161124,#161125,#161126,#161127,
#161128,#161129,#161130,#161131,#161132,#161133,#161134,#161135,#161136,
#161137,#161138,#161139,#161140,#161141,#161142,#161143,#161144,#161145,
#161146,#161147,#161148,#161149,#161150,#161151,#161152,#161153,#161154,
#161155,#161156,#161157,#161158,#161159,#161160,#161161,#161162,#161163,
#161164,#161165,#161166,#161167,#161168,#161169,#161170,#161171,#161172,
#161173,#161174,#161175,#161176,#161177,#161178,#161179,#161180,#161181,
#161182,#161183,#161184,#161185,#161186,#161187,#161188,#161189,#161190,
#161191,#161192,#161193,#161194,#161195,#161196,#161197,#161198,#161199,
#161200,#161201,#161202,#161203,#161204,#161205,#161206,#161207,#161208,
#161209,#161210,#161211,#161212,#161213,#161214,#161215,#161216,#161217,
#161218,#161219,#161220,#161221,#161222,#161223,#161224,#161225,#161226,
#161227,#161228,#161229,#161230,#161231,#161232,#161233,#161234,#161235,
#161236,#161237,#161238,#161239,#161240,#161241,#161242,#161243,#161244,
#161245,#161246,#161247,#161248,#161249,#161250,#161251,#161252,#161253,
#161254,#161255,#161256,#161257,#161258,#161259,#161260,#161261,#161262,
#161263,#161264,#161265,#161266,#161267,#161268,#161269,#161270,#161271,
#161272,#161273,#161274,#161275,#161276,#161277,#161278,#161279,#161280,
#161281,#161282,#161283,#161284,#161285,#161286,#161287,#161288,#161289,
#161290,#161291,#161292,#161293,#161294,#161295,#161296,#161297,#161298,
#161299,#161300),.UNSPECIFIED.,.F.,.F.,(4,2,2,2,2,2,2,2,2,2,2,2,2,2,2,2,
2,2,2,2,2,2,2,2,2,2,2,2,2,2,2,2,2,2,2,2,2,2,2,2,2,2,2,2,2,2,2,2,2,2,2,2,
2,2,2,2,2,2,2,2,2,2,2,2,2,2,2,2,2,2,2,2,2,2,2,2,2,2,2,2,2,2,2,2,2,2,2,2,
2,2,2,2,2,2,2,2,2,2,2,2,2,2,2,2,2,2,2,2,2,2,2,2,2,2,2,4),(0.000810718701221239,
0.00554260920676304,0.00881069049620377,0.0102445705775083,0.0113189793639876,
0.0123417958007916,0.013364997589063,0.0148060135692522,0.018652612309518,
0.0263910026761921,0.0833917197290533,0.101376797239213,0.112318970037956,
0.115637673150875,0.117726086427897,0.119660511337923,0.122164583149168,
0.126333317872102,0.155180738303453,0.200461313494667,0.213470785694448,
0.21829327494598,0.220684984061829,0.222655718012321,0.223833871222962,
0.223837515898326,0.223841183790664,0.223844881997329,0.224893785280639,
0.226286911041078,0.22859848991649,0.2426512180014,0.246702722448747,0.295875971010819,
0.320268890090069,0.326173935108442,0.328795347896809,0.330746248224604,
0.332566375929547,0.335070246102484,0.341451014444341,0.399907259755484,
0.422483015974022,0.432907130575143,0.435130958039406,0.436379033592028,
0.437454788729539,0.438822933631868,0.441001419341293,0.452511668185328,
0.456228031163227,0.458210453133546,0.507969235807919,0.532835636036655,
0.53880221340975,0.541434703689076,0.543387524753794,0.54520491588675,0.547697940995197,
0.554013729704037,0.612970783520306,0.644629005737836,0.647423945944726,
0.648791613782613,0.64985760339708,0.651102362889227,0.653253199647321,
0.661646900927268,0.66851258319867,0.676919549212547,0.690113838868585,
0.723067667516947,0.745876052435108,0.751571588847899,0.754155296717372,
0.756100431149762,0.757931462534918,0.760476262317749,0.767106219692119,
0.823431411539454,0.847370014597311,0.858172580304495,0.860420245030225,
0.861673653540622,0.862749020387333,0.864110265999117,0.866783348118166,
0.88400989640664,0.929650504394038,0.957595998133478,0.963947949737999,
0.966647900175744,0.968612685372211,0.970414651743481,0.973308820189539,
0.980337182079209,1.03183631782581,1.0590913619819,1.0707506369482,1.07304823960531,
1.07431253075116,1.07538696131069,1.07673398002563,1.07934075859183,1.09490105320128,
1.10149592559763,1.14300544954136,1.17035691015266,1.1766366096842,1.17932425579853,
1.18128691731234,1.18309169238097,1.18600087326701,1.19311889565946,1.24290532459789,
1.26320710672139),.UNSPECIFIED.);
#1726=B_SPLINE_CURVE_WITH_KNOTS('',3,(#161302,#161303,#161304,#161305,#161306,
#161307,#161308,#161309,#161310,#161311,#161312,#161313,#161314,#161315,
#161316,#161317,#161318,#161319,#161320,#161321,#161322,#161323,#161324,
#161325,#161326,#161327,#161328,#161329,#161330,#161331,#161332,#161333,
#161334,#161335,#161336,#161337,#161338,#161339,#161340,#161341,#161342,
#161343,#161344,#161345,#161346,#161347,#161348,#161349,#161350,#161351,
#161352,#161353,#161354,#161355,#161356,#161357,#161358,#161359,#161360,
#161361,#161362,#161363,#161364,#161365,#161366,#161367,#161368,#161369,
#161370,#161371,#161372,#161373,#161374,#161375,#161376,#161377,#161378,
#161379,#161380,#161381,#161382,#161383,#161384,#161385,#161386,#161387,
#161388,#161389,#161390,#161391,#161392,#161393,#161394,#161395,#161396,
#161397,#161398,#161399,#161400,#161401,#161402,#161403,#161404,#161405,
#161406,#161407,#161408,#161409,#161410,#161411,#161412,#161413,#161414,
#161415,#161416,#161417,#161418,#161419,#161420,#161421,#161422,#161423,
#161424,#161425,#161426,#161427,#161428,#161429,#161430,#161431,#161432,
#161433,#161434,#161435,#161436,#161437,#161438,#161439,#161440,#161441,
#161442,#161443,#161444,#161445,#161446,#161447,#161448,#161449,#161450,
#161451,#161452,#161453,#161454,#161455,#161456,#161457,#161458,#161459,
#161460,#161461,#161462,#161463,#161464,#161465,#161466,#161467,#161468,
#161469,#161470,#161471,#161472,#161473,#161474,#161475,#161476,#161477,
#161478,#161479,#161480,#161481,#161482,#161483,#161484,#161485,#161486,
#161487,#161488,#161489,#161490,#161491,#161492,#161493,#161494,#161495,
#161496,#161497,#161498,#161499,#161500,#161501,#161502,#161503,#161504,
#161505,#161506,#161507,#161508,#161509,#161510,#161511,#161512,#161513,
#161514,#161515,#161516,#161517,#161518,#161519,#161520,#161521,#161522,
#161523,#161524,#161525,#161526,#161527),.UNSPECIFIED.,.F.,.F.,(4,2,2,2,
2,2,2,2,2,2,2,2,2,2,2,2,2,2,2,2,2,2,2,2,2,2,2,2,2,2,2,2,2,2,2,2,2,2,2,2,
2,2,2,2,2,2,2,2,2,2,2,2,2,2,2,2,2,2,2,2,2,2,2,2,2,2,2,2,2,2,2,2,2,2,2,2,
2,2,2,2,2,2,2,2,2,2,2,2,2,2,2,2,2,2,2,2,2,2,2,2,2,2,2,2,2,2,2,2,2,2,2,2,
4),(1.4083236437572,1.41333088102273,1.43113507874003,1.43481460833219,
1.43719828185415,1.43911380859235,1.44129260787215,1.44501750954835,1.46042424063277,
1.51176001269828,1.53943960591465,1.54234661805959,1.54373395565199,1.54480881996912,
1.54603793152059,1.54818521995648,1.5575410729071,1.60680754718084,1.64203163357876,
1.64632838195724,1.6488702241749,1.65081120474635,1.65288464475482,1.65613311175937,
1.66643977270715,1.68299341831262,1.71587590631286,1.72932272850514,1.73690850471888,
1.75190581616602,1.75425534624431,1.75565756083092,1.75673697171553,1.75794334773225,
1.75998828226784,1.76803229050528,1.78317232121768,1.82287871736754,1.85411353439998,
1.85833888367202,1.86085992235106,1.86279749047767,1.86487949205803,1.86816713072526,
1.87882061679871,1.89614899638409,1.94436622567246,1.94866622868069,1.95164780867162,
1.964114487631,1.96634200506697,1.96772295144803,1.96879713313419,1.97003026604958,
1.97219594288744,1.98181269988829,2.03085053856742,2.06600585940044,2.07030157363753,
2.07284306510737,2.07478392816005,2.07685738836378,2.08010619126858,2.09041648203885,
2.1069783966275,2.13986700711218,2.15403049940507,2.1599766382467,2.17581378956652,
2.17842647832321,2.17977231448054,2.18084356398319,2.1821015189154,2.18438096846461,
2.19580920798741,2.22219368929917,2.27459135630503,2.28152570238893,2.28439890186766,
2.28619305096762,2.2881535114613,2.29085517423541,2.29724700768573,2.34319558300291,
2.36575831840106,2.37225027459431,2.38783353350176,2.39043517498929,2.39177859327856,
2.39284965042523,2.39410939384263,2.39639723893086,2.40797587152629,2.43496484031123,
2.47463666767185,2.49124595386254,2.49484613103896,2.49720516282961,2.49911867099566,
2.50092102866028,2.50411069483385,2.51448476108362,2.53127830882496,2.55157207583426,
2.59669168652602,2.60141377415054,2.60315522484572,2.6041807997957,2.60527312030848,
2.60678322172997,2.61036438665645,2.6481167165806,2.6673459870611),
 .UNSPECIFIED.);
#1727=B_SPLINE_CURVE_WITH_KNOTS('',3,(#161528,#161529,#161530,#161531,#161532,
#161533,#161534,#161535,#161536,#161537,#161538,#161539,#161540,#161541,
#161542,#161543,#161544,#161545,#161546,#161547),.UNSPECIFIED.,.F.,.F.,
(4,2,2,2,2,2,2,2,2,4),(0.000704181919289228,0.0257174334271328,0.0359847052706526,
0.0390634794182119,0.041189796444609,0.0432709609679292,0.045208316296964,
0.0477298861286788,0.0519579423206877,0.0751489568361618),.UNSPECIFIED.);
#1728=B_SPLINE_CURVE_WITH_KNOTS('',3,(#161552,#161553,#161554,#161555,#161556,
#161557,#161558,#161559,#161560,#161561,#161562,#161563,#161564,#161565,
#161566,#161567,#161568,#161569,#161570,#161571,#161572,#161573,#161574,
#161575,#161576,#161577,#161578,#161579,#161580,#161581,#161582,#161583,
#161584,#161585,#161586,#161587,#161588,#161589,#161590,#161591,#161592,
#161593,#161594,#161595,#161596,#161597,#161598,#161599,#161600,#161601,
#161602,#161603,#161604,#161605,#161606,#161607,#161608,#161609,#161610,
#161611,#161612,#161613,#161614,#161615,#161616,#161617,#161618,#161619,
#161620,#161621,#161622,#161623,#161624,#161625,#161626,#161627,#161628,
#161629,#161630,#161631,#161632,#161633,#161634,#161635,#161636,#161637,
#161638,#161639,#161640,#161641,#161642,#161643,#161644,#161645,#161646,
#161647,#161648,#161649,#161650,#161651,#161652,#161653,#161654,#161655,
#161656,#161657,#161658,#161659,#161660,#161661,#161662,#161663,#161664,
#161665,#161666,#161667,#161668,#161669,#161670,#161671,#161672,#161673,
#161674,#161675,#161676,#161677,#161678,#161679,#161680,#161681,#161682,
#161683,#161684,#161685,#161686,#161687,#161688,#161689,#161690,#161691,
#161692,#161693,#161694,#161695,#161696,#161697,#161698,#161699,#161700,
#161701,#161702,#161703,#161704,#161705,#161706,#161707,#161708,#161709,
#161710,#161711,#161712,#161713,#161714,#161715,#161716,#161717,#161718,
#161719,#161720,#161721,#161722,#161723,#161724,#161725,#161726,#161727,
#161728,#161729,#161730,#161731,#161732,#161733,#161734,#161735,#161736,
#161737,#161738,#161739,#161740,#161741,#161742,#161743,#161744,#161745,
#161746,#161747,#161748,#161749,#161750,#161751,#161752,#161753,#161754,
#161755,#161756,#161757,#161758,#161759,#161760,#161761,#161762,#161763,
#161764,#161765,#161766,#161767,#161768,#161769,#161770,#161771,#161772,
#161773,#161774,#161775,#161776,#161777,#161778,#161779,#161780,#161781,
#161782,#161783,#161784,#161785,#161786,#161787,#161788,#161789,#161790,
#161791,#161792,#161793,#161794,#161795,#161796,#161797,#161798,#161799,
#161800,#161801,#161802,#161803,#161804,#161805,#161806,#161807,#161808,
#161809,#161810,#161811,#161812,#161813,#161814,#161815,#161816,#161817,
#161818,#161819,#161820,#161821,#161822,#161823,#161824,#161825,#161826,
#161827,#161828,#161829,#161830,#161831,#161832,#161833,#161834,#161835),
 .UNSPECIFIED.,.F.,.F.,(4,2,2,2,2,2,2,2,2,2,2,2,2,2,2,2,2,2,2,2,2,2,2,2,
2,2,2,2,2,2,2,2,2,2,2,2,2,2,2,2,2,2,2,2,2,2,2,2,2,2,2,2,2,2,2,2,2,2,2,2,
2,2,2,2,2,2,2,2,2,2,2,2,2,2,2,2,2,2,2,2,2,2,2,2,2,2,2,2,2,2,2,2,2,2,2,2,
2,2,2,2,2,2,2,2,2,2,2,2,2,2,2,2,2,2,2,2,2,2,2,2,2,2,2,2,2,2,2,2,2,2,2,2,
2,2,2,2,2,2,2,2,2,4),(1.26013242656284,1.26847918134053,1.2938564122058,
1.29812711955091,1.30042465381827,1.30231772666777,1.3045584725669,1.30845763746593,
1.3243663415617,1.33458859927051,1.37387299698104,1.4024572161702,1.4053697735664,
1.40675832499297,1.40783346977875,1.40906216367256,1.41120699114716,1.42052526401983,
1.46970173840529,1.50507092651571,1.50937010626214,1.51191286829673,1.51385425276344,
1.51592783494069,1.51917592094151,1.52947628965138,1.54601499838239,1.57356179924573,
1.5897043460026,1.60078541295709,1.61502070589077,1.61733730448075,1.61872998294231,
1.61980826017967,1.62102030954763,1.6230902427204,1.6314329097389,1.64741501045388,
1.68972964697637,1.71734583451292,1.72148352025247,1.72397909849109,1.72591296472535,
1.72800675256841,1.73134689975681,1.7424786549331,1.76090055733768,1.80770061574921,
1.81249826086563,1.82339984547313,1.82845376648346,1.83024456505479,1.83128003435429,
1.83236713223855,1.83384477279152,1.83723798187632,1.84192243504985,1.85438809617534,
1.88539080905029,1.92909919171492,1.93338877780441,1.93592874243147,1.93786964938256,
1.93994433061575,1.94319750069632,1.95354238542488,1.97017964780189,2.00313452907881,
2.02128581528153,2.03881227559786,2.04149029520036,2.04285029656371,2.04392274505452,
2.04517053947875,2.04740263377742,2.05802725879118,2.08135818609268,2.13831025169886,
2.1448319530684,2.14735509137067,2.14917705166816,2.15111858720384,2.15370785936002,
2.1594584038067,2.18273718211609,2.2232585956789,2.2379885967061,2.25117560153088,
2.25344040570918,2.25483260280213,2.25590799356616,2.25713409396543,2.25926769005325,
2.26843475405723,2.31716148689409,2.35312562790782,2.35784809405546,2.36027128666429,
2.36219053876016,2.36434389000288,2.36795350025004,2.38192047521569,2.43273432932107,
2.46258728964277,2.4654995248621,2.46688790208378,2.46793103838049,2.46793599692886,
2.46794086746965,2.46794565197622,2.46795035244432,2.46795497071022,2.46795950855504,
2.46796396780665,2.46796835018156,2.46797265740426,2.46797689093535,2.46798105251445,
2.46798514361251,2.46798916574424,2.46799312034853,2.46799700881634,2.46800061011772,
2.46800419784891,2.46800777221051,2.46801133342244,2.4680148813335,2.46923820354584,
2.47054910125195,2.47257198390835,2.47638445811796,2.48565763471479,2.52352802125493,
2.53702592018721,2.56540108051988,2.56955862836313,2.57205996523756,2.57399461867134,
2.57608560313406,2.57941339266775,2.59043117045207,2.59382545345877),
 .UNSPECIFIED.);
#1729=B_SPLINE_CURVE_WITH_KNOTS('',3,(#161836,#161837,#161838,#161839,#161840,
#161841,#161842,#161843,#161844,#161845,#161846,#161847,#161848,#161849,
#161850,#161851,#161852,#161853,#161854,#161855,#161856,#161857,#161858,
#161859,#161860,#161861,#161862,#161863,#161864,#161865,#161866,#161867,
#161868,#161869,#161870,#161871,#161872,#161873,#161874,#161875,#161876,
#161877,#161878,#161879,#161880,#161881,#161882,#161883,#161884,#161885,
#161886,#161887,#161888,#161889,#161890,#161891,#161892,#161893,#161894,
#161895,#161896,#161897,#161898,#161899,#161900,#161901,#161902,#161903,
#161904,#161905,#161906,#161907,#161908,#161909,#161910,#161911,#161912,
#161913,#161914,#161915,#161916,#161917,#161918,#161919,#161920,#161921,
#161922,#161923,#161924,#161925,#161926,#161927,#161928,#161929,#161930,
#161931,#161932,#161933,#161934,#161935,#161936,#161937,#161938,#161939,
#161940,#161941,#161942,#161943,#161944,#161945,#161946,#161947,#161948,
#161949,#161950,#161951,#161952,#161953,#161954,#161955,#161956,#161957,
#161958,#161959,#161960,#161961,#161962,#161963,#161964,#161965,#161966,
#161967,#161968,#161969,#161970,#161971,#161972,#161973,#161974,#161975,
#161976,#161977,#161978,#161979,#161980,#161981,#161982,#161983,#161984,
#161985,#161986,#161987,#161988,#161989,#161990,#161991,#161992,#161993,
#161994,#161995,#161996,#161997,#161998,#161999,#162000,#162001,#162002,
#162003,#162004,#162005,#162006,#162007,#162008,#162009,#162010,#162011,
#162012,#162013,#162014,#162015,#162016,#162017,#162018,#162019,#162020,
#162021,#162022,#162023,#162024,#162025,#162026,#162027,#162028,#162029,
#162030,#162031,#162032,#162033,#162034,#162035,#162036,#162037,#162038,
#162039,#162040,#162041,#162042,#162043,#162044,#162045,#162046,#162047,
#162048,#162049,#162050,#162051,#162052,#162053,#162054,#162055,#162056,
#162057,#162058,#162059,#162060,#162061,#162062,#162063,#162064,#162065),
 .UNSPECIFIED.,.F.,.F.,(4,2,2,2,2,2,2,2,2,2,2,2,2,2,2,2,2,2,2,2,2,2,2,2,
2,2,2,2,2,2,2,2,2,2,2,2,2,2,2,2,2,2,2,2,2,2,2,2,2,2,2,2,2,2,2,2,2,2,2,2,
2,2,2,2,2,2,2,2,2,2,2,2,2,2,2,2,2,2,2,2,2,2,2,2,2,2,2,2,2,2,2,2,2,2,2,2,
2,2,2,2,2,2,2,2,2,2,2,2,2,2,2,2,2,2,4),(0.0751489568361618,0.0833449554465519,
0.108641044920857,0.13643639417136,0.145888780373659,0.148042561636215,
0.149272889427158,0.150347200439784,0.151731685845863,0.15397150696322,
0.166679492706045,0.189075522143858,0.21602105826756,0.237186514044569,
0.245292357039389,0.251237193407344,0.253852945759734,0.255807448099823,
0.257608548802691,0.260520314133154,0.267687292186551,0.315460101430164,
0.355564539204594,0.35916186777971,0.360674655778008,0.361767379036676,
0.362792108113141,0.364529513521338,0.369225456412141,0.4100672476177,0.456723676866092,
0.463116321672252,0.465818002434891,0.467778359893003,0.469572338490051,
0.472445086812289,0.4793774053219,0.531828880147045,0.558201172160656,0.569625398196958,
0.571904539571247,0.573162375005064,0.5742335568168,0.575579345175449,0.578192051861403,
0.594045473246712,0.598812469573507,0.614066862527545,0.646942646584495,
0.663524224601453,0.673844261091207,0.677094043431458,0.679167632965294,
0.681108269480274,0.683648964137022,0.68794224291894,0.730340769312746,
0.759394175981448,0.774119156147365,0.782012070532489,0.78404402550762,
0.785247464640317,0.786327541631833,0.78773492830596,0.790102318017432,
0.805539438786653,0.812257187230313,0.826054822290535,0.858915373230047,
0.875477569270088,0.885788964040406,0.889037844799358,0.891111296217081,
0.893052110514189,0.895593480881535,0.899888894180826,0.935008265132251,
0.98391811743147,0.993716904537488,0.995895161085198,0.997131070231455,
0.99820486564332,0.999581639982368,1.00243471029315,1.02510631592757,1.03806040668731,
1.07091616283321,1.08747013021954,1.0977781014675,1.10102680821244,1.10310036600066,
1.10504143261076,1.10758335377593,1.11188019211292,1.14707724642032,1.19622694753891,
1.20575167390782,1.20791111016212,1.20914295954032,1.21021749394502,1.2116008152167,
1.21383590954592,1.22644269909234,1.23297510085648,1.23810837803455,1.27817128215072,
1.30767505401814,1.31208547029223,1.31441240100971,1.31613949187338,1.31829592426455,
1.32191875657871,1.33436950633737,1.38533028477281,1.40863209392471),
 .UNSPECIFIED.);
#1730=B_SPLINE_CURVE_WITH_KNOTS('',3,(#162071,#162072,#162073,#162074,#162075,
#162076,#162077,#162078,#162079,#162080),.UNSPECIFIED.,.F.,.F.,(4,2,2,2,
4),(2.59333918514653,2.59405628316297,2.6039559079893,2.65275178216379,
2.66750871075831),.UNSPECIFIED.);
#1731=B_SPLINE_CURVE_WITH_KNOTS('',3,(#162081,#162082,#162083,#162084,#162085,
#162086,#162087,#162088,#162089,#162090,#162091,#162092,#162093,#162094,
#162095,#162096,#162097,#162098,#162099,#162100,#162101,#162102,#162103,
#162104,#162105,#162106,#162107,#162108,#162109,#162110,#162111,#162112,
#162113,#162114,#162115,#162116,#162117,#162118,#162119,#162120,#162121,
#162122,#162123,#162124,#162125,#162126,#162127,#162128,#162129,#162130,
#162131,#162132,#162133,#162134,#162135,#162136,#162137,#162138,#162139,
#162140,#162141,#162142,#162143,#162144,#162145,#162146,#162147,#162148,
#162149,#162150,#162151,#162152,#162153,#162154,#162155,#162156,#162157,
#162158,#162159,#162160,#162161,#162162,#162163,#162164,#162165,#162166,
#162167,#162168,#162169,#162170,#162171,#162172,#162173,#162174,#162175,
#162176,#162177,#162178,#162179,#162180,#162181,#162182,#162183,#162184,
#162185,#162186,#162187,#162188,#162189,#162190,#162191,#162192,#162193,
#162194,#162195,#162196,#162197,#162198,#162199,#162200,#162201,#162202,
#162203,#162204,#162205,#162206,#162207,#162208,#162209,#162210,#162211,
#162212,#162213,#162214,#162215,#162216,#162217,#162218,#162219,#162220,
#162221,#162222,#162223,#162224,#162225,#162226,#162227,#162228,#162229,
#162230,#162231,#162232,#162233,#162234,#162235,#162236,#162237,#162238,
#162239,#162240,#162241,#162242,#162243,#162244,#162245,#162246,#162247,
#162248,#162249,#162250,#162251,#162252,#162253,#162254,#162255,#162256,
#162257,#162258,#162259,#162260,#162261,#162262,#162263,#162264,#162265,
#162266,#162267,#162268,#162269,#162270,#162271,#162272,#162273,#162274,
#162275,#162276,#162277,#162278,#162279,#162280,#162281,#162282,#162283,
#162284,#162285,#162286,#162287,#162288,#162289,#162290,#162291,#162292,
#162293,#162294,#162295,#162296,#162297,#162298,#162299,#162300,#162301,
#162302,#162303,#162304),.UNSPECIFIED.,.F.,.F.,(4,2,2,2,2,2,2,2,2,2,2,2,
2,2,2,2,2,2,2,2,2,2,2,2,2,2,2,2,2,2,2,2,2,2,2,2,2,2,2,2,2,2,2,2,2,2,2,2,
2,2,2,2,2,2,2,2,2,2,2,2,2,2,2,2,2,2,2,2,2,2,2,2,2,2,2,2,2,2,2,2,2,2,2,2,
2,2,2,2,2,2,2,2,2,2,2,2,2,2,2,2,2,2,2,2,2,2,2,2,2,2,2,4),(0.000768646098525406,
0.0217309817958381,0.0248341135680857,0.0269704303777135,0.0287696752420724,
0.0306848669530417,0.0330688062049348,0.0367500644603691,0.0545889053194324,
0.072976426511539,0.121840731681455,0.131681559431032,0.133862402465048,
0.135098744280054,0.136172254774499,0.137547801196249,0.140395367973628,
0.176851300966736,0.209417973596582,0.225629647754282,0.232376498172673,
0.237517164998177,0.239979927065182,0.241821109356285,0.243648389985645,
0.24619263155957,0.252848770294063,0.308527217431946,0.332702250954838,
0.343555212971455,0.345800986701256,0.347051608827662,0.348123517583509,
0.349479016880949,0.351622788493995,0.362631176800057,0.41390476092387,
0.442559457110958,0.448987263154324,0.45169501212071,0.453656578007115,
0.455449463209985,0.458315670049848,0.465207432626328,0.518223304340964,
0.544204779337861,0.55553046951741,0.557804109580375,0.55906080818677,0.560132173748389,
0.561479658771376,0.564099964090362,0.580119165322993,0.585171725011565,
0.629884117999277,0.648404509572726,0.659579206323581,0.662923538439578,
0.66501800966143,0.666951188477761,0.669444035816599,0.673573230202735,
0.700872959537443,0.74313000808192,0.759409658662449,0.767854453894341,
0.76993243152354,0.771146140908599,0.772223829844904,0.773613062349352,
0.775918320327097,0.78993599693432,0.791300662880673,0.798313629024612,
0.811988486142423,0.844849500022869,0.861411040465311,0.871722287033649,
0.874971259424407,0.877044802557563,0.878985726048627,0.881527273081773,
0.885823060478109,0.920955452540655,0.969902002886644,0.979660845880634,
0.981836453631895,0.983071820463264,0.98414575958055,0.985523521937409,
0.988381404501232,1.01124164447141,1.02400683492131,1.05686258733372,1.07341533033534,
1.08372289663384,1.08697166607503,1.08904530962754,1.09098648866183,1.09352860343324,
1.09782587301926,1.13304060983893,1.18224601591773,1.19170998865719,1.19386521180401,
1.19509617320075,1.19617091431267,1.19755579201663,1.19979593007968,1.21249735659049,
1.23487541233553,1.26013242656284),.UNSPECIFIED.);
#1732=B_SPLINE_CURVE_WITH_KNOTS('',3,(#162306,#162307,#162308,#162309,#162310,
#162311,#162312,#162313,#162314,#162315,#162316,#162317,#162318,#162319,
#162320,#162321,#162322,#162323,#162324,#162325,#162326,#162327,#162328,
#162329,#162330,#162331,#162332,#162333,#162334,#162335,#162336,#162337,
#162338,#162339,#162340,#162341,#162342,#162343,#162344,#162345,#162346,
#162347,#162348,#162349,#162350,#162351,#162352,#162353,#162354,#162355,
#162356,#162357,#162358,#162359,#162360,#162361,#162362,#162363,#162364,
#162365,#162366,#162367,#162368,#162369,#162370,#162371,#162372,#162373,
#162374,#162375,#162376,#162377,#162378,#162379,#162380,#162381,#162382,
#162383,#162384,#162385,#162386,#162387,#162388,#162389,#162390,#162391,
#162392,#162393,#162394,#162395,#162396,#162397,#162398,#162399,#162400,
#162401,#162402,#162403,#162404,#162405,#162406,#162407,#162408,#162409,
#162410,#162411,#162412,#162413,#162414,#162415,#162416,#162417,#162418,
#162419,#162420,#162421,#162422,#162423,#162424,#162425,#162426,#162427,
#162428,#162429,#162430,#162431,#162432,#162433,#162434,#162435,#162436,
#162437,#162438,#162439,#162440,#162441,#162442,#162443,#162444,#162445,
#162446,#162447,#162448,#162449,#162450,#162451,#162452,#162453,#162454,
#162455,#162456,#162457,#162458,#162459,#162460,#162461,#162462,#162463,
#162464,#162465,#162466,#162467,#162468,#162469,#162470,#162471,#162472,
#162473,#162474,#162475,#162476,#162477,#162478,#162479,#162480,#162481,
#162482,#162483,#162484,#162485,#162486,#162487,#162488,#162489,#162490,
#162491,#162492,#162493,#162494,#162495,#162496,#162497,#162498,#162499,
#162500,#162501,#162502,#162503,#162504,#162505,#162506,#162507,#162508,
#162509,#162510,#162511,#162512,#162513,#162514,#162515,#162516,#162517,
#162518,#162519,#162520,#162521,#162522,#162523,#162524,#162525,#162526,
#162527,#162528,#162529,#162530,#162531),.UNSPECIFIED.,.F.,.F.,(4,2,2,2,
2,2,2,2,2,2,2,2,2,2,2,2,2,2,2,2,2,2,2,2,2,2,2,2,2,2,2,2,2,2,2,2,2,2,2,2,
2,2,2,2,2,2,2,2,2,2,2,2,2,2,2,2,2,2,2,2,2,2,2,2,2,2,2,2,2,2,2,2,2,2,2,2,
2,2,2,2,2,2,2,2,2,2,2,2,2,2,2,2,2,2,2,2,2,2,2,2,2,2,2,2,2,2,2,2,2,2,2,2,
4),(1.40863209392471,1.41654004015942,1.41945322232817,1.42084187779814,
1.42191701390898,1.42314559807403,1.42529000014722,1.43460280781364,1.48376179701782,
1.51915216916635,1.52345152062868,1.52599430522233,1.52793566143861,1.53000916937361,
1.5332570471261,1.54355598158733,1.56009165224911,1.5929619616422,1.60448792644199,
1.61424432011087,1.616083043487,1.62920572003994,1.63146738296949,1.63285867803094,
1.63393402438427,1.63516080211121,1.63729727256023,1.6465024232659,1.6650626351445,
1.70910389964158,1.73177230506072,1.73572450676605,1.73819157751035,1.74011589131014,
1.7422444183836,1.74574152273181,1.75844262846443,1.78069138277645,1.82661416362083,
1.84109882641281,1.84342683756833,1.84482287069084,1.84590159531708,1.84711174698918,
1.84917310970567,1.85741106613972,1.87309470335307,1.91500271990899,1.94340736467262,
1.94756591043407,1.9500676219038,1.95200243176961,1.95409345285052,1.95742101540776,
1.96843542360814,1.98658578893815,2.03627510442844,2.03766423139636,2.03787170234985,
2.04116319860353,2.05333850278761,2.05555053616329,2.05692693064984,2.05800083663026,
2.05923734118391,2.06141775571317,2.07124506207417,2.12011418295603,2.15521860878868,
2.15951431615174,2.16205602934499,2.16399719176571,2.16607109788608,2.1693208627816,
2.17963642647082,2.1962089237285,2.22910963071889,2.26471089204683,2.2675774835449,
2.26895701128334,2.27003118301784,2.27126553685399,2.27343629182438,2.28312333534856,
2.3321089936017,2.36725061824319,2.37154667908901,2.37408844848276,2.37602956573768,
2.37810333819365,2.38135271529671,2.39166554439082,2.40823221768773,2.47087662185185,
2.47223807011973,2.4784121202474,2.4803506188615,2.48153349538097,2.4825652255805,
2.48397838287725,2.48699359698213,2.4910919890305,2.50137087532382,2.52419460816738,
2.57590998757691,2.58289424438075,2.58577628814764,2.58757249419691,2.58953243240337,
2.59222832476124,2.59858285211227,2.62662180212059,2.66831522286306),
 .UNSPECIFIED.);
#1733=B_SPLINE_CURVE_WITH_KNOTS('',3,(#162532,#162533,#162534,#162535,#162536,
#162537,#162538,#162539,#162540,#162541,#162542,#162543,#162544),
 .UNSPECIFIED.,.F.,.F.,(4,3,3,3,4),(-48.1740291001457,-48.070804245227,
-47.9674104963029,-47.94414959817,-47.8233361836797),.UNSPECIFIED.);
#1734=B_SPLINE_CURVE_WITH_KNOTS('',3,(#162549,#162550,#162551,#162552,#162553,
#162554,#162555,#162556,#162557,#162558,#162559,#162560,#162561,#162562,
#162563,#162564,#162565,#162566,#162567,#162568,#162569,#162570,#162571,
#162572,#162573,#162574,#162575,#162576,#162577,#162578,#162579,#162580,
#162581,#162582,#162583,#162584,#162585,#162586,#162587,#162588,#162589,
#162590,#162591,#162592,#162593,#162594,#162595,#162596,#162597,#162598,
#162599,#162600,#162601,#162602,#162603,#162604,#162605,#162606,#162607,
#162608,#162609,#162610,#162611,#162612,#162613,#162614,#162615,#162616,
#162617,#162618,#162619,#162620,#162621,#162622,#162623,#162624,#162625,
#162626,#162627,#162628,#162629,#162630,#162631,#162632,#162633,#162634,
#162635,#162636,#162637,#162638,#162639,#162640,#162641,#162642,#162643,
#162644,#162645,#162646,#162647,#162648,#162649,#162650,#162651,#162652,
#162653,#162654,#162655,#162656,#162657,#162658,#162659,#162660,#162661,
#162662,#162663,#162664,#162665,#162666,#162667,#162668,#162669,#162670,
#162671,#162672,#162673,#162674,#162675,#162676,#162677,#162678,#162679,
#162680,#162681,#162682,#162683,#162684,#162685,#162686,#162687,#162688,
#162689,#162690,#162691,#162692,#162693,#162694,#162695,#162696,#162697,
#162698,#162699,#162700,#162701,#162702,#162703,#162704,#162705,#162706,
#162707,#162708,#162709,#162710,#162711,#162712,#162713,#162714,#162715,
#162716,#162717,#162718,#162719,#162720,#162721,#162722,#162723,#162724,
#162725,#162726,#162727,#162728,#162729,#162730,#162731,#162732,#162733,
#162734,#162735,#162736,#162737,#162738,#162739,#162740,#162741,#162742,
#162743,#162744,#162745,#162746,#162747,#162748,#162749,#162750,#162751,
#162752,#162753,#162754,#162755,#162756,#162757,#162758,#162759,#162760,
#162761,#162762,#162763,#162764,#162765,#162766,#162767,#162768,#162769,
#162770,#162771,#162772,#162773,#162774,#162775,#162776,#162777,#162778,
#162779,#162780),.UNSPECIFIED.,.F.,.F.,(4,2,2,2,2,2,2,2,2,2,2,2,2,2,2,2,
2,2,2,2,2,2,2,2,2,2,2,2,2,2,2,2,2,2,2,2,2,2,2,2,2,2,2,2,2,2,2,2,2,2,2,2,
2,2,2,2,2,2,2,2,2,2,2,2,2,2,2,2,2,2,2,2,2,2,2,2,2,2,2,2,2,2,2,2,2,2,2,2,
2,2,2,2,2,2,2,2,2,2,2,2,2,2,2,2,2,2,2,2,2,2,2,2,2,2,2,4),(1.25968344386625,
1.28150393949821,1.30395459826603,1.31433181789067,1.31654822237659,1.31779250816769,
1.31886523225317,1.32022982656628,1.32240323674052,1.33389993938574,1.38263554309166,
1.41583881962656,1.42010267369441,1.42263496489568,1.42457438527109,1.42665174044739,
1.42991805103097,1.440381112104,1.45728206404355,1.49511039169191,1.52518596249867,
1.52810055377774,1.52948933043945,1.5305643070714,1.53179242573215,1.53393535200595,
1.54323150792161,1.56207804948947,1.6024785251327,1.61474061934373,1.62934646323569,
1.63313474148773,1.63534973117589,1.63726199042886,1.63959702007219,1.64404694231465,
1.67495964457103,1.7218063003911,1.73760402139448,1.74021650558827,1.74156239028271,
1.74263375961614,1.74389194951601,1.74617206525345,1.75760864352059,1.78402404438808,
1.83638781280756,1.84332624544597,1.84620032318074,1.847994782719,1.84995539175352,
1.85265691075267,1.85904676502496,1.88738505136668,1.93728489306762,1.94991460954658,
1.95215085420973,1.95353447610928,1.95460898415596,1.95584052030327,1.95799872417219,
1.96750744967562,2.01664201563862,2.05182814883153,2.05612450854903,2.05866627047294,
2.06060727589271,2.06268082597604,2.06592963981941,2.0762388705972,2.09279804116576,
2.1256856002288,2.13955191023882,2.14611402275446,2.16166405363361,2.16426448434662,
2.16560772427733,2.16667887608442,2.16793900642414,2.17022826098598,2.18182902855897,
2.20890564652439,2.26033635833336,2.26733508487012,2.27021903465975,2.27201522785433,
2.27397419398567,2.27666700567814,2.28300614085763,2.31092468184607,2.3569364842496,
2.35799573600593,2.37367266475889,2.37627850051508,2.37762290532363,2.37869412496694,
2.37995333413688,2.38223835174115,2.39376346889887,2.42053434164097,2.47236736426887,
2.47935688017427,2.48223929524866,2.48403520171132,2.48585600442242,2.48840937961275,
2.49400406753632,2.50151762643898,2.52045156533893,2.54849914024973,2.58534459312385,
2.58818603325233,2.58956046783506,2.59063397996847,2.59187131574407,2.59333918514653),
 .UNSPECIFIED.);
#1735=B_SPLINE_CURVE_WITH_KNOTS('',3,(#162782,#162783,#162784,#162785,#162786,
#162787,#162788,#162789,#162790,#162791,#162792,#162793,#162794,#162795,
#162796,#162797,#162798,#162799,#162800,#162801,#162802,#162803,#162804,
#162805,#162806,#162807,#162808,#162809,#162810,#162811,#162812,#162813,
#162814,#162815,#162816,#162817,#162818,#162819,#162820,#162821,#162822,
#162823,#162824,#162825,#162826,#162827,#162828,#162829,#162830,#162831,
#162832,#162833,#162834,#162835,#162836,#162837,#162838,#162839,#162840,
#162841,#162842,#162843,#162844,#162845,#162846,#162847,#162848,#162849,
#162850,#162851,#162852,#162853,#162854,#162855,#162856,#162857,#162858,
#162859,#162860,#162861,#162862,#162863,#162864,#162865,#162866,#162867,
#162868,#162869,#162870,#162871,#162872,#162873,#162874,#162875,#162876,
#162877,#162878,#162879,#162880,#162881,#162882,#162883,#162884,#162885,
#162886,#162887,#162888,#162889,#162890,#162891,#162892,#162893,#162894,
#162895,#162896,#162897,#162898,#162899,#162900,#162901,#162902,#162903,
#162904,#162905,#162906,#162907,#162908,#162909,#162910,#162911,#162912,
#162913,#162914,#162915,#162916,#162917,#162918,#162919,#162920,#162921,
#162922,#162923,#162924,#162925,#162926,#162927,#162928,#162929,#162930,
#162931,#162932,#162933,#162934,#162935,#162936,#162937,#162938,#162939,
#162940,#162941,#162942,#162943,#162944,#162945,#162946,#162947,#162948,
#162949,#162950,#162951,#162952,#162953,#162954,#162955,#162956,#162957,
#162958,#162959),.UNSPECIFIED.,.F.,.F.,(4,3,3,3,3,3,3,3,3,3,3,3,3,3,3,3,
3,3,3,3,3,3,3,3,3,3,3,3,3,3,3,3,3,3,3,3,3,3,3,3,3,3,3,3,3,3,3,3,3,3,3,3,
3,3,3,3,3,3,3,4),(-54.1065214908593,-53.9371682979412,-53.8337735608933,
-53.7305322787782,-53.6274123133859,-53.5243577451769,-53.4213345368191,
-53.3183086941466,-53.2151759273684,-53.1119868359586,-53.0086148425769,
-52.9383318479794,-52.8349371109313,-52.7316958288162,-52.6285758634238,
-52.5255212952148,-52.4224980868569,-52.3194722441843,-52.2163394774061,
-52.1131503859961,-52.0097783926143,-51.9394953980175,-51.8361006609696,
-51.7328593788547,-51.6297394134624,-51.5266848452536,-51.4236616368959,
-51.3206357942235,-51.2175030274454,-51.1143139360357,-51.0109419426541,
-50.9406589480556,-50.8372642110076,-50.7340229288926,-50.6309029635003,
-50.5278483952914,-50.4248251869336,-50.3217993442611,-50.218666577483,
-50.1154774860731,-50.0121054926915,-49.9418224980937,-49.8384277610458,
-49.7351864789307,-49.6320665135385,-49.5290119453296,-49.4259887369718,
-49.3229628942993,-49.2198301275212,-49.1166410361114,-49.0132690427297,
-48.9429860481318,-48.8396205066898,-48.7363953136868,-48.6332762150803,
-48.5302290794512,-48.4271932051626,-48.324164639594,-48.2210652728402,
-48.1740291001457),.UNSPECIFIED.);
#1736=B_SPLINE_CURVE_WITH_KNOTS('',3,(#162960,#162961,#162962,#162963),
 .UNSPECIFIED.,.F.,.F.,(4,4),(-54.4565131158552,-54.1065275198801),
 .UNSPECIFIED.);
#1737=B_SPLINE_CURVE_WITH_KNOTS('',3,(#162969,#162970,#162971,#162972,#162973,
#162974,#162975,#162976,#162977,#162978,#162979,#162980,#162981,#162982,
#162983,#162984,#162985,#162986,#162987,#162988),.UNSPECIFIED.,.F.,.F.,
(4,2,2,2,2,2,2,2,2,4),(2.59334882414752,2.59907506457794,2.60333221459039,
2.60586227935457,2.60780101189424,2.60987862294918,2.61314742471985,2.6169507883377,
2.62421563735964,2.66784423020342),.UNSPECIFIED.);
#1738=B_SPLINE_CURVE_WITH_KNOTS('',3,(#162989,#162990,#162991,#162992,#162993,
#162994,#162995,#162996,#162997,#162998,#162999,#163000,#163001,#163002,
#163003,#163004,#163005,#163006,#163007,#163008,#163009,#163010,#163011,
#163012,#163013,#163014,#163015,#163016,#163017,#163018,#163019,#163020,
#163021,#163022,#163023,#163024,#163025,#163026,#163027,#163028,#163029,
#163030,#163031,#163032,#163033,#163034,#163035,#163036,#163037,#163038,
#163039,#163040,#163041,#163042,#163043,#163044,#163045,#163046,#163047,
#163048,#163049,#163050,#163051,#163052,#163053,#163054,#163055,#163056,
#163057,#163058,#163059,#163060,#163061,#163062,#163063,#163064,#163065,
#163066,#163067,#163068,#163069,#163070,#163071,#163072,#163073,#163074,
#163075,#163076,#163077,#163078,#163079,#163080,#163081,#163082,#163083,
#163084,#163085,#163086,#163087,#163088,#163089,#163090,#163091,#163092,
#163093,#163094,#163095,#163096,#163097,#163098,#163099,#163100,#163101,
#163102,#163103,#163104,#163105,#163106,#163107,#163108,#163109,#163110,
#163111,#163112,#163113,#163114,#163115,#163116,#163117,#163118,#163119,
#163120,#163121,#163122,#163123,#163124,#163125,#163126,#163127,#163128,
#163129,#163130,#163131,#163132,#163133,#163134,#163135,#163136,#163137,
#163138,#163139,#163140,#163141,#163142,#163143,#163144,#163145,#163146,
#163147,#163148,#163149,#163150,#163151,#163152,#163153,#163154,#163155,
#163156,#163157,#163158,#163159,#163160,#163161,#163162,#163163,#163164,
#163165,#163166,#163167,#163168,#163169,#163170,#163171,#163172,#163173,
#163174,#163175,#163176,#163177,#163178,#163179,#163180,#163181,#163182,
#163183,#163184,#163185,#163186,#163187,#163188,#163189,#163190,#163191,
#163192,#163193,#163194,#163195,#163196,#163197,#163198,#163199,#163200,
#163201,#163202),.UNSPECIFIED.,.F.,.F.,(4,2,2,2,2,2,2,2,2,2,2,2,2,2,2,2,
2,2,2,2,2,2,2,2,2,2,2,2,2,2,2,2,2,2,2,2,2,2,2,2,2,2,2,2,2,2,2,2,2,2,2,2,
2,2,2,2,2,2,2,2,2,2,2,2,2,2,2,2,2,2,2,2,2,2,2,2,2,2,2,2,2,2,2,2,2,2,2,2,
2,2,2,2,2,2,2,2,2,2,2,2,2,2,2,2,2,2,4),(0.000649988335642877,0.0375152704990541,
0.0412926024578486,0.0433020294432964,0.0446072108356044,0.0458444142180878,
0.0469177266873797,0.0482917858053277,0.0511320544688072,0.0879796920395742,
0.109399124786516,0.136182092967779,0.146436026521021,0.149706920435959,
0.15178501628728,0.153723612827992,0.156252658605983,0.16050625487588,0.193185552789801,
0.222555354354387,0.244174106165292,0.254295247008305,0.256485228349918,
0.25773337791172,0.258805379538652,0.260163839407445,0.262835887780087,
0.280216640231541,0.329255233688801,0.347302837500602,0.354572268411801,
0.360002060810804,0.36256744550423,0.364504808798455,0.366332959206393,
0.368880882447617,0.375561602311507,0.430977353873264,0.455320875693043,
0.466218627605919,0.468466956050601,0.469718065506778,0.470789816457095,
0.472144378813639,0.47488629622175,0.493335007454673,0.537461269541001,
0.565331974112842,0.571665382296963,0.574357002609424,0.576315561046172,
0.578111702417444,0.580996264298724,0.58800001788294,0.639383010169877,
0.666515187811272,0.678128410926827,0.680418181092506,0.681678325206265,
0.682749329532794,0.684092177014792,0.686691244963384,0.702216369315421,
0.708761471480629,0.722633921401398,0.755493983493896,0.77205648267286,
0.782367905406938,0.785616709426293,0.787690091313945,0.789630826090766,
0.792172071500364,0.79646722690795,0.831578348115309,0.880465471459157,
0.890288659601052,0.892468517871547,0.893704749634407,0.89477845082597,
0.896154615331692,0.899004743368698,0.935374677289219,0.989163075558435,
0.995619128476982,0.998331696209567,1.00029419032283,1.00208616374467,1.00494709012616,
1.01180636960978,1.06524497318811,1.090935227857,1.10218662724822,1.10445604494005,
1.10571185352532,1.10678333809307,1.10813209108801,1.110758156089,1.12692234086465,
1.17758033537424,1.2019943210918,1.20789434186422,1.21051040626931,1.21245610456172,
1.21427050097894,1.21676510975846,1.22311495397694,1.25968344386625),
 .UNSPECIFIED.);
#1739=B_SPLINE_CURVE_WITH_KNOTS('',3,(#163204,#163205,#163206,#163207,#163208,
#163209,#163210,#163211,#163212,#163213),.UNSPECIFIED.,.F.,.F.,(4,1,1,1,
1,1,1,4),(-60.3897037700897,-59.9301869977125,-58.9313505477506,-57.9325140977887,
-56.9336776478269,-55.934841197865,-54.9360047479031,-54.4565131158552),
 .UNSPECIFIED.);
#1740=B_SPLINE_CURVE_WITH_KNOTS('',3,(#163214,#163215,#163216,#163217,#163218,
#163219,#163220,#163221,#163222,#163223,#163224,#163225,#163226,#163227,
#163228,#163229,#163230,#163231),.UNSPECIFIED.,.F.,.F.,(4,2,2,2,2,2,2,2,
4),(0.000658789415650989,0.00332970172644197,0.0059216589075676,0.00778879691858933,
0.00964368950037614,0.0114909185893229,0.0146445375726767,0.0233614964880355,
0.0750722492145438),.UNSPECIFIED.);
#1741=B_SPLINE_CURVE_WITH_KNOTS('',3,(#163236,#163237,#163238,#163239,#163240,
#163241,#163242,#163243,#163244,#163245,#163246,#163247,#163248,#163249,
#163250,#163251,#163252,#163253,#163254,#163255,#163256,#163257,#163258,
#163259,#163260,#163261,#163262,#163263,#163264,#163265,#163266,#163267,
#163268,#163269,#163270,#163271,#163272,#163273,#163274,#163275,#163276,
#163277,#163278,#163279,#163280,#163281,#163282,#163283,#163284,#163285,
#163286,#163287,#163288,#163289,#163290,#163291,#163292,#163293,#163294,
#163295,#163296,#163297,#163298,#163299,#163300,#163301,#163302,#163303,
#163304,#163305,#163306,#163307,#163308,#163309,#163310,#163311,#163312,
#163313,#163314,#163315,#163316,#163317,#163318,#163319,#163320,#163321,
#163322,#163323,#163324,#163325,#163326,#163327,#163328,#163329,#163330,
#163331,#163332,#163333,#163334,#163335,#163336,#163337,#163338,#163339,
#163340,#163341,#163342,#163343,#163344,#163345,#163346,#163347,#163348,
#163349,#163350,#163351,#163352,#163353,#163354,#163355,#163356,#163357,
#163358,#163359,#163360,#163361,#163362,#163363,#163364,#163365,#163366,
#163367,#163368,#163369,#163370,#163371,#163372,#163373,#163374,#163375,
#163376,#163377,#163378,#163379,#163380,#163381,#163382,#163383,#163384,
#163385,#163386,#163387,#163388,#163389,#163390,#163391,#163392,#163393,
#163394,#163395,#163396,#163397,#163398,#163399,#163400,#163401,#163402,
#163403,#163404,#163405,#163406,#163407,#163408,#163409,#163410,#163411,
#163412,#163413,#163414,#163415,#163416,#163417,#163418,#163419,#163420,
#163421,#163422,#163423,#163424,#163425,#163426,#163427,#163428,#163429,
#163430,#163431,#163432,#163433,#163434,#163435,#163436,#163437,#163438,
#163439,#163440,#163441,#163442,#163443,#163444,#163445,#163446,#163447,
#163448,#163449,#163450,#163451,#163452,#163453,#163454,#163455,#163456,
#163457),.UNSPECIFIED.,.F.,.F.,(4,2,2,2,2,2,2,2,2,2,2,2,2,2,2,2,2,2,2,2,
2,2,2,2,2,2,2,2,2,2,2,2,2,2,2,2,2,2,2,2,2,2,2,2,2,2,2,2,2,2,2,2,2,2,2,2,
2,2,2,2,2,2,2,2,2,2,2,2,2,2,2,2,2,2,2,2,2,2,2,2,2,2,2,2,2,2,2,2,2,2,2,2,
2,2,2,2,2,2,2,2,2,2,2,2,2,2,2,2,2,2,4),(1.25996006495675,1.28597380944536,
1.32674485088401,1.33181142606065,1.33427121096303,1.33619431271336,1.33832607326192,
1.34183902862498,1.35471582196281,1.37741958663076,1.41601236368063,1.42100702049356,
1.43701511615223,1.439634657082,1.44098193712491,1.44205323813183,1.44330998086227,
1.44558399481097,1.45691813035294,1.48293120542186,1.53585432794066,1.54275018415212,
1.54561697653284,1.54740990675929,1.54937126959613,1.55207826794206,1.55850204924136,
1.58712802854869,1.6384137574983,1.64947627869533,1.65162341522331,1.65297992887205,
1.65405190176624,1.65530175680869,1.65754404067806,1.6683401259638,1.69230181102095,
1.7482595273408,1.75488535343838,1.75742482539986,1.75925083788514,1.76118954825343,
1.7637628543973,1.76942781234478,1.79207264981186,1.82489292604725,1.82936666735762,
1.86060995899561,1.86352206217553,1.86491022324517,1.86598498575407,1.86721315325864,
1.86935685212576,1.87866697764114,1.92781063757243,1.96318650993906,1.96748434638255,
1.97002624300663,1.97196692592091,1.97403971921933,1.97728648697316,1.98758198063248,
2.00411220184513,2.03697136145416,2.0485222492667,2.0580882762403,2.07304463335334,
2.07539212821845,2.07679360363977,2.0778727343703,2.07907911818313,2.08112476943751,
2.08918051648865,2.10435470460193,2.14436455266355,2.17524266362502,2.17945964517444,
2.18197798267303,2.18391481249275,2.18599733515636,2.18928858714235,2.19997838021427,
2.21739013031273,2.25491166888488,2.28448034825575,2.28739436561197,2.2887828350069,
2.28985755825139,2.29108537004048,2.29322772015703,2.30252074880178,2.32135992475989,
2.3691444305163,2.38804715265221,2.39179672343498,2.39420162815337,2.39611860978283,
2.39828237714473,2.40194076057161,2.41628811257928,2.46674887119079,2.49644856364972,
2.49936273260099,2.50075125350221,2.50182600707965,2.50305384286103,2.50434565237812,
2.50899003897626,2.53312554767631,2.55402964662815,2.59334882414752),
 .UNSPECIFIED.);
#1742=B_SPLINE_CURVE_WITH_KNOTS('',3,(#163458,#163459,#163460,#163461,#163462,
#163463,#163464,#163465,#163466,#163467,#163468,#163469,#163470,#163471,
#163472,#163473,#163474,#163475,#163476,#163477,#163478,#163479,#163480,
#163481,#163482,#163483,#163484,#163485,#163486,#163487,#163488,#163489,
#163490,#163491,#163492,#163493,#163494,#163495,#163496,#163497,#163498,
#163499,#163500,#163501,#163502,#163503,#163504,#163505,#163506,#163507,
#163508,#163509,#163510,#163511,#163512,#163513,#163514,#163515,#163516,
#163517,#163518,#163519,#163520,#163521,#163522,#163523,#163524,#163525,
#163526,#163527,#163528,#163529,#163530,#163531,#163532,#163533,#163534,
#163535,#163536,#163537,#163538,#163539,#163540,#163541,#163542,#163543,
#163544,#163545,#163546,#163547,#163548,#163549,#163550,#163551,#163552,
#163553,#163554,#163555,#163556,#163557,#163558,#163559,#163560,#163561,
#163562,#163563,#163564,#163565,#163566,#163567,#163568,#163569,#163570,
#163571,#163572,#163573,#163574,#163575,#163576,#163577,#163578,#163579,
#163580,#163581,#163582,#163583,#163584,#163585,#163586,#163587,#163588,
#163589,#163590,#163591,#163592,#163593,#163594,#163595,#163596,#163597,
#163598,#163599,#163600,#163601,#163602,#163603,#163604,#163605,#163606,
#163607,#163608,#163609,#163610,#163611,#163612,#163613,#163614,#163615,
#163616,#163617,#163618,#163619,#163620,#163621,#163622,#163623,#163624,
#163625,#163626,#163627,#163628,#163629,#163630,#163631,#163632,#163633,
#163634,#163635,#163636,#163637,#163638,#163639,#163640,#163641,#163642,
#163643,#163644,#163645,#163646,#163647,#163648,#163649,#163650,#163651,
#163652,#163653,#163654,#163655,#163656,#163657,#163658,#163659,#163660,
#163661,#163662,#163663,#163664,#163665,#163666,#163667,#163668,#163669,
#163670,#163671,#163672,#163673,#163674,#163675,#163676,#163677,#163678,
#163679,#163680,#163681,#163682,#163683,#163684,#163685,#163686,#163687,
#163688,#163689),.UNSPECIFIED.,.F.,.F.,(4,2,2,2,2,2,2,2,2,2,2,2,2,2,2,2,
2,2,2,2,2,2,2,2,2,2,2,2,2,2,2,2,2,2,2,2,2,2,2,2,2,2,2,2,2,2,2,2,2,2,2,2,
2,2,2,2,2,2,2,2,2,2,2,2,2,2,2,2,2,2,2,2,2,2,2,2,2,2,2,2,2,2,2,2,2,2,2,2,
2,2,2,2,2,2,2,2,2,2,2,2,2,2,2,2,2,2,2,2,2,2,2,2,2,2,2,4),(0.0750722492145438,
0.089273883774724,0.108736238450361,0.112675312821005,0.114244472673274,
0.115347616226248,0.116358705151943,0.118025380652166,0.122269071395783,
0.177793694177577,0.20980237985404,0.214435981151818,0.217207823473553,
0.219715316432243,0.221616785883321,0.223439946924427,0.225968447943757,
0.23252618265342,0.289135495830322,0.312706921624991,0.323396188599504,
0.325632024315669,0.326880500483277,0.327952665500023,0.329311181849471,
0.331982887691663,0.349344799089393,0.367622576687107,0.400551307754336,
0.417194792829087,0.427543042342775,0.430796238022716,0.432870694703231,
0.434811223168959,0.437350451056223,0.441638284565254,0.476878520823009,
0.526123759127554,0.535534348299561,0.537685601829783,0.53891560030055,
0.539990347196359,0.541376346694768,0.544276404838197,0.571047910819831,
0.604901022440056,0.634235374311171,0.640744266195993,0.643465965726574,
0.645430367194715,0.647220865877107,0.650072482212639,0.656873699709213,
0.711030798235968,0.736238318680125,0.747365576963437,0.749628025633159,
0.750882442839031,0.751954244112297,0.753305315181373,0.755941569721024,
0.772353473841486,0.822423716415776,0.840492796456449,0.85147298973827,
0.854796816312565,0.856886996706432,0.858822060696727,0.861325554531746,
0.86549026163651,0.894122056722588,0.947186140854307,0.959329892388681,
0.961648912215588,0.962915634525559,0.963986564537474,0.965322182956684,
0.967400428234967,0.977395418297254,0.98298968078243,0.992387406060152,
1.00395842269926,1.0368083948603,1.05335110980195,1.06365451181599,1.06690307695976,
1.06897685660727,1.07091835030893,1.0734611474474,1.07776017657869,1.11307373987275,
1.16233282766085,1.17167136585897,1.17381782426907,1.17504695403105,1.17612216086331,
1.1775103606059,1.1804206757723,1.20855458469213,1.24824747237768,1.26519455449022,
1.27568027571575,1.27894981726275,1.28102832364675,1.28296818879352,1.28550015870478,
1.28976149589151,1.33476567404375,1.379821053785,1.38454671693276,1.3862891876652,
1.38731528140148,1.38840808509425,1.38991874143622,1.39350070371916,1.40892859190044),
 .UNSPECIFIED.);
#1743=B_SPLINE_CURVE_WITH_KNOTS('',3,(#163695,#163696,#163697,#163698,#163699),
 .UNSPECIFIED.,.F.,.F.,(4,1,4),(76.7075601022117,76.9104066470643,77.0584304498949),
 .UNSPECIFIED.);
#1744=B_SPLINE_CURVE_WITH_KNOTS('',3,(#163700,#163701,#163702,#163703,#163704,
#163705,#163706,#163707,#163708,#163709,#163710,#163711,#163712,#163713,
#163714,#163715,#163716,#163717,#163718,#163719,#163720,#163721,#163722,
#163723,#163724,#163725,#163726,#163727,#163728,#163729,#163730,#163731,
#163732,#163733,#163734,#163735,#163736,#163737,#163738,#163739,#163740,
#163741,#163742,#163743,#163744,#163745,#163746,#163747,#163748,#163749,
#163750,#163751,#163752,#163753,#163754,#163755,#163756,#163757,#163758,
#163759,#163760,#163761,#163762,#163763,#163764,#163765,#163766,#163767,
#163768,#163769,#163770,#163771,#163772,#163773,#163774,#163775,#163776,
#163777,#163778,#163779,#163780,#163781,#163782,#163783,#163784,#163785,
#163786,#163787,#163788,#163789,#163790,#163791,#163792,#163793,#163794,
#163795,#163796,#163797,#163798,#163799,#163800,#163801,#163802,#163803,
#163804,#163805,#163806,#163807,#163808,#163809,#163810,#163811,#163812,
#163813,#163814,#163815,#163816,#163817,#163818,#163819,#163820,#163821,
#163822,#163823,#163824,#163825,#163826,#163827,#163828,#163829,#163830,
#163831,#163832,#163833,#163834,#163835,#163836,#163837,#163838,#163839,
#163840,#163841,#163842,#163843,#163844,#163845,#163846,#163847,#163848,
#163849,#163850,#163851,#163852,#163853,#163854,#163855,#163856,#163857,
#163858,#163859,#163860,#163861,#163862,#163863,#163864,#163865,#163866,
#163867,#163868,#163869,#163870,#163871,#163872,#163873,#163874,#163875,
#163876,#163877,#163878,#163879,#163880,#163881,#163882,#163883,#163884,
#163885,#163886,#163887,#163888,#163889,#163890,#163891,#163892,#163893,
#163894,#163895,#163896,#163897,#163898,#163899,#163900,#163901,#163902,
#163903,#163904,#163905,#163906,#163907,#163908,#163909,#163910,#163911,
#163912,#163913,#163914,#163915,#163916,#163917,#163918,#163919),
 .UNSPECIFIED.,.F.,.F.,(4,2,2,2,2,2,2,2,2,2,2,2,2,2,2,2,2,2,2,2,2,2,2,2,
2,2,2,2,2,2,2,2,2,2,2,2,2,2,2,2,2,2,2,2,2,2,2,2,2,2,2,2,2,2,2,2,2,2,2,2,
2,2,2,2,2,2,2,2,2,2,2,2,2,2,2,2,2,2,2,2,2,2,2,2,2,2,2,2,2,2,2,2,2,2,2,2,
2,2,2,2,2,2,2,2,2,2,2,2,2,4),(0.000629226549544607,0.046842092175668,0.0541657575285493,
0.0579911612059392,0.0612752544363508,0.0633561305284231,0.0652934283883815,
0.0678152242493139,0.0720443245894624,0.118700329279881,0.138793897037419,
0.156963094474695,0.166022017532338,0.168062688078218,0.169315730423518,
0.1703871574697,0.171738779642116,0.174379144044047,0.190917543624233,0.199764859285149,
0.243742949382162,0.259907590363103,0.269996325263167,0.273243717522023,
0.27531653418407,0.277256975786934,0.279798177711421,0.284094022729987,
0.319313332422387,0.368562126872632,0.377950976793733,0.38010027972992,
0.381329644954602,0.382404151719005,0.383790254026362,0.386035372754029,
0.398844428626804,0.401655625631889,0.40593911242359,0.448927943809981,
0.47686676063002,0.483208308591596,0.485901261068954,0.487860007173649,
0.48965577917277,0.49253855924609,0.499531921315542,0.551066850555209,0.578088456860946,
0.589674282153311,0.591962469797789,0.593222244789865,0.594293237545087,
0.595636453608052,0.598237350724384,0.61380689768479,0.620262240882701,
0.661679829577953,0.688953552007046,0.695214266325076,0.697893453563024,
0.699849814058667,0.70164870862721,0.704548219403095,0.711641621297567,
0.761302991780524,0.799617001575597,0.803221546299077,0.804735597480476,
0.805828574784582,0.806853018956235,0.808588829136208,0.813273992121576,
0.854358207744742,0.900791019632297,0.907183313454101,0.909885000778856,
0.911845419513227,0.913639493175818,0.916512478861638,0.923445809804724,
0.975895767454485,1.00227120613405,1.01369641930391,1.01597568328913,1.01723357649087,
1.01830480150809,1.01965063653427,1.02226341151027,1.03811575328452,1.0428600613946,
1.05813888688782,1.09101631580087,1.10759893567686,1.11791955846622,1.12116949240115,
1.12324317073249,1.12518388478307,1.12772467291816,1.13201809166524,1.17442090269835,
1.20348006573086,1.22309714942415,1.22705256328181,1.22862432579257,1.22972797012696,
1.2307384947667,1.2324022084367,1.2366275620297,1.25996006495675),
 .UNSPECIFIED.);
#1745=B_SPLINE_CURVE_WITH_KNOTS('',3,(#163921,#163922,#163923,#163924,#163925,
#163926,#163927,#163928,#163929,#163930,#163931,#163932,#163933,#163934,
#163935,#163936,#163937,#163938,#163939,#163940,#163941,#163942,#163943,
#163944,#163945,#163946,#163947,#163948,#163949,#163950,#163951,#163952,
#163953,#163954,#163955,#163956,#163957,#163958,#163959,#163960,#163961,
#163962,#163963,#163964,#163965,#163966,#163967,#163968,#163969,#163970,
#163971,#163972,#163973,#163974,#163975,#163976,#163977,#163978,#163979,
#163980,#163981,#163982,#163983,#163984,#163985,#163986,#163987,#163988,
#163989,#163990,#163991,#163992,#163993,#163994,#163995,#163996,#163997,
#163998,#163999,#164000,#164001,#164002,#164003,#164004,#164005,#164006,
#164007,#164008,#164009,#164010,#164011,#164012,#164013,#164014,#164015,
#164016,#164017,#164018,#164019,#164020,#164021,#164022,#164023,#164024,
#164025,#164026,#164027,#164028,#164029,#164030,#164031,#164032,#164033,
#164034,#164035,#164036,#164037,#164038,#164039,#164040,#164041,#164042,
#164043,#164044,#164045,#164046,#164047,#164048,#164049,#164050,#164051,
#164052,#164053,#164054,#164055,#164056,#164057,#164058,#164059,#164060,
#164061,#164062,#164063,#164064,#164065,#164066,#164067,#164068,#164069,
#164070,#164071,#164072,#164073,#164074,#164075,#164076,#164077,#164078,
#164079,#164080,#164081,#164082,#164083,#164084,#164085,#164086,#164087,
#164088,#164089,#164090,#164091,#164092,#164093,#164094,#164095,#164096,
#164097,#164098,#164099,#164100,#164101,#164102,#164103,#164104,#164105,
#164106,#164107,#164108,#164109,#164110,#164111,#164112,#164113,#164114,
#164115,#164116,#164117,#164118,#164119,#164120,#164121,#164122,#164123,
#164124,#164125,#164126,#164127,#164128,#164129,#164130,#164131,#164132,
#164133,#164134,#164135,#164136,#164137,#164138,#164139,#164140,#164141,
#164142,#164143,#164144,#164145,#164146),.UNSPECIFIED.,.F.,.F.,(4,2,2,2,
2,2,2,2,2,2,2,2,2,2,2,2,2,2,2,2,2,2,2,2,2,2,2,2,2,2,2,2,2,2,2,2,2,2,2,2,
2,2,2,2,2,2,2,2,2,2,2,2,2,2,2,2,2,2,2,2,2,2,2,2,2,2,2,2,2,2,2,2,2,2,2,2,
2,2,2,2,2,2,2,2,2,2,2,2,2,2,2,2,2,2,2,2,2,2,2,2,2,2,2,2,2,2,2,2,2,2,2,2,
4),(1.40892859190044,1.43114189525,1.48156963760009,1.48862884966623,1.49152354603348,
1.49332221530073,1.49528052898801,1.49796636219948,1.50426089205288,1.5318023820529,
1.56020878468567,1.58254081662385,1.59524891900965,1.59748968510969,1.59887485677546,
1.59994976947127,1.60118087293459,1.60333620221715,1.61279870529294,1.66198861182054,
1.69719664481167,1.70149430577838,1.70403678888311,1.70597831701588,1.70805239834854,
1.71130198785045,1.721613202209,1.73817510452622,1.77107000802575,1.78480619463583,
1.79167956450897,1.79189418137142,1.79536650019118,1.80737171117298,1.80957450844001,
1.81094817097448,1.81202190509395,1.81326043127816,1.81544975243714,1.825407228245,
1.87417264068421,1.90924350060804,1.91353909054562,1.91608088179307,1.91802218880617,
1.92009633181582,1.92334664001236,1.93366537978797,1.95024436120885,1.98315211084013,
1.99823835888684,2.0031473962221,2.01907406400683,2.02168979752071,2.0230364933786,
2.02410805362961,2.02536594006684,2.02764416092539,2.03904333943293,2.06530752573197,
2.11789890057591,2.12482260230917,2.12769449841476,2.1294887402672,2.13145002916269,
2.13415416338517,2.14055810834717,2.1493891515329,2.20069624065193,2.23073837411376,
2.23364986311164,2.23503820339814,2.23611332207084,2.2373421398203,2.23948754375142,
2.24881389940775,2.29801565533926,2.33335075691658,2.33764950756903,2.34019213947976,
2.34213349578752,2.34420711688365,2.34745540783189,2.35775763847839,2.37430048861872,
2.40717708608884,2.44285422472894,2.44571910689232,2.44709832297037,2.4481380605453,
2.44933265324992,2.45060555987713,2.45253662007598,2.4561069498846,2.46455680718911,
2.52380836385539,2.54607880918444,2.55001381715811,2.55247565713357,2.55439930196016,
2.55653057598231,2.56004021933743,2.57287658598738,2.5954737366041,2.64831919803709,
2.65619097239154,2.65828700262456,2.65951699757958,2.66057382320596,2.66161973450024,
2.66297018535776,2.66542827555432,2.66852198484313),.UNSPECIFIED.);
#1746=B_SPLINE_CURVE_WITH_KNOTS('',3,(#164147,#164148,#164149,#164150,#164151,
#164152),.UNSPECIFIED.,.F.,.F.,(4,2,4),(0.000817339722073156,0.0612254310813656,
0.0752219538553924),.UNSPECIFIED.);
#1747=B_SPLINE_CURVE_WITH_KNOTS('',3,(#164158,#164159,#164160,#164161,#164162,
#164163,#164164,#164165,#164166,#164167,#164168,#164169,#164170),
 .UNSPECIFIED.,.F.,.F.,(4,3,3,3,4),(82.9907456874083,83.0928761471772,83.1948834239356,
83.2967928187794,83.3413405014001),.UNSPECIFIED.);
#1748=B_SPLINE_CURVE_WITH_KNOTS('',3,(#164171,#164172,#164173,#164174,#164175,
#164176,#164177,#164178,#164179,#164180),.UNSPECIFIED.,.F.,.F.,(4,1,1,1,
1,1,1,4),(77.0584304498949,77.9092430970262,78.9080795469881,79.90691599695,
80.9057524469118,81.9045888968737,82.9034253468356,82.9907454093913),
 .UNSPECIFIED.);
#1749=B_SPLINE_CURVE_WITH_KNOTS('',3,(#164181,#164182,#164183,#164184,#164185,
#164186,#164187,#164188,#164189,#164190,#164191,#164192,#164193,#164194,
#164195,#164196,#164197,#164198,#164199,#164200,#164201,#164202,#164203,
#164204,#164205,#164206,#164207,#164208,#164209,#164210,#164211,#164212,
#164213,#164214,#164215,#164216,#164217,#164218,#164219,#164220,#164221,
#164222,#164223,#164224,#164225,#164226,#164227,#164228,#164229,#164230,
#164231,#164232,#164233,#164234,#164235,#164236,#164237,#164238,#164239,
#164240,#164241,#164242,#164243,#164244,#164245,#164246,#164247,#164248,
#164249,#164250,#164251,#164252,#164253,#164254,#164255,#164256,#164257,
#164258,#164259,#164260,#164261,#164262,#164263,#164264,#164265,#164266,
#164267,#164268,#164269,#164270,#164271,#164272,#164273,#164274,#164275,
#164276,#164277,#164278,#164279,#164280,#164281,#164282,#164283,#164284,
#164285,#164286,#164287,#164288,#164289,#164290,#164291,#164292,#164293,
#164294,#164295,#164296,#164297,#164298,#164299,#164300,#164301,#164302,
#164303,#164304,#164305,#164306,#164307,#164308,#164309,#164310,#164311,
#164312,#164313,#164314,#164315,#164316,#164317,#164318,#164319,#164320,
#164321,#164322,#164323,#164324,#164325,#164326,#164327,#164328,#164329,
#164330,#164331,#164332,#164333,#164334,#164335,#164336,#164337,#164338,
#164339,#164340,#164341,#164342,#164343,#164344,#164345,#164346,#164347,
#164348,#164349,#164350,#164351,#164352,#164353,#164354,#164355,#164356,
#164357,#164358,#164359,#164360,#164361,#164362,#164363,#164364,#164365,
#164366,#164367,#164368,#164369,#164370,#164371,#164372,#164373,#164374,
#164375,#164376,#164377,#164378,#164379,#164380,#164381,#164382,#164383,
#164384,#164385,#164386,#164387,#164388,#164389,#164390,#164391,#164392,
#164393,#164394,#164395,#164396,#164397,#164398,#164399,#164400,#164401,
#164402,#164403,#164404,#164405,#164406,#164407,#164408,#164409,#164410,
#164411,#164412,#164413,#164414,#164415,#164416,#164417,#164418,#164419,
#164420,#164421,#164422,#164423,#164424,#164425,#164426,#164427,#164428,
#164429,#164430,#164431,#164432,#164433,#164434,#164435,#164436,#164437,
#164438,#164439,#164440,#164441,#164442,#164443,#164444,#164445,#164446,
#164447,#164448,#164449,#164450,#164451,#164452),.UNSPECIFIED.,.F.,.F.,
(4,2,2,2,2,2,2,2,2,2,2,2,2,2,2,2,2,2,2,2,2,2,2,2,2,2,2,2,2,2,2,2,2,2,2,
2,2,2,2,2,2,2,2,2,2,2,2,2,2,2,2,2,2,2,2,2,2,2,2,2,2,2,2,2,2,2,2,2,2,2,2,
2,2,2,2,2,2,2,2,2,2,2,2,2,2,2,2,2,2,2,2,2,2,2,2,2,2,2,2,2,2,2,2,2,2,2,2,
2,2,2,2,2,2,2,2,2,2,2,2,2,2,2,2,2,2,2,2,2,2,2,2,2,2,2,2,4),(0.0752219538553924,
0.0876737708541335,0.0938318742109832,0.0964929811556149,0.0984458548898336,
0.100248360570854,0.103168886737211,0.110389679589265,0.154249340375915,
0.195394743117652,0.199213037433027,0.201237853233969,0.202549373332438,
0.203773000142621,0.203776566961232,0.20378014633625,0.203783738344437,
0.203787576062818,0.203791475620769,0.203795438321307,0.203799465536059,
0.203803558471933,0.203807718709299,0.203811947684853,0.203816246902364,
0.203820618031701,0.203825062595836,0.20382958214438,0.203834178495644,
0.20383885333795,0.203843608503851,0.203848445798754,0.204892188634865,
0.206274906167045,0.209159727727915,0.243329463902013,0.277571728409199,
0.294126608529013,0.304434011130635,0.307681933460342,0.309754845148587,
0.311695204779934,0.314236052710389,0.318530746432302,0.353665860888674,
0.402638504555908,0.412346629803975,0.414518311734997,0.415752592306471,
0.416826320029807,0.418204770135486,0.421067385718614,0.45674511001175,
0.48957118273493,0.506095244510139,0.516388962923495,0.519635506027736,
0.521708242933433,0.523648934759903,0.526190933368832,0.530489176948989,
0.565878123660799,0.615047144328223,0.624359823472386,0.626503768937628,
0.627732011539939,0.628806801992257,0.630194938639619,0.633106794523024,
0.664374889134527,0.698027864840962,0.716835852182718,0.728133512349959,
0.731490771685652,0.733588042679064,0.735520217769766,0.738006767535329,
0.742114736855211,0.76858503955736,0.82369449053593,0.836025073979104,0.838353481940201,
0.839622072387379,0.840692655893767,0.842025423707611,0.844094869680189,
0.853967703999288,0.859546786547861,0.8599910416698,0.866878668556703,0.880605864107274,
0.913468555540373,0.930031312953361,0.940343208578569,0.943592327683018,
0.945665950564827,0.947606938949967,0.950148556885713,0.954444432580003,
0.989573379916252,1.03850731938857,1.04828346516449,1.05046030904877,1.05169597405116,
1.05276991396152,1.05414733960082,1.05700336173895,1.07978617932669,1.09263096531517,
1.12548858440065,1.14204277479925,1.15235109418109,1.15560002206625,1.15767374778362,
1.15961499040838,1.16215716922543,1.16645450396551,1.20166389770812,1.25084883176782,
1.26033868215133,1.26249578897222,1.26372719167067,1.26480190722889,1.26618621191743,
1.26907693598538,1.29478181286462,1.33423137066986,1.36195679610043,1.36609770007442,
1.36859435658635,1.37052854731926,1.37262217691922,1.37596096942245,1.38707796583593,
1.40546485002873,1.40868741081837),.UNSPECIFIED.);
#1750=B_SPLINE_CURVE_WITH_KNOTS('',3,(#164458,#164459,#164460,#164461,#164462,
#164463,#164464,#164465,#164466,#164467,#164468,#164469,#164470,#164471,
#164472,#164473,#164474,#164475,#164476,#164477,#164478,#164479,#164480,
#164481,#164482,#164483),.UNSPECIFIED.,.F.,.F.,(4,2,2,2,2,2,2,2,2,2,2,2,
4),(2.59401617871736,2.61331896027604,2.62543797507626,2.62726567564924,
2.62826739459209,2.63695713257526,2.64010895985652,2.64195641923086,2.64381178633705,
2.64568025361034,2.64808223741416,2.65182298569027,2.66845987342429),
 .UNSPECIFIED.);
#1751=B_SPLINE_CURVE_WITH_KNOTS('',3,(#164484,#164485,#164486,#164487,#164488,
#164489,#164490,#164491,#164492,#164493,#164494,#164495,#164496,#164497,
#164498,#164499,#164500,#164501,#164502,#164503,#164504,#164505,#164506,
#164507,#164508,#164509,#164510,#164511,#164512,#164513,#164514,#164515,
#164516,#164517,#164518,#164519,#164520,#164521,#164522,#164523,#164524,
#164525,#164526,#164527,#164528,#164529,#164530,#164531,#164532,#164533,
#164534,#164535,#164536,#164537,#164538,#164539,#164540,#164541,#164542,
#164543,#164544,#164545,#164546,#164547,#164548,#164549,#164550,#164551,
#164552,#164553,#164554,#164555,#164556,#164557,#164558,#164559,#164560,
#164561,#164562,#164563,#164564,#164565,#164566,#164567,#164568,#164569,
#164570,#164571,#164572,#164573,#164574,#164575,#164576,#164577,#164578,
#164579,#164580,#164581,#164582,#164583,#164584,#164585,#164586,#164587,
#164588,#164589,#164590,#164591,#164592,#164593,#164594,#164595,#164596,
#164597,#164598,#164599,#164600,#164601,#164602,#164603,#164604,#164605,
#164606,#164607,#164608,#164609,#164610,#164611,#164612,#164613,#164614,
#164615,#164616,#164617,#164618,#164619,#164620,#164621,#164622,#164623,
#164624,#164625,#164626,#164627,#164628,#164629,#164630,#164631,#164632,
#164633,#164634,#164635,#164636,#164637,#164638,#164639,#164640,#164641,
#164642,#164643,#164644,#164645,#164646,#164647,#164648,#164649,#164650,
#164651,#164652,#164653,#164654,#164655,#164656,#164657,#164658,#164659,
#164660,#164661,#164662,#164663,#164664),.UNSPECIFIED.,.F.,.F.,(4,3,3,3,
3,3,3,3,3,3,3,3,3,3,3,3,3,3,3,3,3,3,3,3,3,3,3,3,3,3,3,3,3,3,3,3,3,3,3,3,
3,3,3,3,3,3,3,3,3,3,3,3,3,3,3,3,3,3,3,3,4),(83.3413405014001,83.4431911867645,
83.5450420715455,83.6469949427505,83.7490047344159,83.8511878793355,83.9022617967974,
84.0056565338454,84.1088978159603,84.2120177813527,84.3150723495616,84.4180955579194,
84.521121400592,84.6242541673701,84.7274432587799,84.8308152521616,84.9010982467593,
85.0044929838071,85.1077342659222,85.2108542313145,85.3139087995234,85.4169320078811,
85.5199578505539,85.6230906173319,85.7262797087418,85.8296517021234,85.8999346967212,
86.0033294337692,86.1065707158841,86.2096906812764,86.3127452494853,86.4157684578429,
86.518794300515,86.6219270672931,86.7251161587029,86.8284881520845,86.8987711466831,
87.0021658837311,87.1054071658464,87.2085271312386,87.3115816994476,87.4146049078053,
87.5176307504778,87.6207635172559,87.7239526086657,87.8273246020474,87.897607596645,
88.0010023336929,88.1042436158081,88.2073635812004,88.3104181494092,88.4134413577667,
88.5164672004388,88.6195999672169,88.7227890586266,88.8261610520081,88.8964440466068,
89.0132269961635,89.1295586830743,89.2451399878357,89.2739307161836),
 .UNSPECIFIED.);
#1752=B_SPLINE_CURVE_WITH_KNOTS('',3,(#164666,#164667,#164668,#164669,#164670,
#164671,#164672,#164673,#164674,#164675,#164676,#164677,#164678,#164679,
#164680,#164681,#164682,#164683,#164684,#164685,#164686,#164687,#164688,
#164689,#164690,#164691,#164692,#164693,#164694,#164695,#164696,#164697,
#164698,#164699,#164700,#164701,#164702,#164703,#164704,#164705,#164706,
#164707,#164708,#164709,#164710,#164711,#164712,#164713,#164714,#164715,
#164716,#164717,#164718,#164719,#164720,#164721,#164722,#164723,#164724,
#164725,#164726,#164727,#164728,#164729,#164730,#164731,#164732,#164733,
#164734,#164735,#164736,#164737,#164738,#164739,#164740,#164741,#164742,
#164743,#164744,#164745,#164746,#164747,#164748,#164749,#164750,#164751,
#164752,#164753,#164754,#164755,#164756,#164757,#164758,#164759,#164760,
#164761,#164762,#164763,#164764,#164765,#164766,#164767,#164768,#164769,
#164770,#164771,#164772,#164773,#164774,#164775,#164776,#164777,#164778,
#164779,#164780,#164781,#164782,#164783,#164784,#164785,#164786,#164787,
#164788,#164789,#164790,#164791,#164792,#164793,#164794,#164795,#164796,
#164797,#164798,#164799,#164800,#164801,#164802,#164803,#164804,#164805,
#164806,#164807,#164808,#164809,#164810,#164811,#164812,#164813,#164814,
#164815,#164816,#164817,#164818,#164819,#164820,#164821,#164822,#164823,
#164824,#164825,#164826,#164827,#164828,#164829,#164830,#164831,#164832,
#164833,#164834,#164835,#164836,#164837,#164838,#164839,#164840,#164841,
#164842,#164843,#164844,#164845,#164846,#164847,#164848,#164849,#164850,
#164851,#164852,#164853,#164854,#164855,#164856,#164857,#164858,#164859,
#164860,#164861,#164862,#164863,#164864,#164865,#164866,#164867,#164868,
#164869,#164870,#164871,#164872,#164873,#164874,#164875,#164876,#164877,
#164878,#164879,#164880,#164881,#164882,#164883),.UNSPECIFIED.,.F.,.F.,
(4,2,2,2,2,2,2,2,2,2,2,2,2,2,2,2,2,2,2,2,2,2,2,2,2,2,2,2,2,2,2,2,2,2,2,
2,2,2,2,2,2,2,2,2,2,2,2,2,2,2,2,2,2,2,2,2,2,2,2,2,2,2,2,2,2,2,2,2,2,2,2,
2,2,2,2,2,2,2,2,2,2,2,2,2,2,2,2,2,2,2,2,2,2,2,2,2,2,2,2,2,2,2,2,2,2,2,2,
2,4),(1.40868741081837,1.45282114574026,1.47138519875834,1.47413177679089,
1.47548761578519,1.47655987155254,1.4778109953015,1.48005790009866,1.49092124667973,
1.5151268521298,1.55576058997058,1.57471715275601,1.57847201680425,1.58087920003979,
1.58279727863786,1.58496151875286,1.58861884365142,1.60315479954775,1.63041096933856,
1.67885891028047,1.68487663847429,1.68679600014785,1.68797464733558,1.68906339401333,
1.69055035593317,1.69399567412729,1.72058648372916,1.74987872522115,1.78575915275887,
1.79048218761372,1.79290596228412,1.79482581833564,1.79697999747668,1.80059135438659,
1.81456962428922,1.86539442246418,1.89525060834919,1.89816654566859,1.89955590972665,
1.90063131619709,1.9018598981651,1.9040035678585,1.91330194616448,1.93215135579698,
1.97256231653036,1.98482739612756,1.99945074480414,2.0032415632813,2.00545767029186,
2.0073706717409,2.00970632810299,2.01415658502488,2.04502863803953,2.09142711888106,
2.10771915549577,2.11035260598368,2.11170331311897,2.11277538648445,2.11403077664091,
2.11629662263216,2.12747402129667,2.15286648941136,2.20673784874064,2.21356422178613,
2.21642053034251,2.2182122676365,2.22017665378882,2.22289578986132,2.22938634569801,
2.25856105646812,2.30111524236714,2.31970024688058,2.32244781926679,2.32380398246119,
2.32487641294606,2.32612764658098,2.3283745138691,2.33923315584635,2.36341874369873,
2.41908468850141,2.42574444335819,2.42828998172059,2.43011817371655,2.4320183137549,
2.43450383031192,2.43725314588343,2.44183093288911,2.45123417697265,2.47774179575797,
2.51518035463293,2.51690561967688,2.52220690407069,2.53248598616245,2.53458334527713,
2.53592493386245,2.53699633411449,2.53825858113818,2.54055637530816,2.55230118277678,
2.60144042319159,2.62013544234763,2.63560978979366,2.63947549573205,2.64170872938115,
2.64343985595649,2.64525080325019,2.64744527432452,2.6506882096222,2.66858622124742),
 .UNSPECIFIED.);
#1753=B_SPLINE_CURVE_WITH_KNOTS('',3,(#164884,#164885,#164886,#164887,#164888,
#164889,#164890,#164891,#164892,#164893),.UNSPECIFIED.,.F.,.F.,(4,3,3,4),
(-85.8723819833138,-85.7556990490293,-85.639073538087,-85.5224480271446),
 .UNSPECIFIED.);
#1754=B_SPLINE_CURVE_WITH_KNOTS('',3,(#164898,#164899,#164900,#164901,#164902,
#164903,#164904,#164905,#164906,#164907,#164908,#164909,#164910,#164911,
#164912,#164913,#164914,#164915,#164916,#164917,#164918,#164919,#164920,
#164921,#164922,#164923,#164924,#164925,#164926,#164927,#164928,#164929,
#164930,#164931,#164932,#164933,#164934,#164935,#164936,#164937,#164938,
#164939,#164940,#164941,#164942,#164943,#164944,#164945,#164946,#164947,
#164948,#164949,#164950,#164951,#164952,#164953,#164954,#164955,#164956,
#164957,#164958,#164959,#164960,#164961,#164962,#164963,#164964,#164965,
#164966,#164967,#164968,#164969,#164970,#164971,#164972,#164973,#164974,
#164975,#164976,#164977,#164978,#164979,#164980,#164981,#164982,#164983,
#164984,#164985,#164986,#164987,#164988,#164989,#164990,#164991,#164992,
#164993,#164994,#164995,#164996,#164997,#164998,#164999,#165000,#165001,
#165002,#165003,#165004,#165005,#165006,#165007,#165008,#165009,#165010,
#165011,#165012,#165013,#165014,#165015,#165016,#165017,#165018,#165019,
#165020,#165021,#165022,#165023,#165024,#165025,#165026,#165027,#165028,
#165029,#165030,#165031,#165032,#165033,#165034,#165035,#165036,#165037,
#165038,#165039,#165040,#165041,#165042,#165043,#165044,#165045,#165046,
#165047,#165048,#165049,#165050,#165051,#165052,#165053,#165054,#165055,
#165056,#165057,#165058,#165059,#165060,#165061,#165062,#165063,#165064,
#165065,#165066,#165067,#165068,#165069,#165070,#165071,#165072,#165073,
#165074,#165075,#165076,#165077,#165078,#165079,#165080,#165081,#165082,
#165083,#165084,#165085,#165086,#165087,#165088,#165089,#165090,#165091,
#165092,#165093,#165094,#165095,#165096,#165097,#165098,#165099,#165100,
#165101,#165102,#165103,#165104,#165105,#165106,#165107,#165108,#165109,
#165110,#165111,#165112,#165113,#165114,#165115,#165116,#165117,#165118,
#165119,#165120,#165121,#165122,#165123,#165124,#165125,#165126,#165127,
#165128,#165129),.UNSPECIFIED.,.F.,.F.,(4,2,2,2,2,2,2,2,2,2,2,2,2,2,2,2,
2,2,2,2,2,2,2,2,2,2,2,2,2,2,2,2,2,2,2,2,2,2,2,2,2,2,2,2,2,2,2,2,2,2,2,2,
2,2,2,2,2,2,2,2,2,2,2,2,2,2,2,2,2,2,2,2,2,2,2,2,2,2,2,2,2,2,2,2,2,2,2,2,
2,2,2,2,2,2,2,2,2,2,2,2,2,2,2,2,2,2,2,2,2,2,2,2,2,2,2,4),(1.26002615597782,
1.26028070805043,1.26243765844669,1.26366897184768,1.26474360947128,1.26612781377373,
1.26901832820632,1.29472133876866,1.33416803952351,1.36189145497452,1.36603205869553,
1.36852853416931,1.37046258464448,1.37255606241967,1.37589461278971,1.38701080285806,
1.40539635323422,1.4527492291279,1.47131192493545,1.47405830345727,1.47541404406432,
1.47648622207153,1.47773725514394,1.47998399723173,1.4908465597794,1.51505042368327,
1.55568120554435,1.57463638800517,1.57839097932564,1.58079798786816,1.58271592736377,
1.58488001062529,1.58853707070335,1.60307197732221,1.63032618449044,1.67877073002063,
1.68478791337691,1.68670712240226,1.68788568111764,1.68897435003655,1.69046121140794,
1.69390632131056,1.72150369537025,1.75670359743434,1.78588842039213,1.79006778318002,
1.79257577918699,1.79451177788885,1.79660044572339,1.79991645399402,1.81082150801718,
1.82871959207018,1.87939916826945,1.89553735609574,1.89816679294372,1.89951654559467,
1.90058843991112,1.90184428978855,1.90411265949309,1.91533666153275,1.94091152279756,
1.99450684191176,2.00135460355215,2.00421424001118,2.00600643001736,2.00796999337776,
2.01068556187289,2.01715599963737,2.07136894588758,2.10734801499149,2.11021314503983,
2.11159256056708,2.11266692187228,2.11390180578823,2.11607423748684,2.12578094808153,
2.17476207518025,2.20992245583459,2.21421041223912,2.21675010787067,2.21869121070358,
2.22076649111642,2.2240214160925,2.23437878726975,2.25104272870629,2.28402275387341,
2.30302734564579,2.30404951385746,2.31976336255357,2.32237134124086,2.32371643803482,
2.32478799036656,2.3260473364914,2.32833195266626,2.33984138667691,2.36654348994477,
2.41852437352912,2.42549083804804,2.42836994827758,2.43016562485505,2.43208673814767,
2.43469532868378,2.43761573579464,2.44261318292921,2.4532382945637,2.48450054508195,
2.52882031075396,2.53348992219872,2.53522377222595,2.5362481016298,2.53734184502224,
2.53885840904915,2.54247568196251,2.54756136826203,2.56162299028348,2.59401617871736),
 .UNSPECIFIED.);
#1755=B_SPLINE_CURVE_WITH_KNOTS('',3,(#165131,#165132,#165133,#165134,#165135,
#165136,#165137,#165138,#165139,#165140,#165141,#165142,#165143,#165144,
#165145,#165146,#165147,#165148,#165149,#165150,#165151,#165152,#165153,
#165154,#165155,#165156,#165157,#165158,#165159,#165160,#165161,#165162,
#165163,#165164,#165165,#165166,#165167,#165168,#165169,#165170,#165171,
#165172,#165173,#165174,#165175,#165176,#165177,#165178,#165179,#165180,
#165181,#165182,#165183,#165184,#165185,#165186,#165187,#165188,#165189,
#165190,#165191,#165192,#165193,#165194,#165195,#165196,#165197,#165198,
#165199,#165200,#165201,#165202,#165203,#165204,#165205,#165206,#165207,
#165208,#165209,#165210,#165211,#165212,#165213,#165214,#165215,#165216,
#165217,#165218,#165219,#165220,#165221,#165222,#165223,#165224,#165225,
#165226,#165227,#165228,#165229,#165230,#165231,#165232,#165233,#165234,
#165235,#165236,#165237,#165238,#165239,#165240,#165241,#165242,#165243,
#165244,#165245,#165246,#165247,#165248,#165249,#165250,#165251,#165252,
#165253,#165254,#165255,#165256,#165257,#165258,#165259,#165260,#165261,
#165262,#165263,#165264,#165265,#165266,#165267,#165268,#165269,#165270,
#165271,#165272,#165273,#165274,#165275,#165276,#165277,#165278,#165279,
#165280,#165281,#165282,#165283,#165284,#165285,#165286,#165287,#165288,
#165289,#165290,#165291,#165292,#165293,#165294,#165295,#165296,#165297,
#165298,#165299,#165300,#165301,#165302,#165303,#165304,#165305,#165306,
#165307,#165308,#165309,#165310,#165311),.UNSPECIFIED.,.F.,.F.,(4,3,3,3,
3,3,3,3,3,3,3,3,3,3,3,3,3,3,3,3,3,3,3,3,3,3,3,3,3,3,3,3,3,3,3,3,3,3,3,3,
3,3,3,3,3,3,3,3,3,3,3,3,3,3,3,3,3,3,3,3,4),(-91.8056330559184,-91.703478392043,
-91.6014794906832,-91.4995669524773,-91.3977052133679,-91.2958587787063,
-91.1939207704849,-91.0919397623249,-90.989771706694,-90.8941169465306,
-90.7907222094828,-90.6874809273678,-90.5843609619755,-90.4813063937666,
-90.378283185409,-90.2752573427367,-90.1721245759587,-90.068935484549,-89.9655634911674,
-89.8952804965687,-89.7918857595207,-89.6886444774058,-89.5855245120134,
-89.4824699438044,-89.3794467354466,-89.2764208927741,-89.173288125996,
-89.0700990345862,-88.9667270412044,-88.8964440466068,-88.793049309559,
-88.6898080274439,-88.5866880620516,-88.4836334938427,-88.3806102854849,
-88.2775844428122,-88.1744516760342,-88.0712625846245,-87.9678905912428,
-87.897607596645,-87.794212859597,-87.690971577482,-87.5878516120898,-87.4847970438808,
-87.3817738355229,-87.2787479928504,-87.1756152260723,-87.0724261346625,
-86.9690541412809,-86.8987711466831,-86.7953764096353,-86.69213512752,-86.5890151621277,
-86.4859605939189,-86.382937385561,-86.279911542888,-86.1767787761099,-86.0735896847,
-85.9702176913185,-85.8999346967212,-85.8723819833138),.UNSPECIFIED.);
#1756=B_SPLINE_CURVE_WITH_KNOTS('',3,(#165312,#165313,#165314,#165315,#165316),
 .UNSPECIFIED.,.F.,.F.,(4,1,4),(-92.1566392527806,-91.8929533964925,-91.8056333339369),
 .UNSPECIFIED.);
#1757=B_SPLINE_CURVE_WITH_KNOTS('',3,(#165322,#165323,#165324,#165325,#165326,
#165327,#165328,#165329,#165330,#165331,#165332,#165333,#165334,#165335,
#165336,#165337,#165338,#165339,#165340,#165341),.UNSPECIFIED.,.F.,.F.,
(4,2,2,2,2,2,2,2,2,4),(2.59390681890108,2.64803077420865,2.65590234473983,
2.65799832092765,2.65922828409126,2.66028508238674,2.66133096658783,2.66268138243313,
2.66513940918834,2.66823303858644),.UNSPECIFIED.);
#1758=B_SPLINE_CURVE_WITH_KNOTS('',3,(#165342,#165343,#165344,#165345,#165346,
#165347,#165348,#165349,#165350,#165351,#165352,#165353,#165354,#165355,
#165356,#165357,#165358,#165359,#165360,#165361,#165362,#165363,#165364,
#165365,#165366,#165367,#165368,#165369,#165370,#165371,#165372,#165373,
#165374,#165375,#165376,#165377,#165378,#165379,#165380,#165381,#165382,
#165383,#165384,#165385,#165386,#165387,#165388,#165389,#165390,#165391,
#165392,#165393,#165394,#165395,#165396,#165397,#165398,#165399,#165400,
#165401,#165402,#165403,#165404,#165405,#165406,#165407,#165408,#165409,
#165410,#165411,#165412,#165413,#165414,#165415,#165416,#165417,#165418,
#165419,#165420,#165421,#165422,#165423,#165424,#165425,#165426,#165427,
#165428,#165429,#165430,#165431,#165432,#165433,#165434,#165435,#165436,
#165437,#165438,#165439,#165440,#165441,#165442,#165443,#165444,#165445,
#165446,#165447,#165448,#165449,#165450,#165451,#165452,#165453,#165454,
#165455,#165456,#165457,#165458,#165459,#165460,#165461,#165462,#165463,
#165464,#165465,#165466,#165467,#165468,#165469,#165470,#165471,#165472,
#165473,#165474,#165475,#165476,#165477,#165478,#165479,#165480,#165481,
#165482,#165483,#165484,#165485,#165486,#165487,#165488,#165489,#165490,
#165491,#165492,#165493,#165494,#165495,#165496,#165497,#165498,#165499,
#165500,#165501,#165502,#165503,#165504,#165505,#165506,#165507,#165508,
#165509,#165510,#165511,#165512,#165513,#165514,#165515,#165516,#165517,
#165518,#165519,#165520,#165521,#165522,#165523,#165524,#165525,#165526,
#165527,#165528,#165529,#165530,#165531,#165532,#165533,#165534,#165535,
#165536,#165537,#165538,#165539,#165540,#165541,#165542,#165543,#165544,
#165545,#165546,#165547,#165548,#165549,#165550,#165551,#165552,#165553,
#165554,#165555,#165556,#165557,#165558,#165559,#165560,#165561,#165562,
#165563,#165564,#165565,#165566,#165567,#165568,#165569,#165570,#165571,
#165572,#165573,#165574,#165575,#165576,#165577,#165578,#165579,#165580,
#165581,#165582,#165583),.UNSPECIFIED.,.F.,.F.,(4,2,2,2,2,2,2,2,2,2,2,2,
2,2,2,2,2,2,2,2,2,2,2,2,2,2,2,2,2,2,2,2,2,2,2,2,2,2,2,2,2,2,2,2,2,2,2,2,
2,2,2,2,2,2,2,2,2,2,2,2,2,2,2,2,2,2,2,2,2,2,2,2,2,2,2,2,2,2,2,2,2,2,2,2,
2,2,2,2,2,2,2,2,2,2,2,2,2,2,2,2,2,2,2,2,2,2,2,2,2,2,2,2,2,2,2,2,2,2,2,2,
4),(0.000817339072717396,0.0612254327528195,0.0876737705967202,0.0938318736697624,
0.0964929805366432,0.0984458542304952,0.100248359885734,0.103168886035034,
0.110389678966243,0.154249311684379,0.195394740453527,0.199213035784798,
0.201237851957825,0.202549372202172,0.203772999109811,0.203776565900573,
0.203780144963764,0.203783736777643,0.203787574314428,0.203791473684978,
0.203795436057235,0.203799463015975,0.203803555948668,0.203807715984486,
0.203811944716874,0.203816243954876,0.203820615083323,0.203825059546327,
0.203829579099047,0.203834175258828,0.203838849929433,0.203843605092771,
0.203848442246181,0.204892136000352,0.206274788297811,0.20915947304974,
0.243327703493716,0.277568497356708,0.294122448124397,0.304429297822026,
0.307677059612904,0.309749872128427,0.311690141237809,0.31423087396419,
0.318525380427928,0.353659954588658,0.402633763010693,0.412337348700009,
0.414508647350004,0.415742808062672,0.416816494385944,0.418194973612607,
0.421057933634848,0.45665134743274,0.489504290229703,0.506061808151536,
0.516370537069155,0.519618709137008,0.521691739801433,0.52363218241276,
0.526173098043653,0.530467814386623,0.565590939106778,0.614523621310496,
0.624282119736505,0.626457330666071,0.627692422823497,0.628766091559657,
0.630143465734079,0.633000400899712,0.656099199057216,0.698304056580163,
0.716918313426454,0.728132929179101,0.731481262618382,0.73357646712124,
0.735509119134418,0.737999605418669,0.742121252942593,0.769138869453326,
0.823719433370545,0.836002065275706,0.838327871257832,0.83959584527571,
0.840666381763847,0.84199968538415,0.84407103513996,0.853972468995163,0.859516307815003,
0.859961922570091,0.866849346951346,0.880575423486423,0.913435731176484,
0.929997286362807,0.94030843369783,0.943557317130617,0.945630789628183,
0.94757163726462,0.950113070921443,0.954408635198058,0.989535041580374,
1.03846544714543,1.04824086681503,1.05041755166975,1.0516531268085,1.05272698887713,
1.05410431501674,1.05696013201451,1.07974137623904,1.092585151773,1.12544038801377,
1.14199337745437,1.15230094909718,1.15554964135732,1.15762321668979,1.15956431854414,
1.1621063130231,1.16640333617586,1.20161017838112,1.25079154582779,1.26002615597782),
 .UNSPECIFIED.);
#1759=B_SPLINE_CURVE_WITH_KNOTS('',3,(#165585,#165586,#165587,#165588,#165589,
#165590,#165591,#165592,#165593,#165594),.UNSPECIFIED.,.F.,.F.,(4,1,1,1,
1,1,1,4),(-98.0888186411165,-97.8859720962637,-96.8871356463018,-95.88829919634,
-94.8894627463781,-93.8906262964162,-92.8917898464543,-92.1566392527806),
 .UNSPECIFIED.);
#1760=B_SPLINE_CURVE_WITH_KNOTS('',3,(#165595,#165596,#165597,#165598,#165599,
#165600,#165601,#165602,#165603,#165604,#165605,#165606,#165607,#165608,
#165609,#165610,#165611,#165612,#165613,#165614),.UNSPECIFIED.,.F.,.F.,
(4,2,2,2,2,2,2,2,2,4),(0.000629226362741632,0.0468682715409837,0.0541782011601138,
0.0579984688717706,0.0612790161803505,0.0633591116006488,0.065296700611161,
0.0678203279030634,0.0720557143177805,0.0751037492301708),.UNSPECIFIED.);
#1761=B_SPLINE_CURVE_WITH_KNOTS('',3,(#165619,#165620,#165621,#165622,#165623,
#165624,#165625,#165626,#165627,#165628,#165629,#165630,#165631,#165632,
#165633,#165634,#165635,#165636,#165637,#165638,#165639,#165640,#165641,
#165642,#165643,#165644,#165645,#165646,#165647,#165648,#165649,#165650,
#165651,#165652,#165653,#165654,#165655,#165656,#165657,#165658,#165659,
#165660,#165661,#165662,#165663,#165664,#165665,#165666,#165667,#165668,
#165669,#165670,#165671,#165672,#165673,#165674,#165675,#165676,#165677,
#165678,#165679,#165680,#165681,#165682,#165683,#165684,#165685,#165686,
#165687,#165688,#165689,#165690,#165691,#165692,#165693,#165694,#165695,
#165696,#165697,#165698,#165699,#165700,#165701,#165702,#165703,#165704,
#165705,#165706,#165707,#165708,#165709,#165710,#165711,#165712,#165713,
#165714,#165715,#165716,#165717,#165718,#165719,#165720,#165721,#165722,
#165723,#165724,#165725,#165726,#165727,#165728,#165729,#165730,#165731,
#165732,#165733,#165734,#165735,#165736,#165737,#165738,#165739,#165740,
#165741,#165742,#165743,#165744,#165745,#165746,#165747,#165748,#165749,
#165750,#165751,#165752,#165753,#165754,#165755,#165756,#165757,#165758,
#165759,#165760,#165761,#165762,#165763,#165764,#165765,#165766,#165767,
#165768,#165769,#165770,#165771,#165772,#165773,#165774,#165775,#165776,
#165777,#165778,#165779,#165780,#165781,#165782,#165783,#165784,#165785,
#165786,#165787,#165788,#165789,#165790,#165791,#165792,#165793,#165794,
#165795,#165796,#165797,#165798,#165799,#165800,#165801,#165802,#165803,
#165804,#165805,#165806,#165807,#165808,#165809,#165810,#165811,#165812,
#165813,#165814,#165815,#165816,#165817,#165818,#165819,#165820,#165821,
#165822,#165823,#165824,#165825,#165826,#165827,#165828,#165829,#165830,
#165831,#165832,#165833,#165834,#165835,#165836,#165837,#165838,#165839,
#165840,#165841,#165842,#165843,#165844,#165845,#165846,#165847,#165848,
#165849,#165850,#165851,#165852,#165853,#165854,#165855,#165856,#165857,
#165858),.UNSPECIFIED.,.F.,.F.,(4,2,2,2,2,2,2,2,2,2,2,2,2,2,2,2,2,2,2,2,
2,2,2,2,2,2,2,2,2,2,2,2,2,2,2,2,2,2,2,2,2,2,2,2,2,2,2,2,2,2,2,2,2,2,2,2,
2,2,2,2,2,2,2,2,2,2,2,2,2,2,2,2,2,2,2,2,2,2,2,2,2,2,2,2,2,2,2,2,2,2,2,2,
2,2,2,2,2,2,2,2,2,2,2,2,2,2,2,2,2,2,2,2,2,2,2,2,2,2,2,4),(1.26010921737026,
1.26507519904627,1.27555923729397,1.27882825410422,1.28090642691018,1.28284598073427,
1.28537754430456,1.289638197626,1.3346351541466,1.37968330383748,1.3844082086735,
1.3861503997765,1.38717632884007,1.38826895714846,1.38977937103468,1.39336075837539,
1.43099589455533,1.48141556130892,1.48847363970178,1.49136787137908,1.49316625195796,
1.49512425137757,1.49780965364733,1.50410317390092,1.53164024864648,1.56004209019016,
1.58237053593612,1.5950765993546,1.59731700586766,1.59870195523859,1.59977669542454,
1.60100760130327,1.60316258464822,1.61262356863888,1.66180558128258,1.69700796564163,
1.70130493692629,1.70384701200501,1.70578822854744,1.70786197700883,1.71111104496496,
1.72142060427254,1.73797984807966,1.77086947219409,1.78460338246217,1.79147582093191,
1.79169109545741,1.79518015772773,1.80716705030004,1.8093685823388,1.81074174855965,
1.81181528521042,1.81305379946272,1.81524362016794,1.82521222274992,1.87395926435719,
1.90902084475786,1.91331569651985,1.91585706580136,1.91779805907657,1.91987187516282,
1.92312168834769,1.93343900250753,1.95001583226262,1.98291872545002,1.99803667495543,
2.00292469361331,2.01883478782531,2.02144944463696,2.02279578282252,2.02386716213014,
2.02512495642997,2.02740331687887,2.03880954001362,2.06510468833873,2.1176375520257,
2.12456375774258,2.12743578826596,2.12922985062767,2.13119073204009,2.13389391795494,
2.14029379588092,2.18941824182025,2.22775583662013,2.23251803597426,2.23426570143994,
2.23529257860472,2.23638429695794,2.23789033096065,2.24144708894313,2.27664190372315,
2.3297665595455,2.33664873732664,2.33951356055126,2.34130633905714,2.3432684043734,
2.3459779654706,2.35241537963936,2.38115170514505,2.4253317692948,2.42894637740709,
2.44306264667357,2.44537282296395,2.44676354558292,2.44780989200213,2.4489851033896,
2.45023044687475,2.45209499031907,2.45549251038601,2.46337194216412,2.51337437630157,
2.54520995529924,2.5494477005681,2.55197237865418,2.55391055729918,2.55599107212067,
2.55927182787169,2.5698633194134,2.58705194835977,2.59390681890108),
 .UNSPECIFIED.);
#1762=B_SPLINE_CURVE_WITH_KNOTS('',3,(#165859,#165860,#165861,#165862,#165863,
#165864,#165865,#165866,#165867,#165868,#165869,#165870,#165871,#165872,
#165873,#165874,#165875,#165876,#165877,#165878,#165879,#165880,#165881,
#165882,#165883,#165884,#165885,#165886,#165887,#165888,#165889,#165890,
#165891,#165892,#165893,#165894,#165895,#165896,#165897,#165898,#165899,
#165900,#165901,#165902,#165903,#165904,#165905,#165906,#165907,#165908,
#165909,#165910,#165911,#165912,#165913,#165914,#165915,#165916,#165917,
#165918,#165919,#165920,#165921,#165922,#165923,#165924,#165925,#165926,
#165927,#165928,#165929,#165930,#165931,#165932,#165933,#165934,#165935,
#165936,#165937,#165938,#165939,#165940,#165941,#165942,#165943,#165944,
#165945,#165946,#165947,#165948,#165949,#165950,#165951,#165952,#165953,
#165954,#165955,#165956,#165957,#165958,#165959,#165960,#165961,#165962,
#165963,#165964,#165965,#165966,#165967,#165968,#165969,#165970,#165971,
#165972,#165973,#165974,#165975,#165976,#165977,#165978,#165979,#165980,
#165981,#165982,#165983,#165984,#165985,#165986,#165987,#165988,#165989,
#165990,#165991,#165992,#165993,#165994,#165995,#165996,#165997,#165998,
#165999,#166000,#166001,#166002,#166003,#166004,#166005,#166006,#166007,
#166008,#166009,#166010,#166011,#166012,#166013,#166014,#166015,#166016,
#166017,#166018,#166019,#166020,#166021,#166022,#166023,#166024,#166025,
#166026,#166027,#166028,#166029,#166030,#166031,#166032,#166033,#166034,
#166035,#166036,#166037,#166038,#166039,#166040,#166041,#166042,#166043,
#166044,#166045,#166046,#166047,#166048,#166049,#166050,#166051,#166052,
#166053,#166054,#166055,#166056,#166057,#166058,#166059,#166060,#166061,
#166062,#166063,#166064,#166065,#166066,#166067,#166068,#166069,#166070,
#166071,#166072,#166073,#166074,#166075,#166076,#166077,#166078),
 .UNSPECIFIED.,.F.,.F.,(4,2,2,2,2,2,2,2,2,2,2,2,2,2,2,2,2,2,2,2,2,2,2,2,
2,2,2,2,2,2,2,2,2,2,2,2,2,2,2,2,2,2,2,2,2,2,2,2,2,2,2,2,2,2,2,2,2,2,2,2,
2,2,2,2,2,2,2,2,2,2,2,2,2,2,2,2,2,2,2,2,2,2,2,2,2,2,2,2,2,2,2,2,2,2,2,2,
2,2,2,2,2,2,2,2,2,2,2,2,2,4),(0.0751037492301708,0.118880917795946,0.139376817903217,
0.162219030290009,0.1668645224268,0.168156402197407,0.169384240099947,0.170458911131563,
0.171847203283008,0.174760478527842,0.204939955840196,0.25644351367738,
0.26944615321281,0.272989263665715,0.275127428116121,0.27704870403762,0.279495695920477,
0.283383389282271,0.304699992500162,0.352239606498166,0.369333915622309,
0.37805575371251,0.380155277212108,0.381373589679308,0.382450006624803,
0.383830705743057,0.38610757303591,0.39954906470426,0.401671935001865,0.405953171131185,
0.448938066353763,0.476874669080311,0.483215758041737,0.485908528233608,
0.487867146392035,0.489662804304886,0.492545408287964,0.499538379224643,
0.551069004424207,0.578089566859801,0.589674817009573,0.591962866590075,
0.593222562354446,0.594293485817936,0.595636612522682,0.598237329464448,
0.613805583386551,0.620261087972416,0.661675792697354,0.688947702140474,
0.695208005898256,0.697887019092948,0.699843253114721,0.701642031816917,
0.704541356783058,0.711634308872206,0.761292293849531,0.799603994996305,
0.803208308632069,0.804722262352918,0.805815169155305,0.806839547130502,
0.808575244902419,0.813260103061409,0.854341746075041,0.900771483197287,
0.907163364146536,0.909864877039203,0.911825169225872,0.913619127096042,
0.916491927392863,0.923424811140936,0.975871376244757,1.00224511615172,
1.01366959274197,1.01594870965649,1.01720652167612,1.01827767754899,1.01962342569414,
1.0222360319686,1.03808734827923,1.04283130672364,1.05810918948618,1.09098449621427,
1.1075660460329,1.1178860027798,1.12113572695467,1.12320927143933,1.12514986022135,
1.12769048434938,1.13198362594672,1.17438369867638,1.20344098471063,1.22305680282963,
1.22701196143879,1.2285836225058,1.22968719560523,1.23069765501811,1.2323612612938,
1.23658634211238,1.28592939951302,1.32669781224683,1.33176406047032,1.33422368661709,
1.33614666424004,1.33827828718448,1.34179101576568,1.35466697760074,1.37736927597896,
1.40852037702754),.UNSPECIFIED.);
#1763=B_SPLINE_CURVE_WITH_KNOTS('',3,(#166084,#166085,#166086,#166087),
 .UNSPECIFIED.,.F.,.F.,(4,4),(114.406674973252,114.756144714286),
 .UNSPECIFIED.);
#1764=B_SPLINE_CURVE_WITH_KNOTS('',3,(#166088,#166089,#166090,#166091,#166092,
#166093,#166094,#166095,#166096,#166097,#166098,#166099,#166100,#166101,
#166102,#166103,#166104,#166105,#166106,#166107,#166108,#166109,#166110,
#166111,#166112,#166113,#166114,#166115,#166116,#166117,#166118,#166119,
#166120,#166121,#166122,#166123,#166124,#166125,#166126,#166127,#166128,
#166129,#166130,#166131,#166132,#166133,#166134,#166135,#166136,#166137,
#166138,#166139,#166140,#166141,#166142,#166143,#166144,#166145,#166146,
#166147,#166148,#166149,#166150,#166151,#166152,#166153,#166154,#166155,
#166156,#166157,#166158,#166159,#166160,#166161,#166162,#166163,#166164,
#166165,#166166,#166167,#166168,#166169,#166170,#166171,#166172,#166173,
#166174,#166175,#166176,#166177,#166178,#166179,#166180,#166181,#166182,
#166183,#166184,#166185,#166186,#166187,#166188,#166189,#166190,#166191,
#166192,#166193,#166194,#166195,#166196,#166197,#166198,#166199,#166200,
#166201,#166202,#166203,#166204,#166205,#166206,#166207,#166208,#166209,
#166210,#166211,#166212,#166213,#166214,#166215,#166216,#166217,#166218,
#166219,#166220,#166221,#166222,#166223,#166224,#166225,#166226,#166227,
#166228,#166229,#166230,#166231,#166232,#166233,#166234,#166235,#166236,
#166237,#166238,#166239,#166240,#166241,#166242,#166243,#166244,#166245,
#166246,#166247,#166248,#166249,#166250,#166251,#166252,#166253,#166254,
#166255,#166256,#166257,#166258,#166259,#166260,#166261,#166262,#166263,
#166264,#166265,#166266,#166267,#166268,#166269,#166270,#166271,#166272,
#166273,#166274,#166275,#166276,#166277,#166278,#166279,#166280,#166281,
#166282,#166283,#166284,#166285,#166286,#166287,#166288,#166289,#166290,
#166291,#166292,#166293,#166294,#166295,#166296,#166297,#166298,#166299,
#166300,#166301,#166302,#166303,#166304,#166305),.UNSPECIFIED.,.F.,.F.,
(4,2,2,2,2,2,2,2,2,2,2,2,2,2,2,2,2,2,2,2,2,2,2,2,2,2,2,2,2,2,2,2,2,2,2,
2,2,2,2,2,2,2,2,2,2,2,2,2,2,2,2,2,2,2,2,2,2,2,2,2,2,2,2,2,2,2,2,2,2,2,2,
2,2,2,2,2,2,2,2,2,2,2,2,2,2,2,2,2,2,2,2,2,2,2,2,2,2,2,2,2,2,2,2,2,2,2,2,
2,4),(0.000658789515707303,0.00332970180415904,0.00592165902641297,0.00778879700177709,
0.00964368955138184,0.0114909186089904,0.0146445375462132,0.0233614963763356,
0.0882031581702577,0.10859694712227,0.112633279300404,0.114217804455085,
0.115323920171485,0.116331747666332,0.117981260296211,0.122122285944367,
0.172468751005332,0.209103911759757,0.21404883968213,0.216947679594109,
0.219546315887063,0.221463438656713,0.223262615789461,0.226163322652698,
0.233240925903314,0.283134745524853,0.321237734036367,0.32484039700091,
0.326354173578048,0.32744714437323,0.328471734809312,0.330208116667581,
0.334896706617737,0.375891352156246,0.422413598326696,0.428806451658905,
0.431508314614591,0.433468838592159,0.435262993252094,0.438136075204148,
0.445069465778075,0.497521833869186,0.523899061692082,0.535324964039552,
0.537604348547007,0.538862306004373,0.539933584374217,0.541279484692083,
0.543892381332811,0.559745117646786,0.564467327213708,0.609730512029555,
0.628225324282423,0.639389069357717,0.642732263372665,0.644826500865052,
0.646759789689279,0.649253234594747,0.653384405443102,0.68075952231016,
0.723082618470413,0.739259590348515,0.7476688771705,0.749744014098205,0.750957103079242,
0.752034946544863,0.753425291596481,0.755734300121712,0.769827652572318,
0.772669413539149,0.822247298681764,0.840396918145557,0.851411582559185,
0.854738789655328,0.856829496553685,0.858763954196761,0.861265124926505,
0.865422615588646,0.893801367847194,0.947093326898015,0.959257576785838,
0.961577403978429,0.962844177535305,0.963914919843751,0.965250013507755,
0.967326916370838,0.97730575193491,0.98291454772312,0.992312010149648,1.00388099133634,
1.03672569067058,1.05326574937608,1.06356749723049,1.06681554095262,1.06888898776942,
1.07083016989094,1.07337255897637,1.07767089828658,1.11297880245535,1.16222997987263,
1.17156701784788,1.17371313167014,1.17494206414828,1.17601709842688,1.17740507541625,
1.18031492369544,1.20844434728681,1.24813083709657,1.26010921737026),
 .UNSPECIFIED.);
#1765=B_SPLINE_CURVE_WITH_KNOTS('',3,(#166307,#166308,#166309,#166310,#166311,
#166312,#166313,#166314,#166315,#166316,#166317,#166318,#166319,#166320,
#166321,#166322,#166323,#166324,#166325,#166326,#166327,#166328,#166329,
#166330,#166331,#166332,#166333,#166334,#166335,#166336,#166337,#166338,
#166339,#166340,#166341,#166342,#166343,#166344,#166345,#166346,#166347,
#166348,#166349,#166350,#166351,#166352,#166353,#166354,#166355,#166356,
#166357,#166358,#166359,#166360,#166361,#166362,#166363,#166364,#166365,
#166366,#166367,#166368,#166369,#166370,#166371,#166372,#166373,#166374,
#166375,#166376,#166377,#166378,#166379,#166380,#166381,#166382,#166383,
#166384,#166385,#166386,#166387,#166388,#166389,#166390,#166391,#166392,
#166393,#166394,#166395,#166396,#166397,#166398,#166399,#166400,#166401,
#166402,#166403,#166404,#166405,#166406,#166407,#166408,#166409,#166410,
#166411,#166412,#166413,#166414,#166415,#166416,#166417,#166418,#166419,
#166420,#166421,#166422,#166423,#166424,#166425,#166426,#166427,#166428,
#166429,#166430,#166431,#166432,#166433,#166434,#166435,#166436,#166437,
#166438,#166439,#166440,#166441,#166442,#166443,#166444,#166445,#166446,
#166447,#166448,#166449,#166450,#166451,#166452,#166453,#166454,#166455,
#166456,#166457,#166458,#166459,#166460,#166461,#166462,#166463,#166464,
#166465,#166466,#166467,#166468,#166469,#166470,#166471,#166472,#166473,
#166474,#166475,#166476,#166477,#166478,#166479,#166480,#166481,#166482,
#166483,#166484,#166485,#166486,#166487,#166488,#166489,#166490,#166491,
#166492,#166493,#166494,#166495,#166496,#166497,#166498,#166499,#166500,
#166501,#166502,#166503,#166504,#166505,#166506,#166507,#166508,#166509,
#166510,#166511,#166512,#166513,#166514,#166515,#166516,#166517,#166518,
#166519,#166520,#166521,#166522,#166523,#166524,#166525,#166526),
 .UNSPECIFIED.,.F.,.F.,(4,2,2,2,2,2,2,2,2,2,2,2,2,2,2,2,2,2,2,2,2,2,2,2,
2,2,2,2,2,2,2,2,2,2,2,2,2,2,2,2,2,2,2,2,2,2,2,2,2,2,2,2,2,2,2,2,2,2,2,2,
2,2,2,2,2,2,2,2,2,2,2,2,2,2,2,2,2,2,2,2,2,2,2,2,2,2,2,2,2,2,2,2,2,2,2,2,
2,2,2,2,2,2,2,2,2,2,2,2,2,4),(1.40852037702754,1.41595952831496,1.42095388239778,
1.43696095698081,1.43958032952729,1.44092752275851,1.44199875462644,1.44325541612354,
1.44552928276432,1.45686267755102,1.48287403764511,1.53579379382189,1.5426892009883,
1.54555580767838,1.54734862205882,1.54930985839816,1.55201668258124,1.5584400525967,
1.587064212374,1.63834665401397,1.64940840938901,1.65155540412573,1.65291182923959,
1.65398373286765,1.65523350795285,1.65747565037909,1.66827109295293,1.69223143156492,
1.74818522847414,1.75481065816892,1.75734997113946,1.7591758670615,1.76111445160845,
1.76368758723061,1.76935215543428,1.79199535293755,1.82481339615918,1.82925953898682,
1.86052855248765,1.8634404249806,1.86482848821479,1.865903180561,1.8671312741363,
1.86927485860266,1.87858471365108,1.92772623338111,1.96309845209544,1.96739599507743,
1.9699377230736,1.97187828008559,1.97395094166477,1.97719750884374,1.98749241484776,
2.00402173851242,2.03687891921335,2.04844679064327,2.05789193589881,2.07294229793109,
2.07529362352922,2.07669617215181,2.0777753926561,2.07898105911017,2.08102370323427,
2.0890449570702,2.10412364450517,2.14357820280149,2.17511544237045,2.17934612522303,
2.18186837571774,2.18380572726972,2.18588637031083,2.18916947880309,2.19978736861725,
2.21703729298442,2.25266391193605,2.28437456570608,2.28728570742664,2.28867356480054,
2.28974816337607,2.29097622319617,2.29311992072815,2.30243292720451,2.3515827274682,
2.38693606851853,2.39123308462749,2.39377455913906,2.39571495608015,2.39778747911725,
2.40103389694969,2.41112434453458,2.42729141912476,2.46900282389672,2.49632888141909,
2.49923242750349,2.50061878657169,2.50169320466273,2.50292215527821,2.50421560674167,
2.5088811015245,2.53299182872568,2.55388883690921,2.59892722220135,2.60318389446238,
2.60571366671517,2.60765217013647,2.60972953080684,2.61299792841729,2.61680081734889,
2.62406474248904,2.66768826363348),.UNSPECIFIED.);
#1766=B_SPLINE_CURVE_WITH_KNOTS('',3,(#166527,#166528,#166529,#166530,#166531,
#166532,#166533,#166534,#166535,#166536,#166537,#166538,#166539,#166540,
#166541,#166542,#166543,#166544,#166545,#166546),.UNSPECIFIED.,.F.,.F.,
(4,2,2,2,2,2,2,2,2,4),(0.000649988982928049,0.0375152709071572,0.0412926030068312,
0.0433020300555975,0.0446072114830325,0.0458444148964173,0.0469177273846094,
0.0482917865179784,0.051132055185458,0.0747588911148556),.UNSPECIFIED.);
#1767=B_SPLINE_CURVE_WITH_KNOTS('',3,(#166552,#166553,#166554,#166555,#166556,
#166557,#166558,#166559,#166560,#166561),.UNSPECIFIED.,.F.,.F.,(4,3,3,4),
(120.689857252469,120.859210445387,120.962579625168,121.040544022956),
 .UNSPECIFIED.);
#1768=B_SPLINE_CURVE_WITH_KNOTS('',3,(#166562,#166563,#166564,#166565,#166566,
#166567,#166568,#166569,#166570,#166571),.UNSPECIFIED.,.F.,.F.,(4,1,1,1,
1,1,1,4),(114.756144714286,114.866191745616,115.865028195577,116.863864645539,
117.862701095501,118.861537545463,119.860373995425,120.689851223516),
 .UNSPECIFIED.);
#1769=B_SPLINE_CURVE_WITH_KNOTS('',3,(#166572,#166573,#166574,#166575,#166576,
#166577,#166578,#166579,#166580,#166581,#166582,#166583,#166584,#166585,
#166586,#166587,#166588,#166589,#166590,#166591,#166592,#166593,#166594,
#166595,#166596,#166597,#166598,#166599,#166600,#166601,#166602,#166603,
#166604,#166605,#166606,#166607,#166608,#166609,#166610,#166611,#166612,
#166613,#166614,#166615,#166616,#166617,#166618,#166619,#166620,#166621,
#166622,#166623,#166624,#166625,#166626,#166627,#166628,#166629,#166630,
#166631,#166632,#166633,#166634,#166635,#166636,#166637,#166638,#166639,
#166640,#166641,#166642,#166643,#166644,#166645,#166646,#166647,#166648,
#166649,#166650,#166651,#166652,#166653,#166654,#166655,#166656,#166657,
#166658,#166659,#166660,#166661,#166662,#166663,#166664,#166665,#166666,
#166667,#166668,#166669,#166670,#166671,#166672,#166673,#166674,#166675,
#166676,#166677,#166678,#166679,#166680,#166681,#166682,#166683,#166684,
#166685,#166686,#166687,#166688,#166689,#166690,#166691,#166692,#166693,
#166694,#166695,#166696,#166697,#166698,#166699,#166700,#166701,#166702,
#166703,#166704,#166705,#166706,#166707,#166708,#166709,#166710,#166711,
#166712,#166713,#166714,#166715,#166716,#166717,#166718,#166719,#166720,
#166721,#166722,#166723,#166724,#166725,#166726,#166727,#166728,#166729,
#166730,#166731,#166732,#166733,#166734,#166735,#166736,#166737,#166738,
#166739,#166740,#166741,#166742,#166743,#166744,#166745,#166746,#166747,
#166748,#166749,#166750,#166751,#166752,#166753,#166754,#166755,#166756,
#166757,#166758,#166759,#166760,#166761,#166762,#166763,#166764,#166765,
#166766,#166767,#166768,#166769,#166770,#166771,#166772,#166773,#166774,
#166775,#166776,#166777,#166778,#166779,#166780,#166781,#166782,#166783,
#166784,#166785,#166786,#166787,#166788,#166789),.UNSPECIFIED.,.F.,.F.,
(4,2,2,2,2,2,2,2,2,2,2,2,2,2,2,2,2,2,2,2,2,2,2,2,2,2,2,2,2,2,2,2,2,2,2,
2,2,2,2,2,2,2,2,2,2,2,2,2,2,2,2,2,2,2,2,2,2,2,2,2,2,2,2,2,2,2,2,2,2,2,2,
2,2,2,2,2,2,2,2,2,2,2,2,2,2,2,2,2,2,2,2,2,2,2,2,2,2,2,2,2,2,2,2,2,2,2,2,
2,4),(0.0747588911148556,0.087979694588596,0.109399136949241,0.136182140554699,
0.146436035987435,0.149706925655296,0.151785020597418,0.153723617536559,
0.156252665620082,0.160506269737635,0.193185982491467,0.22255610653982,
0.244174291645429,0.254295267426268,0.256485238129221,0.257733385334679,
0.258805387235881,0.26016385040786,0.26283591418482,0.28021709369287,0.329256334993405,
0.347303221259107,0.354572452419847,0.360002124569805,0.362567486827097,
0.364504846715067,0.366333003885582,0.368880952611567,0.375561837111131,
0.430975921106836,0.455320546238687,0.466218593280985,0.468466939481635,
0.469718052812365,0.470789803387546,0.472144360538783,0.474886251973298,
0.493334149644452,0.537461144228889,0.565331953351833,0.571665374198063,
0.574356996676347,0.576315555506733,0.57811169641977,0.580996255765975,
0.587999994025098,0.639383233690721,0.666515232559005,0.678128411701344,
0.680418179427137,0.681678323015426,0.682749327388064,0.684092175553081,
0.686691246643468,0.702216444472666,0.708761400960079,0.722633915488646,
0.755493977812072,0.772056477515175,0.782367900486531,0.785616704542271,
0.787690086444634,0.789630821229254,0.792172066640925,0.796467222035025,
0.831578342181658,0.880465467159598,0.89028865354969,0.892468511707725,
0.893704743449463,0.894778444650492,0.896154609205564,0.899004737472686,
0.935374661653975,0.989163067608613,0.995619120739391,0.998331688515185,
1.00029418264342,1.00208615606779,1.00494708242994,1.01180636174837,1.06524496581856,
1.09093521918544,1.10218661822474,1.10445603590278,1.10571184448875,1.10678332906235,
1.10813208207245,1.1107581471268,1.1269223330942,1.1775803274199,1.20199431100506,
1.20789433150569,1.21051039586907,1.21245609416164,1.21427049060166,1.21676509944741,
1.22311494402584,1.28150392542795,1.30395458582152,1.31433180589374,1.31654821041432,
1.31779249621548,1.31886522030498,1.32022981461843,1.32240322478293,1.33389992718014,
1.38263552906857,1.40832427926634),.UNSPECIFIED.);
#1770=B_SPLINE_CURVE_WITH_KNOTS('',3,(#166795,#166796,#166797,#166798,#166799,
#166800,#166801,#166802),.UNSPECIFIED.,.F.,.F.,(4,2,2,4),(2.59385008432844,
2.59859935883543,2.62663692859619,2.66832834108701),.UNSPECIFIED.);
#1771=B_SPLINE_CURVE_WITH_KNOTS('',3,(#166803,#166804,#166805,#166806,#166807,
#166808,#166809,#166810,#166811,#166812,#166813,#166814,#166815,#166816,
#166817,#166818,#166819,#166820,#166821,#166822,#166823,#166824,#166825,
#166826,#166827,#166828,#166829,#166830,#166831,#166832,#166833,#166834,
#166835,#166836,#166837,#166838,#166839,#166840,#166841,#166842,#166843,
#166844,#166845,#166846,#166847,#166848,#166849,#166850,#166851,#166852,
#166853,#166854,#166855,#166856,#166857,#166858,#166859,#166860,#166861,
#166862,#166863,#166864,#166865,#166866,#166867,#166868,#166869,#166870,
#166871,#166872,#166873,#166874,#166875,#166876,#166877,#166878,#166879,
#166880,#166881,#166882,#166883,#166884,#166885,#166886,#166887,#166888,
#166889,#166890,#166891,#166892,#166893,#166894,#166895,#166896,#166897,
#166898,#166899,#166900,#166901,#166902,#166903,#166904,#166905,#166906,
#166907,#166908,#166909,#166910,#166911,#166912,#166913,#166914,#166915,
#166916,#166917,#166918,#166919,#166920,#166921,#166922,#166923,#166924,
#166925,#166926,#166927,#166928,#166929,#166930,#166931,#166932,#166933,
#166934,#166935,#166936,#166937,#166938,#166939,#166940,#166941,#166942,
#166943,#166944,#166945,#166946,#166947,#166948,#166949,#166950,#166951,
#166952,#166953,#166954,#166955,#166956,#166957,#166958,#166959,#166960,
#166961,#166962,#166963,#166964,#166965,#166966,#166967,#166968,#166969,
#166970,#166971,#166972,#166973,#166974,#166975,#166976,#166977,#166978,
#166979,#166980),.UNSPECIFIED.,.F.,.F.,(4,3,3,3,3,3,3,3,3,3,3,3,3,3,3,3,
3,3,3,3,3,3,3,3,3,3,3,3,3,3,3,3,3,3,3,3,3,3,3,3,3,3,3,3,3,3,3,3,3,3,3,3,
3,3,3,3,3,3,3,4),(121.040544022956,121.143685231131,121.246752684529,121.349780436244,
121.452802487907,121.55592611181,121.659098574575,121.762462086372,121.858046895349,
121.961441632397,122.064682914512,122.167802879905,122.270857448114,122.373880656472,
122.476906499144,122.580039265923,122.683228357333,122.786600350714,122.856883345311,
122.960278082359,123.063519364473,123.166639329865,123.269693898074,123.372717106431,
123.475742949104,123.578875715881,123.682064807291,123.785436800672,123.855719795272,
123.95911453232,124.062355814435,124.165475779827,124.268530348036,124.371553556394,
124.474579399066,124.577712165844,124.680901257254,124.784273250636,124.854556245234,
124.957950982282,125.061192264397,125.16431222979,125.267366797999,125.370390006357,
125.473415849029,125.576548615808,125.679737707218,125.783109700599,125.853392695196,
125.956787432244,126.060028714359,126.163148679751,126.26620324796,126.369226456318,
126.472252298991,126.575385065769,126.678574157179,126.78194615056,126.852229145158,
126.973042559648),.UNSPECIFIED.);
#1772=B_SPLINE_CURVE_WITH_KNOTS('',3,(#166982,#166983,#166984,#166985,#166986,
#166987,#166988,#166989,#166990,#166991,#166992,#166993,#166994,#166995,
#166996,#166997,#166998,#166999,#167000,#167001,#167002,#167003,#167004,
#167005,#167006,#167007,#167008,#167009,#167010,#167011,#167012,#167013,
#167014,#167015,#167016,#167017,#167018,#167019,#167020,#167021,#167022,
#167023,#167024,#167025,#167026,#167027,#167028,#167029,#167030,#167031,
#167032,#167033,#167034,#167035,#167036,#167037,#167038,#167039,#167040,
#167041,#167042,#167043,#167044,#167045,#167046,#167047,#167048,#167049,
#167050,#167051,#167052,#167053,#167054,#167055,#167056,#167057,#167058,
#167059,#167060,#167061,#167062,#167063,#167064,#167065,#167066,#167067,
#167068,#167069,#167070,#167071,#167072,#167073,#167074,#167075,#167076,
#167077,#167078,#167079,#167080,#167081,#167082,#167083,#167084,#167085,
#167086,#167087,#167088,#167089,#167090,#167091,#167092,#167093,#167094,
#167095,#167096,#167097,#167098,#167099,#167100,#167101,#167102,#167103,
#167104,#167105,#167106,#167107,#167108,#167109,#167110,#167111,#167112,
#167113,#167114,#167115,#167116,#167117,#167118,#167119,#167120,#167121,
#167122,#167123,#167124,#167125,#167126,#167127,#167128,#167129,#167130,
#167131,#167132,#167133,#167134,#167135,#167136,#167137,#167138,#167139,
#167140,#167141,#167142,#167143,#167144,#167145,#167146,#167147,#167148,
#167149,#167150,#167151,#167152,#167153,#167154,#167155,#167156,#167157,
#167158,#167159,#167160,#167161,#167162,#167163,#167164,#167165,#167166,
#167167,#167168,#167169,#167170,#167171,#167172,#167173,#167174,#167175,
#167176,#167177,#167178,#167179,#167180,#167181,#167182,#167183,#167184,
#167185,#167186,#167187,#167188,#167189,#167190,#167191,#167192,#167193,
#167194,#167195,#167196,#167197,#167198,#167199),.UNSPECIFIED.,.F.,.F.,
(4,2,2,2,2,2,2,2,2,2,2,2,2,2,2,2,2,2,2,2,2,2,2,2,2,2,2,2,2,2,2,2,2,2,2,
2,2,2,2,2,2,2,2,2,2,2,2,2,2,2,2,2,2,2,2,2,2,2,2,2,2,2,2,2,2,2,2,2,2,2,2,
2,2,2,2,2,2,2,2,2,2,2,2,2,2,2,2,2,2,2,2,2,2,2,2,2,2,2,2,2,2,2,2,2,2,2,2,
2,4),(1.40832427926634,1.4158388062147,1.42010266029481,1.42263495150552,
1.42457437188948,1.42665172707618,1.42991803767986,1.44038109885889,1.45728205103867,
1.49511040246738,1.52518594762253,1.52810053893145,1.52948931560261,1.53056429223976,
1.53179241090507,1.53393533718452,1.54323149310023,1.56207803469736,1.60247851019985,
1.61474060438569,1.62934644710789,1.63313472526375,1.63534971493536,1.63726197419843,
1.63959700388483,1.64404692630448,1.6749596348227,1.72180634881348,1.73760400443668,
1.74021648824691,1.74156237286273,1.74263374219591,1.74389193216911,1.7461720482291,
1.75760863207442,1.78402405523123,1.83638779062094,1.84332622545897,1.84620030356327,
1.8479947631746,1.84995537216268,1.85265689086746,1.85904674336266,1.88738501485849,
1.93728474532696,1.94991457736624,1.95215082810244,1.9535344518334,1.95460896006765,
1.95584049504417,1.9579986935857,1.96750734347849,2.01664197498015,2.05182812617918,
2.05612448612284,2.05866624811658,2.06060725355324,2.06268080361921,2.06592961736213,
2.07623884721228,2.09279801573864,2.12568557287272,2.13955174482702,2.1461141664972,
2.16166404073964,2.16426446477404,2.16560770326363,2.16667885498645,2.16793898646776,
2.17022824628745,2.18182910816754,2.20890610924678,2.2603362859139,2.26733504531375,
2.27021900055765,2.27201519475415,2.27397416006816,2.27666696716224,2.28300607532969,
2.31092439298894,2.35693401362682,2.35802620661315,2.37367486915399,2.37627933554951,
2.37762344466943,2.37869464608864,2.37995408655873,2.38224017082084,2.39378430044301,
2.42063176551538,2.47235791712428,2.47935400996171,2.4822375149983,2.48403362086753,
2.48585454824163,2.48840725970004,2.49399834014362,2.50150583662065,2.5204175318765,
2.54640017272129,2.58249627838875,2.58727554921537,2.58902572115793,2.59005302557666,
2.59114431881853,2.5926483382996,2.59619385941298,2.6289385996989,2.66749524589182),
 .UNSPECIFIED.);
#1773=B_SPLINE_CURVE_WITH_KNOTS('',3,(#167200,#167201,#167202,#167203,#167204,
#167205,#167206,#167207,#167208,#167209,#167210,#167211,#167212,#167213,
#167214,#167215,#167216,#167217,#167218,#167219,#167220,#167221),
 .UNSPECIFIED.,.F.,.F.,(4,2,2,2,2,2,2,2,2,2,4),(0.000768645035296635,0.0217310010489876,
0.0248341253626711,0.0269704391246487,0.0287696835339234,0.0306848756723677,
0.0330688196914889,0.0367500933377631,0.0545891744943505,0.0729777540908564,
0.0751664254368708),.UNSPECIFIED.);
#1774=B_SPLINE_CURVE_WITH_KNOTS('',3,(#167226,#167227,#167228,#167229,#167230,
#167231,#167232,#167233,#167234,#167235,#167236,#167237,#167238,#167239,
#167240,#167241,#167242,#167243,#167244,#167245,#167246,#167247,#167248,
#167249,#167250,#167251,#167252,#167253,#167254,#167255,#167256,#167257,
#167258,#167259,#167260,#167261,#167262,#167263,#167264,#167265,#167266,
#167267,#167268,#167269,#167270,#167271,#167272,#167273,#167274,#167275,
#167276,#167277,#167278,#167279,#167280,#167281,#167282,#167283,#167284,
#167285,#167286,#167287,#167288,#167289,#167290,#167291,#167292,#167293,
#167294,#167295,#167296,#167297,#167298,#167299,#167300,#167301,#167302,
#167303,#167304,#167305,#167306,#167307,#167308,#167309,#167310,#167311,
#167312,#167313,#167314,#167315,#167316,#167317,#167318,#167319,#167320,
#167321,#167322,#167323,#167324,#167325,#167326,#167327,#167328,#167329,
#167330,#167331,#167332,#167333,#167334,#167335,#167336,#167337,#167338,
#167339,#167340,#167341,#167342,#167343,#167344,#167345,#167346,#167347,
#167348,#167349,#167350,#167351,#167352,#167353,#167354,#167355,#167356,
#167357,#167358,#167359,#167360,#167361,#167362,#167363,#167364,#167365,
#167366,#167367,#167368,#167369,#167370,#167371,#167372,#167373,#167374,
#167375,#167376,#167377,#167378,#167379,#167380,#167381,#167382,#167383,
#167384,#167385,#167386,#167387,#167388,#167389,#167390,#167391,#167392,
#167393,#167394,#167395,#167396,#167397,#167398,#167399,#167400,#167401,
#167402,#167403,#167404,#167405,#167406,#167407,#167408,#167409,#167410,
#167411,#167412,#167413,#167414,#167415,#167416,#167417,#167418,#167419,
#167420,#167421,#167422,#167423,#167424,#167425,#167426,#167427,#167428,
#167429,#167430,#167431,#167432,#167433,#167434,#167435,#167436,#167437,
#167438,#167439,#167440,#167441,#167442,#167443,#167444,#167445,#167446,
#167447,#167448,#167449,#167450,#167451,#167452,#167453,#167454,#167455),
 .UNSPECIFIED.,.F.,.F.,(4,2,2,2,2,2,2,2,2,2,2,2,2,2,2,2,2,2,2,2,2,2,2,2,
2,2,2,2,2,2,2,2,2,2,2,2,2,2,2,2,2,2,2,2,2,2,2,2,2,2,2,2,2,2,2,2,2,2,2,2,
2,2,2,2,2,2,2,2,2,2,2,2,2,2,2,2,2,2,2,2,2,2,2,2,2,2,2,2,2,2,2,2,2,2,2,2,
2,2,2,2,2,2,2,2,2,2,2,2,2,2,2,2,2,2,4),(1.25997501180952,1.2781789465602,
1.30768283917131,1.31209327376651,1.31442021416852,1.31614731222761,1.31830375361268,
1.32192660105968,1.33437740302623,1.38533839436569,1.4165482807573,1.4194614750814,
1.42085013634194,1.42192527693291,1.42315386621344,1.42529827720666,1.43461112346177,
1.48377031670444,1.51916083916367,1.52346020859321,1.52600300379715,1.52794436810435,
1.53001788467215,1.53326577592756,1.54356475303071,1.56010049196427,1.59297093809217,
1.60449684565962,1.61425394219995,1.6160834713369,1.62921411944707,1.63147619039573,
1.63286761083593,1.63394297443524,1.63516968294175,1.6373058256739,1.64650641360302,
1.66505235444365,1.70908280759338,1.73177956170391,1.73573300667775,1.73820045845035,
1.74012482527639,1.74225316210225,1.74574938287702,1.75844095315729,1.80939893074747,
1.84061062632473,1.84352373068957,1.84491235031177,1.84598745923835,1.84721601297642,
1.84936036343403,1.85867296999624,1.90783082486616,1.94322016748382,1.94751940897756,
1.95006212902028,1.95200343623404,1.95407689210245,1.95732468886643,1.9676233712772,
1.98415864175162,2.01702813681136,2.05272380342247,2.05558630847344,2.05696502449738,
2.05803910557485,2.05927396579576,2.06144706787455,2.07116845650035,2.12012418868578,
2.1552559962964,2.15955187855519,2.1620935793153,2.16403466548044,2.16610842539875,
2.16935782602938,2.17967109375628,2.19623881795404,2.2291346267226,2.264743987593,
2.26761022074736,2.26898963847532,2.27006375378906,2.27129807574626,2.27346885319651,
2.28315728077931,2.33213897684789,2.36727839141135,2.37157423670341,2.37411588053553,
2.37605690303558,2.37813057536138,2.38137979786745,2.39169215565431,2.40825809022025,
2.47089938433272,2.47226076536006,2.47843448250944,2.48037288284897,2.48155570093292,
2.48258738047931,2.48400047045733,2.48701554544795,2.49111375097756,2.50139218337894,
2.52421476761476,2.57592759698011,2.58291151628283,2.58579342020861,2.58758953893425,
2.58954938172231,2.59224514258579,2.59385008432844),.UNSPECIFIED.);
#1775=B_SPLINE_CURVE_WITH_KNOTS('',3,(#167456,#167457,#167458,#167459,#167460,
#167461,#167462,#167463,#167464,#167465,#167466,#167467,#167468,#167469,
#167470,#167471,#167472,#167473,#167474,#167475,#167476,#167477,#167478,
#167479,#167480,#167481,#167482,#167483,#167484,#167485,#167486,#167487,
#167488,#167489,#167490,#167491,#167492,#167493,#167494,#167495,#167496,
#167497,#167498,#167499,#167500,#167501,#167502,#167503,#167504,#167505,
#167506,#167507,#167508,#167509,#167510,#167511,#167512,#167513,#167514,
#167515,#167516,#167517,#167518,#167519,#167520,#167521,#167522,#167523,
#167524,#167525,#167526,#167527,#167528,#167529,#167530,#167531,#167532,
#167533,#167534,#167535,#167536,#167537,#167538,#167539,#167540,#167541,
#167542,#167543,#167544,#167545,#167546,#167547,#167548,#167549,#167550,
#167551,#167552,#167553,#167554,#167555,#167556,#167557,#167558,#167559,
#167560,#167561,#167562,#167563,#167564,#167565,#167566,#167567,#167568,
#167569,#167570,#167571,#167572,#167573,#167574,#167575,#167576,#167577,
#167578,#167579,#167580,#167581,#167582,#167583,#167584,#167585,#167586,
#167587,#167588,#167589,#167590,#167591,#167592,#167593,#167594,#167595,
#167596,#167597,#167598,#167599,#167600,#167601,#167602,#167603,#167604,
#167605,#167606,#167607,#167608,#167609,#167610,#167611,#167612,#167613,
#167614,#167615,#167616,#167617,#167618,#167619,#167620,#167621,#167622,
#167623,#167624,#167625,#167626,#167627,#167628,#167629,#167630,#167631,
#167632,#167633,#167634,#167635,#167636,#167637,#167638,#167639,#167640,
#167641,#167642,#167643,#167644,#167645,#167646,#167647,#167648,#167649,
#167650,#167651,#167652,#167653,#167654,#167655,#167656,#167657,#167658,
#167659,#167660,#167661,#167662,#167663,#167664,#167665,#167666,#167667,
#167668,#167669,#167670,#167671,#167672,#167673,#167674,#167675,#167676,
#167677,#167678,#167679,#167680,#167681,#167682,#167683,#167684,#167685,
#167686,#167687,#167688,#167689),.UNSPECIFIED.,.F.,.F.,(4,2,2,2,2,2,2,2,
2,2,2,2,2,2,2,2,2,2,2,2,2,2,2,2,2,2,2,2,2,2,2,2,2,2,2,2,2,2,2,2,2,2,2,2,
2,2,2,2,2,2,2,2,2,2,2,2,2,2,2,2,2,2,2,2,2,2,2,2,2,2,2,2,2,2,2,2,2,2,2,2,
2,2,2,2,2,2,2,2,2,2,2,2,2,2,2,2,2,2,2,2,2,2,2,2,2,2,2,2,2,2,2,2,2,2,2,2,
4),(0.0751664254368708,0.121845955344527,0.131682137292399,0.133862665319429,
0.135098937946201,0.136172458199343,0.137548108280382,0.140396202121225,
0.176828797185436,0.209403310472754,0.225624337256069,0.232373911160273,
0.237516241657923,0.239979328300749,0.241820421564232,0.243647570729462,
0.246191314375334,0.252844260980652,0.308554353084904,0.3327085642093,0.343555926381325,
0.345801361990051,0.347051910603007,0.348123827059192,0.349479426759677,
0.351623526946022,0.362637199903487,0.413913723232091,0.442560878010676,
0.448987785534373,0.451695383130414,0.453656921841771,0.455449838961509,
0.458316220325194,0.46520904244774,0.518210971510428,0.544202176327027,
0.555530343689891,0.557804126181521,0.559060855862157,0.560132218997533,
0.561479664165487,0.564099783774063,0.580115853324613,0.58515641325212,
0.629885439006828,0.64840508235415,0.659579457989206,0.662923756175396,
0.665018220058885,0.666951401558858,0.669444265585323,0.673573516242521,
0.700875431160467,0.743135477132519,0.759411357262032,0.7678548497415,0.769932722873498,
0.771146409166725,0.772224103332976,0.773613375875094,0.775918769636958,
0.789939218927439,0.791301065984591,0.798313691139858,0.811988689662026,
0.844849708791797,0.861411252811406,0.871722501364627,0.874971474260879,
0.877045017688488,0.878985941435396,0.881527488775433,0.885823276629063,
0.920955665558956,0.969902203516858,0.97966107016502,0.981836679738371,
0.983072047071761,0.984145986284646,0.985523748320218,0.988381628690608,
1.01124176969533,1.02400706443002,1.05686282156235,1.07341556753015,1.08372313553391,
1.08697190544598,1.08904554928356,1.09098672857402,1.09352884366621,1.09782611376155,
1.13304085164816,1.18224625769595,1.19171023916762,1.19386546313084,1.19509642480876,
1.19617116604592,1.19755604375425,1.19979618151898,1.21249759832307,1.2348756064397,
1.26847944014398,1.29385667535051,1.2981273832955,1.30042491787518,1.30231799097671,
1.30455873716748,1.30845790255933,1.32436660850639,1.33458886721821,1.37387326870316,
1.40245749186511,1.40537004963331,1.40675860124106,1.40783374616902,1.40876564968185),
 .UNSPECIFIED.);
#1776=B_SPLINE_CURVE_WITH_KNOTS('',3,(#167695,#167696,#167697,#167698,#167699,
#167700,#167701,#167702,#167703,#167704,#167705,#167706,#167707,#167708,
#167709,#167710,#167711,#167712,#167713,#167714,#167715,#167716),
 .UNSPECIFIED.,.F.,.F.,(4,2,2,2,2,2,2,2,2,2,4),(2.59321272354364,2.59676257810928,
2.60140795147772,2.60313777369838,2.60416108640238,2.60525490880966,2.6067734902191,
2.61040446374374,2.61551550281731,2.62968314141178,2.66731559418949),
 .UNSPECIFIED.);
#1777=B_SPLINE_CURVE_WITH_KNOTS('',3,(#167717,#167718,#167719,#167720,#167721,
#167722,#167723,#167724,#167725,#167726,#167727,#167728,#167729,#167730,
#167731,#167732,#167733,#167734,#167735,#167736,#167737,#167738,#167739,
#167740,#167741,#167742,#167743,#167744,#167745,#167746,#167747,#167748,
#167749,#167750,#167751,#167752,#167753,#167754,#167755,#167756,#167757,
#167758,#167759,#167760,#167761,#167762,#167763,#167764,#167765,#167766,
#167767,#167768,#167769,#167770,#167771,#167772,#167773,#167774,#167775,
#167776,#167777,#167778,#167779,#167780,#167781,#167782,#167783,#167784,
#167785,#167786,#167787,#167788,#167789,#167790,#167791,#167792,#167793,
#167794,#167795,#167796,#167797,#167798,#167799,#167800,#167801,#167802,
#167803,#167804,#167805,#167806,#167807,#167808,#167809,#167810,#167811,
#167812,#167813,#167814,#167815,#167816,#167817,#167818,#167819,#167820,
#167821,#167822,#167823,#167824,#167825,#167826,#167827,#167828,#167829,
#167830,#167831,#167832,#167833,#167834,#167835,#167836,#167837,#167838,
#167839,#167840,#167841,#167842,#167843,#167844,#167845,#167846,#167847,
#167848,#167849,#167850,#167851,#167852,#167853,#167854,#167855,#167856,
#167857,#167858,#167859,#167860,#167861,#167862,#167863,#167864,#167865,
#167866,#167867,#167868,#167869,#167870,#167871,#167872,#167873,#167874,
#167875,#167876,#167877,#167878,#167879,#167880,#167881,#167882,#167883,
#167884,#167885,#167886,#167887,#167888,#167889,#167890,#167891,#167892,
#167893,#167894,#167895,#167896,#167897,#167898,#167899,#167900,#167901,
#167902,#167903,#167904,#167905,#167906,#167907,#167908,#167909,#167910,
#167911,#167912,#167913,#167914,#167915,#167916,#167917,#167918,#167919,
#167920,#167921,#167922,#167923,#167924,#167925,#167926,#167927,#167928,
#167929,#167930,#167931,#167932,#167933,#167934,#167935,#167936,#167937,
#167938,#167939,#167940,#167941,#167942,#167943,#167944),.UNSPECIFIED.,
 .F.,.F.,(4,2,2,2,2,2,2,2,2,2,2,2,2,2,2,2,2,2,2,2,2,2,2,2,2,2,2,2,2,2,2,
2,2,2,2,2,2,2,2,2,2,2,2,2,2,2,2,2,2,2,2,2,2,2,2,2,2,2,2,2,2,2,2,2,2,2,2,
2,2,2,2,2,2,2,2,2,2,2,2,2,2,2,2,2,2,2,2,2,2,2,2,2,2,2,2,2,2,2,2,2,2,2,2,
2,2,2,2,2,2,2,2,2,2,4),(0.000704182981740823,0.025717628190997,0.0359848718289681,
0.03906358535599,0.0411898775184007,0.0432710250581594,0.0452083866403788,
0.0477299960570225,0.0519581881395003,0.0833517469152109,0.108702852437119,
0.13665961579832,0.145914702164939,0.148054314070839,0.14928151697485,0.150356340023211,
0.151745763369213,0.15400201116064,0.167029448661604,0.188640582450494,
0.215343078701711,0.236968499593147,0.245192539158449,0.251206096285135,
0.253833976559155,0.25579066677997,0.257588990735752,0.260485650014074,
0.267562362499414,0.317897166975829,0.355567136046225,0.359165334448484,
0.360678274131995,0.361771027273397,0.362795721022258,0.364532931729908,
0.369227564009042,0.410091366748055,0.456727973956269,0.46312059249124,
0.465822275557283,0.467782639577261,0.469576627552671,0.472449398259115,
0.479381808821687,0.531832612605671,0.558205643024063,0.56963007483175,
0.571909234692174,0.573167077321925,0.5742382634427,0.57558405490196,0.578196760828911,
0.594049725598797,0.598811519778327,0.614071539478433,0.646947531783168,
0.663529264405269,0.673849382583489,0.677099182913534,0.679172782068762,
0.681113426283792,0.683654129139571,0.687947417560457,0.730346714312759,
0.759401303224733,0.774125195971442,0.782017724573933,0.784049651902801,
0.785253088016879,0.786333171619793,0.787740579140585,0.790108030106355,
0.805546523747528,0.812261789130739,0.826060561359919,0.858921261247343,
0.875483540258535,0.885794984344839,0.889043879387732,0.89111733961951,
0.893058161954385,0.895599542539845,0.899894972422117,0.935014387027832,
0.98392412590432,0.99372333135132,0.995901622710922,0.997137542667392,0.998211341754463,
0.999588113337181,1.00244115227971,1.02511108920957,1.03806701684262,1.07092292722108,
1.0874769840124,1.09778500748103,1.10103372883791,1.103107295508,1.10504837011985,
1.10759030131288,1.11188715558912,1.14708420180628,1.19623358777709,1.20575895584113,
1.20791844347136,1.2091503073185,1.21022484475367,1.21160815732742,1.21384321294934,
1.22644914254929,1.23298243684644,1.23811588181959,1.25997501180952),
 .UNSPECIFIED.);
#1778=B_SPLINE_CURVE_WITH_KNOTS('',3,(#167946,#167947,#167948,#167949,#167950,
#167951,#167952,#167953,#167954,#167955,#167956,#167957,#167958,#167959,
#167960,#167961,#167962,#167963,#167964,#167965,#167966,#167967,#167968,
#167969,#167970,#167971,#167972,#167973,#167974,#167975,#167976,#167977,
#167978,#167979,#167980,#167981,#167982,#167983,#167984,#167985,#167986,
#167987,#167988,#167989,#167990,#167991,#167992,#167993,#167994,#167995,
#167996,#167997,#167998,#167999,#168000,#168001,#168002,#168003,#168004,
#168005,#168006,#168007,#168008,#168009,#168010,#168011,#168012,#168013,
#168014,#168015,#168016,#168017,#168018,#168019,#168020,#168021,#168022,
#168023,#168024,#168025,#168026,#168027,#168028,#168029,#168030,#168031,
#168032,#168033,#168034,#168035,#168036,#168037,#168038,#168039,#168040,
#168041,#168042,#168043,#168044,#168045,#168046,#168047,#168048,#168049,
#168050,#168051,#168052,#168053,#168054,#168055,#168056,#168057,#168058,
#168059,#168060,#168061,#168062,#168063,#168064,#168065,#168066,#168067,
#168068,#168069,#168070,#168071,#168072,#168073,#168074,#168075,#168076,
#168077,#168078,#168079,#168080,#168081,#168082,#168083,#168084,#168085,
#168086,#168087,#168088,#168089,#168090,#168091,#168092,#168093,#168094,
#168095,#168096,#168097,#168098,#168099,#168100,#168101,#168102,#168103,
#168104,#168105,#168106,#168107,#168108,#168109,#168110,#168111,#168112,
#168113,#168114,#168115,#168116,#168117,#168118,#168119,#168120,#168121,
#168122,#168123,#168124,#168125,#168126,#168127,#168128,#168129,#168130,
#168131,#168132,#168133,#168134,#168135,#168136,#168137,#168138,#168139,
#168140,#168141,#168142,#168143,#168144,#168145,#168146,#168147,#168148,
#168149,#168150,#168151,#168152,#168153,#168154,#168155,#168156,#168157,
#168158,#168159,#168160,#168161,#168162,#168163,#168164,#168165,#168166,
#168167,#168168,#168169,#168170,#168171,#168172,#168173,#168174,#168175,
#168176,#168177),.UNSPECIFIED.,.F.,.F.,(4,2,2,2,2,2,2,2,2,2,2,2,2,2,2,2,
2,2,2,2,2,2,2,2,2,2,2,2,2,2,2,2,2,2,2,2,2,2,2,2,2,2,2,2,2,2,2,2,2,2,2,2,
2,2,2,2,2,2,2,2,2,2,2,2,2,2,2,2,2,2,2,2,2,2,2,2,2,2,2,2,2,2,2,2,2,2,2,2,
2,2,2,2,2,2,2,2,2,2,2,2,2,2,2,2,2,2,2,2,2,2,2,2,2,2,2,4),(1.40876564968185,
1.40906244022885,1.41120726800264,1.42052554231052,1.46970202397115,1.5050712140085,
1.50937039427449,1.51191315663174,1.51385454135423,1.515928123814,1.51917621027683,
1.52947658062611,1.54601529218143,1.57356209642858,1.58970472045944,1.60078604712632,
1.61502103630848,1.61733761851502,1.61873029225954,1.61980856900322,1.62102062135248,
1.62309056749968,1.63143339162205,1.64741594131852,1.68973078454812,1.71734618386345,
1.72148384944831,1.7239794219376,1.72591328751353,1.72800707843134,1.73134723872194,
1.74247911383865,1.76090129375285,1.80769700377346,1.81248095721591,1.82701279929761,
1.82934290764825,1.83073956473504,1.83181838361534,1.83302820823886,1.83508805560075,
1.84330745271654,1.8589384169442,1.9007140705049,1.9293168194412,1.93348063663692,
1.93598391032542,1.93791897929598,1.94000933801229,1.9433338187686,1.95431945620387,
1.97240346137979,2.02247902304394,2.03890900988,2.04154614361546,2.04289744429846,
2.04396931159355,2.04522367799794,2.04748570091486,2.05860471830522,2.08377710415533,
2.13794821256296,2.14474594974472,2.14759707900135,2.14938756027183,2.15135218195495,
2.15407462077514,2.160587350901,2.18995687257223,2.23282297953381,2.25087240414281,
2.25356874959489,2.25493267721593,2.25600547090369,2.25725052298043,2.25946996388073,
2.26989206621916,2.29249681398209,2.35060633464067,2.35699003053181,2.35949049399086,
2.3613065689382,2.36325164626465,2.3658626526649,2.37173323864884,2.39592146672386,
2.44361404677803,2.46288490292848,2.46565407641264,2.46701432736083,2.46805600265418,
2.46806008033713,2.46806408942824,2.46806803122212,2.46807190727129,2.4680755060714,
2.4680790912502,2.46808266308603,2.46808622159869,2.46808976703347,2.46931345131289,
2.47062483679419,2.47264882762886,2.47646415089008,2.48574693661712,2.52369343304925,
2.53806500336148,2.56552438768444,2.56965801232864,2.57215240472521,2.57408610132007,
2.57618045330948,2.57952311983,2.59067836207953,2.60915478976905,2.66836429282343),
 .UNSPECIFIED.);
#1779=B_SPLINE_CURVE_WITH_KNOTS('',3,(#168178,#168179,#168180,#168181,#168182,
#168183,#168184,#168185,#168186,#168187,#168188,#168189,#168190,#168191,
#168192,#168193,#168194,#168195,#168196,#168197,#168198,#168199),
 .UNSPECIFIED.,.F.,.F.,(4,2,2,2,2,2,2,2,2,2,4),(0.000810719349047726,0.00554260972535774,
0.00881069122763486,0.0102445713069489,0.0113189801030348,0.0123417965676871,
0.0133649983883814,0.0148060144441036,0.0186526135973435,0.0263910041242044,
0.0750784321551894),.UNSPECIFIED.);
#1780=B_SPLINE_CURVE_WITH_KNOTS('',3,(#168204,#168205,#168206,#168207,#168208,
#168209,#168210,#168211,#168212,#168213,#168214,#168215,#168216,#168217,
#168218,#168219,#168220,#168221,#168222,#168223,#168224,#168225,#168226,
#168227,#168228,#168229,#168230,#168231,#168232,#168233,#168234,#168235,
#168236,#168237,#168238,#168239,#168240,#168241,#168242,#168243,#168244,
#168245,#168246,#168247,#168248,#168249,#168250,#168251,#168252,#168253,
#168254,#168255,#168256,#168257,#168258,#168259,#168260,#168261,#168262,
#168263,#168264,#168265,#168266,#168267,#168268,#168269,#168270,#168271,
#168272,#168273,#168274,#168275,#168276,#168277,#168278,#168279,#168280,
#168281,#168282,#168283,#168284,#168285,#168286,#168287,#168288,#168289,
#168290,#168291,#168292,#168293,#168294,#168295,#168296,#168297,#168298,
#168299,#168300,#168301,#168302,#168303,#168304,#168305,#168306,#168307,
#168308,#168309,#168310,#168311,#168312,#168313,#168314,#168315,#168316,
#168317,#168318,#168319,#168320,#168321,#168322,#168323,#168324,#168325,
#168326,#168327,#168328,#168329,#168330,#168331,#168332,#168333,#168334,
#168335,#168336,#168337,#168338,#168339,#168340,#168341,#168342,#168343,
#168344,#168345,#168346,#168347,#168348,#168349,#168350,#168351,#168352,
#168353,#168354,#168355,#168356,#168357,#168358,#168359,#168360,#168361,
#168362,#168363,#168364,#168365,#168366,#168367,#168368,#168369,#168370,
#168371,#168372,#168373,#168374,#168375,#168376,#168377,#168378,#168379,
#168380,#168381,#168382,#168383,#168384,#168385,#168386,#168387,#168388,
#168389,#168390,#168391,#168392,#168393,#168394,#168395,#168396,#168397,
#168398,#168399,#168400,#168401,#168402,#168403,#168404,#168405,#168406,
#168407,#168408,#168409,#168410,#168411,#168412,#168413,#168414,#168415,
#168416,#168417,#168418,#168419,#168420,#168421,#168422,#168423,#168424,
#168425,#168426,#168427,#168428,#168429,#168430,#168431,#168432,#168433),
 .UNSPECIFIED.,.F.,.F.,(4,2,2,2,2,2,2,2,2,2,2,2,2,2,2,2,2,2,2,2,2,2,2,2,
2,2,2,2,2,2,2,2,2,2,2,2,2,2,2,2,2,2,2,2,2,2,2,2,2,2,2,2,2,2,2,2,2,2,2,2,
2,2,2,2,2,2,2,2,2,2,2,2,2,2,2,2,2,2,2,2,2,2,2,2,2,2,2,2,2,2,2,2,2,2,2,2,
2,2,2,2,2,2,2,2,2,2,2,2,2,2,2,2,2,2,4),(1.25962401162403,1.26430974686983,
1.30525389854892,1.32773367756853,1.33039711422683,1.33173595952838,1.33270394114661,
1.33392756104424,1.33605009385992,1.34506885777096,1.36305411295081,1.41326996295484,
1.43107393322947,1.4347534136824,1.437137055044,1.43905255572398,1.44123132513247,
1.44495617516341,1.46036268422653,1.5116976762596,1.53937698828192,1.54228396149099,
1.54367128031833,1.54474613001321,1.54597522474859,1.54812248357969,1.55747820401669,
1.60674401211132,1.64196762190877,1.64626431184035,1.6488061194656,1.65074707361159,
1.65282048538134,1.65606890812334,1.66637542844875,1.68292884799442,1.7158108880148,
1.72925743961491,1.73684334193375,1.75184032035586,1.75418981295129,1.75559200684074,
1.7566714028084,1.75787776328051,1.75992267393493,1.76796661948303,1.78310657436369,
1.82281314578867,1.85404667218651,1.85827194568919,1.86079294472355,1.86273048562428,
1.86481246113277,1.8681000653812,1.87875349925591,1.8960818523767,1.94430089592049,
1.94860187229289,1.95167182499473,1.96405441542428,1.96627741309421,1.96765698675116,
1.96873102171676,1.96996502397064,1.97213469744821,1.98180935212029,2.03079696332603,
2.06593626548011,2.07023171975053,2.0727731185893,2.07471394613278,2.07678740255964,
2.08003627086668,2.09034737039031,2.10691115606774,2.13980106738308,2.15412310478184,
2.15979001781808,2.1757365431188,2.17835279667591,2.17969939104971,2.1807706760656,
2.18202801382229,2.18430466643489,2.19568412361328,2.22187539247344,2.2745466783258,
2.28146129242589,2.28433122035439,2.28612475724525,2.28808569654836,2.29079011932666,
2.29719838256437,2.30603771755433,2.35731649014562,2.38733951594719,2.39025396021666,
2.39164264936553,2.392717550224,2.39394557333261,2.39608831184729,2.40538332880179,
2.42422703132016,2.47041776955285,2.47187665102907,2.49090040361457,2.49466012115544,
2.4970683558831,2.49898594683945,2.50078321080397,2.50387581650965,2.51342015358757,
2.52841976651408,2.55071276904625,2.59321272354364),.UNSPECIFIED.);
#1781=B_SPLINE_CURVE_WITH_KNOTS('',3,(#168434,#168435,#168436,#168437,#168438,
#168439,#168440,#168441,#168442,#168443,#168444,#168445,#168446,#168447,
#168448,#168449,#168450,#168451,#168452,#168453,#168454,#168455,#168456,
#168457,#168458,#168459,#168460,#168461,#168462,#168463,#168464,#168465,
#168466,#168467,#168468,#168469,#168470,#168471,#168472,#168473,#168474,
#168475,#168476,#168477,#168478,#168479,#168480,#168481,#168482,#168483,
#168484,#168485,#168486,#168487,#168488,#168489,#168490,#168491,#168492,
#168493,#168494,#168495,#168496,#168497,#168498,#168499,#168500,#168501,
#168502,#168503,#168504,#168505,#168506,#168507,#168508,#168509,#168510,
#168511,#168512,#168513,#168514,#168515,#168516,#168517,#168518,#168519,
#168520,#168521,#168522,#168523,#168524,#168525,#168526,#168527,#168528,
#168529,#168530,#168531,#168532,#168533,#168534,#168535,#168536,#168537,
#168538,#168539,#168540,#168541,#168542,#168543,#168544,#168545,#168546,
#168547,#168548,#168549,#168550,#168551,#168552,#168553,#168554,#168555,
#168556,#168557,#168558,#168559,#168560,#168561,#168562,#168563,#168564,
#168565,#168566,#168567,#168568,#168569,#168570,#168571,#168572,#168573,
#168574,#168575,#168576,#168577,#168578,#168579,#168580,#168581,#168582,
#168583,#168584,#168585,#168586,#168587,#168588,#168589,#168590,#168591,
#168592,#168593,#168594,#168595,#168596,#168597,#168598,#168599,#168600,
#168601,#168602,#168603,#168604,#168605,#168606,#168607,#168608,#168609,
#168610,#168611,#168612,#168613,#168614,#168615,#168616,#168617,#168618,
#168619,#168620,#168621,#168622,#168623,#168624,#168625,#168626,#168627,
#168628,#168629,#168630,#168631,#168632,#168633,#168634,#168635,#168636,
#168637,#168638,#168639,#168640,#168641,#168642,#168643,#168644,#168645,
#168646,#168647,#168648,#168649,#168650,#168651,#168652,#168653,#168654,
#168655,#168656,#168657,#168658,#168659,#168660,#168661,#168662,#168663,
#168664,#168665,#168666,#168667,#168668,#168669),.UNSPECIFIED.,.F.,.F.,
(4,2,2,2,2,2,2,2,2,2,2,2,2,2,2,2,2,2,2,2,2,2,2,2,2,2,2,2,2,2,2,2,2,2,2,
2,2,2,2,2,2,2,2,2,2,2,2,2,2,2,2,2,2,2,2,2,2,2,2,2,2,2,2,2,2,2,2,2,2,2,2,
2,2,2,2,2,2,2,2,2,2,2,2,2,2,2,2,2,2,2,2,2,2,2,2,2,2,2,2,2,2,2,2,2,2,2,2,
2,2,2,2,2,2,2,2,2,2,4),(0.0750784321551894,0.0856872623994721,0.102193393147575,
0.112478518569802,0.115723726458095,0.117795941871022,0.119736378108385,
0.122278377924875,0.12657737730363,0.170030212772573,0.206390717145988,
0.215473289989933,0.219229765834113,0.221231249014688,0.22253308265916,
0.22374714081406,0.224790570685267,0.226140989918893,0.228775973475969,
0.245124041647403,0.289987075516811,0.319112007183808,0.325594883103514,
0.328311510938096,0.330274343106106,0.332064843634442,0.334919559901776,
0.34174405124641,0.395569126131839,0.420976331839343,0.432153467138812,
0.434418128315438,0.435672693654804,0.436743963674678,0.438093525868189,
0.440724353832407,0.456997756690263,0.507260214488163,0.525272304700002,
0.536226338249603,0.539546395202698,0.541635149565268,0.543569540359618,
0.546073074719094,0.55023983799993,0.579007410580277,0.620668305417106,
0.636259006936096,0.644462203559628,0.646520103232366,0.64772915482517,
0.648807545384551,0.650203973910826,0.652534381872989,0.6670915941988,0.675376366596123,
0.688562202379701,0.72140976150465,0.74414487954246,0.749822061529322,0.752397424511272,
0.75433626897467,0.7561613738279,0.75869792794741,0.765306350934032,0.821450195604848,
0.845310809628617,0.856078281621258,0.858318666635289,0.859568018740797,
0.860639907305439,0.861996752433854,0.864661200746954,0.881832375376879,
0.927325018123464,0.955180081594329,0.96151148229728,0.964202698482331,
0.966161128059916,0.96795726576907,0.970842073309733,0.977847705744469,
1.02918016800007,1.05634711330801,1.0679686894587,1.07025886091832,1.07151906264762,
1.07259001773328,1.07393267901382,1.07653102435352,1.09204096082917,1.09861454965795,
1.13998978460787,1.16725276669186,1.17351215268915,1.17619110497389,1.17814741784952,
1.17994635503659,1.18284612572453,1.18994112421196,1.23956648931162,1.27794079158437,
1.28152639688112,1.28303722127884,1.28412963324536,1.28515495154683,1.28689523444239,
1.29160989292968,1.33201667301647,1.33390594999482,1.37772798415467,1.38494942829632,
1.38787046320037,1.38967335423326,1.39162670736977,1.39428857074071,1.40044887524773,
1.40839008782515),.UNSPECIFIED.);
#1782=B_SPLINE_CURVE_WITH_KNOTS('',3,(#168675,#168676,#168677,#168678),
 .UNSPECIFIED.,.F.,.F.,(4,4),(152.105783788367,152.455231433536),
 .UNSPECIFIED.);
#1783=B_SPLINE_CURVE_WITH_KNOTS('',3,(#168679,#168680,#168681,#168682,#168683,
#168684,#168685,#168686,#168687,#168688,#168689,#168690,#168691,#168692,
#168693,#168694,#168695,#168696,#168697,#168698,#168699,#168700,#168701,
#168702,#168703,#168704,#168705,#168706,#168707,#168708,#168709,#168710,
#168711,#168712,#168713,#168714,#168715,#168716,#168717,#168718,#168719,
#168720,#168721,#168722,#168723,#168724,#168725,#168726,#168727,#168728,
#168729,#168730,#168731,#168732,#168733,#168734,#168735,#168736,#168737,
#168738,#168739,#168740,#168741,#168742,#168743,#168744,#168745,#168746,
#168747,#168748,#168749,#168750,#168751,#168752,#168753,#168754,#168755,
#168756,#168757,#168758,#168759,#168760,#168761,#168762,#168763,#168764,
#168765,#168766,#168767,#168768,#168769,#168770,#168771,#168772,#168773,
#168774,#168775,#168776,#168777,#168778,#168779,#168780,#168781,#168782,
#168783,#168784,#168785,#168786,#168787,#168788,#168789,#168790,#168791,
#168792,#168793,#168794,#168795,#168796,#168797,#168798,#168799,#168800,
#168801,#168802,#168803,#168804,#168805,#168806,#168807,#168808,#168809,
#168810,#168811,#168812,#168813,#168814,#168815,#168816,#168817,#168818,
#168819,#168820,#168821,#168822,#168823,#168824,#168825,#168826,#168827,
#168828,#168829,#168830,#168831,#168832,#168833,#168834,#168835,#168836,
#168837,#168838,#168839,#168840,#168841,#168842,#168843,#168844,#168845,
#168846,#168847,#168848,#168849,#168850,#168851,#168852,#168853,#168854,
#168855,#168856,#168857,#168858,#168859,#168860,#168861,#168862,#168863,
#168864,#168865,#168866,#168867,#168868,#168869,#168870,#168871,#168872,
#168873,#168874,#168875,#168876,#168877,#168878,#168879,#168880,#168881,
#168882,#168883,#168884,#168885,#168886,#168887,#168888,#168889,#168890,
#168891,#168892,#168893,#168894,#168895,#168896,#168897,#168898,#168899,
#168900,#168901,#168902,#168903,#168904),.UNSPECIFIED.,.F.,.F.,(4,2,2,2,
2,2,2,2,2,2,2,2,2,2,2,2,2,2,2,2,2,2,2,2,2,2,2,2,2,2,2,2,2,2,2,2,2,2,2,2,
2,2,2,2,2,2,2,2,2,2,2,2,2,2,2,2,2,2,2,2,2,2,2,2,2,2,2,2,2,2,2,2,2,2,2,2,
2,2,2,2,2,2,2,2,2,2,2,2,2,2,2,2,2,2,2,2,2,2,2,2,2,2,2,2,2,2,2,2,2,2,2,2,
4),(0.000629332229582586,0.0482573633288315,0.0568193170551446,0.0589064612736026,
0.0601221095219334,0.0611992138773799,0.062584716532025,0.0648776103157659,
0.0786443976343827,0.120752779311643,0.14613932269728,0.159987626849096,
0.163516551337431,0.165693677576201,0.167609091198328,0.169994401368663,
0.173679853376456,0.191581938916001,0.198098502048847,0.242174718696393,
0.267696256798199,0.270413011096965,0.271762538844294,0.272833962575786,
0.274088923348135,0.276294079630585,0.285361610131089,0.288512788438226,
0.292119880904416,0.299321262310599,0.344360823284317,0.361848219246277,
0.372572793949327,0.375868084933978,0.377951621868027,0.379888330021888,
0.382404997095814,0.386615880088181,0.417193768036229,0.447298528592423,
0.470014542107235,0.480465934499665,0.482686756419762,0.48393186660931,
0.485004267210109,0.486367114909076,0.488535210969449,0.499945914043641,
0.504034520254718,0.504274790767321,0.511101106317111,0.524851430062145,
0.557709293246772,0.574269799213613,0.584580239844121,0.587828872151129,
0.589902177540771,0.591842863955748,0.594384079573048,0.59867925978644,
0.633800476137799,0.68271983574467,0.692502772744039,0.694679846759915,
0.695915445100066,0.696989200845538,0.698366225332436,0.700580854735983,
0.712810635935287,0.762460585500933,0.791343503503508,0.797798556630073,
0.800510952929573,0.802473412959469,0.804265417018526,0.807126526334425,
0.813986937857747,0.867411151635365,0.89311122459648,0.904365135933374,
0.906634695762748,0.907890533747698,0.908962013437402,0.910310722116163,
0.912936588292257,0.929095934771815,0.929561755882191,0.973907069665223,
1.00327706802672,1.00978979739154,1.01251194992555,1.01447626492199,1.0162664021171,
1.01911683260179,1.0259121107722,1.0801223800764,1.1052865151388,1.11640193197941,
1.11866349939461,1.11991763664288,1.12098932616527,1.12234041909693,1.12497719842511,
1.14140829716088,1.19199685838209,1.20970840693508,1.22053206228131,1.22383857175399,
1.22592477151939,1.22786090190283,1.23037249208948,1.23456537884827,1.25962401162403),
 .UNSPECIFIED.);
#1784=B_SPLINE_CURVE_WITH_KNOTS('',3,(#168906,#168907,#168908,#168909,#168910,
#168911,#168912,#168913,#168914,#168915,#168916,#168917,#168918,#168919,
#168920,#168921,#168922,#168923,#168924,#168925,#168926,#168927,#168928,
#168929,#168930,#168931,#168932,#168933,#168934,#168935,#168936,#168937,
#168938,#168939,#168940,#168941,#168942,#168943,#168944,#168945,#168946,
#168947,#168948,#168949,#168950,#168951,#168952,#168953,#168954,#168955,
#168956,#168957,#168958,#168959,#168960,#168961,#168962,#168963,#168964,
#168965,#168966,#168967,#168968,#168969,#168970,#168971,#168972,#168973,
#168974,#168975,#168976,#168977,#168978,#168979,#168980,#168981,#168982,
#168983,#168984,#168985,#168986,#168987,#168988,#168989,#168990,#168991,
#168992,#168993,#168994,#168995,#168996,#168997,#168998,#168999,#169000,
#169001,#169002,#169003,#169004,#169005,#169006,#169007,#169008,#169009,
#169010,#169011,#169012,#169013,#169014,#169015,#169016,#169017,#169018,
#169019,#169020,#169021,#169022,#169023,#169024,#169025,#169026,#169027,
#169028,#169029,#169030,#169031,#169032,#169033,#169034,#169035,#169036,
#169037,#169038,#169039,#169040,#169041,#169042,#169043,#169044,#169045,
#169046,#169047,#169048,#169049,#169050,#169051,#169052,#169053,#169054,
#169055,#169056,#169057,#169058,#169059,#169060,#169061,#169062,#169063,
#169064,#169065,#169066,#169067,#169068,#169069,#169070,#169071,#169072,
#169073,#169074,#169075,#169076,#169077,#169078,#169079,#169080,#169081,
#169082,#169083,#169084,#169085,#169086,#169087,#169088,#169089,#169090,
#169091,#169092,#169093,#169094,#169095,#169096,#169097,#169098,#169099,
#169100,#169101,#169102,#169103,#169104,#169105,#169106,#169107,#169108,
#169109,#169110,#169111,#169112,#169113,#169114,#169115,#169116,#169117,
#169118,#169119,#169120,#169121,#169122,#169123,#169124,#169125),
 .UNSPECIFIED.,.F.,.F.,(4,2,2,2,2,2,2,2,2,2,2,2,2,2,2,2,2,2,2,2,2,2,2,2,
2,2,2,2,2,2,2,2,2,2,2,2,2,2,2,2,2,2,2,2,2,2,2,2,2,2,2,2,2,2,2,2,2,2,2,2,
2,2,2,2,2,2,2,2,2,2,2,2,2,2,2,2,2,2,2,2,2,2,2,2,2,2,2,2,2,2,2,2,2,2,2,2,
2,2,2,2,2,2,2,2,2,2,2,2,2,4),(1.40839008782515,1.42691295402479,1.46582634767065,
1.47396801211054,1.491240619284,1.49390897104638,1.49526669837756,1.49633871234769,
1.49758756100695,1.49982541509922,1.51055030637073,1.53425079338281,1.56162148035616,
1.59355075685834,1.59778999759066,1.60031497971922,1.60225305038923,1.60433311502111,
1.60761245417449,1.61819321096669,1.6353583907911,1.68108903783519,1.68786757938709,
1.70330445862708,1.70567189461123,1.70707928880048,1.70815936140263,1.70936279676019,
1.7113947314429,1.71928758134134,1.73401038903081,1.76304115779599,1.80542080777784,
1.80971357198255,1.81225412704556,1.81419474103193,1.81626838716067,1.81951842550255,
1.8298406023543,1.84642919553635,1.87933877755081,1.89535760794404,1.89906704082739,
1.91519272937833,1.91782051739067,1.91916955752039,1.92024095617011,1.92149630652645,
1.92376397963471,1.93498869485887,1.96057453365421,2.01411249530492,2.02095981388174,
2.02381858724575,2.02561003931624,2.02757263529074,2.03028657357222,2.03675173263053,
2.09085791764579,2.12691082377215,2.12977136490755,2.13114950752416,2.1322233166408,
2.13345806132456,2.13563143076813,2.14536175323461,2.19429673867642,2.22943289517577,
2.23371909577794,2.23625769081201,2.2381979174631,2.24027222715142,2.24352555853709,
2.25387725649414,2.2705314948256,2.30349473002634,2.32242311388581,2.32484986247365,
2.33931586075786,2.34164253155749,2.34303795371653,2.34411632436838,2.34532621080509,
2.34738741397025,2.35562855478718,2.37132356966962,2.41418052996645,2.44164464922037,
2.44613896165899,2.44853219799288,2.45039850434395,2.45250822153758,2.45472513303732,
2.45802319933091,2.50312882243945,2.54811753459776,2.5528410366246,2.55458266001092,
2.55560824090958,2.55670048669667,2.55821035269146,2.56179035326915,2.59939070000387,
2.64830575180194,2.65646873999949,2.65954002493247,2.6613713531806,2.66321533633006,
2.66550720848957,2.66757157114197),.UNSPECIFIED.);
#1785=B_SPLINE_CURVE_WITH_KNOTS('',3,(#169126,#169127,#169128,#169129,#169130,
#169131,#169132,#169133,#169134,#169135),.UNSPECIFIED.,.F.,.F.,(4,2,2,2,
4),(0.000823830745865882,0.00400944464107275,0.0104637662401864,0.0609495485411902,
0.0751148559371182),.UNSPECIFIED.);
#1786=B_SPLINE_CURVE_WITH_KNOTS('',3,(#169141,#169142,#169143,#169144,#169145,
#169146),.UNSPECIFIED.,.F.,.F.,(4,2,4),(2.59315594695257,2.608916316382,
2.66742168368829),.UNSPECIFIED.);
#1787=B_SPLINE_CURVE_WITH_KNOTS('',3,(#169147,#169148,#169149,#169150,#169151,
#169152,#169153,#169154,#169155,#169156),.UNSPECIFIED.,.F.,.F.,(4,1,1,1,
1,1,1,4),(152.455231433536,152.821976844167,153.820813294129,154.819649744091,
155.818486194052,156.817322644014,157.816159093976,158.388969095546),
 .UNSPECIFIED.);
#1788=B_SPLINE_CURVE_WITH_KNOTS('',3,(#169157,#169158,#169159,#169160,#169161,
#169162,#169163,#169164,#169165,#169166,#169167,#169168,#169169,#169170,
#169171,#169172,#169173,#169174,#169175,#169176,#169177,#169178,#169179,
#169180,#169181,#169182,#169183,#169184,#169185,#169186,#169187,#169188,
#169189,#169190,#169191,#169192,#169193,#169194,#169195,#169196,#169197,
#169198,#169199,#169200,#169201,#169202,#169203,#169204,#169205,#169206,
#169207,#169208,#169209,#169210,#169211,#169212,#169213,#169214,#169215,
#169216,#169217,#169218,#169219,#169220,#169221,#169222,#169223,#169224,
#169225,#169226,#169227,#169228,#169229,#169230,#169231,#169232,#169233,
#169234,#169235,#169236,#169237,#169238,#169239,#169240,#169241,#169242,
#169243,#169244,#169245,#169246,#169247,#169248,#169249,#169250,#169251,
#169252,#169253,#169254,#169255,#169256,#169257,#169258,#169259,#169260,
#169261,#169262,#169263,#169264,#169265,#169266,#169267,#169268,#169269,
#169270,#169271,#169272,#169273,#169274,#169275,#169276,#169277,#169278,
#169279,#169280,#169281,#169282,#169283,#169284,#169285,#169286,#169287,
#169288,#169289,#169290,#169291,#169292,#169293,#169294,#169295,#169296,
#169297,#169298,#169299,#169300,#169301,#169302,#169303,#169304,#169305,
#169306,#169307,#169308,#169309,#169310,#169311,#169312,#169313,#169314,
#169315,#169316,#169317,#169318,#169319,#169320,#169321,#169322,#169323,
#169324,#169325,#169326,#169327,#169328,#169329,#169330,#169331,#169332,
#169333,#169334,#169335,#169336,#169337,#169338,#169339,#169340,#169341,
#169342,#169343,#169344,#169345,#169346,#169347,#169348,#169349,#169350,
#169351,#169352,#169353,#169354,#169355,#169356,#169357,#169358,#169359,
#169360,#169361,#169362,#169363,#169364,#169365,#169366,#169367,#169368,
#169369,#169370,#169371,#169372,#169373,#169374,#169375,#169376,#169377,
#169378,#169379,#169380,#169381,#169382,#169383,#169384,#169385,#169386,
#169387,#169388,#169389,#169390,#169391,#169392,#169393,#169394,#169395,
#169396,#169397,#169398,#169399,#169400,#169401,#169402,#169403,#169404,
#169405,#169406,#169407,#169408,#169409,#169410,#169411,#169412,#169413,
#169414,#169415,#169416,#169417,#169418,#169419,#169420,#169421,#169422,
#169423,#169424,#169425,#169426,#169427,#169428,#169429,#169430,#169431,
#169432,#169433,#169434),.UNSPECIFIED.,.F.,.F.,(4,2,2,2,2,2,2,2,2,2,2,2,
2,2,2,2,2,2,2,2,2,2,2,2,2,2,2,2,2,2,2,2,2,2,2,2,2,2,2,2,2,2,2,2,2,2,2,2,
2,2,2,2,2,2,2,2,2,2,2,2,2,2,2,2,2,2,2,2,2,2,2,2,2,2,2,2,2,2,2,2,2,2,2,2,
2,2,2,2,2,2,2,2,2,2,2,2,2,2,2,2,2,2,2,2,2,2,2,2,2,2,2,2,2,2,2,2,2,2,2,2,
2,2,2,2,2,2,2,2,2,2,2,2,2,2,2,2,2,2,4),(0.0751148559371182,0.0860173565209092,
0.0971067048898559,0.099366421733957,0.100620005721105,0.101691511545057,
0.103042742115049,0.105680884786454,0.122156785029108,0.172105730457344,
0.19018988390567,0.201175650792015,0.203636608709365,0.20592175810014,0.205936339486492,
0.205951514815512,0.205967323561641,0.205983808940996,0.206001018358443,
0.206019003919534,0.206037823133189,0.206057539636935,0.206078224011931,
0.206099954803837,0.206122819810584,0.206146917423792,0.206172358373818,
0.206199267857957,0.20622778807395,0.206258081290851,0.206290333750001,
0.206324760463609,0.20636161164916,0.206401180049667,0.206443809270907,
0.208321243029849,0.210755231903719,0.21543366746984,0.25055489342284,0.299497528275576,
0.309248234611211,0.311423000670789,0.312658039605414,0.313731789764809,
0.315109435347169,0.317967508302371,0.354058597180914,0.386748527096364,
0.409232518987205,0.414876188662865,0.41744565234437,0.419383843388974,
0.421211117362214,0.423755154818648,0.430409589924325,0.486119084923605,
0.510275166526602,0.521123209584095,0.523368751289448,0.524619354116576,
0.525691314061793,0.527046964930249,0.529191138841733,0.540205037851785,
0.591483586306157,0.620132182606221,0.626559385061205,0.629267098770382,
0.631228718645903,0.63302170791922,0.635888200213497,0.642781266181648,
0.695789031150177,0.72177847968669,0.733106392775542,0.735380227068554,
0.736636999189641,0.737708406864187,0.739055918696434,0.741676199297979,
0.757693834792938,0.763001774591121,0.774891703142893,0.777783592845092,
0.810579437265844,0.833225470791656,0.838891373722051,0.841465103814933,
0.843404133354895,0.845230450360933,0.847770352469685,0.854397290928634,
0.91039599306278,0.934368765256254,0.945167857462076,0.947410618365238,
0.948660704734029,0.949732858662897,0.951089571798029,0.953236957396969,
0.964299921129829,1.01544515888258,1.04417038111282,1.05060707288519,1.05331658161546,
1.05527870280231,1.05707160072483,1.05993675177385,1.06682040084819,1.11996764026672,
1.14586756475152,1.15717322464207,1.15944597457333,1.16070260234554,1.16177416341594,
1.16312222008114,1.16574459494106,1.18179282283111,1.185904715611,1.20159687313965,
1.23448609797719,1.25727490290768,1.26296037265423,1.2655378736431,1.2674776709501,
1.26930319149391,1.27183955315164,1.27844296751682,1.33468292779439,1.35363648187875,
1.36863946196255,1.37098961041877,1.3723921633433,1.37347181593448,1.37467844110652,
1.37672375260365,1.38476866900953,1.39990963280193,1.40880224667499),
 .UNSPECIFIED.);
#1789=B_SPLINE_CURVE_WITH_KNOTS('',3,(#169439,#169440,#169441,#169442,#169443,
#169444,#169445,#169446,#169447,#169448,#169449,#169450,#169451,#169452,
#169453,#169454,#169455,#169456,#169457,#169458,#169459,#169460,#169461,
#169462,#169463,#169464,#169465,#169466,#169467,#169468,#169469,#169470,
#169471,#169472,#169473,#169474,#169475,#169476,#169477,#169478,#169479,
#169480,#169481,#169482,#169483,#169484,#169485,#169486,#169487,#169488,
#169489,#169490,#169491,#169492,#169493,#169494,#169495,#169496,#169497,
#169498,#169499,#169500,#169501,#169502,#169503,#169504,#169505,#169506,
#169507,#169508,#169509,#169510,#169511,#169512,#169513,#169514,#169515,
#169516,#169517,#169518,#169519,#169520,#169521,#169522,#169523,#169524,
#169525,#169526,#169527,#169528,#169529,#169530,#169531,#169532,#169533,
#169534,#169535,#169536,#169537,#169538,#169539,#169540,#169541,#169542,
#169543,#169544,#169545,#169546,#169547,#169548,#169549,#169550,#169551,
#169552,#169553,#169554,#169555,#169556,#169557,#169558,#169559,#169560,
#169561,#169562,#169563,#169564,#169565,#169566,#169567,#169568,#169569,
#169570,#169571,#169572,#169573,#169574,#169575,#169576,#169577,#169578,
#169579,#169580,#169581,#169582,#169583,#169584,#169585,#169586,#169587,
#169588,#169589,#169590,#169591,#169592,#169593,#169594,#169595,#169596,
#169597,#169598,#169599,#169600,#169601,#169602,#169603,#169604,#169605,
#169606,#169607,#169608,#169609,#169610,#169611,#169612,#169613,#169614,
#169615,#169616,#169617,#169618,#169619,#169620,#169621,#169622,#169623,
#169624,#169625,#169626,#169627,#169628,#169629,#169630,#169631,#169632,
#169633,#169634,#169635,#169636,#169637,#169638,#169639,#169640,#169641,
#169642,#169643,#169644,#169645,#169646,#169647,#169648,#169649,#169650,
#169651,#169652,#169653,#169654,#169655,#169656,#169657,#169658,#169659,
#169660,#169661,#169662,#169663,#169664,#169665,#169666,#169667,#169668,
#169669,#169670,#169671,#169672),.UNSPECIFIED.,.F.,.F.,(4,2,2,2,2,2,2,2,
2,2,2,2,2,2,2,2,2,2,2,2,2,2,2,2,2,2,2,2,2,2,2,2,2,2,2,2,2,2,2,2,2,2,2,2,
2,2,2,2,2,2,2,2,2,2,2,2,2,2,2,2,2,2,2,2,2,2,2,2,2,2,2,2,2,2,2,2,2,2,2,2,
2,2,2,2,2,2,2,2,2,2,2,2,2,2,2,2,2,2,2,2,2,2,2,2,2,2,2,2,2,2,2,2,2,2,2,2,
4),(1.2596092693515,1.26784056841611,1.2907030567374,1.30119586166856,1.30341928440153,
1.30466495350844,1.3057372346681,1.30709916325351,1.30978754790108,1.32763512290863,
1.33373204541121,1.37574265376523,1.40292854542174,1.40705404731663,1.40954560736123,
1.41147833458491,1.4135728603315,1.41691845362249,1.42810815351804,1.44666701723586,
1.49069798611586,1.49656822344423,1.51244823745516,1.51506158391389,1.51640744634026,
1.5174786193471,1.51873640232671,1.52101503445713,1.53242869128707,1.55875522997995,
1.61123422843723,1.61816336233886,1.621035778792,1.62282984253785,1.62479053416427,
1.62749310976847,1.63388991324282,1.6817978741314,1.72137455636647,1.72610765750908,
1.72785087451443,1.72887686118778,1.72996902526844,1.73147803536465,1.73505268959622,
1.77422753331241,1.82298231529457,1.83011261701673,1.8330184057441,1.8348185296299,
1.83677412553914,1.8394484687519,1.84568047266152,1.87272244748268,1.9134469125147,
1.93614300379738,1.93899644014806,1.94037318987295,1.94144686727011,1.94268253522423,
1.94486010182034,1.9546517296156,2.00353502824768,2.03864077367805,2.04293545726612,
2.04547651510881,2.04741714815061,2.04949046049159,2.05273923559215,2.06305114794245,
2.07961726688403,2.11250761211196,2.12707470125624,2.13238357672141,2.1484237410175,
2.15104509852067,2.15239272196825,2.15346399410987,2.15472035750734,2.1569927688334,
2.16830014810116,2.19420894063555,2.24727819003548,2.25416222114205,2.25702700600421,
2.2588195257827,2.26078111927962,2.26348968281929,2.26992308807602,2.29863084376951,
2.34984288103329,2.36088073530258,2.36302629524007,2.36438230460374,2.36545420270438,
2.36670434047412,2.36894807597475,2.37976923032601,2.40382441604716,2.45963858842994,
2.46627634892691,2.468817626103,2.47064406087855,2.47252013026213,2.47500439199581,
2.47774260579395,2.48229452037214,2.49162589168426,2.54226133630486,2.57203625244806,
2.57495062302803,2.57633923563372,2.57741405840187,2.57864197125914,2.5807844665034,
2.59007764170921,2.59315594695257),.UNSPECIFIED.);
#1790=B_SPLINE_CURVE_WITH_KNOTS('',3,(#169674,#169675,#169676,#169677,#169678,
#169679,#169680,#169681,#169682,#169683,#169684,#169685,#169686,#169687,
#169688,#169689,#169690,#169691,#169692,#169693,#169694,#169695,#169696,
#169697,#169698,#169699,#169700,#169701,#169702,#169703,#169704,#169705,
#169706,#169707,#169708,#169709,#169710,#169711,#169712,#169713,#169714,
#169715,#169716,#169717,#169718,#169719,#169720,#169721,#169722,#169723,
#169724,#169725,#169726,#169727,#169728,#169729,#169730,#169731,#169732,
#169733,#169734,#169735,#169736,#169737,#169738,#169739,#169740,#169741,
#169742,#169743,#169744,#169745,#169746,#169747,#169748,#169749,#169750,
#169751,#169752,#169753,#169754,#169755,#169756,#169757,#169758,#169759,
#169760,#169761,#169762,#169763,#169764,#169765,#169766,#169767,#169768,
#169769,#169770,#169771,#169772,#169773,#169774,#169775,#169776,#169777,
#169778,#169779,#169780,#169781,#169782,#169783,#169784,#169785,#169786,
#169787,#169788,#169789,#169790,#169791,#169792,#169793,#169794,#169795,
#169796,#169797,#169798,#169799,#169800,#169801,#169802,#169803,#169804,
#169805,#169806,#169807,#169808,#169809,#169810,#169811,#169812,#169813,
#169814,#169815,#169816,#169817,#169818,#169819,#169820,#169821,#169822,
#169823,#169824,#169825,#169826,#169827,#169828,#169829,#169830,#169831,
#169832,#169833,#169834,#169835,#169836,#169837,#169838,#169839,#169840,
#169841,#169842,#169843,#169844,#169845,#169846,#169847,#169848,#169849,
#169850,#169851,#169852,#169853,#169854,#169855,#169856,#169857,#169858,
#169859,#169860,#169861,#169862,#169863,#169864,#169865,#169866,#169867,
#169868,#169869,#169870,#169871,#169872,#169873,#169874,#169875,#169876,
#169877,#169878,#169879,#169880,#169881,#169882,#169883,#169884,#169885,
#169886,#169887,#169888,#169889,#169890,#169891,#169892,#169893,#169894,
#169895,#169896,#169897,#169898,#169899),.UNSPECIFIED.,.F.,.F.,(4,2,2,2,
2,2,2,2,2,2,2,2,2,2,2,2,2,2,2,2,2,2,2,2,2,2,2,2,2,2,2,2,2,2,2,2,2,2,2,2,
2,2,2,2,2,2,2,2,2,2,2,2,2,2,2,2,2,2,2,2,2,2,2,2,2,2,2,2,2,2,2,2,2,2,2,2,
2,2,2,2,2,2,2,2,2,2,2,2,2,2,2,2,2,2,2,2,2,2,2,2,2,2,2,2,2,2,2,2,2,2,2,2,
4),(1.40880224667499,1.43961157073764,1.47086924577839,1.47509586135457,
1.47761755273777,1.4795555625412,1.48163797986083,1.48492615019491,1.49558026185905,
1.51290857721919,1.55319610960695,1.58019008650297,1.58309251547741,1.58447908464852,
1.58555400903655,1.58678392347576,1.5889343406719,1.59833078069535,1.64757023363411,
1.68278989810848,1.68708716824877,1.6896293560631,1.69157062179235,1.69364438702036,
1.69689340654677,1.70720218269439,1.72375957064368,1.75664804549484,1.77020265705881,
1.77751739841314,1.78186853654147,1.79304041252785,1.79519457097785,1.79655336872559,
1.79762571522802,1.79887436353224,1.8011103953453,1.8117989510688,1.835362518185,
1.89195134346187,1.89851313365991,1.90104272958297,1.90286637716281,1.90480695521465,
1.90739022680765,1.91310790195329,1.93614073437515,1.96921271377465,1.99068775996686,
2.0047808629009,2.0070899754305,2.00848038597147,2.00955828336901,2.01077144685872,
2.01284673118582,2.02125710714381,2.03743457119017,2.07973706793973,2.10709479977152,
2.11122544366403,2.11371882707531,2.1156522100081,2.11774669010319,2.12109057481832,
2.13225934821722,2.15076801969815,2.19595391381947,2.21639908458475,2.21919539700334,
2.22056098506142,2.22163380413166,2.22287742419837,2.22509073036959,2.23541950216045,
2.2576968117535,2.31632919780073,2.322643564461,2.32513223497133,2.32694511889544,
2.32889183966653,2.33151389671942,2.33744727820757,2.36212117128085,2.39106278201487,
2.42837343754691,2.43120665730518,2.43257948888165,2.43365287752092,2.43486646680045,
2.43697180760491,2.43957284873205,2.44499399831273,2.46045951398037,2.50169974687982,
2.53100449050529,2.53519459596823,2.53770535330162,2.53964132024482,2.54172781584236,
2.54503580178152,2.55587324477922,2.5736188983316,2.61954524127795,2.62787682755203,
2.64088199695592,2.64313751906312,2.64452688409231,2.64560190538519,2.64661071036363,
2.64782386588663,2.64961025778248,2.65534542984729,2.66801380144248),
 .UNSPECIFIED.);
#1791=B_SPLINE_CURVE_WITH_KNOTS('',3,(#169900,#169901,#169902,#169903,#169904,
#169905,#169906,#169907,#169908,#169909,#169910,#169911,#169912),
 .UNSPECIFIED.,.F.,.F.,(4,3,3,3,4),(-161.271232439372,-161.169466228941,
-161.067655520383,-160.965694042516,-160.920671713183),.UNSPECIFIED.);
#1792=B_SPLINE_CURVE_WITH_KNOTS('',3,(#169918,#169919,#169920,#169921,#169922,
#169923,#169924,#169925,#169926,#169927,#169928,#169929,#169930),
 .UNSPECIFIED.,.F.,.F.,(4,3,3,3,4),(170.955339710339,171.057208849126,171.158971104986,
171.260660144695,171.305836655045),.UNSPECIFIED.);
#1793=B_SPLINE_CURVE_WITH_KNOTS('',3,(#169931,#169932,#169933,#169934,#169935,
#169936,#169937,#169938,#169939,#169940,#169941,#169942,#169943,#169944,
#169945,#169946,#169947,#169948,#169949,#169950,#169951,#169952,#169953,
#169954,#169955,#169956,#169957,#169958,#169959,#169960,#169961,#169962,
#169963,#169964,#169965,#169966,#169967,#169968,#169969,#169970,#169971,
#169972,#169973,#169974,#169975,#169976,#169977,#169978,#169979,#169980,
#169981,#169982,#169983,#169984,#169985,#169986,#169987,#169988,#169989,
#169990,#169991,#169992,#169993,#169994,#169995,#169996,#169997,#169998,
#169999,#170000,#170001,#170002,#170003,#170004,#170005,#170006,#170007,
#170008,#170009,#170010,#170011,#170012,#170013,#170014,#170015,#170016,
#170017,#170018,#170019,#170020,#170021,#170022,#170023,#170024,#170025,
#170026,#170027,#170028,#170029,#170030,#170031,#170032,#170033,#170034,
#170035,#170036,#170037,#170038,#170039,#170040,#170041,#170042,#170043,
#170044,#170045,#170046,#170047,#170048,#170049,#170050,#170051,#170052,
#170053,#170054,#170055,#170056,#170057,#170058,#170059,#170060,#170061,
#170062,#170063,#170064,#170065,#170066,#170067,#170068,#170069,#170070,
#170071,#170072,#170073,#170074,#170075,#170076,#170077,#170078,#170079,
#170080,#170081,#170082,#170083,#170084,#170085,#170086,#170087,#170088,
#170089,#170090,#170091,#170092,#170093,#170094,#170095,#170096,#170097,
#170098,#170099,#170100,#170101,#170102,#170103,#170104,#170105,#170106,
#170107,#170108,#170109,#170110,#170111,#170112,#170113,#170114,#170115,
#170116,#170117,#170118,#170119,#170120,#170121,#170122,#170123,#170124,
#170125,#170126,#170127,#170128,#170129,#170130,#170131,#170132,#170133,
#170134,#170135,#170136,#170137,#170138,#170139,#170140,#170141,#170142,
#170143,#170144,#170145,#170146,#170147,#170148,#170149,#170150,#170151,
#170152),.UNSPECIFIED.,.F.,.F.,(4,2,2,2,2,2,2,2,2,2,2,2,2,2,2,2,2,2,2,2,
2,2,2,2,2,2,2,2,2,2,2,2,2,2,2,2,2,2,2,2,2,2,2,2,2,2,2,2,2,2,2,2,2,2,2,2,
2,2,2,2,2,2,2,2,2,2,2,2,2,2,2,2,2,2,2,2,2,2,2,2,2,2,2,2,2,2,2,2,2,2,2,2,
2,2,2,2,2,2,2,2,2,2,2,2,2,2,2,2,2,2,4),(0.000655565290617039,0.0215326227087458,
0.0285520710486535,0.0303960629521583,0.0316335607159248,0.0326484285716836,
0.0337175069904086,0.0350633930395249,0.0377854288917679,0.0559544034455085,
0.0616383873005818,0.0739383147691349,0.0845186242864435,0.106384758506318,
0.122977226240448,0.133286131125452,0.136520278985314,0.13858070980606,
0.140506707952375,0.143024766653336,0.147271569276199,0.192337973141826,
0.22091807838469,0.234451255841387,0.241869173568767,0.243841554482253,
0.244851270225045,0.245918308402917,0.247244927128634,0.249294265923087,
0.258883353206475,0.318505182680996,0.335297146712612,0.345718998927197,
0.348985053123623,0.351065350606082,0.353009727700483,0.35555172346558,
0.359839415602083,0.39423194403244,0.443433223563238,0.453286877168867,
0.455474595401037,0.456715604686166,0.457791868669989,0.459170491607426,
0.462028184696963,0.484797499509343,0.527329548590344,0.545904458535281,
0.557102064951541,0.560449566794869,0.562545228055637,0.564478970452924,
0.566971800761908,0.571099347367187,0.598278955703666,0.640350658381965,
0.656908939161571,0.665449707380976,0.667534981446109,0.668750097521971,
0.66982654936366,0.6712113028048,0.67350376882571,0.687289260686422,0.698622940530256,
0.737950194812959,0.764492408746576,0.770660422150587,0.773322051898098,
0.775273872650231,0.777074388192578,0.77998939464479,0.787184938532417,
0.833860946690508,0.856214114887312,0.870037786566998,0.875062862512361,
0.878645356469889,0.880154645396697,0.881246079267879,0.882271364737024,
0.884011344247576,0.888723737535384,0.929075838788759,0.977359064926128,
0.982966799285399,0.985530056472904,0.987467732993937,0.989297600835379,
0.991850217201394,0.998557418009532,1.05366046053509,1.07817665918164,1.08912117441691,
1.09137327484703,1.09262569274372,1.09369779389037,1.09505198329242,1.09779132353903,
1.11614970257119,1.1651496610562,1.18898299999316,1.19480672140833,1.19740892751408,
1.19935221826704,1.20117007595888,1.20367843671327,1.21011170514138,1.2596092693515),
 .UNSPECIFIED.);
#1794=B_SPLINE_CURVE_WITH_KNOTS('',3,(#170154,#170155,#170156,#170157,#170158,
#170159,#170160,#170161,#170162,#170163,#170164,#170165,#170166,#170167,
#170168,#170169,#170170,#170171,#170172,#170173,#170174,#170175,#170176,
#170177,#170178,#170179,#170180,#170181,#170182,#170183,#170184,#170185,
#170186,#170187,#170188,#170189,#170190,#170191,#170192,#170193,#170194,
#170195,#170196,#170197,#170198,#170199,#170200,#170201,#170202,#170203,
#170204,#170205,#170206,#170207,#170208,#170209,#170210,#170211,#170212,
#170213,#170214,#170215,#170216,#170217,#170218,#170219,#170220,#170221,
#170222,#170223,#170224,#170225,#170226,#170227,#170228,#170229,#170230,
#170231,#170232,#170233,#170234,#170235,#170236,#170237,#170238,#170239,
#170240,#170241,#170242,#170243,#170244,#170245,#170246,#170247,#170248,
#170249,#170250,#170251,#170252,#170253,#170254,#170255,#170256,#170257,
#170258,#170259,#170260,#170261,#170262,#170263,#170264,#170265,#170266,
#170267,#170268,#170269,#170270,#170271,#170272,#170273,#170274,#170275,
#170276,#170277,#170278,#170279,#170280,#170281,#170282,#170283,#170284,
#170285,#170286,#170287,#170288,#170289,#170290,#170291,#170292,#170293,
#170294,#170295,#170296,#170297,#170298,#170299,#170300,#170301,#170302,
#170303,#170304,#170305,#170306,#170307,#170308,#170309,#170310,#170311,
#170312,#170313,#170314,#170315,#170316,#170317,#170318,#170319,#170320,
#170321,#170322,#170323,#170324,#170325,#170326,#170327,#170328,#170329,
#170330,#170331,#170332,#170333,#170334),.UNSPECIFIED.,.F.,.F.,(4,3,3,3,
3,3,3,3,3,3,3,3,3,3,3,3,3,3,3,3,3,3,3,3,3,3,3,3,3,3,3,3,3,3,3,3,3,3,3,3,
3,3,3,3,3,3,3,3,3,3,3,3,3,3,3,3,3,3,3,3,4),(-167.203857019737,-167.089811042057,
-166.975344485129,-166.860315113754,-166.805687143633,-166.702287417193,
-166.599041109048,-166.495916087595,-166.3928564475,-166.289828158908,-166.186797235114,
-166.083659421327,-165.980465294178,-165.877088339511,-165.806850693671,
-165.703453681301,-165.600210066751,-165.4970876947,-165.39403067537,-165.291004974943,
-165.187976602729,-165.084841265902,-164.981649577785,-164.878274973299,
-164.808014243709,-164.704622128712,-164.601383510577,-164.498266258922,
-164.395214433679,-164.292193993531,-164.189170940353,-164.08604097664,
-163.98285470024,-163.879485509913,-163.809177793747,-163.705782196268,
-163.602540045536,-163.499419203548,-163.396363754289,-163.293339661723,
-163.190312932971,-163.087179283398,-162.983989309662,-162.880616444552,
-162.810341343786,-162.706946383838,-162.603704872123,-162.500584668206,
-162.397529856099,-162.294506398816,-162.191480302535,-162.088347276647,
-161.985157922646,-161.881785663941,-161.811504893824,-161.709471729551,
-161.607582179598,-161.505807286823,-161.404097848661,-161.302405178504,
-161.271232439372),.UNSPECIFIED.);
#1795=B_SPLINE_CURVE_WITH_KNOTS('',3,(#170335,#170336,#170337,#170338,#170339,
#170340,#170341,#170342,#170343,#170344,#170345,#170346,#170347),
 .UNSPECIFIED.,.F.,.F.,(4,3,3,3,4),(-167.55333773927,-167.448855810974,
-167.344457556961,-167.240110620773,-167.203857020092),.UNSPECIFIED.);
#1796=B_SPLINE_CURVE_WITH_KNOTS('',3,(#170353,#170354,#170355,#170356,#170357,
#170358,#170359,#170360,#170361,#170362),.UNSPECIFIED.,.F.,.F.,(4,3,3,4),
(7.5925217235916,7.70650210579109,7.82442143144844,7.9423407571058),
 .UNSPECIFIED.);
#1797=B_SPLINE_CURVE_WITH_KNOTS('',3,(#170364,#170365,#170366,#170367,#170368,
#170369,#170370,#170371,#170372,#170373,#170374,#170375,#170376,#170377,
#170378,#170379,#170380,#170381,#170382,#170383,#170384,#170385,#170386,
#170387,#170388,#170389,#170390,#170391,#170392,#170393,#170394,#170395,
#170396,#170397,#170398,#170399,#170400,#170401,#170402,#170403,#170404,
#170405,#170406,#170407,#170408,#170409,#170410,#170411,#170412,#170413,
#170414,#170415,#170416,#170417,#170418,#170419,#170420,#170421,#170422,
#170423,#170424,#170425,#170426,#170427,#170428,#170429,#170430,#170431,
#170432,#170433,#170434,#170435,#170436,#170437,#170438,#170439,#170440,
#170441,#170442,#170443,#170444,#170445,#170446,#170447,#170448,#170449,
#170450,#170451,#170452,#170453,#170454,#170455,#170456,#170457,#170458,
#170459,#170460,#170461,#170462,#170463,#170464,#170465,#170466,#170467,
#170468,#170469,#170470,#170471,#170472,#170473,#170474,#170475,#170476,
#170477,#170478,#170479,#170480,#170481,#170482,#170483,#170484,#170485,
#170486,#170487,#170488,#170489,#170490,#170491,#170492,#170493,#170494,
#170495,#170496,#170497,#170498,#170499,#170500,#170501,#170502,#170503,
#170504,#170505,#170506,#170507,#170508,#170509,#170510,#170511,#170512,
#170513,#170514,#170515,#170516,#170517,#170518,#170519,#170520,#170521,
#170522,#170523,#170524,#170525,#170526,#170527,#170528,#170529,#170530,
#170531,#170532),.UNSPECIFIED.,.F.,.F.,(4,3,3,3,3,3,3,3,3,3,3,3,3,3,3,3,
3,3,3,3,3,3,3,3,3,3,3,3,3,3,3,3,3,3,3,3,3,3,3,3,3,3,3,3,3,3,3,3,3,3,3,3,
3,3,3,3,4),(2.00878451784277,2.1121038592252,2.21526978906708,2.31831430239281,
2.42129361283972,2.52424186610789,2.6271931648727,2.73024926544087,2.83336236205174,
2.93665172410156,2.99650934988563,3.10008230044164,3.20350555624697,3.30681221854451,
3.41005628885956,3.51327152250976,3.61649163431342,3.71982077793706,3.82320772460313,
3.92677776279761,3.99534579984751,4.09860814851247,4.20171513491831,4.30469859633612,
4.40761536822807,4.51049968437652,4.61338573414333,4.71637827780363,4.8194266839831,
4.92265880761429,4.99418224980938,5.09760357317466,5.20087154158791,5.30401821033476,
5.40709947808643,5.51014934245974,5.61320175788195,5.7163607823649,5.81957599567373,
5.92297359909413,5.99301869977126,6.09643423501025,6.19969678171233,6.30283860648641,
6.40591538895672,6.50896113435575,6.61200980509545,6.71516569207011,6.81837810297347,
6.92177347981602,6.99185514973314,7.09670699182257,7.20139082240131,7.30591390630536,
7.41034216218022,7.51471170479246,7.59252172323623),.UNSPECIFIED.);
#1798=B_SPLINE_CURVE_WITH_KNOTS('',3,(#170536,#170537,#170538,#170539,#170540,
#170541,#170542,#170543,#170544,#170545,#170546,#170547,#170548,#170549,
#170550,#170551,#170552,#170553,#170554,#170555,#170556,#170557,#170558,
#170559,#170560,#170561,#170562,#170563,#170564,#170565,#170566,#170567,
#170568,#170569,#170570,#170571,#170572,#170573,#170574,#170575,#170576,
#170577,#170578,#170579,#170580,#170581,#170582,#170583,#170584,#170585,
#170586,#170587,#170588,#170589,#170590,#170591,#170592,#170593,#170594,
#170595,#170596,#170597,#170598,#170599,#170600,#170601,#170602,#170603,
#170604,#170605,#170606,#170607,#170608,#170609,#170610,#170611,#170612,
#170613,#170614,#170615,#170616,#170617,#170618,#170619,#170620,#170621,
#170622,#170623,#170624,#170625,#170626,#170627,#170628,#170629,#170630,
#170631,#170632,#170633,#170634,#170635,#170636,#170637,#170638,#170639,
#170640,#170641,#170642,#170643,#170644,#170645,#170646,#170647,#170648,
#170649,#170650,#170651,#170652,#170653),.UNSPECIFIED.,.F.,.F.,(4,3,3,3,
3,3,3,3,3,3,3,3,3,3,3,3,3,3,3,3,3,3,3,3,3,3,3,3,3,3,3,3,3,3,3,3,3,3,3,4),
(-3.84103903298819,-3.73547282260037,-3.63371534129195,-3.532025649837,
-3.43036801686642,-3.32870675955683,-3.22694496839026,-3.12512265260723,
-3.0231391456354,-2.99650934988562,-2.89298804639364,-2.7896177431212,-2.6863657748023,
-2.58317744783227,-2.48001894053971,-2.37685647276339,-2.2735860348565,
-2.17025847843688,-2.06674831927575,-1.99767289992375,-1.89536969270601,
-1.79322053934975,-1.69118879043613,-1.58921974834484,-1.48727804733066,
-1.38532836211997,-1.28325632553546,-1.18112129116516,-1.0787805560955,
-0.998836449961877,-0.892562651586185,-0.780992320137912,-0.67507184468024,
-0.56925096547428,-0.463501942676278,-0.357797126152519,-0.25207917949123,
-0.14635615172218,-0.0405601678050039,0.),.UNSPECIFIED.);
#1799=B_SPLINE_CURVE_WITH_KNOTS('',3,(#170654,#170655,#170656,#170657,#170658,
#170659,#170660,#170661,#170662,#170663,#170664,#170665,#170666,#170667,
#170668,#170669,#170670,#170671,#170672,#170673,#170674,#170675,#170676,
#170677,#170678,#170679),.UNSPECIFIED.,.F.,.F.,(4,2,2,2,2,2,2,2,2,2,2,2,
4),(0.000655568373726633,0.0215326025103882,0.0285520600990642,0.030396058279881,
0.0316335578306403,0.032648424817314,0.0337175011697388,0.0350633794126454,
0.0377853822300375,0.0559534379118389,0.0616384583380826,0.0739384474895044,
0.0747573410445804),.UNSPECIFIED.);
#1800=B_SPLINE_CURVE_WITH_KNOTS('',3,(#170685,#170686,#170687,#170688,#170689,
#170690,#170691,#170692,#170693,#170694,#170695,#170696,#170697,#170698,
#170699,#170700,#170701,#170702,#170703,#170704,#170705,#170706,#170707,
#170708),.UNSPECIFIED.,.F.,.F.,(4,2,2,2,2,2,2,2,2,2,2,4),(2.59396097058535,
2.61966488148547,2.62799719025607,2.64100348253462,2.64325919998503,2.64464868542601,
2.64572379995559,2.64673269247101,2.64794595330706,2.64973250033605,2.6554681689063,
2.66813763591281),.UNSPECIFIED.);
#1801=B_SPLINE_CURVE_WITH_KNOTS('',3,(#170709,#170710,#170711,#170712,#170713,
#170714,#170715,#170716,#170717,#170718,#170719,#170720,#170721,#170722,
#170723,#170724,#170725,#170726,#170727,#170728,#170729,#170730,#170731,
#170732,#170733,#170734,#170735,#170736,#170737,#170738,#170739,#170740,
#170741,#170742,#170743,#170744,#170745,#170746,#170747,#170748,#170749,
#170750,#170751,#170752,#170753,#170754,#170755,#170756,#170757,#170758,
#170759,#170760,#170761,#170762,#170763,#170764,#170765,#170766,#170767,
#170768,#170769,#170770,#170771,#170772,#170773,#170774,#170775,#170776,
#170777,#170778,#170779,#170780,#170781,#170782,#170783,#170784,#170785,
#170786,#170787,#170788,#170789,#170790,#170791,#170792,#170793,#170794,
#170795,#170796,#170797,#170798,#170799,#170800,#170801,#170802,#170803,
#170804,#170805,#170806,#170807,#170808,#170809,#170810,#170811,#170812,
#170813,#170814,#170815,#170816,#170817,#170818,#170819,#170820,#170821,
#170822,#170823,#170824,#170825,#170826,#170827,#170828,#170829,#170830,
#170831,#170832,#170833,#170834,#170835,#170836,#170837,#170838,#170839,
#170840,#170841,#170842,#170843,#170844,#170845,#170846,#170847,#170848,
#170849,#170850,#170851,#170852,#170853,#170854,#170855,#170856,#170857,
#170858,#170859,#170860,#170861,#170862,#170863,#170864,#170865,#170866,
#170867,#170868,#170869,#170870,#170871,#170872,#170873,#170874,#170875,
#170876,#170877,#170878,#170879,#170880,#170881,#170882,#170883,#170884,
#170885,#170886,#170887,#170888,#170889),.UNSPECIFIED.,.F.,.F.,(4,3,3,3,
3,3,3,3,3,3,3,3,3,3,3,3,3,3,3,3,3,3,3,3,3,3,3,3,3,3,3,3,3,3,3,3,3,3,3,3,
3,3,3,3,3,3,3,3,3,3,3,3,3,3,3,3,3,3,3,3,4),(7.9423407571058,7.99069159969502,
8.0940913166079,8.19733761512875,8.30046262686177,8.40352225718067,8.50655053595679,
8.60958144990777,8.71271925388011,8.81591337121366,8.9192903161747,8.98952804965688,
9.09292506023253,9.19616867293108,9.29929104305031,9.40234806040229,9.50537375880478,
9.608402128953,9.71153746366316,9.81472914963136,9.91810375194011,9.98836449961875,
10.0917566187677,10.1949952411212,10.2981124970725,10.4011643266588,10.504184771191,
10.6072078287861,10.7103377969385,10.8135240777969,10.916893272565,10.9872009495806,
11.0905965451736,11.1938386939995,11.2969595340606,11.400014981379,11.5030390719965,
11.6060657987925,11.7091994464135,11.8123894181962,11.9157622813734,11.9860373995425,
12.0894323592964,12.1926738708075,12.2957940745085,12.3988488863923,12.5018723434439,
12.6048984394876,12.7080314651285,12.8112208188763,12.9145930773222,12.9848738495044,
13.0869196152918,13.1887917830724,13.2905669750553,13.3922809421219,13.493969350127,
13.5957283282564,13.697522003712,13.7994743430358,13.8757070301447),
 .UNSPECIFIED.);
#1802=B_SPLINE_CURVE_WITH_KNOTS('',3,(#170890,#170891,#170892,#170893,#170894,
#170895,#170896,#170897,#170898,#170899,#170900,#170901,#170902,#170903,
#170904,#170905,#170906,#170907,#170908,#170909,#170910,#170911,#170912,
#170913,#170914,#170915,#170916,#170917,#170918,#170919,#170920,#170921,
#170922,#170923,#170924,#170925,#170926,#170927,#170928,#170929,#170930,
#170931,#170932,#170933,#170934,#170935,#170936,#170937,#170938,#170939,
#170940,#170941,#170942,#170943,#170944,#170945,#170946,#170947,#170948,
#170949,#170950,#170951,#170952,#170953,#170954,#170955,#170956,#170957,
#170958,#170959,#170960,#170961,#170962,#170963,#170964,#170965,#170966,
#170967,#170968,#170969,#170970,#170971,#170972,#170973,#170974,#170975,
#170976,#170977,#170978,#170979,#170980,#170981,#170982,#170983,#170984,
#170985,#170986,#170987,#170988,#170989,#170990,#170991,#170992,#170993,
#170994,#170995,#170996,#170997,#170998,#170999,#171000,#171001,#171002,
#171003,#171004,#171005,#171006,#171007,#171008,#171009,#171010,#171011,
#171012,#171013,#171014,#171015,#171016,#171017,#171018,#171019,#171020,
#171021,#171022,#171023,#171024,#171025,#171026,#171027,#171028,#171029,
#171030,#171031,#171032,#171033,#171034,#171035,#171036,#171037,#171038,
#171039,#171040,#171041,#171042,#171043,#171044,#171045,#171046,#171047,
#171048,#171049,#171050,#171051,#171052,#171053,#171054,#171055,#171056,
#171057,#171058,#171059,#171060,#171061,#171062,#171063,#171064,#171065,
#171066,#171067,#171068,#171069,#171070,#171071,#171072,#171073,#171074,
#171075,#171076,#171077,#171078,#171079,#171080,#171081,#171082,#171083,
#171084,#171085,#171086,#171087,#171088,#171089,#171090,#171091,#171092,
#171093,#171094,#171095,#171096,#171097,#171098,#171099,#171100,#171101,
#171102,#171103,#171104,#171105,#171106,#171107,#171108,#171109,#171110,
#171111,#171112,#171113,#171114,#171115),.UNSPECIFIED.,.F.,.F.,(4,2,2,2,
2,2,2,2,2,2,2,2,2,2,2,2,2,2,2,2,2,2,2,2,2,2,2,2,2,2,2,2,2,2,2,2,2,2,2,2,
2,2,2,2,2,2,2,2,2,2,2,2,2,2,2,2,2,2,2,2,2,2,2,2,2,2,2,2,2,2,2,2,2,2,2,2,
2,2,2,2,2,2,2,2,2,2,2,2,2,2,2,2,2,2,2,2,2,2,2,2,2,2,2,2,2,2,2,2,2,2,2,2,
4),(0.0747573410445804,0.0845186705731368,0.106384833159163,0.122977268432354,
0.133286155948304,0.136520299082465,0.138580727010485,0.140506722518262,
0.143024777841391,0.147271574858557,0.192338078811951,0.220918211426313,
0.23445132756505,0.241869219920678,0.243841596800967,0.244851311040615,
0.245918348998624,0.247244968472377,0.249294309205372,0.258883419242254,
0.318505107182258,0.33529716797821,0.345719066135449,0.348985127201808,
0.351065427293654,0.353009805601841,0.355551801208321,0.359839489253536,
0.394231670214988,0.443432623867018,0.453286793494708,0.455474548716315,
0.456715567136985,0.457791830935739,0.459170443254487,0.462028080891041,
0.484795161151365,0.527329653025948,0.545904467624627,0.557102032473282,
0.560449529785833,0.562545189975799,0.564478932583876,0.566971764837944,
0.571099318266019,0.598279189460489,0.640351486123511,0.656909177905306,
0.665449744169385,0.667535001735122,0.668750113887454,0.669826566067397,
0.671211324852166,0.673503809869498,0.68728970579793,0.698623488257327,
0.737950319022652,0.76449243597379,0.77066043653915,0.773322063534953,0.775273883311026,
0.77707439868121,0.779989406474173,0.787184961628708,0.833860412060123,
0.856214203934402,0.870037822399162,0.875062884842747,0.878645371106983,
0.880154658430758,0.881246091825336,0.882271377615306,0.884011358682575,
0.88872376206493,0.929076069033313,0.977359083840166,0.982966816849575,
0.985530073990243,0.987467750712657,0.989297618920964,0.99185023608595,
0.998557440794016,1.05366042084994,1.07817664749199,1.08912117038505,1.09137327161863,
1.09262568986451,1.09369779112269,1.09505198049589,1.09779132050781,1.11614969127593,
1.16514965369926,1.18898299191255,1.19480671307616,1.19740891905937,1.19935220971603,
1.20117006731361,1.20367842793102,1.21011169596083,1.26784057161457,1.29070305801019,
1.30119586228216,1.30341928481243,1.30466495379317,1.30573723483708,1.30709916325547,
1.30978754749906,1.32763511612353,1.3337320454579,1.37574265902158,1.40292854662424,
1.4070540481674,1.40817976059961),.UNSPECIFIED.);
#1803=B_SPLINE_CURVE_WITH_KNOTS('',3,(#171120,#171121,#171122,#171123,#171124,
#171125,#171126,#171127,#171128,#171129,#171130,#171131,#171132,#171133,
#171134,#171135,#171136,#171137,#171138,#171139,#171140,#171141,#171142,
#171143,#171144,#171145,#171146,#171147,#171148,#171149,#171150,#171151,
#171152,#171153,#171154,#171155,#171156,#171157,#171158,#171159,#171160,
#171161,#171162,#171163,#171164,#171165,#171166,#171167,#171168,#171169,
#171170,#171171,#171172,#171173,#171174,#171175,#171176,#171177,#171178,
#171179,#171180,#171181,#171182,#171183,#171184,#171185,#171186,#171187,
#171188,#171189,#171190,#171191,#171192,#171193,#171194,#171195,#171196,
#171197,#171198,#171199,#171200,#171201,#171202,#171203,#171204,#171205,
#171206,#171207,#171208,#171209,#171210,#171211,#171212,#171213,#171214,
#171215,#171216,#171217,#171218,#171219,#171220,#171221,#171222,#171223,
#171224,#171225,#171226,#171227,#171228,#171229,#171230,#171231,#171232,
#171233,#171234,#171235,#171236,#171237,#171238,#171239,#171240,#171241,
#171242,#171243,#171244,#171245,#171246,#171247,#171248,#171249,#171250,
#171251,#171252,#171253,#171254,#171255,#171256,#171257,#171258,#171259,
#171260,#171261,#171262,#171263,#171264,#171265,#171266,#171267,#171268,
#171269,#171270,#171271,#171272,#171273,#171274,#171275,#171276,#171277,
#171278,#171279,#171280,#171281,#171282,#171283,#171284,#171285,#171286,
#171287,#171288,#171289,#171290,#171291,#171292,#171293,#171294,#171295,
#171296,#171297,#171298,#171299,#171300,#171301,#171302,#171303,#171304,
#171305,#171306,#171307,#171308,#171309,#171310,#171311,#171312,#171313,
#171314,#171315,#171316,#171317,#171318,#171319,#171320,#171321,#171322,
#171323,#171324,#171325,#171326,#171327,#171328,#171329,#171330,#171331,
#171332,#171333,#171334,#171335,#171336,#171337,#171338,#171339,#171340,
#171341,#171342,#171343,#171344,#171345,#171346,#171347,#171348,#171349,
#171350,#171351,#171352,#171353,#171354,#171355),.UNSPECIFIED.,.F.,.F.,
(4,2,2,2,2,2,2,2,2,2,2,2,2,2,2,2,2,2,2,2,2,2,2,2,2,2,2,2,2,2,2,2,2,2,2,
2,2,2,2,2,2,2,2,2,2,2,2,2,2,2,2,2,2,2,2,2,2,2,2,2,2,2,2,2,2,2,2,2,2,2,2,
2,2,2,2,2,2,2,2,2,2,2,2,2,2,2,2,2,2,2,2,2,2,2,2,2,2,2,2,2,2,2,2,2,2,2,2,
2,2,2,2,2,2,2,2,2,2,4),(1.26014274045541,1.26297209927859,1.26554984345313,
1.26748982372479,1.26931551641608,1.27185211719372,1.27845615377098,1.33470141050411,
1.35365674900082,1.36866114306478,1.37101151311199,1.37241419829855,1.37349395271473,
1.37470069170799,1.37674619619045,1.38479187235191,1.39993426723045,1.43963996922864,
1.47090055718122,1.47512757055363,1.47764949952585,1.47958769207543,1.48167030590745,
1.48495878685757,1.49561390783155,1.51294386781522,1.55323518103887,1.58023169425134,
1.58313439680814,1.58452109672224,1.58559612249024,1.58682615295961,1.58897677310651,
1.59837410128736,1.64761819587377,1.6828411695857,1.6871388447366,1.68968127223282,
1.6916227210389,1.69369668189028,1.69694600801346,1.70725575793492,1.72381471101445,
1.75670628863334,1.77026267743675,1.7775768382212,1.78191404428974,1.79310050992532,
1.79525569839796,1.7966148761427,1.79768734324328,1.79893592628009,1.8011713306124,
1.81184728693573,1.83536345053879,1.89203457860106,1.89858858463189,1.90111706860915,
1.90294053294031,1.90488148850446,1.90746624357967,1.91319125427484,1.93627703918399,
1.97002382608581,1.99225669543721,2.00498804876792,2.0072297005631,2.00861499200257,
2.00968972307797,2.0109203095309,2.01307400992551,2.02251793649443,2.07171202003201,
2.1069170963119,2.11121391611252,2.11375588398395,2.11569700849964,2.11777064877978,
2.12101952657924,2.13132830733565,2.14788613005514,2.18077366189977,2.21641126348564,
2.21927453521325,2.22065336931389,2.22172742429494,2.22296212080951,2.22513461690257,
2.23484807285045,2.28380809990575,2.31894137921001,2.32323714025563,2.32577875681878,
2.32771977142962,2.32979344784715,2.33304270287299,2.34335538374999,2.35992205251161,
2.39137460394602,2.42846956081233,2.43130759466556,2.43268144536678,2.43375500902394,
2.43496810604408,2.43707097282812,2.43966818532776,2.44507801256525,2.46049453097618,
2.50154000946738,2.53111678952409,2.53530707945431,2.53781800221899,2.53975412894107,
2.54184082857001,2.54514920602675,2.55598854329349,2.57373791311194,2.59396097058535),
 .UNSPECIFIED.);
#1804=B_SPLINE_CURVE_WITH_KNOTS('',3,(#171357,#171358,#171359,#171360,#171361,
#171362,#171363,#171364,#171365,#171366,#171367,#171368,#171369,#171370,
#171371,#171372,#171373,#171374,#171375,#171376,#171377,#171378,#171379,
#171380,#171381,#171382,#171383,#171384,#171385,#171386,#171387,#171388,
#171389,#171390,#171391,#171392,#171393,#171394,#171395,#171396,#171397,
#171398,#171399,#171400,#171401,#171402,#171403,#171404,#171405,#171406,
#171407,#171408,#171409,#171410,#171411,#171412,#171413,#171414,#171415,
#171416,#171417,#171418,#171419,#171420,#171421,#171422,#171423,#171424,
#171425,#171426,#171427,#171428,#171429,#171430,#171431,#171432,#171433,
#171434,#171435,#171436,#171437,#171438,#171439,#171440,#171441,#171442,
#171443,#171444,#171445,#171446,#171447,#171448,#171449,#171450,#171451,
#171452,#171453,#171454,#171455,#171456,#171457,#171458,#171459,#171460,
#171461,#171462,#171463,#171464,#171465,#171466,#171467,#171468,#171469,
#171470,#171471,#171472,#171473,#171474,#171475,#171476,#171477,#171478,
#171479,#171480,#171481,#171482,#171483,#171484,#171485,#171486,#171487,
#171488,#171489,#171490,#171491,#171492,#171493,#171494,#171495,#171496,
#171497,#171498,#171499,#171500,#171501,#171502,#171503,#171504,#171505,
#171506,#171507,#171508,#171509,#171510,#171511,#171512,#171513,#171514,
#171515,#171516,#171517,#171518,#171519,#171520,#171521,#171522,#171523,
#171524,#171525,#171526,#171527,#171528,#171529,#171530,#171531,#171532,
#171533,#171534,#171535,#171536,#171537,#171538,#171539,#171540,#171541,
#171542,#171543,#171544,#171545,#171546,#171547,#171548,#171549,#171550,
#171551,#171552,#171553,#171554,#171555,#171556,#171557,#171558,#171559,
#171560,#171561,#171562,#171563,#171564,#171565,#171566),.UNSPECIFIED.,
 .F.,.F.,(4,2,2,2,2,2,2,2,2,2,2,2,2,2,2,2,2,2,2,2,2,2,2,2,2,2,2,2,2,2,2,
2,2,2,2,2,2,2,2,2,2,2,2,2,2,2,2,2,2,2,2,2,2,2,2,2,2,2,2,2,2,2,2,2,2,2,2,
2,2,2,2,2,2,2,2,2,2,2,2,2,2,2,2,2,2,2,2,2,2,2,2,2,2,2,2,2,2,2,2,2,2,2,2,
2,4),(1.40817976059961,1.40954560798892,1.41147833503154,1.41357286057273,
1.41691845351314,1.42810815196938,1.44666701284211,1.49069806272605,1.49656815679459,
1.51244823560637,1.51506158353223,1.5164074462051,1.51747861916724,1.5187364018262,
1.52101503256817,1.53242866566733,1.55875511038331,1.61123424300218,1.61816336737727,
1.62103578224914,1.62282984569815,1.62479053755441,1.62749311448799,1.63388992588092,
1.68180166895086,1.72137451008661,1.72610764741294,1.7278508699183,1.72887685767718,
1.72996902105914,1.73147802721958,1.73505265857317,1.77422260144584,1.82298260616433,
1.83011270279042,1.83301845707072,1.83481857454488,1.83677417528322,1.83944854634883,
1.84568071219699,1.87272400329981,1.91345111090567,1.93614316951335,1.93899650693946,
1.9403732371886,1.94144691268922,1.94268259347209,1.94486021861204,1.95465270611566,
2.00353527789093,2.03864078780423,2.04293546813942,2.04547652497697,2.0474171577801,
2.04949047037842,2.05273924695119,2.06305117296332,2.07961732234454,2.1125076926792,
2.12707698170315,2.13238313539665,2.14842370753174,2.15104509069604,2.15239271963392,
2.15346399209599,2.15472035118399,2.15699274279259,2.16829978004372,2.19420723197035,
2.24727840870293,2.25416229203494,2.25702705254161,2.25881956785921,2.26078116514355,
2.2634897498175,2.26992328067746,2.29863209204647,2.34984120859534,2.36088056279273,
2.36302621553676,2.36438225315829,2.36545415330734,2.36670427012878,2.36894790980019,
2.37976748576411,2.4038168235839,2.4596399162556,2.46627675903133,2.46881789208597,
2.47064428867979,2.47252037775033,2.47500476100931,2.47774314421726,2.48229547136513,
2.49162801998579,2.54226197104376,2.57203627007789,2.57495064032719,2.57633925275901,
2.57741407538504,2.57864198807004,2.58078448298667,2.59007765633515,2.60891632639188,
2.66742169222757),.UNSPECIFIED.);
#1805=B_SPLINE_CURVE_WITH_KNOTS('',3,(#171567,#171568,#171569,#171570),
 .UNSPECIFIED.,.F.,.F.,(4,4),(-16.7565928429673,-16.4074096477818),
 .UNSPECIFIED.);
#1806=B_SPLINE_CURVE_WITH_KNOTS('',3,(#171576,#171577,#171578,#171579,#171580,
#171581,#171582,#171583,#171584,#171585,#171586,#171587,#171588,#171589,
#171590,#171591),.UNSPECIFIED.,.F.,.F.,(4,2,2,2,2,2,2,4),(2.593432104111,
2.64858655332197,2.65674930219105,2.65982049707518,2.66165177161212,2.66349570067702,
2.66578750456173,2.66785180667336),.UNSPECIFIED.);
#1807=B_SPLINE_CURVE_WITH_KNOTS('',3,(#171592,#171593,#171594,#171595,#171596,
#171597,#171598,#171599,#171600,#171601,#171602,#171603,#171604,#171605,
#171606,#171607,#171608,#171609,#171610,#171611,#171612,#171613,#171614,
#171615,#171616,#171617,#171618,#171619,#171620,#171621,#171622,#171623,
#171624,#171625,#171626,#171627,#171628,#171629,#171630,#171631,#171632,
#171633,#171634,#171635,#171636,#171637,#171638,#171639,#171640,#171641,
#171642,#171643,#171644,#171645,#171646,#171647,#171648,#171649,#171650,
#171651,#171652,#171653,#171654,#171655,#171656,#171657,#171658,#171659,
#171660,#171661,#171662,#171663,#171664,#171665,#171666,#171667,#171668,
#171669,#171670,#171671,#171672,#171673,#171674,#171675,#171676,#171677,
#171678,#171679,#171680,#171681,#171682,#171683,#171684,#171685,#171686,
#171687,#171688,#171689,#171690,#171691,#171692,#171693,#171694,#171695,
#171696,#171697,#171698,#171699,#171700,#171701,#171702,#171703,#171704,
#171705,#171706,#171707,#171708,#171709,#171710,#171711,#171712,#171713,
#171714,#171715,#171716,#171717,#171718,#171719,#171720,#171721,#171722,
#171723,#171724,#171725,#171726,#171727,#171728,#171729,#171730,#171731,
#171732,#171733,#171734,#171735,#171736,#171737,#171738,#171739,#171740,
#171741,#171742,#171743,#171744,#171745,#171746,#171747,#171748,#171749,
#171750,#171751,#171752,#171753,#171754,#171755,#171756,#171757,#171758,
#171759,#171760,#171761,#171762,#171763,#171764,#171765,#171766,#171767,
#171768,#171769,#171770,#171771,#171772,#171773,#171774,#171775,#171776,
#171777,#171778,#171779,#171780,#171781,#171782,#171783,#171784,#171785,
#171786,#171787,#171788,#171789,#171790,#171791,#171792,#171793,#171794,
#171795,#171796,#171797,#171798,#171799,#171800,#171801,#171802,#171803,
#171804,#171805,#171806,#171807,#171808,#171809,#171810,#171811,#171812,
#171813,#171814,#171815,#171816,#171817,#171818,#171819,#171820,#171821,
#171822,#171823,#171824,#171825,#171826,#171827,#171828,#171829,#171830,
#171831,#171832,#171833,#171834,#171835,#171836,#171837,#171838,#171839,
#171840,#171841,#171842,#171843,#171844,#171845),.UNSPECIFIED.,.F.,.F.,
(4,2,2,2,2,2,2,2,2,2,2,2,2,2,2,2,2,2,2,2,2,2,2,2,2,2,2,2,2,2,2,2,2,2,2,
2,2,2,2,2,2,2,2,2,2,2,2,2,2,2,2,2,2,2,2,2,2,2,2,2,2,2,2,2,2,2,2,2,2,2,2,
2,2,2,2,2,2,2,2,2,2,2,2,2,2,2,2,2,2,2,2,2,2,2,2,2,2,2,2,2,2,2,2,2,2,2,2,
2,2,2,2,2,2,2,2,2,2,2,2,2,2,2,2,2,2,2,4),(0.000823823589073982,0.00401009754324733,
0.0104659483184938,0.0609229667697557,0.0860113303179115,0.0971060554871067,
0.0993660887595639,0.100619741586636,0.101691241033782,0.10304238027135,
0.105680097639832,0.122145136882367,0.172110404056795,0.190191463422201,
0.201175885338313,0.203636754898609,0.205921840859828,0.205936427926701,
0.205951609293238,0.205967424553085,0.205983916850553,0.206001133630138,
0.206019127167111,0.206037954961812,0.206057680693129,0.206078375018293,
0.206100116615346,0.206122993333903,0.206147103683314,0.206172558526066,
0.206199483218856,0.206228020157709,0.206258331859729,0.206290604770655,
0.206325054226357,0.206361930827868,0.206401527780941,0.2064441892766,0.208321645320361,
0.210755871651084,0.215435397659435,0.250651908671031,0.299904881970501,
0.309294805197645,0.311444316535687,0.312673795009294,0.313748396883222,
0.315134616790653,0.31803656645619,0.350185389684556,0.382953121290837,
0.401774809307777,0.409258081551224,0.414880033872189,0.417445509367957,
0.419383103178602,0.421211590465703,0.423760175375085,0.430443801089756,
0.485860352738926,0.510210499873265,0.521110638551203,0.523359333814898,
0.524610629906711,0.52568253000632,0.527037267122833,0.529779493374406,
0.548228425699099,0.555160156134684,0.565632680004139,0.598466987138945,
0.614996067048697,0.62529265649893,0.628539969214722,0.63061316478851,0.63255426309132,
0.635096760958085,0.639395774357405,0.67478009936686,0.723968707593928,
0.733286290179115,0.735430903098509,0.73665945386373,0.737734465576581,
0.739122824163678,0.742034920542572,0.773631431240273,0.777736026984134,
0.810539671413484,0.833195206346511,0.83886263834764,0.841436793687725,
0.843376034235288,0.845202469710275,0.847742407903289,0.854368680439053,
0.910385235380532,0.934352020626436,0.945149898831714,0.947392735437358,
0.94864291006491,0.949715168119158,0.951072049505975,0.953219769852569,
0.96428591771816,1.0154324883676,1.04416133862173,1.05059874678806,1.05330852949945,
1.05527083909119,1.05706390229297,1.05992930251803,1.06681347281615,1.11996736034945,
1.14586858267119,1.15717501638262,1.15944796383811,1.16070470647357,1.16177636892278,
1.16312455750329,1.16574720186828,1.18179728296908,1.18590882563297,1.20160280711238,
1.23449513449812,1.25728609280512,1.26014274045541),.UNSPECIFIED.);
#1808=B_SPLINE_CURVE_WITH_KNOTS('',3,(#171847,#171848,#171849,#171850,#171851,
#171852,#171853,#171854,#171855,#171856),.UNSPECIFIED.,.F.,.F.,(4,1,1,1,
1,1,1,4),(-22.6905949549614,-21.9744018991612,-20.9755654491994,-19.9767289992375,
-18.9778925492756,-17.9790560993137,-16.9802196493519,-16.7565928429673),
 .UNSPECIFIED.);
#1809=B_SPLINE_CURVE_WITH_KNOTS('',3,(#171857,#171858,#171859,#171860,#171861,
#171862,#171863,#171864,#171865,#171866,#171867,#171868,#171869,#171870,
#171871,#171872,#171873,#171874),.UNSPECIFIED.,.F.,.F.,(4,2,2,2,2,2,2,2,
4),(0.000629331914479173,0.0468846876811639,0.0566532975426214,0.0588292040485486,
0.060064451053258,0.0611381007239059,0.062515249563224,0.0653710260823552,
0.0747567910363916),.UNSPECIFIED.);
#1810=B_SPLINE_CURVE_WITH_KNOTS('',3,(#171879,#171880,#171881,#171882,#171883,
#171884,#171885,#171886,#171887,#171888,#171889,#171890,#171891,#171892,
#171893,#171894,#171895,#171896,#171897,#171898,#171899,#171900,#171901,
#171902,#171903,#171904,#171905,#171906,#171907,#171908,#171909,#171910,
#171911,#171912,#171913,#171914,#171915,#171916,#171917,#171918,#171919,
#171920,#171921,#171922,#171923,#171924,#171925,#171926,#171927,#171928,
#171929,#171930,#171931,#171932,#171933,#171934,#171935,#171936,#171937,
#171938,#171939,#171940,#171941,#171942,#171943,#171944,#171945,#171946,
#171947,#171948,#171949,#171950,#171951,#171952,#171953,#171954,#171955,
#171956,#171957,#171958,#171959,#171960,#171961,#171962,#171963,#171964,
#171965,#171966,#171967,#171968,#171969,#171970,#171971,#171972,#171973,
#171974,#171975,#171976,#171977,#171978,#171979,#171980,#171981,#171982,
#171983,#171984,#171985,#171986,#171987,#171988,#171989,#171990,#171991,
#171992,#171993,#171994,#171995,#171996,#171997,#171998,#171999,#172000,
#172001,#172002,#172003,#172004,#172005,#172006,#172007,#172008,#172009,
#172010,#172011,#172012,#172013,#172014,#172015,#172016,#172017,#172018,
#172019,#172020,#172021,#172022,#172023,#172024,#172025,#172026,#172027,
#172028,#172029,#172030,#172031,#172032,#172033,#172034,#172035,#172036,
#172037,#172038,#172039,#172040,#172041,#172042,#172043,#172044,#172045,
#172046,#172047,#172048,#172049,#172050,#172051,#172052,#172053,#172054,
#172055,#172056,#172057,#172058,#172059,#172060,#172061,#172062,#172063,
#172064,#172065,#172066,#172067,#172068,#172069,#172070,#172071,#172072,
#172073,#172074,#172075,#172076,#172077,#172078,#172079,#172080,#172081,
#172082,#172083,#172084,#172085,#172086,#172087,#172088,#172089,#172090,
#172091,#172092,#172093,#172094,#172095,#172096,#172097,#172098,#172099,
#172100,#172101,#172102,#172103,#172104,#172105,#172106,#172107,#172108,
#172109,#172110,#172111,#172112,#172113,#172114),.UNSPECIFIED.,.F.,.F.,
(4,2,2,2,2,2,2,2,2,2,2,2,2,2,2,2,2,2,2,2,2,2,2,2,2,2,2,2,2,2,2,2,2,2,2,
2,2,2,2,2,2,2,2,2,2,2,2,2,2,2,2,2,2,2,2,2,2,2,2,2,2,2,2,2,2,2,2,2,2,2,2,
2,2,2,2,2,2,2,2,2,2,2,2,2,2,2,2,2,2,2,2,2,2,2,2,2,2,2,2,2,2,2,2,2,2,2,2,
2,2,2,2,2,2,2,2,2,2,4),(1.25989869578533,1.27803777571643,1.28162356492777,
1.28313446666498,1.28422693449528,1.28525230518831,1.28699267692713,1.29170757564036,
1.33211640603649,1.33400578949135,1.37783005827692,1.38505187095889,1.38797305507987,
1.38977603825891,1.39172949126977,1.39439149081119,1.40055211078964,1.42701754731372,
1.46593296247835,1.47407593030229,1.49134853466584,1.49401699056791,1.49537478041499,
1.49644684866122,1.49769576620184,1.49993375778852,1.51065957418799,1.53436265518954,
1.56173432592115,1.59366388420552,1.59790331481537,1.6004284182099,1.60236658671307,
1.60444676100264,1.60772628288389,1.61830771511249,1.63547407489022,1.68121297299587,
1.68797737603305,1.70342262003362,1.7057904745399,1.70719802739904,1.7082781674308,
1.70948161782518,1.71151344742636,1.71940427865583,1.73412119512362,1.76315957553927,
1.80554479278682,1.80983774025507,1.81237841472571,1.81431912623184,1.81639288268724,
1.81964310673741,1.82996598145874,1.84655579928852,1.87946737489397,1.89550907695404,
1.89932180907876,1.91533533736798,1.91795524474975,1.91930262868772,1.9203739678258,
1.9216307037395,1.92390457432152,1.93523530636968,1.96123440779445,2.01418044130187,
2.02107490612349,2.02394152494074,2.02573446421028,2.02769593144562,2.03040324713488,
2.03682860164504,2.06546697008432,2.11676194568742,2.127805999408,2.12995204042049,
2.13130824240475,2.13238022285594,2.13363037861163,2.13587393020343,2.14669005256395,
2.17072535207003,2.22657436422238,2.23321130725402,2.23575257505088,2.23757909894064,
2.23951763436412,2.24208948632968,2.24774625846598,2.27032990718819,2.30311153642334,
2.33903525050865,2.34189309223774,2.34327070004228,2.34434445197047,2.34557953664187,
2.34775447412086,2.35750779793843,2.40642295223264,2.44153144884381,2.4462092247807,
2.44864312953156,2.45051307210154,2.4525986609391,2.45478120837742,2.45799632070294,
2.4931273459558,2.54892180846205,2.55320147152664,2.55487402507419,2.55588626101695,
2.55698847717449,2.55855264167954,2.56246030563949,2.58162420589184,2.593432104111),
 .UNSPECIFIED.);
#1811=B_SPLINE_CURVE_WITH_KNOTS('',3,(#172115,#172116,#172117,#172118,#172119,
#172120,#172121,#172122,#172123,#172124,#172125,#172126,#172127,#172128,
#172129,#172130,#172131,#172132,#172133,#172134,#172135,#172136,#172137,
#172138,#172139,#172140,#172141,#172142,#172143,#172144,#172145,#172146,
#172147,#172148,#172149,#172150,#172151,#172152,#172153,#172154,#172155,
#172156,#172157,#172158,#172159,#172160,#172161,#172162,#172163,#172164,
#172165,#172166,#172167,#172168,#172169,#172170,#172171,#172172,#172173,
#172174,#172175,#172176,#172177,#172178,#172179,#172180,#172181,#172182,
#172183,#172184,#172185,#172186,#172187,#172188,#172189,#172190,#172191,
#172192,#172193,#172194,#172195,#172196,#172197,#172198,#172199,#172200,
#172201,#172202,#172203,#172204,#172205,#172206,#172207,#172208,#172209,
#172210,#172211,#172212,#172213,#172214,#172215,#172216,#172217,#172218,
#172219,#172220,#172221,#172222,#172223,#172224,#172225,#172226,#172227,
#172228,#172229,#172230,#172231,#172232,#172233,#172234,#172235,#172236,
#172237,#172238,#172239,#172240,#172241,#172242,#172243,#172244,#172245,
#172246,#172247,#172248,#172249,#172250,#172251,#172252,#172253,#172254,
#172255,#172256,#172257,#172258,#172259,#172260,#172261,#172262,#172263,
#172264,#172265,#172266,#172267,#172268,#172269,#172270,#172271,#172272,
#172273,#172274,#172275,#172276,#172277,#172278,#172279,#172280,#172281,
#172282,#172283,#172284,#172285,#172286,#172287,#172288,#172289,#172290,
#172291,#172292,#172293,#172294,#172295,#172296,#172297,#172298,#172299,
#172300,#172301,#172302,#172303,#172304,#172305,#172306,#172307,#172308,
#172309,#172310,#172311,#172312,#172313,#172314,#172315,#172316,#172317,
#172318,#172319,#172320,#172321,#172322,#172323,#172324,#172325,#172326,
#172327,#172328,#172329,#172330,#172331,#172332,#172333,#172334,#172335,
#172336,#172337,#172338,#172339,#172340,#172341,#172342,#172343,#172344,
#172345,#172346),.UNSPECIFIED.,.F.,.F.,(4,2,2,2,2,2,2,2,2,2,2,2,2,2,2,2,
2,2,2,2,2,2,2,2,2,2,2,2,2,2,2,2,2,2,2,2,2,2,2,2,2,2,2,2,2,2,2,2,2,2,2,2,
2,2,2,2,2,2,2,2,2,2,2,2,2,2,2,2,2,2,2,2,2,2,2,2,2,2,2,2,2,2,2,2,2,2,2,2,
2,2,2,2,2,2,2,2,2,2,2,2,2,2,2,2,2,2,2,2,2,2,2,2,2,2,2,4),(0.0747567910363916,
0.101524456188114,0.118346548840528,0.145432256689375,0.159880953081397,
0.163459317400085,0.165647666653395,0.167561843337173,0.169931194533515,
0.173564887856589,0.190666959648489,0.198773286722755,0.245100186900313,
0.260632355566143,0.268815353103309,0.270871847159655,0.272080733752706,
0.273159431087181,0.274556848020972,0.276890151957204,0.291506356757988,
0.299696300380568,0.34502341145215,0.362077704187808,0.372610104253377,
0.375884008462693,0.377962883583548,0.379901417889835,0.382429253110941,
0.386678305314137,0.419101082480044,0.458224706501592,0.472935778016126,
0.480823614708884,0.482855127579296,0.484058466147926,0.485138565467233,
0.48654612900863,0.488914132671086,0.504367042265317,0.508620048289381,
0.55660453872408,0.573910610266322,0.5845550577961,0.587841519528848,0.589923159197865,
0.591860656859772,0.594381984499563,0.59860868992616,0.629910818680944,
0.669588251031157,0.684726668285683,0.692769187121374,0.694813921609099,
0.696020203173269,0.697099552472877,0.698501702836229,0.700851153343846,
0.715850274499841,0.723372725573538,0.766610548811049,0.785190513985374,
0.796390695477342,0.799737676515783,0.801832694909756,0.803765623544705,
0.806257092661958,0.810381720935304,0.837505843098225,0.879435091935224,
0.896079190237384,0.904649081155813,0.906736988979772,0.907952878982071,
0.909030060660038,0.910415486231704,0.912707886900142,0.926461256037331,
0.92845511125291,0.929506506256935,0.973860518976542,1.0032293632098,1.00974182670138,
1.0124638652835,1.01442809703748,1.01621815767796,1.01906846476732,1.02586344113182,
1.0800715532697,1.10523451812109,1.11634943610266,1.11861090576434,1.11986498931481,
1.12093663326277,1.122287669134,1.12492433827512,1.14135478892318,1.19194117065031,
1.20965194988409,1.22047513781774,1.22378150584,1.22586761666604,1.22780366471858,
1.23031514840125,1.23450785801299,1.2642510280766,1.30519338753996,1.32767219399301,
1.33033551699752,1.33167430526232,1.33264224568188,1.33386581355116,1.33598825623172,
1.34500663884769,1.36299113618112,1.40819788515412),.UNSPECIFIED.);
#1812=B_SPLINE_CURVE_WITH_KNOTS('',3,(#172352,#172353,#172354,#172355,#172356,
#172357),.UNSPECIFIED.,.F.,.F.,(4,2,4),(2.59390093981336,2.60707187553918,
2.66837754069951),.UNSPECIFIED.);
#1813=B_SPLINE_CURVE_WITH_KNOTS('',3,(#172358,#172359,#172360,#172361,#172362,
#172363,#172364,#172365,#172366,#172367,#172368,#172369,#172370,#172371,
#172372,#172373,#172374,#172375,#172376,#172377,#172378,#172379,#172380,
#172381,#172382,#172383,#172384,#172385,#172386,#172387,#172388,#172389,
#172390,#172391,#172392,#172393,#172394,#172395,#172396,#172397,#172398,
#172399,#172400,#172401,#172402,#172403,#172404,#172405,#172406,#172407,
#172408,#172409,#172410,#172411,#172412,#172413,#172414,#172415,#172416,
#172417,#172418,#172419,#172420,#172421,#172422,#172423,#172424,#172425,
#172426,#172427,#172428,#172429,#172430,#172431,#172432,#172433,#172434,
#172435,#172436,#172437,#172438,#172439,#172440,#172441,#172442,#172443,
#172444,#172445,#172446,#172447,#172448,#172449,#172450,#172451,#172452,
#172453,#172454,#172455,#172456,#172457,#172458,#172459,#172460,#172461,
#172462,#172463,#172464,#172465,#172466,#172467,#172468,#172469,#172470,
#172471,#172472,#172473,#172474,#172475,#172476,#172477,#172478,#172479,
#172480,#172481,#172482,#172483,#172484,#172485,#172486,#172487,#172488,
#172489,#172490,#172491,#172492,#172493,#172494,#172495,#172496,#172497,
#172498,#172499,#172500,#172501,#172502,#172503,#172504,#172505,#172506,
#172507,#172508,#172509,#172510,#172511,#172512,#172513,#172514,#172515,
#172516,#172517,#172518,#172519,#172520,#172521,#172522,#172523,#172524,
#172525,#172526,#172527,#172528,#172529,#172530,#172531,#172532,#172533,
#172534,#172535,#172536,#172537,#172538,#172539,#172540,#172541,#172542,
#172543,#172544,#172545,#172546,#172547,#172548,#172549,#172550,#172551,
#172552,#172553,#172554,#172555,#172556,#172557,#172558,#172559,#172560,
#172561,#172562,#172563,#172564,#172565,#172566,#172567,#172568,#172569,
#172570,#172571,#172572,#172573,#172574,#172575,#172576,#172577,#172578,
#172579),.UNSPECIFIED.,.F.,.F.,(4,2,2,2,2,2,2,2,2,2,2,2,2,2,2,2,2,2,2,2,
2,2,2,2,2,2,2,2,2,2,2,2,2,2,2,2,2,2,2,2,2,2,2,2,2,2,2,2,2,2,2,2,2,2,2,2,
2,2,2,2,2,2,2,2,2,2,2,2,2,2,2,2,2,2,2,2,2,2,2,2,2,2,2,2,2,2,2,2,2,2,2,2,
2,2,2,2,2,2,2,2,2,2,2,2,2,2,2,2,2,2,4),(0.000810723700984357,0.00554261320572169,
0.00881069613611283,0.0102445762039883,0.0113189850637518,0.0123418017107931,
0.0133650037427745,0.0148060202972169,0.0186526222153408,0.0263910138025746,
0.0845154634150867,0.101772990584215,0.112395144693521,0.115678587832717,
0.117759219523011,0.119696406054065,0.122218222684451,0.126447724277269,
0.173069879744072,0.206916380206583,0.215664608440691,0.219322954632772,
0.221287249650054,0.222573677503932,0.223776849680925,0.22482590592252,
0.226194489868468,0.229007450046979,0.249970475940634,0.296516239281409,
0.320113757092421,0.325905911678698,0.328502109144104,0.33044413263795,
0.332263139443331,0.334776779899351,0.341243839866894,0.398654564430561,
0.421697202537265,0.43223953036286,0.4344659005549,0.435712141173873,0.436784282095004,
0.438145210124105,0.440307245485743,0.451618775422881,0.50268263979348,
0.531210900458154,0.537623037990028,0.540327828391182,0.542288575578362,
0.544081624667631,0.546950080227899,0.55385754424516,0.606640332115945,
0.632772141474778,0.644135100401236,0.646410562123642,0.6476675096593,0.648738627836554,
0.650085217047887,0.652200234739836,0.662760126223501,0.667525711208819,
0.675217676847446,0.688623006160559,0.721474362986219,0.74421396470811,
0.74989188453549,0.752467461194726,0.754406417472323,0.756231591622129,
0.758768184481559,0.765376370826019,0.821528588747223,0.845386821096472,
0.856153865520107,0.858394305382391,0.859643708330882,0.860715653031557,
0.862072585294457,0.864737252988573,0.88191157182582,0.92740438682891,0.955260646894826,
0.961592343664603,0.964283692718814,0.966242221573491,0.968038452126711,
0.970923412728924,0.977929436993805,1.02926394257437,1.05643268653373,1.06805495714825,
1.07034525125476,1.07160551861432,1.07267652835782,1.07401925675635,1.07661772789688,
1.09212829312262,1.09870253532691,1.14007976721838,1.16734411190291,1.17360381401307,
1.17628290258083,1.17823931534818,1.18003834465021,1.18293826439588,1.19003363050845,
1.23966140302115,1.25989869578533),.UNSPECIFIED.);
#1814=B_SPLINE_CURVE_WITH_KNOTS('',3,(#172581,#172582,#172583,#172584,#172585,
#172586,#172587,#172588,#172589,#172590,#172591,#172592,#172593,#172594,
#172595,#172596,#172597,#172598,#172599,#172600,#172601,#172602,#172603,
#172604,#172605,#172606,#172607,#172608,#172609,#172610,#172611,#172612,
#172613,#172614,#172615,#172616,#172617,#172618,#172619,#172620,#172621,
#172622,#172623,#172624,#172625,#172626,#172627,#172628,#172629,#172630,
#172631,#172632,#172633,#172634,#172635,#172636,#172637,#172638,#172639,
#172640,#172641,#172642,#172643,#172644,#172645,#172646,#172647,#172648,
#172649,#172650,#172651,#172652,#172653,#172654,#172655,#172656,#172657,
#172658,#172659,#172660,#172661,#172662,#172663,#172664,#172665,#172666,
#172667,#172668,#172669,#172670,#172671,#172672,#172673,#172674,#172675,
#172676,#172677,#172678,#172679,#172680,#172681,#172682,#172683,#172684,
#172685,#172686,#172687,#172688,#172689,#172690,#172691,#172692,#172693,
#172694,#172695,#172696,#172697,#172698,#172699,#172700,#172701,#172702,
#172703,#172704,#172705,#172706,#172707,#172708,#172709,#172710,#172711,
#172712,#172713,#172714,#172715,#172716,#172717,#172718,#172719,#172720,
#172721,#172722,#172723,#172724,#172725,#172726,#172727,#172728,#172729,
#172730,#172731,#172732,#172733,#172734,#172735,#172736,#172737,#172738,
#172739,#172740,#172741,#172742,#172743,#172744,#172745,#172746,#172747,
#172748,#172749,#172750,#172751,#172752,#172753,#172754,#172755,#172756,
#172757,#172758,#172759,#172760,#172761,#172762,#172763,#172764,#172765,
#172766,#172767,#172768,#172769,#172770,#172771,#172772,#172773,#172774,
#172775,#172776,#172777,#172778,#172779,#172780,#172781,#172782,#172783,
#172784,#172785,#172786,#172787,#172788,#172789,#172790,#172791,#172792,
#172793,#172794,#172795,#172796,#172797,#172798,#172799,#172800,#172801,
#172802,#172803,#172804,#172805,#172806,#172807,#172808),.UNSPECIFIED.,
 .F.,.F.,(4,2,2,2,2,2,2,2,2,2,2,2,2,2,2,2,2,2,2,2,2,2,2,2,2,2,2,2,2,2,2,
2,2,2,2,2,2,2,2,2,2,2,2,2,2,2,2,2,2,2,2,2,2,2,2,2,2,2,2,2,2,2,2,2,2,2,2,
2,2,2,2,2,2,2,2,2,2,2,2,2,2,2,2,2,2,2,2,2,2,2,2,2,2,2,2,2,2,2,2,2,2,2,2,
2,2,2,2,2,2,2,2,2,2,4),(1.40819788515412,1.41320480955033,1.43100805154192,
1.43468737730319,1.43707091781286,1.43898633702858,1.44116501332167,1.44488970303174,
1.46029553252312,1.51162818140741,1.5393065028968,1.5422133536684,1.5436006137059,
1.54467541768557,1.54590445995735,1.54805162669176,1.55740693895738,1.60667065956928,
1.64189277627461,1.64618928346868,1.64873098295828,1.65067185451119,1.652745178032,
1.6559934624727,1.66629954363591,1.68285225744042,1.71573289764331,1.72917870687183,
1.73676473242227,1.75176082213401,1.75411020406588,1.75551233516349,1.75659168476984,
1.75779799561915,1.75984282695774,1.76788652127728,1.78302608529412,1.8227323590549,
1.85396287365098,1.85818793187896,1.86070881328773,1.86264627009395,1.86472816143071,
1.86801564589376,1.87866880699907,1.89599683009939,1.94421862210615,1.94852171496344,
1.95176755675804,1.96398266332999,1.96619652137505,1.96757330590134,1.96864703367207,
1.96988278797529,1.97206057371562,1.98185431033581,2.03073864750066,2.06584379556519,
2.07013863983217,2.07267980745666,2.07462053312108,2.07669395313408,2.07994291562159,
2.090255589143,2.1068231165886,2.13971533624545,2.15436242289754,2.15958048548214,
2.17562924673426,2.17825123591975,2.17959903316586,2.18067035545633,2.181926671319,
2.18419876504807,2.19549982453134,2.22138329857757,2.27449172343357,2.28137310471485,
2.28423749466763,2.28602997251859,2.28799168504442,2.29070071537147,2.29713666181787,
2.306024990725,2.35723578537287,2.38723379368933,2.39014813385419,2.39153676628313,
2.39261161996421,2.39383958551193,2.39598221501358,2.40527662675433,2.42411888605869,
2.47030817984565,2.47176799657821,2.49079024426924,2.49454973560932,2.49695784527914,
2.49887534941399,2.50067253519439,2.50376503716656,2.51330922614352,2.52830875451936,
2.55060007977405,2.59664756030106,2.60129276543145,2.60302251666345,2.60404578508964,
2.60513955821508,2.60665806800296,2.61028885532386,2.61539962203938,2.62956644507116,
2.66719749894963),.UNSPECIFIED.);
#1815=B_SPLINE_CURVE_WITH_KNOTS('',3,(#172809,#172810,#172811,#172812,#172813,
#172814,#172815,#172816,#172817,#172818,#172819,#172820,#172821,#172822,
#172823,#172824,#172825,#172826,#172827,#172828),.UNSPECIFIED.,.F.,.F.,
(4,2,2,2,2,2,2,2,2,4),(0.000704185054399313,0.0257176001801729,0.0359848483797077,
0.0390635712064609,0.0411898671505945,0.04327101724974,0.0452083777863691,
0.0477299809557773,0.0519581517589747,0.0751489472892387),.UNSPECIFIED.);
#1816=B_SPLINE_CURVE_WITH_KNOTS('',3,(#172833,#172834,#172835,#172836,#172837,
#172838,#172839,#172840,#172841,#172842,#172843,#172844,#172845,#172846,
#172847,#172848,#172849,#172850,#172851,#172852,#172853,#172854,#172855,
#172856,#172857,#172858,#172859,#172860,#172861,#172862,#172863,#172864,
#172865,#172866,#172867,#172868,#172869,#172870,#172871,#172872,#172873,
#172874,#172875,#172876,#172877,#172878,#172879,#172880,#172881,#172882,
#172883,#172884,#172885,#172886,#172887,#172888,#172889,#172890,#172891,
#172892,#172893,#172894,#172895,#172896,#172897,#172898,#172899,#172900,
#172901,#172902,#172903,#172904,#172905,#172906,#172907,#172908,#172909,
#172910,#172911,#172912,#172913,#172914,#172915,#172916,#172917,#172918,
#172919,#172920,#172921,#172922,#172923,#172924,#172925,#172926,#172927,
#172928,#172929,#172930,#172931,#172932,#172933,#172934,#172935,#172936,
#172937,#172938,#172939,#172940,#172941,#172942,#172943,#172944,#172945,
#172946,#172947,#172948,#172949,#172950,#172951,#172952,#172953,#172954,
#172955,#172956,#172957,#172958,#172959,#172960,#172961,#172962,#172963,
#172964,#172965,#172966,#172967,#172968,#172969,#172970,#172971,#172972,
#172973,#172974,#172975,#172976,#172977,#172978,#172979,#172980,#172981,
#172982,#172983,#172984,#172985,#172986,#172987,#172988,#172989,#172990,
#172991,#172992,#172993,#172994,#172995,#172996,#172997,#172998,#172999,
#173000,#173001,#173002,#173003,#173004,#173005,#173006,#173007,#173008,
#173009,#173010,#173011,#173012,#173013,#173014,#173015,#173016,#173017,
#173018,#173019,#173020,#173021,#173022,#173023,#173024,#173025,#173026,
#173027,#173028,#173029,#173030,#173031,#173032,#173033,#173034,#173035,
#173036,#173037,#173038,#173039,#173040,#173041,#173042,#173043,#173044,
#173045,#173046,#173047,#173048,#173049,#173050,#173051,#173052,#173053,
#173054,#173055,#173056,#173057,#173058,#173059,#173060,#173061,#173062,
#173063,#173064,#173065,#173066,#173067,#173068,#173069,#173070,#173071,
#173072,#173073,#173074,#173075,#173076,#173077,#173078,#173079,#173080,
#173081,#173082,#173083,#173084,#173085,#173086,#173087,#173088,#173089,
#173090,#173091,#173092,#173093,#173094,#173095,#173096,#173097,#173098,
#173099,#173100,#173101,#173102,#173103,#173104),.UNSPECIFIED.,.F.,.F.,
(4,2,2,2,2,2,2,2,2,2,2,2,2,2,2,2,2,2,2,2,2,2,2,2,2,2,2,2,2,2,2,2,2,2,2,
2,2,2,2,2,2,2,2,2,2,2,2,2,2,2,2,2,2,2,2,2,2,2,2,2,2,2,2,2,2,2,2,2,2,2,2,
2,2,2,2,2,2,2,2,2,2,2,2,2,2,2,2,2,2,2,2,2,2,2,2,2,2,2,2,2,2,2,2,2,2,2,2,
2,2,2,2,2,2,2,2,2,2,2,2,2,2,2,2,2,2,2,2,2,2,2,2,2,2,2,2,4),(1.26009529204153,
1.26844197493161,1.29381908665805,1.29808977294706,1.30038729580617,1.30228035921571,
1.30452109389515,1.30842023916197,1.32432886191597,1.33455106590784,1.3738352565579,
1.4024193346263,1.40533187738955,1.40672042186942,1.40779556129193,1.40902424908107,
1.41116906596271,1.42048729387565,1.46966352868001,1.50503251890401,1.50933167680465,
1.51187442603891,1.51381580080436,1.51588937269098,1.51913744272381,1.52943776213862,
1.54597639320325,1.57352305450409,1.58966610161661,1.60074910637597,1.61498196810458,
1.61729842640309,1.61869106011059,1.6197693270595,1.62098139213644,1.62305141293665,
1.63139524163988,1.6473807097364,1.68969665771436,1.71730662606135,1.72144413217767,
1.72393965127285,1.72587350083235,1.72796729970624,1.73130752743709,1.74244013679484,
1.76086405966356,1.80763034731911,1.81232709764671,1.82696406662867,1.82929874004238,
1.83069673086658,1.8317757227877,1.83298478601298,1.83504122555829,1.84321961617839,
1.85873479280358,1.90015323793686,1.90975608772036,1.92990197006417,1.9337241801803,
1.93615182087995,1.93807174021844,1.94022284482432,1.94382155599842,1.95765691707316,
2.00858847432579,2.03848478022232,2.04140011095768,2.04278919146687,2.04386438098087,
2.04509271791304,2.04723596667405,2.05653262121604,2.07537870364252,2.11578208748357,
2.1280448874829,2.1426640883555,2.14645403678354,2.14866967292115,2.15058229072505,
2.15291750737014,2.15736701469366,2.18823827194742,2.2346751533935,2.25091584498385,
2.25354556935495,2.25489531762309,2.25596712881483,2.25722278915879,2.25949058324815,
2.27070702311502,2.29625407243746,2.34988213657719,2.35672626840969,2.35958516041191,
2.36137710810909,2.36334058690595,2.3660563714244,2.37252891301422,2.42683246281601,
2.46271444433038,2.46557632123003,2.46695503000674,2.4679977587146,2.46800240941345,
2.46800697901051,2.46801146932995,2.4680158820592,2.46802021881731,2.468024481455,
2.46802867152553,2.4680327904781,2.4680368398472,2.46804082120923,2.46804473593346,
2.46804858533323,2.46805217845779,2.46805575817054,2.46805932453551,2.46806287762952,
2.46928594144211,2.47059639747212,2.47261801169278,2.47642684073078,2.48568673577153,
2.52344240916099,2.5331599780408,2.56531506690709,2.56956000770442,2.57208710202107,
2.57402604819646,2.57610632274238,2.5793844513405,2.5899478892837,2.59390093981336),
 .UNSPECIFIED.);
#1817=B_SPLINE_CURVE_WITH_KNOTS('',3,(#173105,#173106,#173107,#173108,#173109,
#173110,#173111,#173112,#173113,#173114,#173115,#173116,#173117,#173118,
#173119,#173120,#173121,#173122,#173123,#173124,#173125,#173126,#173127,
#173128,#173129,#173130,#173131,#173132,#173133,#173134,#173135,#173136,
#173137,#173138,#173139,#173140,#173141,#173142,#173143,#173144,#173145,
#173146,#173147,#173148,#173149,#173150,#173151,#173152,#173153,#173154,
#173155,#173156,#173157,#173158,#173159,#173160,#173161,#173162,#173163,
#173164,#173165,#173166,#173167,#173168,#173169,#173170,#173171,#173172,
#173173,#173174,#173175,#173176,#173177,#173178,#173179,#173180,#173181,
#173182,#173183,#173184,#173185,#173186,#173187,#173188,#173189,#173190,
#173191,#173192,#173193,#173194,#173195,#173196,#173197,#173198,#173199,
#173200,#173201,#173202,#173203,#173204,#173205,#173206,#173207,#173208,
#173209,#173210,#173211,#173212,#173213,#173214,#173215,#173216,#173217,
#173218,#173219,#173220,#173221,#173222,#173223,#173224,#173225,#173226,
#173227,#173228,#173229,#173230,#173231,#173232,#173233,#173234,#173235,
#173236,#173237,#173238,#173239,#173240,#173241,#173242,#173243,#173244,
#173245,#173246,#173247,#173248,#173249,#173250,#173251,#173252,#173253,
#173254,#173255,#173256,#173257,#173258,#173259,#173260,#173261,#173262,
#173263,#173264,#173265,#173266,#173267,#173268,#173269,#173270,#173271,
#173272,#173273,#173274,#173275,#173276,#173277,#173278,#173279,#173280,
#173281,#173282,#173283,#173284,#173285,#173286,#173287,#173288,#173289,
#173290,#173291,#173292,#173293,#173294,#173295,#173296,#173297,#173298,
#173299,#173300,#173301,#173302,#173303,#173304,#173305,#173306,#173307,
#173308,#173309,#173310,#173311,#173312,#173313,#173314,#173315,#173316,
#173317,#173318,#173319,#173320,#173321,#173322,#173323,#173324,#173325,
#173326,#173327,#173328,#173329,#173330,#173331,#173332,#173333,#173334),
 .UNSPECIFIED.,.F.,.F.,(4,2,2,2,2,2,2,2,2,2,2,2,2,2,2,2,2,2,2,2,2,2,2,2,
2,2,2,2,2,2,2,2,2,2,2,2,2,2,2,2,2,2,2,2,2,2,2,2,2,2,2,2,2,2,2,2,2,2,2,2,
2,2,2,2,2,2,2,2,2,2,2,2,2,2,2,2,2,2,2,2,2,2,2,2,2,2,2,2,2,2,2,2,2,2,2,2,
2,2,2,2,2,2,2,2,2,2,2,2,2,2,2,2,2,2,4),(0.0751489472892387,0.0833506903298647,
0.108693179478461,0.136624479574853,0.145910581493636,0.148052443073946,
0.149280142392567,0.150354881899416,0.151743512998436,0.153997122734652,
0.16697267146495,0.188669927722425,0.21538790536825,0.23698283912962,0.245199084137935,
0.251208117972463,0.253835202657818,0.255791748353884,0.257590251491323,
0.260487889091777,0.267570463669636,0.317768473763119,0.35556512818206,
0.359164548317838,0.360677695364973,0.361770484303532,0.362795121015494,
0.364532042274383,0.369224770895711,0.410121627603691,0.456727760812597,
0.463120295750263,0.465821963995688,0.46778232474392,0.469576314887164,
0.472449100333618,0.479381604657555,0.53183102652881,0.558205007536708,
0.569629676589747,0.571908849257935,0.57316669435742,0.574237879798275,
0.575583666863853,0.578196353888663,0.594048508720194,0.598800004794369,
0.614070759120716,0.646946875496303,0.663528766522946,0.673848955191107,
0.677098762767563,0.679172362956032,0.681113005616564,0.683653702799897,
0.687946973484252,0.730347412354117,0.759404062666403,0.774125704647657,
0.782017411858803,0.784049267769345,0.785252687682802,0.786332774959836,
0.787740211173355,0.790107761588505,0.805548807216033,0.812259157611298,
0.826060037640182,0.858920747327703,0.875483046744663,0.885794498952606,
0.889043394098526,0.891116853804617,0.893057675231676,0.895599054028324,
0.89989447953962,0.935013678434636,0.983922775958131,0.993722716270286,
0.995901057091978,0.997136987612726,0.998210784689413,0.999587539076382,
1.00244049216916,1.02510696755175,1.03806638041779,1.07092231103286,1.0874764009265,
1.09778443824991,1.10103316035812,1.10310672663729,1.10504780027098,1.10758972929978,
1.11188657793559,1.14708330643099,1.19623165405848,1.20575819674281,1.20791776643048,
1.20914964803851,1.21022418219166,1.21160746587854,1.21384242657101,1.22644656507153,
1.23298155019536,1.23811527952155,1.27817831512221,1.30768219107849,1.31209262371577,
1.31441956312134,1.31614666045631,1.31830310095657,1.32192594696099,1.33437674435756,
1.38533771546958,1.40863959751122),.UNSPECIFIED.);
#1818=B_SPLINE_CURVE_WITH_KNOTS('',3,(#173340,#173341,#173342,#173343,#173344,
#173345,#173346,#173347,#173348,#173349),.UNSPECIFIED.,.F.,.F.,(4,2,2,2,
4),(2.59331024535127,2.59403892110998,2.60403517669797,2.65275213854603,
2.66748114715309),.UNSPECIFIED.);
#1819=B_SPLINE_CURVE_WITH_KNOTS('',3,(#173350,#173351,#173352,#173353,#173354,
#173355,#173356,#173357,#173358,#173359,#173360,#173361,#173362,#173363,
#173364,#173365,#173366,#173367,#173368,#173369,#173370,#173371,#173372,
#173373,#173374,#173375,#173376,#173377,#173378,#173379,#173380,#173381,
#173382,#173383,#173384,#173385,#173386,#173387,#173388,#173389,#173390,
#173391,#173392,#173393,#173394,#173395,#173396,#173397,#173398,#173399,
#173400,#173401,#173402,#173403,#173404,#173405,#173406,#173407,#173408,
#173409,#173410,#173411,#173412,#173413,#173414,#173415,#173416,#173417,
#173418,#173419,#173420,#173421,#173422,#173423,#173424,#173425,#173426,
#173427,#173428,#173429,#173430,#173431,#173432,#173433,#173434,#173435,
#173436,#173437,#173438,#173439,#173440,#173441,#173442,#173443,#173444,
#173445,#173446,#173447,#173448,#173449,#173450,#173451,#173452,#173453,
#173454,#173455,#173456,#173457,#173458,#173459,#173460,#173461,#173462,
#173463,#173464,#173465,#173466,#173467,#173468,#173469,#173470,#173471,
#173472,#173473,#173474,#173475,#173476,#173477,#173478,#173479,#173480,
#173481,#173482,#173483,#173484,#173485,#173486,#173487,#173488,#173489,
#173490,#173491,#173492,#173493,#173494,#173495,#173496,#173497,#173498,
#173499,#173500,#173501,#173502,#173503,#173504,#173505,#173506,#173507,
#173508,#173509,#173510,#173511,#173512,#173513,#173514,#173515,#173516,
#173517,#173518,#173519,#173520,#173521,#173522,#173523,#173524,#173525,
#173526,#173527,#173528,#173529,#173530,#173531,#173532,#173533,#173534,
#173535,#173536,#173537,#173538,#173539,#173540,#173541,#173542,#173543,
#173544,#173545,#173546,#173547,#173548,#173549,#173550,#173551,#173552,
#173553,#173554,#173555,#173556,#173557,#173558,#173559,#173560,#173561,
#173562,#173563,#173564,#173565,#173566,#173567,#173568,#173569,#173570,
#173571,#173572,#173573,#173574,#173575,#173576,#173577,#173578,#173579),
 .UNSPECIFIED.,.F.,.F.,(4,2,2,2,2,2,2,2,2,2,2,2,2,2,2,2,2,2,2,2,2,2,2,2,
2,2,2,2,2,2,2,2,2,2,2,2,2,2,2,2,2,2,2,2,2,2,2,2,2,2,2,2,2,2,2,2,2,2,2,2,
2,2,2,2,2,2,2,2,2,2,2,2,2,2,2,2,2,2,2,2,2,2,2,2,2,2,2,2,2,2,2,2,2,2,2,2,
2,2,2,2,2,2,2,2,2,2,2,2,2,2,2,2,2,2,4),(0.000768636914663262,0.0205817132677007,
0.0241264022558527,0.026446080246186,0.028288539982056,0.0301791844248606,
0.0323538709578556,0.0360614126099366,0.049342268561374,0.061439469886042,
0.106920494045923,0.123352098338178,0.131848845865215,0.13393077347796,
0.135145246475461,0.136222568716977,0.137609978393136,0.139909404628916,
0.153812066318087,0.165109782804785,0.176052200725826,0.208884599686808,
0.225415111063631,0.232254426277596,0.237451466882633,0.239925174807285,
0.241763389965213,0.243586282406605,0.246113909055398,0.252665291008623,
0.30933679523107,0.332864760921927,0.343541974817081,0.345777015734982,
0.347025293118148,0.348097439213071,0.349456126762224,0.351610368308616,
0.362788846072325,0.413971378521812,0.44254087089606,0.448958497584014,
0.45166452002466,0.453625766366755,0.455419000618713,0.458287161407423,
0.465190855672874,0.518047399066889,0.544139800981525,0.555493658326147,
0.557768904828446,0.559025948816909,0.560097279759711,0.561444302573145,
0.564062478863939,0.580044465753803,0.585011842731264,0.629859531159875,
0.648373658759317,0.659545647407061,0.662889680195208,0.664984078341141,
0.666917267473081,0.669410236886387,0.673539868929175,0.70085739816818,
0.74313635257933,0.759386683810092,0.767821327391028,0.769898481825624,
0.771112004744916,0.772189727806955,0.773579262729555,0.775885560930745,
0.789924643106426,0.791267448697257,0.798277731012625,0.811953601280656,
0.844814457685017,0.861375925978386,0.87168712574952,0.874936082465282,
0.877009615376341,0.878950529147309,0.881492063235158,0.885787828271423,
0.92091998429791,0.969866143718762,0.979625110904711,0.981800719637479,
0.983036082909888,0.984110016300242,0.985487767876626,0.988345616264717,
1.01120495290628,1.02397087336264,1.05682646448888,1.07337913078648,1.08368664822321,
1.08693540174869,1.08900903502374,1.09095020435551,1.09349230630476,1.09778955396186,
1.1330040871773,1.1822091972939,1.19167318002121,1.19382839647008,1.19505935262069,
1.19613408823427,1.19751895765512,1.19975907997433,1.21246035582909,1.23483790921113,
1.26009529204153),.UNSPECIFIED.);
#1820=B_SPLINE_CURVE_WITH_KNOTS('',3,(#173581,#173582,#173583,#173584,#173585,
#173586,#173587,#173588,#173589,#173590,#173591,#173592,#173593,#173594,
#173595,#173596,#173597,#173598,#173599,#173600,#173601,#173602,#173603,
#173604,#173605,#173606,#173607,#173608,#173609,#173610,#173611,#173612,
#173613,#173614,#173615,#173616,#173617,#173618,#173619,#173620,#173621,
#173622,#173623,#173624,#173625,#173626,#173627,#173628,#173629,#173630,
#173631,#173632,#173633,#173634,#173635,#173636,#173637,#173638,#173639,
#173640,#173641,#173642,#173643,#173644,#173645,#173646,#173647,#173648,
#173649,#173650,#173651,#173652,#173653,#173654,#173655,#173656,#173657,
#173658,#173659,#173660,#173661,#173662,#173663,#173664,#173665,#173666,
#173667,#173668,#173669,#173670,#173671,#173672,#173673,#173674,#173675,
#173676,#173677,#173678,#173679,#173680,#173681,#173682,#173683,#173684,
#173685,#173686,#173687,#173688,#173689,#173690,#173691,#173692,#173693,
#173694,#173695,#173696,#173697,#173698,#173699,#173700,#173701,#173702,
#173703,#173704,#173705,#173706,#173707,#173708,#173709,#173710,#173711,
#173712,#173713,#173714,#173715,#173716,#173717,#173718,#173719,#173720,
#173721,#173722,#173723,#173724,#173725,#173726,#173727,#173728,#173729,
#173730,#173731,#173732,#173733,#173734,#173735,#173736,#173737,#173738,
#173739,#173740,#173741,#173742,#173743,#173744,#173745,#173746,#173747,
#173748,#173749,#173750,#173751,#173752,#173753,#173754,#173755,#173756,
#173757,#173758,#173759,#173760,#173761,#173762,#173763,#173764,#173765,
#173766,#173767,#173768,#173769,#173770,#173771,#173772,#173773,#173774,
#173775,#173776,#173777,#173778,#173779,#173780,#173781,#173782,#173783,
#173784,#173785,#173786,#173787,#173788,#173789,#173790,#173791,#173792,
#173793,#173794,#173795,#173796,#173797,#173798,#173799,#173800,#173801,
#173802),.UNSPECIFIED.,.F.,.F.,(4,2,2,2,2,2,2,2,2,2,2,2,2,2,2,2,2,2,2,2,
2,2,2,2,2,2,2,2,2,2,2,2,2,2,2,2,2,2,2,2,2,2,2,2,2,2,2,2,2,2,2,2,2,2,2,2,
2,2,2,2,2,2,2,2,2,2,2,2,2,2,2,2,2,2,2,2,2,2,2,2,2,2,2,2,2,2,2,2,2,2,2,2,
2,2,2,2,2,2,2,2,2,2,2,2,2,2,2,2,2,2,4),(1.40863959751122,1.41654759067579,
1.41946078381403,1.42084944450047,1.42192458464356,1.42315317340584,1.42529758347594,
1.43461042542615,1.48376959661748,1.5191601098776,1.52345947761638,1.52600227178987,
1.52794363529235,1.53001715098209,1.53326504082311,1.54356401310051,1.56009974390899,
1.59297017588028,1.60449587310241,1.61425425826926,1.61606576418613,1.62921191722976,
1.63147476742771,1.63286642133205,1.63394180950153,1.63516837213546,1.63730385572504,
1.64649544979417,1.66501336722716,1.70917978599597,1.73178633348039,1.73573586227892,
1.73820212937626,1.74012635122654,1.74225532216663,1.74575440825437,1.75847661449871,
1.78077943937613,1.82579017005966,1.82762712554879,1.84118669695806,1.84347004156279,
1.84485293422678,1.84592998128415,1.84714779953147,1.84924371411316,1.85791204470865,
1.87484183103985,1.91719759816998,1.94351200520008,1.94761628936432,1.95010205233999,
1.95203446662113,1.95413284985835,1.95749374744105,1.96882119406152,1.98770007500022,
2.01701249497808,2.05265810089185,2.05552162619937,2.05690053739703,2.05797463164986,
2.05920935040837,2.06138182983116,2.07109429955398,2.12005725862705,2.15519127292122,
2.15948716125025,2.16202885601732,2.16396993208504,2.16604367586266,2.16929304002328,
2.17960609773535,2.1961733948144,2.22906873476792,2.26467869901025,2.26754489693501,
2.26892430287168,2.26999841142197,2.27123272833024,2.27340350338935,2.28309202634423,
2.33207329946603,2.3672124659043,2.37150828505844,2.37404991356645,2.37599092444375,
2.3780645844294,2.38131378776061,2.39162608602794,2.40819192620058,2.47083284402741,
2.47219421687869,2.47836789584991,2.48030628444921,2.48148909542873,2.48252076879123,
2.48393385037511,2.48694890762154,2.49104708912107,2.50132546172915,2.52414790866332,
2.57586043076164,2.58284430851619,2.58572619525003,2.58752230324613,2.58948213431421,
2.59217787903489,2.59853205712364,2.62656945764179,2.66826062582537),
 .UNSPECIFIED.);
#1821=B_SPLINE_CURVE_WITH_KNOTS('',3,(#173803,#173804,#173805,#173806,#173807,
#173808,#173809,#173810,#173811,#173812,#173813,#173814,#173815),
 .UNSPECIFIED.,.F.,.F.,(4,3,3,3,4),(-48.174029021668,-48.070804166684,-47.9674104177172,
-47.94414959817,-47.8233361836797),.UNSPECIFIED.);
#1822=B_SPLINE_CURVE_WITH_KNOTS('',3,(#173820,#173821,#173822,#173823,#173824,
#173825,#173826,#173827,#173828,#173829,#173830,#173831,#173832,#173833,
#173834,#173835,#173836,#173837,#173838,#173839,#173840,#173841,#173842,
#173843,#173844,#173845,#173846,#173847,#173848,#173849,#173850,#173851,
#173852,#173853,#173854,#173855,#173856,#173857,#173858,#173859,#173860,
#173861,#173862,#173863,#173864,#173865,#173866,#173867,#173868,#173869,
#173870,#173871,#173872,#173873,#173874,#173875,#173876,#173877,#173878,
#173879,#173880,#173881,#173882,#173883,#173884,#173885,#173886,#173887,
#173888,#173889,#173890,#173891,#173892,#173893,#173894,#173895,#173896,
#173897,#173898,#173899,#173900,#173901,#173902,#173903,#173904,#173905,
#173906,#173907,#173908,#173909,#173910,#173911,#173912,#173913,#173914,
#173915,#173916,#173917,#173918,#173919,#173920,#173921,#173922,#173923,
#173924,#173925,#173926,#173927,#173928,#173929,#173930,#173931,#173932,
#173933,#173934,#173935,#173936,#173937,#173938,#173939,#173940,#173941,
#173942,#173943,#173944,#173945,#173946,#173947,#173948,#173949,#173950,
#173951,#173952,#173953,#173954,#173955,#173956,#173957,#173958,#173959,
#173960,#173961,#173962,#173963,#173964,#173965,#173966,#173967,#173968,
#173969,#173970,#173971,#173972,#173973,#173974,#173975,#173976,#173977,
#173978,#173979,#173980,#173981,#173982,#173983,#173984,#173985,#173986,
#173987,#173988,#173989,#173990,#173991,#173992,#173993,#173994,#173995,
#173996,#173997,#173998,#173999,#174000,#174001,#174002,#174003,#174004,
#174005,#174006,#174007,#174008,#174009,#174010,#174011,#174012,#174013,
#174014,#174015,#174016,#174017,#174018,#174019,#174020,#174021,#174022,
#174023,#174024,#174025,#174026,#174027,#174028,#174029,#174030,#174031,
#174032,#174033,#174034,#174035,#174036,#174037,#174038,#174039,#174040,
#174041,#174042,#174043,#174044,#174045,#174046,#174047,#174048,#174049,
#174050,#174051,#174052,#174053,#174054,#174055,#174056,#174057,#174058,
#174059,#174060,#174061,#174062,#174063,#174064,#174065,#174066,#174067,
#174068,#174069,#174070,#174071,#174072,#174073,#174074,#174075,#174076,
#174077,#174078,#174079,#174080,#174081,#174082,#174083,#174084,#174085,
#174086,#174087,#174088,#174089,#174090,#174091,#174092,#174093,#174094,
#174095,#174096,#174097),.UNSPECIFIED.,.F.,.F.,(4,2,2,2,2,2,2,2,2,2,2,2,
2,2,2,2,2,2,2,2,2,2,2,2,2,2,2,2,2,2,2,2,2,2,2,2,2,2,2,2,2,2,2,2,2,2,2,2,
2,2,2,2,2,2,2,2,2,2,2,2,2,2,2,2,2,2,2,2,2,2,2,2,2,2,2,2,2,2,2,2,2,2,2,2,
2,2,2,2,2,2,2,2,2,2,2,2,2,2,2,2,2,2,2,2,2,2,2,2,2,2,2,2,2,2,2,2,2,2,2,2,
2,2,2,2,2,2,2,2,2,2,2,2,2,2,2,2,2,2,4),(1.25968337114772,1.2815038271417,
1.30395449861653,1.31433172173624,1.31654812649059,1.31779241236542,1.31886513648359,
1.3202297307965,1.32240314089473,1.33389984160313,1.38263543117029,1.41583871239245,
1.42010256654869,1.42263485781704,1.42457427825447,1.42665163350888,1.42991794424423,
1.44038100612086,1.45728195988552,1.4951104704737,1.52518584386112,1.52810043536703,
1.52948921209973,1.53056418877032,1.53179230746531,1.53393523378377,1.54323138971984,
1.56207793156719,1.60247840619797,1.61474050023896,1.62934633499325,1.63313461249557,
1.63534960205452,1.63726186138475,1.63959689136195,1.64404681498353,1.6749595661705,
1.72180667657544,1.73760388660089,1.74021636783017,1.74156225191304,1.74263362124364,
1.74389181171071,1.74617192993923,1.75760855126144,1.78402412413786,1.8363876377799,
1.84332608739892,1.84620016798932,1.84799462809362,1.84995523677239,1.85265675350369,
1.85904659407297,1.88738476591629,1.93728374955004,1.94991435750901,1.95215064902386,
1.95353428505236,1.95460879454741,1.95584032166545,1.95799848444546,1.96750662676836,
2.0166416983383,2.05182797042851,2.05612433189675,2.05866609436234,2.06060709991379,
2.06268064986615,2.06592946293961,2.07623868658228,2.09279784143566,2.12568538566885,
2.13955063270457,2.14611512615142,2.16166395047815,2.16426432974732,2.16560755858078,
2.16667870974449,2.16793884888367,2.17022814395277,2.18182963807436,2.20890920763088,
2.26033579694686,2.26733477660799,2.27021876841521,2.27201496933338,2.27397392917665,
2.27666670546291,2.28300563263239,2.31092245379032,2.35691745824166,2.35824204545841,
2.37368848034884,2.37605644184807,2.37746405043135,2.37854422847606,2.37974771597112,
2.38177959680905,2.38967048629553,2.40438732566613,2.44551765277643,2.47594527327307,
2.48016410013322,2.48268325980229,2.4846205585698,2.48469624893075,2.48474205912219,
2.4847863396922,2.48482649075229,2.48486295713526,2.48489612660784,2.4849263384659,
2.48495389225001,2.48497905121499,2.48500204816063,2.48502308959494,2.48504235924239,
2.48506002098396,2.48507622139417,2.48509898188053,2.48512131832721,2.4851432424048,
2.48516476901952,2.48518591096378,2.48520668057027,2.4852270896672,2.48524714957789,
2.48750337741587,2.49161502728447,2.49674798922724,2.50777813094903,2.53230016490609,
2.54786764107018,2.58533209066512,2.58816295458493,2.58953532329599,2.59060866755098,
2.59184744859274,2.59331024535127),.UNSPECIFIED.);
#1823=B_SPLINE_CURVE_WITH_KNOTS('',3,(#174099,#174100,#174101,#174102,#174103,
#174104,#174105,#174106,#174107,#174108,#174109,#174110,#174111,#174112,
#174113,#174114,#174115,#174116,#174117,#174118,#174119,#174120,#174121,
#174122,#174123,#174124,#174125,#174126,#174127,#174128,#174129,#174130,
#174131,#174132,#174133,#174134,#174135,#174136,#174137,#174138,#174139,
#174140,#174141,#174142,#174143,#174144,#174145,#174146,#174147,#174148,
#174149,#174150,#174151,#174152,#174153,#174154,#174155,#174156,#174157,
#174158,#174159,#174160,#174161,#174162,#174163,#174164,#174165,#174166,
#174167,#174168,#174169,#174170,#174171,#174172,#174173,#174174,#174175,
#174176,#174177,#174178,#174179,#174180,#174181,#174182,#174183,#174184,
#174185,#174186,#174187,#174188,#174189,#174190,#174191,#174192,#174193,
#174194,#174195,#174196,#174197,#174198,#174199,#174200,#174201,#174202,
#174203,#174204,#174205,#174206,#174207,#174208,#174209,#174210,#174211,
#174212,#174213,#174214,#174215,#174216,#174217,#174218,#174219,#174220,
#174221,#174222,#174223,#174224,#174225,#174226,#174227,#174228,#174229,
#174230,#174231,#174232,#174233,#174234,#174235,#174236,#174237,#174238,
#174239,#174240,#174241,#174242,#174243,#174244,#174245,#174246,#174247,
#174248,#174249,#174250,#174251,#174252,#174253,#174254,#174255,#174256,
#174257,#174258,#174259,#174260,#174261,#174262,#174263,#174264,#174265,
#174266,#174267,#174268,#174269,#174270,#174271,#174272,#174273,#174274,
#174275,#174276),.UNSPECIFIED.,.F.,.F.,(4,3,3,3,3,3,3,3,3,3,3,3,3,3,3,3,
3,3,3,3,3,3,3,3,3,3,3,3,3,3,3,3,3,3,3,3,3,3,3,3,3,3,3,3,3,3,3,3,3,3,3,3,
3,3,3,3,3,3,3,4),(-54.1065214908593,-53.9371682979412,-53.8337735608932,
-53.7305322787782,-53.6274123133858,-53.5243577451769,-53.4213345368191,
-53.3183086941465,-53.2151759273684,-53.1119868359585,-53.0086148425768,
-52.9383318479794,-52.8349371109315,-52.7316958288166,-52.6285758634243,
-52.5255212952155,-52.4224980868578,-52.3194722441853,-52.2163394774072,
-52.1131503859974,-52.0097783926158,-51.9394953980175,-51.8361006609695,
-51.7328593788545,-51.6297394134622,-51.5266848452533,-51.4236616368955,
-51.320635794223,-51.2175030274449,-51.114313936035,-51.0109419426534,-50.9406589480556,
-50.8372642110077,-50.7340229288926,-50.6309029635004,-50.5278483952914,
-50.4248251869337,-50.3217993442612,-50.2186665774831,-50.1154774860733,
-50.0121054926917,-49.9418224980937,-49.8384277610458,-49.7351864789308,
-49.6320665135385,-49.5290119453296,-49.4259887369719,-49.3229628942994,
-49.2198301275214,-49.1166410361116,-49.01326904273,-48.9429860481318,-48.8396205066959,
-48.7363953136968,-48.6332762150919,-48.5302290794622,-48.4271932051556,
-48.3241646395681,-48.2210652727541,-48.174029021668),.UNSPECIFIED.);
#1824=B_SPLINE_CURVE_WITH_KNOTS('',3,(#174277,#174278,#174279,#174280),
 .UNSPECIFIED.,.F.,.F.,(4,4),(-54.456513037791,-54.1065275196808),
 .UNSPECIFIED.);
#1825=B_SPLINE_CURVE_WITH_KNOTS('',3,(#174286,#174287,#174288,#174289,#174290,
#174291,#174292,#174293,#174294,#174295,#174296,#174297,#174298,#174299,
#174300,#174301,#174302,#174303,#174304,#174305),.UNSPECIFIED.,.F.,.F.,
(4,2,2,2,2,2,2,2,2,4),(2.59308993462329,2.59881536461045,2.60307197546038,
2.6056017133623,2.60754019170769,2.60961752672368,2.61288588653771,2.61668873260866,
2.62395258021943,2.66757550776084),.UNSPECIFIED.);
#1826=B_SPLINE_CURVE_WITH_KNOTS('',3,(#174306,#174307,#174308,#174309,#174310,
#174311,#174312,#174313,#174314,#174315,#174316,#174317,#174318,#174319,
#174320,#174321,#174322,#174323,#174324,#174325,#174326,#174327,#174328,
#174329,#174330,#174331,#174332,#174333,#174334,#174335,#174336,#174337,
#174338,#174339,#174340,#174341,#174342,#174343,#174344,#174345,#174346,
#174347,#174348,#174349,#174350,#174351,#174352,#174353,#174354,#174355,
#174356,#174357,#174358,#174359,#174360,#174361,#174362,#174363,#174364,
#174365,#174366,#174367,#174368,#174369,#174370,#174371,#174372,#174373,
#174374,#174375,#174376,#174377,#174378,#174379,#174380,#174381,#174382,
#174383,#174384,#174385,#174386,#174387,#174388,#174389,#174390,#174391,
#174392,#174393,#174394,#174395,#174396,#174397,#174398,#174399,#174400,
#174401,#174402,#174403,#174404,#174405,#174406,#174407,#174408,#174409,
#174410,#174411,#174412,#174413,#174414,#174415,#174416,#174417,#174418,
#174419,#174420,#174421,#174422,#174423,#174424,#174425,#174426,#174427,
#174428,#174429,#174430,#174431,#174432,#174433,#174434,#174435,#174436,
#174437,#174438,#174439,#174440,#174441,#174442,#174443,#174444,#174445,
#174446,#174447,#174448,#174449,#174450,#174451,#174452,#174453,#174454,
#174455,#174456,#174457,#174458,#174459,#174460,#174461,#174462,#174463,
#174464,#174465,#174466,#174467,#174468,#174469,#174470,#174471,#174472,
#174473,#174474,#174475,#174476,#174477,#174478,#174479,#174480,#174481,
#174482,#174483,#174484,#174485,#174486,#174487,#174488,#174489,#174490,
#174491,#174492,#174493,#174494,#174495,#174496,#174497,#174498,#174499,
#174500,#174501,#174502,#174503,#174504,#174505,#174506,#174507,#174508,
#174509,#174510,#174511,#174512,#174513,#174514,#174515,#174516,#174517,
#174518,#174519),.UNSPECIFIED.,.F.,.F.,(4,2,2,2,2,2,2,2,2,2,2,2,2,2,2,2,
2,2,2,2,2,2,2,2,2,2,2,2,2,2,2,2,2,2,2,2,2,2,2,2,2,2,2,2,2,2,2,2,2,2,2,2,
2,2,2,2,2,2,2,2,2,2,2,2,2,2,2,2,2,2,2,2,2,2,2,2,2,2,2,2,2,2,2,2,2,2,2,2,
2,2,2,2,2,2,2,2,2,2,2,2,2,2,2,2,2,2,4),(0.000649993331013773,0.0375152736453762,
0.0412926066958227,0.0433020341715962,0.044607215832664,0.045844419448192,
0.0469177320618385,0.0482917912985203,0.0511320599888608,0.0879797115895702,
0.109399218190971,0.136182458586284,0.146436099124581,0.149706960391475,
0.151785049252133,0.153723648856619,0.15625271235973,0.160506368957157,
0.193188856063357,0.222561137876658,0.244175532207324,0.254295403786826,
0.25648530331634,0.257733434758561,0.258805438493602,0.260163923762618,
0.262836090595815,0.280220127817376,0.329263705439906,0.347305789337896,
0.354573683519191,0.36000255078723,0.362567762856761,0.364505099941212,
0.366333302380224,0.368881421716173,0.375563408649001,0.430966318990965,
0.45531833772441,0.466218362236338,0.468466827385657,0.469717966669812,
0.470789714733089,0.472144237015971,0.474885954457074,0.493328404523347,
0.537460304227698,0.56533181314619,0.571665318741461,0.574356955714583,
0.57631551717809,0.578111655021596,0.580996197394739,0.587999833063062,
0.639384728107681,0.6665155305315,0.678128415364886,0.680418166758709,0.681678306830284,
0.682749311508137,0.684092164238236,0.686691256343921,0.702216945856713,
0.708760927231134,0.722633874188153,0.755493937891593,0.772056441017398,
0.782367865525588,0.785616669809531,0.787690051800405,0.789630786629262,
0.792172032044759,0.796467187329842,0.831578300272903,0.880465436321519,
0.89028861056827,0.892468467938671,0.893704699529089,0.894778400789985,
0.896154565678567,0.899004695521442,0.935374552606732,0.989163011369373,
0.995619065943052,0.998331634006407,1.00029412823005,1.0020861016653,1.00494702788069,
1.01180630602425,1.06524491368085,1.09093515786658,1.10218655441291,1.10445597198694,
1.10571178057254,1.10678326518238,1.10813201829251,1.11075808370708,1.12692227782077,
1.1775802709192,1.20199423988746,1.20789425851965,1.21051032259266,1.21245602088232,
1.21427041747359,1.21676502677054,1.2231148737998,1.25968337114772),
 .UNSPECIFIED.);
#1827=B_SPLINE_CURVE_WITH_KNOTS('',3,(#174521,#174522,#174523,#174524,#174525,
#174526,#174527,#174528,#174529,#174530),.UNSPECIFIED.,.F.,.F.,(4,1,1,1,
1,1,1,4),(-60.3897037700498,-59.9301869977125,-58.9313505477506,-57.9325140977887,
-56.9336776478269,-55.934841197865,-54.9360047479031,-54.456513037791),
 .UNSPECIFIED.);
#1828=B_SPLINE_CURVE_WITH_KNOTS('',3,(#174531,#174532,#174533,#174534,#174535,
#174536,#174537,#174538,#174539,#174540,#174541,#174542,#174543,#174544,
#174545,#174546,#174547,#174548),.UNSPECIFIED.,.F.,.F.,(4,2,2,2,2,2,2,2,
4),(0.000658789710875621,0.0033297019558972,0.00592165925672697,0.00778879716285326,
0.00964368964991593,0.0114909186466428,0.0146445374956457,0.0233614961612485,
0.0750732887615297),.UNSPECIFIED.);
#1829=B_SPLINE_CURVE_WITH_KNOTS('',3,(#174553,#174554,#174555,#174556,#174557,
#174558,#174559,#174560,#174561,#174562,#174563,#174564,#174565,#174566,
#174567,#174568,#174569,#174570,#174571,#174572,#174573,#174574,#174575,
#174576,#174577,#174578,#174579,#174580,#174581,#174582,#174583,#174584,
#174585,#174586,#174587,#174588,#174589,#174590,#174591,#174592,#174593,
#174594,#174595,#174596,#174597,#174598,#174599,#174600,#174601,#174602,
#174603,#174604,#174605,#174606,#174607,#174608,#174609,#174610,#174611,
#174612,#174613,#174614,#174615,#174616,#174617,#174618,#174619,#174620,
#174621,#174622,#174623,#174624,#174625,#174626,#174627,#174628,#174629,
#174630,#174631,#174632,#174633,#174634,#174635,#174636,#174637,#174638,
#174639,#174640,#174641,#174642,#174643,#174644,#174645,#174646,#174647,
#174648,#174649,#174650,#174651,#174652,#174653,#174654,#174655,#174656,
#174657,#174658,#174659,#174660,#174661,#174662,#174663,#174664,#174665,
#174666,#174667,#174668,#174669,#174670,#174671,#174672,#174673,#174674,
#174675,#174676,#174677,#174678,#174679,#174680,#174681,#174682,#174683,
#174684,#174685,#174686,#174687,#174688,#174689,#174690,#174691,#174692,
#174693,#174694,#174695,#174696,#174697,#174698,#174699,#174700,#174701,
#174702,#174703,#174704,#174705,#174706,#174707,#174708,#174709,#174710,
#174711,#174712,#174713,#174714,#174715,#174716,#174717,#174718,#174719,
#174720,#174721,#174722,#174723,#174724,#174725,#174726,#174727,#174728,
#174729,#174730,#174731,#174732,#174733,#174734,#174735,#174736,#174737,
#174738,#174739,#174740,#174741,#174742,#174743,#174744,#174745,#174746,
#174747,#174748,#174749,#174750,#174751,#174752,#174753,#174754,#174755,
#174756,#174757,#174758,#174759,#174760,#174761,#174762,#174763,#174764,
#174765,#174766,#174767,#174768,#174769,#174770,#174771,#174772,#174773,
#174774),.UNSPECIFIED.,.F.,.F.,(4,2,2,2,2,2,2,2,2,2,2,2,2,2,2,2,2,2,2,2,
2,2,2,2,2,2,2,2,2,2,2,2,2,2,2,2,2,2,2,2,2,2,2,2,2,2,2,2,2,2,2,2,2,2,2,2,
2,2,2,2,2,2,2,2,2,2,2,2,2,2,2,2,2,2,2,2,2,2,2,2,2,2,2,2,2,2,2,2,2,2,2,2,
2,2,2,2,2,2,2,2,2,2,2,2,2,2,2,2,2,2,4),(1.2598188162962,1.28582910675168,
1.32659483739134,1.33166075036229,1.33412021359612,1.3360430637854,1.33817454540318,
1.34168704094204,1.35456214699032,1.3772629349575,1.41585039442087,1.42084455493994,
1.43685065379829,1.43946985762439,1.44081696261975,1.44188812356032,1.44314470097155,
1.44541841322834,1.45675099277767,1.48276037789335,1.53567697460108,1.54257189724511,
1.54543830941899,1.54723100415685,1.5491921112309,1.55189875997267,1.55832172771228,
1.58694418749935,1.63822339094734,1.64928405207265,1.65143088219273,1.65278721060316,
1.65385904268073,1.6551087399456,1.65735075673663,1.66814586155088,1.69210600879927,
1.74805395327426,1.75467916201693,1.757218341053,1.75904412504075,1.76098257635116,
1.76355551061247,1.76921953544927,1.79185998894947,1.82467505848605,1.82892885538883,
1.86039079648171,1.86330220822099,1.8646901279052,1.86576474414343,1.86699278994439,
1.86913638286826,1.87844769522067,1.92759244244472,1.96295371463675,1.96725087208344,
1.9697924031215,1.97173282764153,1.97380536503933,1.97705177386893,1.98734648215883,
2.00387577778063,2.03673167692832,2.04840959727023,2.05699946981549,2.0727344762376,
2.07534606040473,2.0766914290874,2.07776236004584,2.07902000308596,2.08129904606364,
2.09272854401299,2.11912362483884,2.1714800090376,2.17841409126171,2.18128674014139,
2.18308041658102,2.18504025736265,2.18774087743751,2.19412935638219,2.23964987147934,
2.28171599859575,2.28636347950216,2.28809332059615,2.28911643491209,2.29020986610841,
2.29172761090144,2.29535521465203,2.30046057235922,2.31460692435585,2.36435596823844,
2.37360623771747,2.38839293755108,2.39219622620605,2.39441418037008,2.39632549683361,
2.39865498519619,2.40308089724313,2.42536046955279,2.46852771658149,2.4962144512301,
2.49912046666446,2.50050729541288,2.5015817501905,2.50281037630488,2.50410337152851,
2.50876349509607,2.53287928142517,2.55377715173552,2.59308993462329),
 .UNSPECIFIED.);
#1830=B_SPLINE_CURVE_WITH_KNOTS('',3,(#174775,#174776,#174777,#174778,#174779,
#174780,#174781,#174782,#174783,#174784,#174785,#174786,#174787,#174788,
#174789,#174790,#174791,#174792,#174793,#174794,#174795,#174796,#174797,
#174798,#174799,#174800,#174801,#174802,#174803,#174804,#174805,#174806,
#174807,#174808,#174809,#174810,#174811,#174812,#174813,#174814,#174815,
#174816,#174817,#174818,#174819,#174820,#174821,#174822,#174823,#174824,
#174825,#174826,#174827,#174828,#174829,#174830,#174831,#174832,#174833,
#174834,#174835,#174836,#174837,#174838,#174839,#174840,#174841,#174842,
#174843,#174844,#174845,#174846,#174847,#174848,#174849,#174850,#174851,
#174852,#174853,#174854,#174855,#174856,#174857,#174858,#174859,#174860,
#174861,#174862,#174863,#174864,#174865,#174866,#174867,#174868,#174869,
#174870,#174871,#174872,#174873,#174874,#174875,#174876,#174877,#174878,
#174879,#174880,#174881,#174882,#174883,#174884,#174885,#174886,#174887,
#174888,#174889,#174890,#174891,#174892,#174893,#174894,#174895,#174896,
#174897,#174898,#174899,#174900,#174901,#174902,#174903,#174904,#174905,
#174906,#174907,#174908,#174909,#174910,#174911,#174912,#174913,#174914,
#174915,#174916,#174917,#174918,#174919,#174920,#174921,#174922,#174923,
#174924,#174925,#174926,#174927,#174928,#174929,#174930,#174931,#174932,
#174933,#174934,#174935,#174936,#174937,#174938,#174939,#174940,#174941,
#174942,#174943,#174944,#174945,#174946,#174947,#174948,#174949,#174950,
#174951,#174952,#174953,#174954,#174955,#174956,#174957,#174958,#174959,
#174960,#174961,#174962,#174963,#174964,#174965,#174966,#174967,#174968,
#174969,#174970,#174971,#174972,#174973,#174974,#174975,#174976,#174977,
#174978,#174979,#174980,#174981,#174982,#174983,#174984,#174985,#174986,
#174987,#174988,#174989,#174990,#174991,#174992,#174993,#174994,#174995,
#174996,#174997,#174998,#174999,#175000,#175001,#175002,#175003,#175004,
#175005,#175006),.UNSPECIFIED.,.F.,.F.,(4,2,2,2,2,2,2,2,2,2,2,2,2,2,2,2,
2,2,2,2,2,2,2,2,2,2,2,2,2,2,2,2,2,2,2,2,2,2,2,2,2,2,2,2,2,2,2,2,2,2,2,2,
2,2,2,2,2,2,2,2,2,2,2,2,2,2,2,2,2,2,2,2,2,2,2,2,2,2,2,2,2,2,2,2,2,2,2,2,
2,2,2,2,2,2,2,2,2,2,2,2,2,2,2,2,2,2,2,2,2,2,2,2,2,2,2,4),(0.0750732887615297,
0.0895786872185756,0.108776673444175,0.112687667588427,0.114252339386623,
0.115354626383585,0.116366707255712,0.118038562888942,0.122314119578349,
0.178030895777346,0.209836521089513,0.214455835189256,0.21722182163431,
0.219725106281578,0.221625903726026,0.223450329915231,0.225983634845776,
0.232570915468512,0.288908008162023,0.312655305002868,0.323392618135194,
0.325631403689644,0.326880523911942,0.327952621545743,0.329310255392404,
0.331977827467359,0.349225793650038,0.365434006915295,0.40026058837796,
0.423361560096201,0.42908852568208,0.431673378061521,0.433614092718227,
0.435437105598377,0.437964605124127,0.444513982543606,0.501229072546634,
0.524735771556337,0.535407711707381,0.537642637038817,0.538890990233706,
0.539963288418181,0.541322280536716,0.543995847386938,0.561403803782938,
0.611255794604785,0.635241862161705,0.641086203964012,0.643692398004577,
0.645636600712106,0.647453819283593,0.649958945237493,0.656371159543673,
0.714276531250413,0.73703090948458,0.747494158372973,0.749716141419215,
0.750961706070528,0.752034375427397,0.753397406368537,0.756089736758378,
0.774034475163358,0.822088316566691,0.840408384767806,0.851497265122604,
0.854832750834517,0.856925471406221,0.85885961686657,0.861357330377948,
0.865502438252775,0.893394867270794,0.947161446532259,0.959371234235877,
0.961693681471469,0.962961127490909,0.964031989213525,0.965366667202426,
0.967441902861164,0.977393962372905,0.983033419115146,0.992434620947976,
1.00400487314063,1.03685416617455,1.05339653638974,1.06369972440442,1.06694822242758,
1.06902195931009,1.07096341303229,1.07350615789104,1.07780509881571,1.11311795905019,
1.16237601762062,1.17171435900122,1.17386077287483,1.17508987724573,1.17616506193869,
1.17755323318852,1.18046348893946,1.20859690640356,1.2482888946344,1.26523562654097,
1.27572113131065,1.27899060545621,1.28106906901157,1.28300889420011,1.28554081197511,
1.28980206145261,1.33480531537179,1.37985976923109,1.3845853353168,1.38632777019847,
1.3873538428049,1.38844662397774,1.38995724915956,1.393539137418,1.40896669254699),
 .UNSPECIFIED.);
#1831=B_SPLINE_CURVE_WITH_KNOTS('',3,(#175012,#175013,#175014,#175015,#175016),
 .UNSPECIFIED.,.F.,.F.,(4,1,4),(76.7075601022117,76.9104066470643,77.0584303716429),
 .UNSPECIFIED.);
#1832=B_SPLINE_CURVE_WITH_KNOTS('',3,(#175017,#175018,#175019,#175020,#175021,
#175022,#175023,#175024,#175025,#175026,#175027,#175028,#175029,#175030,
#175031,#175032,#175033,#175034,#175035,#175036,#175037,#175038,#175039,
#175040,#175041,#175042,#175043,#175044,#175045,#175046,#175047,#175048,
#175049,#175050,#175051,#175052,#175053,#175054,#175055,#175056,#175057,
#175058,#175059,#175060,#175061,#175062,#175063,#175064,#175065,#175066,
#175067,#175068,#175069,#175070,#175071,#175072,#175073,#175074,#175075,
#175076,#175077,#175078,#175079,#175080,#175081,#175082,#175083,#175084,
#175085,#175086,#175087,#175088,#175089,#175090,#175091,#175092,#175093,
#175094,#175095,#175096,#175097,#175098,#175099,#175100,#175101,#175102,
#175103,#175104,#175105,#175106,#175107,#175108,#175109,#175110,#175111,
#175112,#175113,#175114,#175115,#175116,#175117,#175118,#175119,#175120,
#175121,#175122,#175123,#175124,#175125,#175126,#175127,#175128,#175129,
#175130,#175131,#175132,#175133,#175134,#175135,#175136,#175137,#175138,
#175139,#175140,#175141,#175142,#175143,#175144,#175145,#175146,#175147,
#175148,#175149,#175150,#175151,#175152,#175153,#175154,#175155,#175156,
#175157,#175158,#175159,#175160,#175161,#175162,#175163,#175164,#175165,
#175166,#175167,#175168,#175169,#175170,#175171,#175172,#175173,#175174,
#175175,#175176,#175177,#175178,#175179,#175180,#175181,#175182,#175183,
#175184,#175185,#175186,#175187,#175188,#175189,#175190,#175191,#175192,
#175193,#175194,#175195,#175196,#175197,#175198,#175199,#175200,#175201,
#175202,#175203,#175204,#175205,#175206,#175207,#175208,#175209,#175210,
#175211,#175212,#175213,#175214,#175215,#175216,#175217,#175218,#175219,
#175220,#175221,#175222,#175223,#175224,#175225,#175226,#175227,#175228,
#175229,#175230,#175231,#175232,#175233,#175234,#175235,#175236,#175237,
#175238),.UNSPECIFIED.,.F.,.F.,(4,2,2,2,2,2,2,2,2,2,2,2,2,2,2,2,2,2,2,2,
2,2,2,2,2,2,2,2,2,2,2,2,2,2,2,2,2,2,2,2,2,2,2,2,2,2,2,2,2,2,2,2,2,2,2,2,
2,2,2,2,2,2,2,2,2,2,2,2,2,2,2,2,2,2,2,2,2,2,2,2,2,2,2,2,2,2,2,2,2,2,2,2,
2,2,2,2,2,2,2,2,2,2,2,2,2,2,2,2,2,2,4),(0.00062922477804048,0.0464652953959511,
0.0539874627083681,0.0578868262224725,0.0612218917618552,0.0633140104223921,
0.0652473689506565,0.0677437427811126,0.0718859251347045,0.0997158380709969,
0.113763875467969,0.12930975099674,0.154610309606332,0.165743607840038,
0.168012355284411,0.16926952399704,0.170340543990751,0.171686645238151,
0.174301472994702,0.190228702005755,0.195859651481846,0.25279017795695,
0.268941263732326,0.272736315114818,0.274930060881375,0.276843183245678,
0.279203796669903,0.282810236411761,0.299521474717382,0.307016312503351,
0.35552052635381,0.370248070400744,0.378141297512718,0.380172947110739,
0.381376133496349,0.382455933488197,0.383862893393866,0.386229424307423,
0.40165571259872,0.405922318104049,0.448896606019998,0.47682861694909,0.483168954246668,
0.485861489510229,0.487819967755852,0.489615518845367,0.492497998416956,
0.499490908048754,0.551011590897581,0.578035038566169,0.58962067389478,
0.591908636141562,0.59316826235519,0.594239113763674,0.595582133715924,
0.598182596225254,0.613747895324114,0.620206829222099,0.661617384913786,
0.68888713635835,0.695146982192309,0.697825810435743,0.699781913499077,
0.70158057463847,0.704479716433519,0.711572252189626,0.761225744758292,
0.799536004107826,0.803140089386526,0.804653944556405,0.805746779238389,
0.806771088843483,0.808506669136336,0.81319120071484,0.854270650314107,
0.90069679167419,0.907088247212731,0.909789580758431,0.911749742973229,
0.913543582016164,0.916416192282476,0.923348618781982,0.975791660662828,
1.00216367739533,1.01358740277245,1.01586636896956,1.01712409769934,1.01819518257729,
1.01954084145329,1.02215327420812,1.03800352486472,1.04274687359478,1.05802403925964,
1.09089716689076,1.10747761982684,1.1177968934593,1.12104640234922,1.12311980943024,
1.12506026959418,1.12760072530062,1.13189358223016,1.17429083615549,1.20334618781477,
1.22296071006421,1.22691560694454,1.22848716391289,1.22959066388589,1.23060105632183,
1.23226455229217,1.23648935279628,1.2598188162962),.UNSPECIFIED.);
#1833=B_SPLINE_CURVE_WITH_KNOTS('',3,(#175240,#175241,#175242,#175243,#175244,
#175245,#175246,#175247,#175248,#175249,#175250,#175251,#175252,#175253,
#175254,#175255,#175256,#175257,#175258,#175259,#175260,#175261,#175262,
#175263,#175264,#175265,#175266,#175267,#175268,#175269,#175270,#175271,
#175272,#175273,#175274,#175275,#175276,#175277,#175278,#175279,#175280,
#175281,#175282,#175283,#175284,#175285,#175286,#175287,#175288,#175289,
#175290,#175291,#175292,#175293,#175294,#175295,#175296,#175297,#175298,
#175299,#175300,#175301,#175302,#175303,#175304,#175305,#175306,#175307,
#175308,#175309,#175310,#175311,#175312,#175313,#175314,#175315,#175316,
#175317,#175318,#175319,#175320,#175321,#175322,#175323,#175324,#175325,
#175326,#175327,#175328,#175329,#175330,#175331,#175332,#175333,#175334,
#175335,#175336,#175337,#175338,#175339,#175340,#175341,#175342,#175343,
#175344,#175345,#175346,#175347,#175348,#175349,#175350,#175351,#175352,
#175353,#175354,#175355,#175356,#175357,#175358,#175359,#175360,#175361,
#175362,#175363,#175364,#175365,#175366,#175367,#175368,#175369,#175370,
#175371,#175372,#175373,#175374,#175375,#175376,#175377,#175378,#175379,
#175380,#175381,#175382,#175383,#175384,#175385,#175386,#175387,#175388,
#175389,#175390,#175391,#175392,#175393,#175394,#175395,#175396,#175397,
#175398,#175399,#175400,#175401,#175402,#175403,#175404,#175405,#175406,
#175407,#175408,#175409,#175410,#175411,#175412,#175413,#175414,#175415,
#175416,#175417,#175418,#175419,#175420,#175421,#175422,#175423,#175424,
#175425,#175426,#175427,#175428,#175429,#175430,#175431,#175432,#175433,
#175434,#175435,#175436,#175437,#175438,#175439,#175440,#175441,#175442,
#175443,#175444,#175445,#175446,#175447,#175448,#175449,#175450,#175451,
#175452,#175453,#175454,#175455,#175456,#175457,#175458,#175459,#175460,
#175461,#175462,#175463),.UNSPECIFIED.,.F.,.F.,(4,2,2,2,2,2,2,2,2,2,2,2,
2,2,2,2,2,2,2,2,2,2,2,2,2,2,2,2,2,2,2,2,2,2,2,2,2,2,2,2,2,2,2,2,2,2,2,2,
2,2,2,2,2,2,2,2,2,2,2,2,2,2,2,2,2,2,2,2,2,2,2,2,2,2,2,2,2,2,2,2,2,2,2,2,
2,2,2,2,2,2,2,2,2,2,2,2,2,2,2,2,2,2,2,2,2,2,2,2,2,2,2,4),(1.40896669254699,
1.43117951109762,1.48160626610979,1.48866533053147,1.49155996689647,1.49335859904134,
1.49531687243928,1.49800265062375,1.50429705257051,1.53183798945899,1.56024380039991,
1.58257536586916,1.59528320803545,1.59752392806156,1.59890907121816,1.59998396177195,
1.60121503985215,1.60337032463693,1.61283263139795,1.66202152608611,1.69722883918779,
1.70152641174088,1.70406884250338,1.70601033064397,1.7080843692321,1.7113338917161,
1.72164489299814,1.73820645258912,1.77110067801436,1.78483636905165,1.79171010539514,
1.79192676507287,1.79545007095206,1.80740666043681,1.80960671783378,1.81097953665053,
1.81205317446822,1.81329222802112,1.81548402248912,1.8254790104123,1.87421219717204,
1.90927148237337,1.91356683841726,1.91610853538612,1.9180497958077,1.92012391368317,
1.92337423396291,1.93369344624765,1.95027360004668,1.98318193416041,1.99836891046661,
2.00321053728236,2.01910159076681,2.02171603681438,2.02306243915953,2.02413396056373,
2.02539202732717,2.02767115058287,2.03908677452003,2.06541657067306,2.11791275224925,
2.12484308668044,2.12771603955699,2.12951044785643,2.13147152279433,2.13417463793488,
2.14057275843119,2.18836823029259,2.22807348290449,2.23281799553136,2.23456311481422,
2.23558958703295,2.23668179567086,2.23819000446309,2.24175873064458,2.2794736160787,
2.3298223184813,2.33688357635813,2.33977825869028,2.34157666324293,2.343534485416,
2.34621927628665,2.35250966335699,2.38002215823233,2.42191963479165,2.44297304607341,
2.44578939258029,2.44715905382501,2.44819622862635,2.44939626614753,2.45067690309327,
2.4526266300887,2.45624584904207,2.46485966520697,2.49773269375569,2.54162822662122,
2.54885151925285,2.55177335728039,2.55357676114043,2.55553068334886,2.55819334626703,
2.56435560956493,2.59082877988912,2.6483497821524,2.65622246182487,2.65831873378907,
2.65954887037209,2.66060581764147,2.66165184919058,2.66300245522682,2.66546082872914,
2.66855489445154),.UNSPECIFIED.);
#1834=B_SPLINE_CURVE_WITH_KNOTS('',3,(#175464,#175465,#175466,#175467,#175468,
#175469),.UNSPECIFIED.,.F.,.F.,(4,2,4),(0.000817337805837695,0.0612255019915846,
0.0752219354471869),.UNSPECIFIED.);
#1835=B_SPLINE_CURVE_WITH_KNOTS('',3,(#175475,#175476,#175477,#175478,#175479,
#175480,#175481,#175482,#175483,#175484,#175485,#175486,#175487),
 .UNSPECIFIED.,.F.,.F.,(4,3,3,3,4),(82.9907456874198,83.0928761471997,83.1948834239681,
83.2967928188084,83.3413404231495),.UNSPECIFIED.);
#1836=B_SPLINE_CURVE_WITH_KNOTS('',3,(#175488,#175489,#175490,#175491,#175492,
#175493,#175494,#175495,#175496,#175497),.UNSPECIFIED.,.F.,.F.,(4,1,1,1,
1,1,1,4),(77.0584303716429,77.9092430970262,78.9080795469881,79.90691599695,
80.9057524469118,81.9045888968737,82.9034253468356,82.9907454093913),
 .UNSPECIFIED.);
#1837=B_SPLINE_CURVE_WITH_KNOTS('',3,(#175498,#175499,#175500,#175501,#175502,
#175503,#175504,#175505,#175506,#175507,#175508,#175509,#175510,#175511,
#175512,#175513,#175514,#175515,#175516,#175517,#175518,#175519,#175520,
#175521,#175522,#175523,#175524,#175525,#175526,#175527,#175528,#175529,
#175530,#175531,#175532,#175533,#175534,#175535,#175536,#175537,#175538,
#175539,#175540,#175541,#175542,#175543,#175544,#175545,#175546,#175547,
#175548,#175549,#175550,#175551,#175552,#175553,#175554,#175555,#175556,
#175557,#175558,#175559,#175560,#175561,#175562,#175563,#175564,#175565,
#175566,#175567,#175568,#175569,#175570,#175571,#175572,#175573,#175574,
#175575,#175576,#175577,#175578,#175579,#175580,#175581,#175582,#175583,
#175584,#175585,#175586,#175587,#175588,#175589,#175590,#175591,#175592,
#175593,#175594,#175595,#175596,#175597,#175598,#175599,#175600,#175601,
#175602,#175603,#175604,#175605,#175606,#175607,#175608,#175609,#175610,
#175611,#175612,#175613,#175614,#175615,#175616,#175617,#175618,#175619,
#175620,#175621,#175622,#175623,#175624,#175625,#175626,#175627,#175628,
#175629,#175630,#175631,#175632,#175633,#175634,#175635,#175636,#175637,
#175638,#175639,#175640,#175641,#175642,#175643,#175644,#175645,#175646,
#175647,#175648,#175649,#175650,#175651,#175652,#175653,#175654,#175655,
#175656,#175657,#175658,#175659,#175660,#175661,#175662,#175663,#175664,
#175665,#175666,#175667,#175668,#175669,#175670,#175671,#175672,#175673,
#175674,#175675,#175676,#175677,#175678,#175679,#175680,#175681,#175682,
#175683,#175684,#175685,#175686,#175687,#175688,#175689,#175690,#175691,
#175692,#175693,#175694,#175695,#175696,#175697,#175698,#175699,#175700,
#175701,#175702,#175703,#175704,#175705,#175706,#175707,#175708,#175709,
#175710,#175711,#175712,#175713,#175714,#175715,#175716,#175717,#175718,
#175719,#175720,#175721,#175722,#175723,#175724,#175725,#175726,#175727,
#175728,#175729,#175730,#175731,#175732,#175733,#175734,#175735,#175736,
#175737,#175738,#175739,#175740,#175741,#175742,#175743,#175744,#175745,
#175746,#175747,#175748,#175749,#175750,#175751,#175752,#175753,#175754,
#175755,#175756,#175757,#175758,#175759,#175760,#175761,#175762,#175763,
#175764,#175765,#175766,#175767,#175768,#175769),.UNSPECIFIED.,.F.,.F.,
(4,2,2,2,2,2,2,2,2,2,2,2,2,2,2,2,2,2,2,2,2,2,2,2,2,2,2,2,2,2,2,2,2,2,2,
2,2,2,2,2,2,2,2,2,2,2,2,2,2,2,2,2,2,2,2,2,2,2,2,2,2,2,2,2,2,2,2,2,2,2,2,
2,2,2,2,2,2,2,2,2,2,2,2,2,2,2,2,2,2,2,2,2,2,2,2,2,2,2,2,2,2,2,2,2,2,2,2,
2,2,2,2,2,2,2,2,2,2,2,2,2,2,2,2,2,2,2,2,2,2,2,2,2,2,2,2,4),(0.0752219354471869,
0.0876737803832443,0.0938318759611345,0.096492981468071,0.0984458548715177,
0.100248360755656,0.103168888387438,0.110389690462612,0.15424713468251,
0.195394582587352,0.199212958657244,0.201237805204114,0.202549338024773,
0.203772973796596,0.20377654050265,0.203780119950459,0.203783712088444,
0.203787549478355,0.203791448764298,0.203795411146991,0.203799437954619,
0.203803530609202,0.203807690589143,0.203811919370073,0.20381621842432,
0.203820589227681,0.203825033406919,0.203829552627674,0.203834148630411,
0.203838823136086,0.203843577879537,0.203848414698621,0.2048921653215,0.206274877504582,
0.209159635945463,0.243336900398366,0.277589533678257,0.294133556780751,
0.304436070586588,0.307683448565633,0.309756252284464,0.311696679080571,
0.314237857731063,0.318533654699075,0.353751370195098,0.402995139423211,
0.412389257103734,0.414538925950045,0.415768366383412,0.416842851758761,
0.41822881172915,0.421129832178343,0.453737204220591,0.489082677107781,
0.512192572655288,0.517920263062228,0.520504973984694,0.522445393980685,
0.524267992549417,0.526794698530033,0.533340773146543,0.590075625735493,
0.613557703932693,0.624222135448335,0.626456317732056,0.627704373743318,
0.628776489699957,0.63013534480763,0.632808925340623,0.650227404118175,
0.698915143009477,0.717170928764429,0.728231285602008,0.731563210335695,
0.733654829485937,0.735588730006404,0.738087212264651,0.742235953847532,
0.770296111813773,0.823884046818624,0.836075479382837,0.838396573882568,
0.839663549231086,0.840734171725199,0.842068750797324,0.844144192816116,
0.854103858557716,0.859578958206535,0.86002731298575,0.86691547220709,0.880641619226851,
0.913502670778416,0.930064599266058,0.940375979427016,0.943624936420555,
0.945698455912095,0.947639347568836,0.950180838914409,0.95447650080002,
0.989603716312452,1.03853525985647,1.04831086776148,1.05048759969225,1.05172320234754,
1.05279708883849,1.05417444696276,1.05703033255149,1.07981224668153,1.09265615970665,
1.12551214073723,1.14206550455317,1.15237330951317,1.15562207539461,1.15769569773731,
1.15963684361155,1.16217889575568,1.16647601642632,1.20168366033932,1.25086614322686,
1.26035552064793,1.26251251995824,1.26374386128169,1.26481852327256,1.2662027589569,
1.26909333890624,1.29479692775303,1.33424453012331,1.36196857526904,1.36610927293393,
1.36860580503195,1.37053989936434,1.37263342460125,1.37597205063585,1.3870884923977,
1.4054744587401,1.40869684638067),.UNSPECIFIED.);
#1838=B_SPLINE_CURVE_WITH_KNOTS('',3,(#175775,#175776,#175777,#175778,#175779,
#175780,#175781,#175782,#175783,#175784,#175785,#175786,#175787,#175788,
#175789,#175790,#175791,#175792,#175793,#175794,#175795,#175796,#175797,
#175798,#175799,#175800),.UNSPECIFIED.,.F.,.F.,(4,2,2,2,2,2,2,2,2,2,2,2,
4),(2.59377040355344,2.61306920303431,2.62518493005823,2.62701213587885,
2.62801357239381,2.63670095557141,2.63985192811609,2.64169888631868,2.64355375008281,
2.64542171035433,2.64782304230046,2.65156277527943,2.66819514587953),
 .UNSPECIFIED.);
#1839=B_SPLINE_CURVE_WITH_KNOTS('',3,(#175801,#175802,#175803,#175804,#175805,
#175806,#175807,#175808,#175809,#175810,#175811,#175812,#175813,#175814,
#175815,#175816,#175817,#175818,#175819,#175820,#175821,#175822,#175823,
#175824,#175825,#175826,#175827,#175828,#175829,#175830,#175831,#175832,
#175833,#175834,#175835,#175836,#175837,#175838,#175839,#175840,#175841,
#175842,#175843,#175844,#175845,#175846,#175847,#175848,#175849,#175850,
#175851,#175852,#175853,#175854,#175855,#175856,#175857,#175858,#175859,
#175860,#175861,#175862,#175863,#175864,#175865,#175866,#175867,#175868,
#175869,#175870,#175871,#175872,#175873,#175874,#175875,#175876,#175877,
#175878,#175879,#175880,#175881,#175882,#175883,#175884,#175885,#175886,
#175887,#175888,#175889,#175890,#175891,#175892,#175893,#175894,#175895,
#175896,#175897,#175898,#175899,#175900,#175901,#175902,#175903,#175904,
#175905,#175906,#175907,#175908,#175909,#175910,#175911,#175912,#175913,
#175914,#175915,#175916,#175917,#175918,#175919,#175920,#175921,#175922,
#175923,#175924,#175925,#175926,#175927,#175928,#175929,#175930,#175931,
#175932,#175933,#175934,#175935,#175936,#175937,#175938,#175939,#175940,
#175941,#175942,#175943,#175944,#175945,#175946,#175947,#175948,#175949,
#175950,#175951,#175952,#175953,#175954,#175955,#175956,#175957,#175958,
#175959,#175960,#175961,#175962,#175963,#175964,#175965,#175966,#175967,
#175968,#175969,#175970,#175971,#175972,#175973,#175974,#175975,#175976,
#175977,#175978,#175979,#175980,#175981),.UNSPECIFIED.,.F.,.F.,(4,3,3,3,
3,3,3,3,3,3,3,3,3,3,3,3,3,3,3,3,3,3,3,3,3,3,3,3,3,3,3,3,3,3,3,3,3,3,3,3,
3,3,3,3,3,3,3,3,3,3,3,3,3,3,3,3,3,3,3,3,4),(83.3413404231495,83.4431911085275,
83.5450419932945,83.646994864468,83.7490046560777,83.8511878009641,83.9022617967974,
84.0056565338454,84.1088978159605,84.2120177813528,84.3150723495617,84.4180955579193,
84.5211214005918,84.6242541673699,84.7274432587796,84.8308152521613,84.9010982467593,
85.0044929838073,85.1077342659222,85.2108542313146,85.3139087995235,85.4169320078813,
85.5199578505539,85.623090617332,85.7262797087419,85.8296517021236,85.8999346967212,
86.0033294337692,86.1065707158841,86.2096906812764,86.3127452494854,86.4157684578432,
86.5187943005158,86.6219270672939,86.7251161587037,86.8284881520853,86.8987711466831,
87.0021658837311,87.105407165846,87.2085271312384,87.3115816994473,87.4146049078052,
87.517630750478,87.620763517256,87.7239526086658,87.8273246020474,87.897607596645,
88.0010023336928,88.1042436158078,88.2073635812001,88.3104181494088,88.4134413577666,
88.5164672004389,88.6195999672169,88.7227890586268,88.8261610520084,88.8964440466068,
89.0132269961626,89.1295586830744,89.2451399878363,89.2739307161836),
 .UNSPECIFIED.);
#1840=B_SPLINE_CURVE_WITH_KNOTS('',3,(#175983,#175984,#175985,#175986,#175987,
#175988,#175989,#175990,#175991,#175992,#175993,#175994,#175995,#175996,
#175997,#175998,#175999,#176000,#176001,#176002,#176003,#176004,#176005,
#176006,#176007,#176008,#176009,#176010,#176011,#176012,#176013,#176014,
#176015,#176016,#176017,#176018,#176019,#176020,#176021,#176022,#176023,
#176024,#176025,#176026,#176027,#176028,#176029,#176030,#176031,#176032,
#176033,#176034,#176035,#176036,#176037,#176038,#176039,#176040,#176041,
#176042,#176043,#176044,#176045,#176046,#176047,#176048,#176049,#176050,
#176051,#176052,#176053,#176054,#176055,#176056,#176057,#176058,#176059,
#176060,#176061,#176062,#176063,#176064,#176065,#176066,#176067,#176068,
#176069,#176070,#176071,#176072,#176073,#176074,#176075,#176076,#176077,
#176078,#176079,#176080,#176081,#176082,#176083,#176084,#176085,#176086,
#176087,#176088,#176089,#176090,#176091,#176092,#176093,#176094,#176095,
#176096,#176097,#176098,#176099,#176100,#176101,#176102,#176103,#176104,
#176105,#176106,#176107,#176108,#176109,#176110,#176111,#176112,#176113,
#176114,#176115,#176116,#176117,#176118,#176119,#176120,#176121,#176122,
#176123,#176124,#176125,#176126,#176127,#176128,#176129,#176130,#176131,
#176132,#176133,#176134,#176135,#176136,#176137,#176138,#176139,#176140,
#176141,#176142,#176143,#176144,#176145,#176146,#176147,#176148,#176149,
#176150,#176151,#176152,#176153,#176154,#176155,#176156,#176157,#176158,
#176159,#176160,#176161,#176162,#176163,#176164,#176165,#176166,#176167,
#176168,#176169,#176170,#176171,#176172,#176173,#176174,#176175,#176176,
#176177,#176178,#176179,#176180,#176181,#176182,#176183,#176184,#176185,
#176186,#176187,#176188,#176189,#176190,#176191,#176192,#176193,#176194,
#176195,#176196,#176197,#176198,#176199,#176200,#176201,#176202,#176203,
#176204,#176205,#176206,#176207,#176208,#176209,#176210),.UNSPECIFIED.,
 .F.,.F.,(4,2,2,2,2,2,2,2,2,2,2,2,2,2,2,2,2,2,2,2,2,2,2,2,2,2,2,2,2,2,2,
2,2,2,2,2,2,2,2,2,2,2,2,2,2,2,2,2,2,2,2,2,2,2,2,2,2,2,2,2,2,2,2,2,2,2,2,
2,2,2,2,2,2,2,2,2,2,2,2,2,2,2,2,2,2,2,2,2,2,2,2,2,2,2,2,2,2,2,2,2,2,2,2,
2,2,2,2,2,2,2,2,2,2,4),(1.40869684638067,1.45282843584756,1.47139153129055,
1.47413797142721,1.47549374264355,1.47656594495266,1.47781700648748,1.48006379995523,
1.49092661598699,1.51513105515911,1.55576274020903,1.57471834154224,1.57847301714692,
1.58088008000737,1.58279806296705,1.58496219546508,1.58861933921804,1.60315458464438,
1.63040943645443,1.67885530689127,1.6848724182356,1.68679164489817,1.68797022456709,
1.68905892046346,1.69054582954117,1.69399109741873,1.72339037290005,1.74244927090556,
1.7857829634416,1.79007584733931,1.79261693152861,1.79455821379679,1.7966328302524,
1.7998849248117,1.81021815464008,1.82682882107904,1.85976403632507,1.87664269438957,
1.88258541443695,1.89582906497522,1.8980970124788,1.89947544063993,1.90055205795811,
1.9017728389302,1.90388172087427,1.91271551805827,1.93013747091191,1.98024680163006,
1.99885474444774,2.0025864252489,2.00498643324687,2.00690376651553,2.0090724765539,
2.01275030228118,2.02754321747452,2.0555561790587,2.10529260279538,2.10950546056186,
2.11116748441838,2.11217792702289,2.11328233968098,2.11485664842832,2.11882605818134,
2.13856756495848,2.16752538738815,2.20987543263793,2.2141699598811,2.21671152958959,
2.21865290204596,2.22072734256464,2.22397859237694,2.2343043333581,2.25089838425513,
2.28381993277496,2.299787081885,2.30320930710508,2.31967420772753,2.32231284691757,
2.32366452388258,2.32473648328883,2.3259907191237,2.32825190546424,2.33935483750962,
2.36446444931113,2.41873422061789,2.42552403892733,2.42837396756816,2.43016431875726,
2.43208993035218,2.43472297659844,2.4376774992918,2.44275935847805,2.4536356672814,
2.48468546992922,2.52883690999794,2.53346430380101,2.53519168928287,2.53621472676427,
2.5373092542562,2.53883045378196,2.54247536084109,2.55926024272092,2.61328639023885,
2.62540476019049,2.62723236323862,2.62823403157241,2.63692330652055,2.64007496601508,
2.64192232708146,2.64377759546468,2.6456459633452,2.64804781939747,2.65178836875005,
2.66842437218317),.UNSPECIFIED.);
#1841=B_SPLINE_CURVE_WITH_KNOTS('',3,(#176211,#176212,#176213,#176214,#176215,
#176216,#176217,#176218,#176219,#176220),.UNSPECIFIED.,.F.,.F.,(4,3,3,4),
(-85.8723819043546,-85.755698970363,-85.6390734987538,-85.5224480271446),
 .UNSPECIFIED.);
#1842=B_SPLINE_CURVE_WITH_KNOTS('',3,(#176225,#176226,#176227,#176228,#176229,
#176230,#176231,#176232,#176233,#176234,#176235,#176236,#176237,#176238,
#176239,#176240,#176241,#176242,#176243,#176244,#176245,#176246,#176247,
#176248,#176249,#176250,#176251,#176252,#176253,#176254,#176255,#176256,
#176257,#176258,#176259,#176260,#176261,#176262,#176263,#176264,#176265,
#176266,#176267,#176268,#176269,#176270,#176271,#176272,#176273,#176274,
#176275,#176276,#176277,#176278,#176279,#176280,#176281,#176282,#176283,
#176284,#176285,#176286,#176287,#176288,#176289,#176290,#176291,#176292,
#176293,#176294,#176295,#176296,#176297,#176298,#176299,#176300,#176301,
#176302,#176303,#176304,#176305,#176306,#176307,#176308,#176309,#176310,
#176311,#176312,#176313,#176314,#176315,#176316,#176317,#176318,#176319,
#176320,#176321,#176322,#176323,#176324,#176325,#176326,#176327,#176328,
#176329,#176330,#176331,#176332,#176333,#176334,#176335,#176336,#176337,
#176338,#176339,#176340,#176341,#176342,#176343,#176344,#176345,#176346,
#176347,#176348,#176349,#176350,#176351,#176352,#176353,#176354,#176355,
#176356,#176357,#176358,#176359,#176360,#176361,#176362,#176363,#176364,
#176365,#176366,#176367,#176368,#176369,#176370,#176371,#176372,#176373,
#176374,#176375,#176376,#176377,#176378,#176379,#176380,#176381,#176382,
#176383,#176384,#176385,#176386,#176387,#176388,#176389,#176390,#176391,
#176392,#176393,#176394,#176395,#176396,#176397,#176398,#176399,#176400,
#176401,#176402,#176403,#176404,#176405,#176406,#176407,#176408,#176409,
#176410,#176411,#176412,#176413,#176414,#176415,#176416,#176417,#176418,
#176419,#176420,#176421,#176422,#176423,#176424,#176425,#176426,#176427,
#176428,#176429,#176430,#176431,#176432,#176433,#176434,#176435,#176436,
#176437,#176438,#176439,#176440,#176441,#176442,#176443,#176444,#176445,
#176446,#176447,#176448,#176449,#176450,#176451,#176452,#176453,#176454,
#176455,#176456,#176457,#176458),.UNSPECIFIED.,.F.,.F.,(4,2,2,2,2,2,2,2,
2,2,2,2,2,2,2,2,2,2,2,2,2,2,2,2,2,2,2,2,2,2,2,2,2,2,2,2,2,2,2,2,2,2,2,2,
2,2,2,2,2,2,2,2,2,2,2,2,2,2,2,2,2,2,2,2,2,2,2,2,2,2,2,2,2,2,2,2,2,2,2,2,
2,2,2,2,2,2,2,2,2,2,2,2,2,2,2,2,2,2,2,2,2,2,2,2,2,2,2,2,2,2,2,2,2,2,2,2,
4),(1.25998791133046,1.26024242500464,1.26239919564322,1.26363040643267,
1.26470495450532,1.26608904347515,1.26897931713014,1.2946802036782,1.33412358883784,
1.36184468975562,1.365984948207,1.36848121557409,1.3704151048674,1.3725084082164,
1.37584668051751,1.38696194568658,1.40534596761406,1.45269478775345,1.47125602150215,
1.47400217378428,1.47535780193761,1.4764298906353,1.47768081907448,1.4799273721928,
1.49078900086812,1.51499074218715,1.5556182103993,1.57457185689772,1.57832613872912,
1.58073294772477,1.58265072748706,1.58481462973893,1.58847138205162,1.60300504053265,
1.63025686999265,1.67869647391258,1.68471398853011,1.68663314099338,1.68781162454298,
1.68890019358684,1.6903868751714,1.69383137905133,1.73244164718219,1.7820191168021,
1.78911702252191,1.79201778588942,1.79381727822345,1.79577415262608,1.79845378998335,
1.8047143767895,1.8319836912695,1.87335236275129,1.87999866272132,1.89550853911073,
1.89810753672073,1.89945057988605,1.90052186307516,1.90178248353017,1.90407348974339,
1.91570147049743,1.9428858704825,1.9941791754067,2.0011879871368,2.004073859346,
2.00587058789711,2.00782961014574,2.01052153930724,2.01685412987579,2.04471505668319,
2.09013785020724,2.1074391827338,2.11010913681588,2.11146742182158,2.11253974323807,
2.11378879751528,2.1160266407964,2.12674430957233,2.15041407152702,2.2068425921498,
2.21342049874239,2.2159526974858,2.21777704697382,2.21971728601298,2.22229824838344,
2.22800315716179,2.25094047087012,2.283951813764,2.30421150100962,2.30447940405299,
2.30917138770076,2.32002049487248,2.32215449014924,2.32350708441768,2.32457889711014,
2.32583195253543,2.32808847167246,2.33911822898416,2.3639527540638,2.41860981546139,
2.42536231845443,2.42820563734438,2.4299945240523,2.43192069962384,2.43455838914489,
2.43751954516248,2.44261831620993,2.45354607783007,2.48454341821539,2.52865262843015,
2.53326833133215,2.53499371288607,2.53601620908544,2.53711071152186,2.53863278588737,
2.54228406115615,2.55912777263654,2.59377040355344),.UNSPECIFIED.);
#1843=B_SPLINE_CURVE_WITH_KNOTS('',3,(#176460,#176461,#176462,#176463,#176464,
#176465,#176466,#176467,#176468,#176469,#176470,#176471,#176472,#176473,
#176474,#176475,#176476,#176477,#176478,#176479,#176480,#176481,#176482,
#176483,#176484,#176485,#176486,#176487,#176488,#176489,#176490,#176491,
#176492,#176493,#176494,#176495,#176496,#176497,#176498,#176499,#176500,
#176501,#176502,#176503,#176504,#176505,#176506,#176507,#176508,#176509,
#176510,#176511,#176512,#176513,#176514,#176515,#176516,#176517,#176518,
#176519,#176520,#176521,#176522,#176523,#176524,#176525,#176526,#176527,
#176528,#176529,#176530,#176531,#176532,#176533,#176534,#176535,#176536,
#176537,#176538,#176539,#176540,#176541,#176542,#176543,#176544,#176545,
#176546,#176547,#176548,#176549,#176550,#176551,#176552,#176553,#176554,
#176555,#176556,#176557,#176558,#176559,#176560,#176561,#176562,#176563,
#176564,#176565,#176566,#176567,#176568,#176569,#176570,#176571,#176572,
#176573,#176574,#176575,#176576,#176577,#176578,#176579,#176580,#176581,
#176582,#176583,#176584,#176585,#176586,#176587,#176588,#176589,#176590,
#176591,#176592,#176593,#176594,#176595,#176596,#176597,#176598,#176599,
#176600,#176601,#176602,#176603,#176604,#176605,#176606,#176607,#176608,
#176609,#176610,#176611,#176612,#176613,#176614,#176615,#176616,#176617,
#176618,#176619,#176620,#176621,#176622,#176623,#176624,#176625,#176626,
#176627,#176628,#176629,#176630,#176631,#176632,#176633,#176634,#176635,
#176636,#176637,#176638,#176639,#176640),.UNSPECIFIED.,.F.,.F.,(4,3,3,3,
3,3,3,3,3,3,3,3,3,3,3,3,3,3,3,3,3,3,3,3,3,3,3,3,3,3,3,3,3,3,3,3,3,3,3,3,
3,3,3,3,3,3,3,3,3,3,3,3,3,3,3,3,3,3,3,3,4),(-91.8056330559228,-91.7034783920473,
-91.6014794906875,-91.4995669524817,-91.3977052133723,-91.2958587787107,
-91.1939207704893,-91.0919397623294,-90.9897717066984,-90.8941169465306,
-90.7907222094827,-90.6874809273677,-90.5843609619754,-90.4813063937665,
-90.3782831854089,-90.2752573427364,-90.1721245759583,-90.0689354845485,
-89.9655634911669,-89.8952804965687,-89.7918857595208,-89.6886444774058,
-89.5855245120135,-89.4824699438045,-89.3794467354467,-89.2764208927743,
-89.1732881259961,-89.0700990345863,-88.9667270412046,-88.8964440466068,
-88.7930493095589,-88.6898080274442,-88.586688062052,-88.4836334938431,
-88.3806102854853,-88.2775844428131,-88.174451676035,-88.0712625846253,
-87.9678905912437,-87.897607596645,-87.7942128595971,-87.690971577482,-87.5878516120897,
-87.4847970438806,-87.3817738355228,-87.2787479928504,-87.1756152260724,
-87.0724261346626,-86.969054141281,-86.8987711466831,-86.7953764096351,
-86.6921351275202,-86.5890151621278,-86.4859605939189,-86.382937385561,
-86.2799115428888,-86.1767787761106,-86.0735896847007,-85.970217691319,
-85.8999346967212,-85.8723819043546),.UNSPECIFIED.);
#1844=B_SPLINE_CURVE_WITH_KNOTS('',3,(#176641,#176642,#176643,#176644,#176645),
 .UNSPECIFIED.,.F.,.F.,(4,1,4),(-92.1566391741352,-91.8929533964925,-91.8056333339369),
 .UNSPECIFIED.);
#1845=B_SPLINE_CURVE_WITH_KNOTS('',3,(#176651,#176652,#176653,#176654,#176655,
#176656,#176657,#176658,#176659,#176660,#176661,#176662,#176663,#176664,
#176665,#176666,#176667,#176668,#176669,#176670,#176671,#176672),
 .UNSPECIFIED.,.F.,.F.,(4,2,2,2,2,2,2,2,2,2,4),(2.59436936426754,2.62465525255589,
2.6484457796913,2.6563175990635,2.65841363975286,2.6596436413572,2.66070047280065,
2.66174639015292,2.66309684904183,2.66555495191749,2.6686486774568),
 .UNSPECIFIED.);
#1846=B_SPLINE_CURVE_WITH_KNOTS('',3,(#176673,#176674,#176675,#176676,#176677,
#176678,#176679,#176680,#176681,#176682,#176683,#176684,#176685,#176686,
#176687,#176688,#176689,#176690,#176691,#176692,#176693,#176694,#176695,
#176696,#176697,#176698,#176699,#176700,#176701,#176702,#176703,#176704,
#176705,#176706,#176707,#176708,#176709,#176710,#176711,#176712,#176713,
#176714,#176715,#176716,#176717,#176718,#176719,#176720,#176721,#176722,
#176723,#176724,#176725,#176726,#176727,#176728,#176729,#176730,#176731,
#176732,#176733,#176734,#176735,#176736,#176737,#176738,#176739,#176740,
#176741,#176742,#176743,#176744,#176745,#176746,#176747,#176748,#176749,
#176750,#176751,#176752,#176753,#176754,#176755,#176756,#176757,#176758,
#176759,#176760,#176761,#176762,#176763,#176764,#176765,#176766,#176767,
#176768,#176769,#176770,#176771,#176772,#176773,#176774,#176775,#176776,
#176777,#176778,#176779,#176780,#176781,#176782,#176783,#176784,#176785,
#176786,#176787,#176788,#176789,#176790,#176791,#176792,#176793,#176794,
#176795,#176796,#176797,#176798,#176799,#176800,#176801,#176802,#176803,
#176804,#176805,#176806,#176807,#176808,#176809,#176810,#176811,#176812,
#176813,#176814,#176815,#176816,#176817,#176818,#176819,#176820,#176821,
#176822,#176823,#176824,#176825,#176826,#176827,#176828,#176829,#176830,
#176831,#176832,#176833,#176834,#176835,#176836,#176837,#176838,#176839,
#176840,#176841,#176842,#176843,#176844,#176845,#176846,#176847,#176848,
#176849,#176850,#176851,#176852,#176853,#176854,#176855,#176856,#176857,
#176858,#176859,#176860,#176861,#176862,#176863,#176864,#176865,#176866,
#176867,#176868,#176869,#176870,#176871,#176872,#176873,#176874,#176875,
#176876,#176877,#176878,#176879,#176880,#176881,#176882,#176883,#176884,
#176885,#176886,#176887,#176888,#176889,#176890,#176891,#176892,#176893,
#176894,#176895,#176896,#176897,#176898,#176899,#176900),.UNSPECIFIED.,
 .F.,.F.,(4,2,2,2,2,2,2,2,2,2,2,2,2,2,2,2,2,2,2,2,2,2,2,2,2,2,2,2,2,2,2,
2,2,2,2,2,2,2,2,2,2,2,2,2,2,2,2,2,2,2,2,2,2,2,2,2,2,2,2,2,2,2,2,2,2,2,2,
2,2,2,2,2,2,2,2,2,2,2,2,2,2,2,2,2,2,2,2,2,2,2,2,2,2,2,2,2,2,2,2,2,2,2,2,
2,2,2,2,2,2,2,2,2,2,4),(0.000817344086041159,0.0612273919498641,0.0876740801193658,
0.0938319778978367,0.0964930492572893,0.098445916956004,0.10024843117888,
0.103169002752325,0.11039006372335,0.154190655546873,0.195390525340292,
0.199210997745504,0.201236633489129,0.202548493583,0.203772360348178,0.203775924959625,
0.20377950209078,0.20378309200526,0.203786919778984,0.20379080898577,0.203794761166127,
0.203798777733783,0.203802859832712,0.203807008834988,0.203811226399929,
0.20485382976206,0.206215941873864,0.208996272577505,0.228693719507084,
0.27474163152674,0.293140210772685,0.304261621807657,0.307599685704812,
0.309692404299447,0.311625444707257,0.314120185036224,0.31825700462144,
0.345888070718099,0.388200003981098,0.404174667384379,0.412512770760822,
0.414581741117975,0.415793247154152,0.416871061291057,0.418263154471234,
0.420578800539232,0.43480898130666,0.483112060256287,0.511251700506572,
0.517617119438996,0.520313936998886,0.52227319669367,0.524067850567381,
0.526945354508734,0.533908091086557,0.585900847573902,0.612587659650053,
0.624089895485527,0.626373200063177,0.627631823572945,0.628702764682022,
0.63004709293401,0.632653579135124,0.648359659618089,0.692810926181391,
0.715109505886791,0.727829795237389,0.731327778194906,0.733455972991943,
0.73537942610946,0.737844614280843,0.741792255381091,0.764379873525667,
0.823320016195228,0.835967143277367,0.838311346381681,0.839583216957975,
0.840653445551531,0.841981864392049,0.844037552281527,0.853719298631803,
0.859523384065908,0.859958365484185,0.866842920809183,0.880568808716069,
0.913426383209187,0.929986567229701,0.940296859256234,0.943545472397734,
0.945618772206083,0.947559458069651,0.950100679709231,0.954395885224703,
0.989519314416273,1.03844552960186,1.04822026746025,1.05039677999474,1.05163225416324,
1.05270602646014,1.05408323483342,1.05693879862438,1.07971753539956,1.09256085135529,
1.12541335058915,1.1419649645055,1.15227167883996,1.15552010055828,1.15759350313277,
1.15953444321355,1.16207622576685,1.16637289051967,1.20157678546922,1.25075405362961,
1.25998791133046),.UNSPECIFIED.);
#1847=B_SPLINE_CURVE_WITH_KNOTS('',3,(#176902,#176903,#176904,#176905,#176906,
#176907,#176908,#176909,#176910,#176911),.UNSPECIFIED.,.F.,.F.,(4,1,1,1,
1,1,1,4),(-98.0888186411165,-97.8859720962637,-96.8871356463018,-95.88829919634,
-94.8894627463781,-93.8906262964162,-92.8917898464543,-92.1566391741352),
 .UNSPECIFIED.);
#1848=B_SPLINE_CURVE_WITH_KNOTS('',3,(#176912,#176913,#176914,#176915,#176916,
#176917,#176918,#176919,#176920,#176921,#176922,#176923,#176924,#176925,
#176926,#176927,#176928,#176929,#176930,#176931),.UNSPECIFIED.,.F.,.F.,
(4,2,2,2,2,2,2,2,2,4),(0.000629226955841834,0.0468644005961875,0.0541763610534283,
0.0579973882184613,0.0612784598809704,0.0633586706615918,0.0652962163607798,
0.0678195720804087,0.0720540263829488,0.0751037223624835),.UNSPECIFIED.);
#1849=B_SPLINE_CURVE_WITH_KNOTS('',3,(#176936,#176937,#176938,#176939,#176940,
#176941,#176942,#176943,#176944,#176945,#176946,#176947,#176948,#176949,
#176950,#176951,#176952,#176953,#176954,#176955,#176956,#176957,#176958,
#176959,#176960,#176961,#176962,#176963,#176964,#176965,#176966,#176967,
#176968,#176969,#176970,#176971,#176972,#176973,#176974,#176975,#176976,
#176977,#176978,#176979,#176980,#176981,#176982,#176983,#176984,#176985,
#176986,#176987,#176988,#176989,#176990,#176991,#176992,#176993,#176994,
#176995,#176996,#176997,#176998,#176999,#177000,#177001,#177002,#177003,
#177004,#177005,#177006,#177007,#177008,#177009,#177010,#177011,#177012,
#177013,#177014,#177015,#177016,#177017,#177018,#177019,#177020,#177021,
#177022,#177023,#177024,#177025,#177026,#177027,#177028,#177029,#177030,
#177031,#177032,#177033,#177034,#177035,#177036,#177037,#177038,#177039,
#177040,#177041,#177042,#177043,#177044,#177045,#177046,#177047,#177048,
#177049,#177050,#177051,#177052,#177053,#177054,#177055,#177056,#177057,
#177058,#177059,#177060,#177061,#177062,#177063,#177064,#177065,#177066,
#177067,#177068,#177069,#177070,#177071,#177072,#177073,#177074,#177075,
#177076,#177077,#177078,#177079,#177080,#177081,#177082,#177083,#177084,
#177085,#177086,#177087,#177088,#177089,#177090,#177091,#177092,#177093,
#177094,#177095,#177096,#177097,#177098,#177099,#177100,#177101,#177102,
#177103,#177104,#177105,#177106,#177107,#177108,#177109,#177110,#177111,
#177112,#177113,#177114,#177115,#177116,#177117,#177118,#177119,#177120,
#177121,#177122,#177123,#177124,#177125,#177126,#177127,#177128,#177129,
#177130,#177131,#177132,#177133,#177134,#177135,#177136,#177137,#177138,
#177139,#177140,#177141,#177142,#177143,#177144,#177145,#177146,#177147,
#177148,#177149,#177150,#177151,#177152,#177153,#177154,#177155,#177156,
#177157,#177158,#177159,#177160,#177161,#177162,#177163,#177164,#177165,
#177166,#177167,#177168,#177169,#177170,#177171,#177172,#177173),
 .UNSPECIFIED.,.F.,.F.,(4,2,2,2,2,2,2,2,2,2,2,2,2,2,2,2,2,2,2,2,2,2,2,2,
2,2,2,2,2,2,2,2,2,2,2,2,2,2,2,2,2,2,2,2,2,2,2,2,2,2,2,2,2,2,2,2,2,2,2,2,
2,2,2,2,2,2,2,2,2,2,2,2,2,2,2,2,2,2,2,2,2,2,2,2,2,2,2,2,2,2,2,2,2,2,2,2,
2,2,2,2,2,2,2,2,2,2,2,2,2,2,2,2,2,2,2,2,2,2,4),(1.2602735482109,1.26524054933663,
1.27572678542071,1.27899648729593,1.2810750955584,1.28301505575824,1.28554714969485,
1.28980869553093,1.33481507250788,1.37987265493806,1.38459854900304,1.38634110502145,
1.38736724901935,1.38846010627813,1.3899708367368,1.39355297507645,1.43119610811479,
1.48162620370429,1.48868576676276,1.49158060582017,1.49337936338234,1.49533777291039,
1.49802373704153,1.50431857130575,1.53186137828442,1.56026918777434,1.5826023287173,
1.59531105022385,1.5975519259267,1.59893716540897,1.60001213077348,1.60124329461293,
1.60339872973208,1.61286169964153,1.66205401313269,1.69726375900075,1.70156163028444,
1.70410423789648,1.70604586115812,1.70812004416496,1.7113697930735,1.72168151420924,
1.73824423161456,1.77114074799051,1.78487809342853,1.79175063948774,1.79196058592751,
1.79531500384449,1.80743272705653,1.80964180457274,1.81101740113463,1.81209135996309,
1.81332868926533,1.81551239220539,1.82538521736245,1.87422390424592,1.90932066511989,
1.91361678748023,1.91615879605051,1.91810021275967,1.92017441839195,1.92342471074427,
1.93374243897526,1.95031888046098,1.9832254465123,1.9980832698433,2.00311584368939,
2.01914780776842,2.02176933599478,2.02311731833539,2.02418900962129,2.02544601531626,
2.02772000984015,2.03904389303407,2.06501019048752,2.11803206612321,2.12492422933445,
2.12779102136437,2.1295843971836,2.13154660584663,2.13425542872474,2.14068665178564,
2.16936621182781,2.22067137106803,2.2316908521092,2.23383583469551,2.23519193710948,
2.23626421898748,2.23751516357257,2.23976122283613,2.25061039974527,2.27476320132649,
2.33046247571524,2.33711872183493,2.33966348919224,2.34149130584987,2.34343008919646,
2.34600035908364,2.35164587457701,2.37414026249403,2.40687040215125,2.44298543729769,
2.44584303621401,2.44722085728533,2.44826025588754,2.44945571223507,2.45072982857325,
2.45266376421573,2.45624155504831,2.46471622201167,2.52444415254189,2.54624111812614,
2.55015681175158,2.55261285073262,2.55453587262887,2.55667046904025,2.56019486561849,
2.57319060392375,2.59436936426754),.UNSPECIFIED.);
#1850=B_SPLINE_CURVE_WITH_KNOTS('',3,(#177174,#177175,#177176,#177177,#177178,
#177179,#177180,#177181,#177182,#177183,#177184,#177185,#177186,#177187,
#177188,#177189,#177190,#177191,#177192,#177193,#177194,#177195,#177196,
#177197,#177198,#177199,#177200,#177201,#177202,#177203,#177204,#177205,
#177206,#177207,#177208,#177209,#177210,#177211,#177212,#177213,#177214,
#177215,#177216,#177217,#177218,#177219,#177220,#177221,#177222,#177223,
#177224,#177225,#177226,#177227,#177228,#177229,#177230,#177231,#177232,
#177233,#177234,#177235,#177236,#177237,#177238,#177239,#177240,#177241,
#177242,#177243,#177244,#177245,#177246,#177247,#177248,#177249,#177250,
#177251,#177252,#177253,#177254,#177255,#177256,#177257,#177258,#177259,
#177260,#177261,#177262,#177263,#177264,#177265,#177266,#177267,#177268,
#177269,#177270,#177271,#177272,#177273,#177274,#177275,#177276,#177277,
#177278,#177279,#177280,#177281,#177282,#177283,#177284,#177285,#177286,
#177287,#177288,#177289,#177290,#177291,#177292,#177293,#177294,#177295,
#177296,#177297,#177298,#177299,#177300,#177301,#177302,#177303,#177304,
#177305,#177306,#177307,#177308,#177309,#177310,#177311,#177312,#177313,
#177314,#177315,#177316,#177317,#177318,#177319,#177320,#177321,#177322,
#177323,#177324,#177325,#177326,#177327,#177328,#177329,#177330,#177331,
#177332,#177333,#177334,#177335,#177336,#177337,#177338,#177339,#177340,
#177341,#177342,#177343,#177344,#177345,#177346,#177347,#177348,#177349,
#177350,#177351,#177352,#177353,#177354,#177355,#177356,#177357,#177358,
#177359,#177360,#177361,#177362,#177363,#177364,#177365,#177366,#177367,
#177368,#177369,#177370,#177371,#177372,#177373,#177374,#177375,#177376,
#177377,#177378,#177379,#177380,#177381,#177382,#177383,#177384,#177385,
#177386,#177387,#177388,#177389,#177390,#177391,#177392,#177393,#177394,
#177395,#177396,#177397,#177398,#177399),.UNSPECIFIED.,.F.,.F.,(4,2,2,2,
2,2,2,2,2,2,2,2,2,2,2,2,2,2,2,2,2,2,2,2,2,2,2,2,2,2,2,2,2,2,2,2,2,2,2,2,
2,2,2,2,2,2,2,2,2,2,2,2,2,2,2,2,2,2,2,2,2,2,2,2,2,2,2,2,2,2,2,2,2,2,2,2,
2,2,2,2,2,2,2,2,2,2,2,2,2,2,2,2,2,2,2,2,2,2,2,2,2,2,2,2,2,2,2,2,2,2,2,2,
4),(0.0751037223624835,0.118900071491345,0.139440611476386,0.162494609014913,
0.166929447372164,0.168203542012268,0.16941891659701,0.170495934977998,
0.171881528995767,0.17417499241479,0.187957175240597,0.190682887305246,
0.190933904540755,0.199768469865087,0.24375060366284,0.259912600165475,
0.270000149625801,0.273247427352306,0.27532023318146,0.27726070839858,0.279802017491679,
0.284098185254886,0.319339705674213,0.368614641292319,0.377961258390835,
0.380107549102336,0.381336258131637,0.382410885506348,0.383798058387966,
0.386046712681178,0.398924057679309,0.401653712218978,0.405940989869747,
0.448932565391636,0.476872490705792,0.483214204736425,0.485907202932065,
0.487865973176792,0.489661760994714,0.492544552608456,0.499537871890721,
0.551075277271631,0.578095800714917,0.589681412156881,0.59196960561499,
0.593229390121345,0.594300394767089,0.595643630561402,0.598244579921869,
0.613814860738228,0.620269138462949,0.661687588346286,0.688961708677915,
0.695222503312131,0.697901721679331,0.699858103700696,0.701657017221726,
0.704556556685558,0.711650019409065,0.761312279955728,0.799626380882392,
0.803230961460248,0.804745028476189,0.805838017498936,0.806862472882087,
0.808598302539427,0.813283520889909,0.854368024800134,0.900801490929616,
0.907193854351943,0.909895570960788,0.911856010895325,0.913650103924896,
0.916523120549423,0.923456525761156,0.975907063984641,1.00228278043963,
1.01370811533073,1.01598740384887,1.0172453106221,1.01831654721534,1.01966239680701,
1.02227520012398,1.0381277176306,1.0428721627749,1.0581510675028,1.09102885175531,
1.10761165021532,1.1179323842797,1.1211823533058,1.12325605403864,1.12519678906149,
1.12773760466332,1.13203106984393,1.17443434157364,1.20349382106149,1.22311111557103,
1.22706657205871,1.22863835153548,1.22974200779255,1.2307525433553,1.23241627501659,
1.2366416743528,1.28598846466241,1.32675994086166,1.33182657063566,1.33428638208849,
1.33620950461565,1.33834128821519,1.34185428160786,1.3547312148031,1.37743522651096,
1.40858865855495),.UNSPECIFIED.);
#1851=B_SPLINE_CURVE_WITH_KNOTS('',3,(#177405,#177406,#177407,#177408),
 .UNSPECIFIED.,.F.,.F.,(4,4),(114.406674973147,114.756144634991),
 .UNSPECIFIED.);
#1852=B_SPLINE_CURVE_WITH_KNOTS('',3,(#177409,#177410,#177411,#177412,#177413,
#177414,#177415,#177416,#177417,#177418,#177419,#177420,#177421,#177422,
#177423,#177424,#177425,#177426,#177427,#177428,#177429,#177430,#177431,
#177432,#177433,#177434,#177435,#177436,#177437,#177438,#177439,#177440,
#177441,#177442,#177443,#177444,#177445,#177446,#177447,#177448,#177449,
#177450,#177451,#177452,#177453,#177454,#177455,#177456,#177457,#177458,
#177459,#177460,#177461,#177462,#177463,#177464,#177465,#177466,#177467,
#177468,#177469,#177470,#177471,#177472,#177473,#177474,#177475,#177476,
#177477,#177478,#177479,#177480,#177481,#177482,#177483,#177484,#177485,
#177486,#177487,#177488,#177489,#177490,#177491,#177492,#177493,#177494,
#177495,#177496,#177497,#177498,#177499,#177500,#177501,#177502,#177503,
#177504,#177505,#177506,#177507,#177508,#177509,#177510,#177511,#177512,
#177513,#177514,#177515,#177516,#177517,#177518,#177519,#177520,#177521,
#177522,#177523,#177524,#177525,#177526,#177527,#177528,#177529,#177530,
#177531,#177532,#177533,#177534,#177535,#177536,#177537,#177538,#177539,
#177540,#177541,#177542,#177543,#177544,#177545,#177546,#177547,#177548,
#177549,#177550,#177551,#177552,#177553,#177554,#177555,#177556,#177557,
#177558,#177559,#177560,#177561,#177562,#177563,#177564,#177565,#177566,
#177567,#177568,#177569,#177570,#177571,#177572,#177573,#177574,#177575,
#177576,#177577,#177578,#177579,#177580,#177581,#177582,#177583,#177584,
#177585,#177586,#177587,#177588,#177589,#177590,#177591,#177592,#177593,
#177594,#177595,#177596,#177597,#177598,#177599,#177600,#177601,#177602,
#177603,#177604,#177605,#177606,#177607,#177608,#177609,#177610,#177611,
#177612,#177613,#177614,#177615,#177616,#177617,#177618,#177619,#177620,
#177621,#177622,#177623,#177624),.UNSPECIFIED.,.F.,.F.,(4,2,2,2,2,2,2,2,
2,2,2,2,2,2,2,2,2,2,2,2,2,2,2,2,2,2,2,2,2,2,2,2,2,2,2,2,2,2,2,2,2,2,2,2,
2,2,2,2,2,2,2,2,2,2,2,2,2,2,2,2,2,2,2,2,2,2,2,2,2,2,2,2,2,2,2,2,2,2,2,2,
2,2,2,2,2,2,2,2,2,2,2,2,2,2,2,2,2,2,2,2,2,2,2,2,2,2,2,4),(0.000658788743625867,
0.00332970120247789,0.0059216581112381,0.00778879636083556,0.00964368915836675,
0.0114909184573996,0.0146445377481801,0.0233614972363175,0.0916990880801217,
0.109068193657669,0.112778808087098,0.114310760389999,0.11540697933727,
0.116426840351137,0.118138930635243,0.122667883778095,0.169431857768071,
0.208758990986267,0.213873118206603,0.216840473135931,0.218921510588389,
0.220936589487488,0.222824536013458,0.225367120679629,0.229666778264646,
0.264877030777271,0.314097831342373,0.323532822729939,0.325685733763093,
0.326916056242964,0.327990681575802,0.329375991757707,0.332272740972979,
0.358675098332123,0.367914145845947,0.400741271683807,0.417260994262733,
0.427553432816872,0.430800331440078,0.432873478033103,0.434814681886291,
0.437357536618714,0.441657643812989,0.476789978187575,0.525756231602942,
0.535494695252995,0.537668971011242,0.538904077655923,0.539978108504761,
0.541356404323984,0.544216825744425,0.580267587356483,0.612981104505948,
0.635495272040016,0.641143633966508,0.643714316398006,0.645653053004703,
0.647480566482349,0.650024495973927,0.656676003782097,0.71244616816722,
0.736576055135473,0.747418055806598,0.749663601083023,0.750914381459764,
0.751986601753206,0.75334272058979,0.756002307100268,0.773020197169769,
0.823201341733096,0.840782435432029,0.851549275611795,0.854849905626905,
0.856935048636541,0.858872028085661,0.861387314033059,0.865592071978735,
0.895849861764218,0.947380641155931,0.959374744285399,0.961685910910082,
0.962950974924926,0.964022068207264,0.965359863396906,0.967445076168874,
0.977540170700345,0.983029053873848,0.9924188375024,1.00399162343487,1.03684321083926,
1.0533867454283,1.06369065632845,1.06693938111617,1.06901326248663,1.07095485129084,
1.07349777279795,1.07779701178068,1.11311224973216,1.1623737843867,1.17171279034325,
1.17385935466317,1.17508854481749,1.17616380431521,1.17755207184592,1.18046252839983,
1.20859761461961,1.24829263426394,1.2602735482109),.UNSPECIFIED.);
#1853=B_SPLINE_CURVE_WITH_KNOTS('',3,(#177626,#177627,#177628,#177629,#177630,
#177631,#177632,#177633,#177634,#177635,#177636,#177637,#177638,#177639,
#177640,#177641,#177642,#177643,#177644,#177645,#177646,#177647,#177648,
#177649,#177650,#177651,#177652,#177653,#177654,#177655,#177656,#177657,
#177658,#177659,#177660,#177661,#177662,#177663,#177664,#177665,#177666,
#177667,#177668,#177669,#177670,#177671,#177672,#177673,#177674,#177675,
#177676,#177677,#177678,#177679,#177680,#177681,#177682,#177683,#177684,
#177685,#177686,#177687,#177688,#177689,#177690,#177691,#177692,#177693,
#177694,#177695,#177696,#177697,#177698,#177699,#177700,#177701,#177702,
#177703,#177704,#177705,#177706,#177707,#177708,#177709,#177710,#177711,
#177712,#177713,#177714,#177715,#177716,#177717,#177718,#177719,#177720,
#177721,#177722,#177723,#177724,#177725,#177726,#177727,#177728,#177729,
#177730,#177731,#177732,#177733,#177734,#177735,#177736,#177737,#177738,
#177739,#177740,#177741,#177742,#177743,#177744,#177745,#177746,#177747,
#177748,#177749,#177750,#177751,#177752,#177753,#177754,#177755,#177756,
#177757,#177758,#177759,#177760,#177761,#177762,#177763,#177764,#177765,
#177766,#177767,#177768,#177769,#177770,#177771,#177772,#177773,#177774,
#177775,#177776,#177777,#177778,#177779,#177780,#177781,#177782,#177783,
#177784,#177785,#177786,#177787,#177788,#177789,#177790,#177791,#177792,
#177793,#177794,#177795,#177796,#177797,#177798,#177799,#177800,#177801,
#177802,#177803,#177804,#177805,#177806,#177807,#177808,#177809,#177810,
#177811,#177812,#177813,#177814,#177815,#177816,#177817,#177818,#177819,
#177820,#177821,#177822,#177823,#177824,#177825,#177826,#177827,#177828,
#177829,#177830,#177831,#177832,#177833,#177834,#177835,#177836,#177837,
#177838,#177839,#177840,#177841,#177842,#177843,#177844,#177845,#177846,
#177847),.UNSPECIFIED.,.F.,.F.,(4,2,2,2,2,2,2,2,2,2,2,2,2,2,2,2,2,2,2,2,
2,2,2,2,2,2,2,2,2,2,2,2,2,2,2,2,2,2,2,2,2,2,2,2,2,2,2,2,2,2,2,2,2,2,2,2,
2,2,2,2,2,2,2,2,2,2,2,2,2,2,2,2,2,2,2,2,2,2,2,2,2,2,2,2,2,2,2,2,2,2,2,2,
2,2,2,2,2,2,2,2,2,2,2,2,2,2,2,2,2,2,4),(1.40858865855495,1.41602849107768,
1.4210231606735,1.43703140374578,1.43965097151703,1.44099826580354,1.44206957836628,
1.44332633491721,1.44560037454426,1.45693465181834,1.48294808340535,1.5358716731755,
1.54276761216823,1.54563443688785,1.5474273867354,1.54938877055155,1.55209579696157,
1.55851964063635,1.58714587007974,1.63843210451319,1.64949485401555,1.65164202046835,
1.65299855082524,1.65407053545689,1.65532040249688,1.65756270368058,1.66835879189345,
1.69232031536541,1.74827928178904,1.75490511378606,1.7574446028402,1.75927063232313,
1.76120936507317,1.76378270830783,1.7694477780549,1.79209323471846,1.82491410613751,
1.82944508984973,1.86063062017755,1.86354284731735,1.86493104121718,1.86600581705397,
1.86723398626325,1.86937765641769,1.87868716725339,1.92782912581056,1.96320834519401,
1.96750626277942,1.97004819672523,1.97198890199243,1.97406171321363,1.97730849662109,
1.98760393538259,2.00413396908774,2.03699317678459,2.04850576240806,2.05831797706443,
2.05928071067701,2.07315419502193,2.07545386849614,2.07684132368472,2.07791861932185,
2.07913300412101,2.08121463403849,2.08970840087768,2.10612935253362,2.14859391205347,
2.17544941434954,2.17956641545037,2.18205546974822,2.1839878181852,2.18608350100494,
2.18943435217851,2.20067379356902,2.21934915538903,2.25535871683837,2.2845047971253,
2.28741809983126,2.28880643182995,2.28988114218869,2.29110904377492,2.29325179528874,
2.30255034156427,2.32140687507338,2.36918815777812,2.38807314822581,2.39182142641946,
2.39422593662769,2.39614288395535,2.39830691098425,2.40196645835302,2.41632806420291,
2.46677742008986,2.49647220492018,2.4993863770695,2.50077489989936,2.50184965515534,
2.50307749306043,2.50436930487639,2.50901370182217,2.53314924658976,2.55405337848608,
2.59909887046265,2.60335602728437,2.60588609608324,2.60782483170709,2.60990244605974,
2.61317125300074,2.6169746226263,2.62423948308767,2.6678681477495),
 .UNSPECIFIED.);
#1854=B_SPLINE_CURVE_WITH_KNOTS('',3,(#177848,#177849,#177850,#177851,#177852,
#177853,#177854,#177855,#177856,#177857,#177858,#177859,#177860,#177861,
#177862,#177863,#177864,#177865,#177866,#177867),.UNSPECIFIED.,.F.,.F.,
(4,2,2,2,2,2,2,2,2,4),(0.000649987072770544,0.0375152697013956,0.0412926013848847,
0.0433020282469795,0.0446072095719178,0.0458444128962429,0.0469177253289979,
0.0482917844166712,0.0511320530737365,0.0747588723678276),.UNSPECIFIED.);
#1855=B_SPLINE_CURVE_WITH_KNOTS('',3,(#177873,#177874,#177875,#177876,#177877,
#177878,#177879,#177880,#177881,#177882),.UNSPECIFIED.,.F.,.F.,(4,3,3,4),
(120.689857252469,120.859210445387,120.962579625196,121.040543944395),
 .UNSPECIFIED.);
#1856=B_SPLINE_CURVE_WITH_KNOTS('',3,(#177883,#177884,#177885,#177886,#177887,
#177888,#177889,#177890,#177891,#177892),.UNSPECIFIED.,.F.,.F.,(4,1,1,1,
1,1,1,4),(114.756144634991,114.866191745616,115.865028195577,116.863864645539,
117.862701095501,118.861537545463,119.860373995425,120.689851222995),
 .UNSPECIFIED.);
#1857=B_SPLINE_CURVE_WITH_KNOTS('',3,(#177893,#177894,#177895,#177896,#177897,
#177898,#177899,#177900,#177901,#177902,#177903,#177904,#177905,#177906,
#177907,#177908,#177909,#177910,#177911,#177912,#177913,#177914,#177915,
#177916,#177917,#177918,#177919,#177920,#177921,#177922,#177923,#177924,
#177925,#177926,#177927,#177928,#177929,#177930,#177931,#177932,#177933,
#177934,#177935,#177936,#177937,#177938,#177939,#177940,#177941,#177942,
#177943,#177944,#177945,#177946,#177947,#177948,#177949,#177950,#177951,
#177952,#177953,#177954,#177955,#177956,#177957,#177958,#177959,#177960,
#177961,#177962,#177963,#177964,#177965,#177966,#177967,#177968,#177969,
#177970,#177971,#177972,#177973,#177974,#177975,#177976,#177977,#177978,
#177979,#177980,#177981,#177982,#177983,#177984,#177985,#177986,#177987,
#177988,#177989,#177990,#177991,#177992,#177993,#177994,#177995,#177996,
#177997,#177998,#177999,#178000,#178001,#178002,#178003,#178004,#178005,
#178006,#178007,#178008,#178009,#178010,#178011,#178012,#178013,#178014,
#178015,#178016,#178017,#178018,#178019,#178020,#178021,#178022,#178023,
#178024,#178025,#178026,#178027,#178028,#178029,#178030,#178031,#178032,
#178033,#178034,#178035,#178036,#178037,#178038,#178039,#178040,#178041,
#178042,#178043,#178044,#178045,#178046,#178047,#178048,#178049,#178050,
#178051,#178052,#178053,#178054,#178055,#178056,#178057,#178058,#178059,
#178060,#178061,#178062,#178063,#178064,#178065,#178066,#178067,#178068,
#178069,#178070,#178071,#178072,#178073,#178074,#178075,#178076,#178077,
#178078,#178079,#178080,#178081,#178082,#178083,#178084,#178085,#178086,
#178087,#178088,#178089,#178090,#178091,#178092,#178093,#178094,#178095,
#178096,#178097,#178098,#178099,#178100,#178101,#178102,#178103,#178104,
#178105,#178106,#178107,#178108,#178109,#178110),.UNSPECIFIED.,.F.,.F.,
(4,2,2,2,2,2,2,2,2,2,2,2,2,2,2,2,2,2,2,2,2,2,2,2,2,2,2,2,2,2,2,2,2,2,2,
2,2,2,2,2,2,2,2,2,2,2,2,2,2,2,2,2,2,2,2,2,2,2,2,2,2,2,2,2,2,2,2,2,2,2,2,
2,2,2,2,2,2,2,2,2,2,2,2,2,2,2,2,2,2,2,2,2,2,2,2,2,2,2,2,2,2,2,2,2,2,2,2,
2,4),(0.0747588723678276,0.0879796870983175,0.109399101208918,0.13618200070148,
0.146436008192385,0.149706910345542,0.151785007961068,0.153723603728772,
0.156252645034177,0.160506226082512,0.193184719377548,0.222553895549607,
0.244173746486992,0.254295207460528,0.256485209434715,0.257733363566383,
0.258805364662574,0.260163818127456,0.262835836630906,0.28021576098978,
0.329253098414348,0.347302093622868,0.354571911865477,0.360001937435935,
0.36256736563645,0.364504735539526,0.366332872841691,0.368880746680496,
0.375561147398386,0.430980131140095,0.455321514737903,0.466218694672533,
0.468466988707819,0.469718090656642,0.47078984233517,0.472144414782186,
0.474886382538451,0.493336671015449,0.53746151312653,0.565332015013005,
0.571665398652692,0.574357014768523,0.576315572444477,0.578111714706853,
0.580996281507104,0.58800006481441,0.639382577525078,0.666515101842847,
0.678128410237519,0.680418185136889,0.681678330270937,0.68274933451004,
0.684092180670403,0.686691242532328,0.702216224453772,0.708761609068164,
0.722633933763404,0.755493995474727,0.772056493671663,0.782367915966502,
0.785616719921701,0.787690101784928,0.789630836549942,0.792172081959859,
0.79646723740172,0.831578360720192,0.880465480908942,0.89028867255224,0.892468531051077,
0.893704762858457,0.894778464033976,0.896154628445178,0.899004756030601,
0.93537470931285,0.989163092423328,0.995619144932156,0.998331712584215,
1.00029420667142,1.00208618009099,1.00494710651599,1.01180638634181,1.0652449889484,
1.09093524626958,1.10218664638406,1.10445606410749,1.10571187269424,1.10678335725249,
1.10813211021972,1.1107581751194,1.12692235755853,1.17758035248144,1.20199434245457,
1.20789436377431,1.21051042826656,1.21245612656223,1.21427052293804,1.21676513158997,
1.22311497510759,1.28150396882532,1.30395462441549,1.31433184317185,1.31654824759285,
1.31779253336388,1.31886525744178,1.32022985175578,1.32240326195016,1.33389996509002,
1.38263557238681,1.40832430342818),.UNSPECIFIED.);
#1858=B_SPLINE_CURVE_WITH_KNOTS('',3,(#178116,#178117,#178118,#178119,#178120,
#178121,#178122,#178123),.UNSPECIFIED.,.F.,.F.,(4,2,2,4),(2.59362475265785,
2.59837330782392,2.62640672493038,2.66809195083791),.UNSPECIFIED.);
#1859=B_SPLINE_CURVE_WITH_KNOTS('',3,(#178124,#178125,#178126,#178127,#178128,
#178129,#178130,#178131,#178132,#178133,#178134,#178135,#178136,#178137,
#178138,#178139,#178140,#178141,#178142,#178143,#178144,#178145,#178146,
#178147,#178148,#178149,#178150,#178151,#178152,#178153,#178154,#178155,
#178156,#178157,#178158,#178159,#178160,#178161,#178162,#178163,#178164,
#178165,#178166,#178167,#178168,#178169,#178170,#178171,#178172,#178173,
#178174,#178175,#178176,#178177,#178178,#178179,#178180,#178181,#178182,
#178183,#178184,#178185,#178186,#178187,#178188,#178189,#178190,#178191,
#178192,#178193,#178194,#178195,#178196,#178197,#178198,#178199,#178200,
#178201,#178202,#178203,#178204,#178205,#178206,#178207,#178208,#178209,
#178210,#178211,#178212,#178213,#178214,#178215,#178216,#178217,#178218,
#178219,#178220,#178221,#178222,#178223,#178224,#178225,#178226,#178227,
#178228,#178229,#178230,#178231,#178232,#178233,#178234,#178235,#178236,
#178237,#178238,#178239,#178240,#178241,#178242,#178243,#178244,#178245,
#178246,#178247,#178248,#178249,#178250,#178251,#178252,#178253,#178254,
#178255,#178256,#178257,#178258,#178259,#178260,#178261,#178262,#178263,
#178264,#178265,#178266,#178267,#178268,#178269,#178270,#178271,#178272,
#178273,#178274,#178275,#178276,#178277,#178278,#178279,#178280,#178281,
#178282,#178283,#178284,#178285,#178286,#178287,#178288,#178289,#178290,
#178291,#178292,#178293,#178294,#178295,#178296,#178297,#178298,#178299,
#178300,#178301),.UNSPECIFIED.,.F.,.F.,(4,3,3,3,3,3,3,3,3,3,3,3,3,3,3,3,
3,3,3,3,3,3,3,3,3,3,3,3,3,3,3,3,3,3,3,3,3,3,3,3,3,3,3,3,3,3,3,3,3,3,3,3,
3,3,3,3,3,3,3,4),(121.040543944395,121.143685152638,121.246752606079,121.349780357811,
121.452802409466,121.555926033343,121.659098496058,121.762462007832,121.858046895349,
121.961441632397,122.064682914512,122.167802879905,122.270857448114,122.373880656472,
122.476906499145,122.580039265923,122.683228357333,122.786600350715,122.856883345311,
122.960278082359,123.063519364473,123.166639329865,123.269693898074,123.372717106431,
123.475742949104,123.578875715882,123.682064807291,123.785436800672,123.855719795272,
123.95911453232,124.062355814435,124.165475779827,124.268530348036,124.371553556393,
124.474579399066,124.577712165844,124.680901257254,124.784273250635,124.854556245234,
124.957950982282,125.061192264397,125.16431222979,125.267366797999,125.370390006357,
125.47341584903,125.576548615808,125.679737707218,125.7831097006,125.853392695196,
125.956787432244,126.060028714359,126.163148679751,126.26620324796,126.369226456318,
126.472252298991,126.575385065769,126.678574157178,126.78194615056,126.852229145158,
126.973042559648),.UNSPECIFIED.);
#1860=B_SPLINE_CURVE_WITH_KNOTS('',3,(#178303,#178304,#178305,#178306,#178307,
#178308,#178309,#178310,#178311,#178312,#178313,#178314,#178315,#178316,
#178317,#178318,#178319,#178320,#178321,#178322,#178323,#178324,#178325,
#178326,#178327,#178328,#178329,#178330,#178331,#178332,#178333,#178334,
#178335,#178336,#178337,#178338,#178339,#178340,#178341,#178342,#178343,
#178344,#178345,#178346,#178347,#178348,#178349,#178350,#178351,#178352,
#178353,#178354,#178355,#178356,#178357,#178358,#178359,#178360,#178361,
#178362,#178363,#178364,#178365,#178366,#178367,#178368,#178369,#178370,
#178371,#178372,#178373,#178374,#178375,#178376,#178377,#178378,#178379,
#178380,#178381,#178382,#178383,#178384,#178385,#178386,#178387,#178388,
#178389,#178390,#178391,#178392,#178393,#178394,#178395,#178396,#178397,
#178398,#178399,#178400,#178401,#178402,#178403,#178404,#178405,#178406,
#178407,#178408,#178409,#178410,#178411,#178412,#178413,#178414,#178415,
#178416,#178417,#178418,#178419,#178420,#178421,#178422,#178423,#178424,
#178425,#178426,#178427,#178428,#178429,#178430,#178431,#178432,#178433,
#178434,#178435,#178436,#178437,#178438,#178439,#178440,#178441,#178442,
#178443,#178444,#178445,#178446,#178447,#178448,#178449,#178450,#178451,
#178452,#178453,#178454,#178455,#178456,#178457,#178458,#178459,#178460,
#178461,#178462,#178463,#178464,#178465,#178466,#178467,#178468,#178469,
#178470,#178471,#178472,#178473,#178474,#178475,#178476,#178477,#178478,
#178479,#178480,#178481,#178482,#178483,#178484,#178485,#178486,#178487,
#178488,#178489,#178490,#178491,#178492,#178493,#178494,#178495,#178496,
#178497,#178498,#178499,#178500,#178501,#178502,#178503,#178504,#178505,
#178506,#178507,#178508,#178509,#178510,#178511,#178512,#178513,#178514,
#178515,#178516,#178517,#178518,#178519,#178520),.UNSPECIFIED.,.F.,.F.,
(4,2,2,2,2,2,2,2,2,2,2,2,2,2,2,2,2,2,2,2,2,2,2,2,2,2,2,2,2,2,2,2,2,2,2,
2,2,2,2,2,2,2,2,2,2,2,2,2,2,2,2,2,2,2,2,2,2,2,2,2,2,2,2,2,2,2,2,2,2,2,2,
2,2,2,2,2,2,2,2,2,2,2,2,2,2,2,2,2,2,2,2,2,2,2,2,2,2,2,2,2,2,2,2,2,2,2,2,
2,4),(1.40832430342818,1.41583884775361,1.42010270180147,1.42263499298702,
1.42457441334773,1.42665176850529,1.42991807905246,1.4403811399291,1.45728209141941,
1.49511037311192,1.5251859935497,1.52810058477316,1.52948936141789,1.53056433804064,
1.5317924566932,1.53393538295632,1.54323153886664,1.56207808036235,1.60247855626088,
1.61474065051465,1.62934649672079,1.633134775163,1.6353497648843,1.63726202411854,
1.63959705367887,1.6440469755749,1.67495966545922,1.72180620623172,1.73760405655992,
1.74021654151974,1.74156242637286,1.74263379570719,1.74389198546095,1.74617210055741,
1.75760866774367,1.78402402434625,1.83638785826709,1.84332628653457,1.84620036353465,
1.84799482292824,1.84995543205559,1.85265695163944,1.85904680944289,1.8873851252852,
1.93728518809846,1.94991467480724,1.9521509073944,1.95353452565234,1.95460903332621,
1.95584057180149,1.95799878626154,1.9675076620991,2.0166420977235,2.0518281950266,
2.05612455429066,2.05866631607403,2.0606073214597,2.06268087157703,2.06592968561963,
2.07623891824444,2.09279809288288,2.12568565576995,2.13955224267007,2.14611373514652,
2.16166408012244,2.16426452422766,2.16560776704704,2.16667891902104,2.16793904706968,
2.17022829108759,2.18182886955132,2.20890471931824,2.26033650400616,2.26733516463324,
2.2702191034823,2.2720152946656,2.27397426243379,2.2766670833449,2.28300627268811,
2.31092526152792,2.35694144007021,2.35793644658125,2.37366886787483,2.37627707080484,
2.37762198667344,2.37869323812628,2.3799520485334,2.38223522731371,2.39372765743041,
2.42036726017418,2.47238397040264,2.4793619331355,2.48224243562505,2.48403799251657,
2.48585857696639,2.48841312006702,2.49401415860211,2.5015383928661,2.52051152887596,
2.54851967678728,2.58534455777052,2.58818633431194,2.58956083432058,2.59063435158216,
2.59187164123774,2.59405640205728,2.6039529815351,2.65275133922535,2.66750913583394),
 .UNSPECIFIED.);
#1861=B_SPLINE_CURVE_WITH_KNOTS('',3,(#178521,#178522,#178523,#178524,#178525,
#178526,#178527,#178528,#178529,#178530,#178531,#178532,#178533,#178534,
#178535,#178536,#178537,#178538,#178539,#178540,#178541,#178542),
 .UNSPECIFIED.,.F.,.F.,(4,2,2,2,2,2,2,2,2,2,4),(0.000768648173035884,0.0217309694116398,
0.024834106463169,0.0269704254108821,0.0287696705621352,0.0306848619248692,
0.0330687977058306,0.0367500448424231,0.0545887128832821,0.0729754669855961,
0.0751664112996189),.UNSPECIFIED.);
#1862=B_SPLINE_CURVE_WITH_KNOTS('',3,(#178547,#178548,#178549,#178550,#178551,
#178552,#178553,#178554,#178555,#178556,#178557,#178558,#178559,#178560,
#178561,#178562,#178563,#178564,#178565,#178566,#178567,#178568,#178569,
#178570,#178571,#178572,#178573,#178574,#178575,#178576,#178577,#178578,
#178579,#178580,#178581,#178582,#178583,#178584,#178585,#178586,#178587,
#178588,#178589,#178590,#178591,#178592,#178593,#178594,#178595,#178596,
#178597,#178598,#178599,#178600,#178601,#178602,#178603,#178604,#178605,
#178606,#178607,#178608,#178609,#178610,#178611,#178612,#178613,#178614,
#178615,#178616,#178617,#178618,#178619,#178620,#178621,#178622,#178623,
#178624,#178625,#178626,#178627,#178628,#178629,#178630,#178631,#178632,
#178633,#178634,#178635,#178636,#178637,#178638,#178639,#178640,#178641,
#178642,#178643,#178644,#178645,#178646,#178647,#178648,#178649,#178650,
#178651,#178652,#178653,#178654,#178655,#178656,#178657,#178658,#178659,
#178660,#178661,#178662,#178663,#178664,#178665,#178666,#178667,#178668,
#178669,#178670,#178671,#178672,#178673,#178674,#178675,#178676,#178677,
#178678,#178679,#178680,#178681,#178682,#178683,#178684,#178685,#178686,
#178687,#178688,#178689,#178690,#178691,#178692,#178693,#178694,#178695,
#178696,#178697,#178698,#178699,#178700,#178701,#178702,#178703,#178704,
#178705,#178706,#178707,#178708,#178709,#178710,#178711,#178712,#178713,
#178714,#178715,#178716,#178717,#178718,#178719,#178720,#178721,#178722,
#178723,#178724,#178725,#178726,#178727,#178728,#178729,#178730,#178731,
#178732,#178733,#178734,#178735,#178736,#178737,#178738,#178739,#178740,
#178741,#178742,#178743,#178744,#178745,#178746,#178747,#178748,#178749,
#178750,#178751,#178752,#178753,#178754,#178755,#178756,#178757,#178758,
#178759,#178760,#178761,#178762,#178763,#178764,#178765,#178766,#178767,
#178768,#178769,#178770,#178771,#178772,#178773,#178774,#178775,#178776,
#178777,#178778),.UNSPECIFIED.,.F.,.F.,(4,2,2,2,2,2,2,2,2,2,2,2,2,2,2,2,
2,2,2,2,2,2,2,2,2,2,2,2,2,2,2,2,2,2,2,2,2,2,2,2,2,2,2,2,2,2,2,2,2,2,2,2,
2,2,2,2,2,2,2,2,2,2,2,2,2,2,2,2,2,2,2,2,2,2,2,2,2,2,2,2,2,2,2,2,2,2,2,2,
2,2,2,2,2,2,2,2,2,2,2,2,2,2,2,2,2,2,2,2,2,2,2,2,2,2,2,4),(1.25995284018407,
1.27815533267849,1.30765697349692,1.31206706936864,1.31439383091612,1.31612079616701,
1.31827707165333,1.32189964021149,1.33434948216398,1.38530655022404,1.41651402911594,
1.41942699928209,1.42081555372547,1.42189061163399,1.42311910645899,1.42526335265726,
1.43457548440155,1.48373090332537,1.5191186820702,1.52341772045822,1.52596031999528,
1.52790153498849,1.5299748921498,1.53322253386872,1.54352072105679,1.56005519322258,
1.59292311329251,1.60444895088282,1.61420015696443,1.61610257435304,1.62916930768846,
1.63142803064148,1.63281839164975,1.6338935711981,1.6351207785474,1.63725944359352,
1.64649611756226,1.665155557615,1.70929886538824,1.73174157288586,1.73568379926241,
1.73814776146543,1.74007158146695,1.74220153389174,1.74570551189524,1.75848205950185,
1.78092536766237,1.80819133767747,1.84051393284874,1.84341562564243,1.84480190532759,
1.84587663413865,1.84710635726372,1.84925651592167,1.85865301629504,1.90788222371777,
1.94309504594036,1.94739154272531,1.94993327551323,1.95187419521534,1.95394759220047,
1.95719603772935,1.96750301755928,1.9840575435563,2.0169402232118,2.05257689975077,
2.05544010149944,2.05681883306758,2.05789277623411,2.0591273087319,2.0612994304239,
2.07100980878776,2.11996641100843,2.15509560822262,2.15939088810079,2.16193222222516,
2.16387302250177,2.16594647128081,2.16919537246461,2.17950695458013,2.19607187559424,
2.2289625194241,2.26456745940368,2.26743324883355,2.26881245849163,2.26988641435369,
2.27112055597793,2.27329102320292,2.28297817945522,2.33195248070879,2.36708663309277,
2.37138184122927,2.37392310835603,2.37586384332775,2.37793720862947,2.38118595038636,
2.39149678517998,2.40806027606265,2.47069227330701,2.47205345242812,2.47822624636479,
2.48016435853052,2.48134700118584,2.48237852780508,2.48379140889466,2.48680603945378,
2.4909036416418,2.50118056489532,2.52399975601406,2.57570490377446,2.58268778886798,
2.58556926597903,2.58736511868518,2.58932467119699,2.59202003277444,2.59362475265785),
 .UNSPECIFIED.);
#1863=B_SPLINE_CURVE_WITH_KNOTS('',3,(#178779,#178780,#178781,#178782,#178783,
#178784,#178785,#178786,#178787,#178788,#178789,#178790,#178791,#178792,
#178793,#178794,#178795,#178796,#178797,#178798,#178799,#178800,#178801,
#178802,#178803,#178804,#178805,#178806,#178807,#178808,#178809,#178810,
#178811,#178812,#178813,#178814,#178815,#178816,#178817,#178818,#178819,
#178820,#178821,#178822,#178823,#178824,#178825,#178826,#178827,#178828,
#178829,#178830,#178831,#178832,#178833,#178834,#178835,#178836,#178837,
#178838,#178839,#178840,#178841,#178842,#178843,#178844,#178845,#178846,
#178847,#178848,#178849,#178850,#178851,#178852,#178853,#178854,#178855,
#178856,#178857,#178858,#178859,#178860,#178861,#178862,#178863,#178864,
#178865,#178866,#178867,#178868,#178869,#178870,#178871,#178872,#178873,
#178874,#178875,#178876,#178877,#178878,#178879,#178880,#178881,#178882,
#178883,#178884,#178885,#178886,#178887,#178888,#178889,#178890,#178891,
#178892,#178893,#178894,#178895,#178896,#178897,#178898,#178899,#178900,
#178901,#178902,#178903,#178904,#178905,#178906,#178907,#178908,#178909,
#178910,#178911,#178912,#178913,#178914,#178915,#178916,#178917,#178918,
#178919,#178920,#178921,#178922,#178923,#178924,#178925,#178926,#178927,
#178928,#178929,#178930,#178931,#178932,#178933,#178934,#178935,#178936,
#178937,#178938,#178939,#178940,#178941,#178942,#178943,#178944,#178945,
#178946,#178947,#178948,#178949,#178950,#178951,#178952,#178953,#178954,
#178955,#178956,#178957,#178958,#178959,#178960,#178961,#178962,#178963,
#178964,#178965,#178966,#178967,#178968,#178969,#178970,#178971,#178972,
#178973,#178974,#178975,#178976,#178977,#178978,#178979,#178980,#178981,
#178982,#178983,#178984,#178985,#178986,#178987,#178988,#178989,#178990,
#178991,#178992,#178993,#178994,#178995,#178996,#178997,#178998,#178999,
#179000,#179001,#179002,#179003,#179004,#179005,#179006,#179007,#179008,
#179009,#179010,#179011,#179012),.UNSPECIFIED.,.F.,.F.,(4,2,2,2,2,2,2,2,
2,2,2,2,2,2,2,2,2,2,2,2,2,2,2,2,2,2,2,2,2,2,2,2,2,2,2,2,2,2,2,2,2,2,2,2,
2,2,2,2,2,2,2,2,2,2,2,2,2,2,2,2,2,2,2,2,2,2,2,2,2,2,2,2,2,2,2,2,2,2,2,2,
2,2,2,2,2,2,2,2,2,2,2,2,2,2,2,2,2,2,2,2,2,2,2,2,2,2,2,2,2,2,2,2,2,2,2,2,
4),(0.0751664112996189,0.121836951464716,0.131681142658904,0.133862213611629,
0.135098605469386,0.136172108887128,0.137547580294155,0.14039476577867,
0.176868086307239,0.2094289106163,0.225633610738257,0.232378429874515,0.237517855736887,
0.239980375628617,0.241821624375069,0.24364900313207,0.246193616401099,
0.252852140385327,0.308506881526599,0.332697523544293,0.343554680832648,
0.345800707706044,0.347051384853921,0.348123287830775,0.349478711949654,
0.351622237597027,0.362626672188654,0.413890619380091,0.442557303123207,
0.448986537823899,0.451694527804662,0.453656137297877,0.455448972236416,
0.458314902646815,0.46520498464097,0.518242956848075,0.544209029002317,
0.555530797239845,0.557804212089946,0.559060861729059,0.560132231379342,
0.561479779883051,0.564100380196642,0.580124489072943,0.585201163504066,
0.629881790974561,0.648403612356206,0.659578923632395,0.662923321289518,
0.665017807074267,0.666950981328522,0.669443797604298,0.67357288603625,
0.700868461682789,0.74311955698701,0.759406575996171,0.767853917475503,
0.769932099700476,0.771145854515035,0.77222353355997,0.773612688327964,
0.775917681979813,0.78992994807999,0.791300118797791,0.798313753017245,
0.811988337896586,0.844849351005156,0.861410889239503,0.871722134906194,
0.874971107247304,0.877044650403876,0.878985573955134,0.881527121121702,
0.885822908864002,0.920955317153874,0.969901905753939,0.979660705440998,
0.98183631026648,0.983071676473829,0.984145615712196,0.98552337908981,0.988381266748878,
1.01124170619927,1.02400669700314,1.05686244962613,1.07341519158678,1.0837227575136,
1.08697152696743,1.08904517055803,1.09098634964885,1.09352846452316,1.09782573434743,
1.13304047916014,1.18224589934266,1.19170985783632,1.1938650800132,1.19509604121575,
1.19617078239087,1.19755566047973,1.19979579975946,1.21249724873201,1.23487540300981,
1.2684790562292,1.2938562858841,1.29812699327806,1.30042452759205,1.30231760049,
1.30455834645752,1.3084575115031,1.32436621650597,1.3345884751666,1.37387287669931,
1.40245709623738,1.40536965373442,1.40675820520218,1.40783335001672,1.40876523686012),
 .UNSPECIFIED.);
#1864=B_SPLINE_CURVE_WITH_KNOTS('',3,(#179018,#179019,#179020,#179021,#179022,
#179023,#179024,#179025,#179026,#179027,#179028,#179029,#179030,#179031,
#179032,#179033,#179034,#179035,#179036,#179037,#179038,#179039),
 .UNSPECIFIED.,.F.,.F.,(4,2,2,2,2,2,2,2,2,2,4),(2.5930073351113,2.59655707612435,
2.60120237925256,2.60293217092639,2.60395546436,2.6050492651463,2.60656781487107,
2.61019870485997,2.6153096210448,2.62947688779406,2.66710874015144),
 .UNSPECIFIED.);
#1865=B_SPLINE_CURVE_WITH_KNOTS('',3,(#179040,#179041,#179042,#179043,#179044,
#179045,#179046,#179047,#179048,#179049,#179050,#179051,#179052,#179053,
#179054,#179055,#179056,#179057,#179058,#179059,#179060,#179061,#179062,
#179063,#179064,#179065,#179066,#179067,#179068,#179069,#179070,#179071,
#179072,#179073,#179074,#179075,#179076,#179077,#179078,#179079,#179080,
#179081,#179082,#179083,#179084,#179085,#179086,#179087,#179088,#179089,
#179090,#179091,#179092,#179093,#179094,#179095,#179096,#179097,#179098,
#179099,#179100,#179101,#179102,#179103,#179104,#179105,#179106,#179107,
#179108,#179109,#179110,#179111,#179112,#179113,#179114,#179115,#179116,
#179117,#179118,#179119,#179120,#179121,#179122,#179123,#179124,#179125,
#179126,#179127,#179128,#179129,#179130,#179131,#179132,#179133,#179134,
#179135,#179136,#179137,#179138,#179139,#179140,#179141,#179142,#179143,
#179144,#179145,#179146,#179147,#179148,#179149,#179150,#179151,#179152,
#179153,#179154,#179155,#179156,#179157,#179158,#179159,#179160,#179161,
#179162,#179163,#179164,#179165,#179166,#179167,#179168,#179169,#179170,
#179171,#179172,#179173,#179174,#179175,#179176,#179177,#179178,#179179,
#179180,#179181,#179182,#179183,#179184,#179185,#179186,#179187,#179188,
#179189,#179190,#179191,#179192,#179193,#179194,#179195,#179196,#179197,
#179198,#179199,#179200,#179201,#179202,#179203,#179204,#179205,#179206,
#179207,#179208,#179209,#179210,#179211,#179212,#179213,#179214,#179215,
#179216,#179217,#179218,#179219,#179220,#179221,#179222,#179223,#179224,
#179225,#179226,#179227,#179228,#179229,#179230,#179231,#179232,#179233,
#179234,#179235,#179236,#179237,#179238,#179239,#179240,#179241,#179242,
#179243,#179244,#179245,#179246,#179247,#179248,#179249,#179250,#179251,
#179252,#179253,#179254,#179255,#179256,#179257,#179258,#179259,#179260,
#179261,#179262,#179263),.UNSPECIFIED.,.F.,.F.,(4,2,2,2,2,2,2,2,2,2,2,2,
2,2,2,2,2,2,2,2,2,2,2,2,2,2,2,2,2,2,2,2,2,2,2,2,2,2,2,2,2,2,2,2,2,2,2,2,
2,2,2,2,2,2,2,2,2,2,2,2,2,2,2,2,2,2,2,2,2,2,2,2,2,2,2,2,2,2,2,2,2,2,2,2,
2,2,2,2,2,2,2,2,2,2,2,2,2,2,2,2,2,2,2,2,2,2,2,2,2,2,2,4),(0.000704174783266484,
0.0257175604482853,0.0359848121210841,0.0390635446877278,0.0411898447752388,
0.0432709978131024,0.0452083577367602,0.0477299553379147,0.0519581062662032,
0.0833496643500498,0.108683991109725,0.136591220283264,0.145906684913021,
0.148050668850133,0.149278836543247,0.150353498249269,0.151741385255173,
0.154652423469552,0.186428100892679,0.237019928806342,0.245245998359551,
0.251260637921565,0.253888587904228,0.255845177211792,0.257643302003301,
0.260539405344161,0.267613575549391,0.317990518515176,0.355630100276971,
0.359217020733819,0.360727971305265,0.361820314740776,0.362845441579523,
0.364585128297621,0.369296593408011,0.409885702767462,0.456766765021495,
0.463159531935094,0.465861115581181,0.467821348318664,0.469615175354509,
0.472487599269587,0.479418712975679,0.53187624579876,0.55823965171709,0.569661293388527,
0.571940169362427,0.573197891653986,0.574268997283979,0.575614715574956,
0.578227361376873,0.594085310341687,0.598886501397849,0.614100754358038,
0.646973648978801,0.663553423044398,0.673872438409335,0.677121953267134,
0.679195385113979,0.681135883172054,0.683676409714467,0.6879694338944,0.730360837973206,
0.75940491758315,0.774136636136039,0.782031822114532,0.784063874694209,
0.785267280880008,0.786347264976097,0.78775444750052,0.790121315900346,
0.805548432964546,0.812282711181535,0.826072038655682,0.858930118198779,
0.87549101521074,0.885801617049223,0.88905025645457,0.891123555881361,0.893064229345933,
0.895605417375026,0.899900527140571,0.935018038083059,0.983926479072149,
0.993721999751709,0.995899923745845,0.997135704694492,0.99820942740478,
0.999586159067221,1.00243931456665,1.02512119130855,1.03806228554941,1.0709155347101,
1.08746815996987,1.09777531880078,1.10102378197149,1.10309718729489,1.10503811329192,
1.10757985336449,1.11187639242141,1.14707193209009,1.19622157390507,1.20574153761124,
1.20790053021267,1.20913222685479,1.2102066928978,1.21159001138132,1.2138252679769,
1.22643731494536,1.23296338685451,1.2380952997305,1.25995284018407),
 .UNSPECIFIED.);
#1866=B_SPLINE_CURVE_WITH_KNOTS('',3,(#179265,#179266,#179267,#179268,#179269,
#179270,#179271,#179272,#179273,#179274,#179275,#179276,#179277,#179278,
#179279,#179280,#179281,#179282,#179283,#179284,#179285,#179286,#179287,
#179288,#179289,#179290,#179291,#179292,#179293,#179294,#179295,#179296,
#179297,#179298,#179299,#179300,#179301,#179302,#179303,#179304,#179305,
#179306,#179307,#179308,#179309,#179310,#179311,#179312,#179313,#179314,
#179315,#179316,#179317,#179318,#179319,#179320,#179321,#179322,#179323,
#179324,#179325,#179326,#179327,#179328,#179329,#179330,#179331,#179332,
#179333,#179334,#179335,#179336,#179337,#179338,#179339,#179340,#179341,
#179342,#179343,#179344,#179345,#179346,#179347,#179348,#179349,#179350,
#179351,#179352,#179353,#179354,#179355,#179356,#179357,#179358,#179359,
#179360,#179361,#179362,#179363,#179364,#179365,#179366,#179367,#179368,
#179369,#179370,#179371,#179372,#179373,#179374,#179375,#179376,#179377,
#179378,#179379,#179380,#179381,#179382,#179383,#179384,#179385,#179386,
#179387,#179388,#179389,#179390,#179391,#179392,#179393,#179394,#179395,
#179396,#179397,#179398,#179399,#179400,#179401,#179402,#179403,#179404,
#179405,#179406,#179407,#179408,#179409,#179410,#179411,#179412,#179413,
#179414,#179415,#179416,#179417,#179418,#179419,#179420,#179421,#179422,
#179423,#179424,#179425,#179426,#179427,#179428,#179429,#179430,#179431,
#179432,#179433,#179434,#179435,#179436,#179437,#179438,#179439,#179440,
#179441,#179442,#179443,#179444,#179445,#179446,#179447,#179448,#179449,
#179450,#179451,#179452,#179453,#179454,#179455,#179456,#179457,#179458,
#179459,#179460,#179461,#179462,#179463,#179464,#179465,#179466,#179467,
#179468,#179469,#179470,#179471,#179472,#179473,#179474,#179475,#179476,
#179477,#179478,#179479,#179480,#179481,#179482,#179483,#179484,#179485,
#179486,#179487,#179488,#179489,#179490,#179491,#179492,#179493,#179494,
#179495,#179496,#179497,#179498,#179499,#179500,#179501,#179502,#179503,
#179504,#179505,#179506,#179507,#179508,#179509,#179510,#179511,#179512,
#179513,#179514,#179515,#179516,#179517,#179518,#179519,#179520),
 .UNSPECIFIED.,.F.,.F.,(4,2,2,2,2,2,2,2,2,2,2,2,2,2,2,2,2,2,2,2,2,2,2,2,
2,2,2,2,2,2,2,2,2,2,2,2,2,2,2,2,2,2,2,2,2,2,2,2,2,2,2,2,2,2,2,2,2,2,2,2,
2,2,2,2,2,2,2,2,2,2,2,2,2,2,2,2,2,2,2,2,2,2,2,2,2,2,2,2,2,2,2,2,2,2,2,2,
2,2,2,2,2,2,2,2,2,2,2,2,2,2,2,2,2,2,2,2,2,2,2,2,2,2,2,2,2,2,2,4),(1.40876523686012,
1.40906204393765,1.41120687144366,1.42052514418392,1.46970161844819,1.50507081289879,
1.50936999286094,1.51191275499292,1.51385413951598,1.51592772173571,1.51917580776507,
1.52947617622816,1.54601488419058,1.57356168633321,1.58970408754065,1.60078465259348,
1.6150205401593,1.6173371712821,1.6187298593166,1.61980813782155,1.62102018173609,
1.62309009026263,1.6314324540752,1.6474136860404,1.68972792942271,1.71734566106792,
1.72148338727517,1.72397897743458,1.72591284550596,1.72800662795603,1.73134675056564,
1.74247827516818,1.76089964199186,1.80770817811134,1.81253297817898,1.82701627756262,
1.82934425026303,1.83074028129115,1.83181901714088,1.83302919573545,1.83509063606512,
1.84332931772284,1.85901491237136,1.90092755750791,1.92932631736605,1.93348475129867,
1.9359864464662,1.93792127381585,1.94001234369268,1.94334004829138,1.95435551753042,
1.97250823563918,2.02218424317245,2.02373330487373,2.02563794733054,2.03913289798561,
2.04141316979618,2.04279519462395,2.04387218595884,2.04509064120281,2.04718924198271,
2.05589101581214,2.07291936302207,2.11593620512401,2.1282171496421,2.14272193700362,
2.14650164868605,2.14871489652755,2.15062763117179,2.1529657335204,2.1574291941509,
2.18882831143217,2.23938702440558,2.25132987941368,2.25352918546455,2.25490178413962,
2.25597541182666,2.25721463742382,2.25940718010277,2.26941316893368,2.31813785790198,
2.35319435175552,2.3574897097279,2.36003142069175,2.36197269920623,2.36404684359362,
2.36729722041653,2.37761673872991,2.39419750467077,2.4279021680599,2.46267411909094,
2.46555349924636,2.46693559163019,2.46797846857451,2.46798322666971,2.46798790131232,
2.46799249431981,2.46799700757368,2.46800144279414,2.46800580147029,2.4680100855505,
2.46801429655875,2.46801843592317,2.46802250542493,2.46802650641665,2.46803044037086,
2.46803430867444,2.46803790597397,2.4680414897071,2.46804506013325,2.4680486173852,
2.46805216134702,2.4692761030427,2.47058782654189,2.4726125604927,2.4764297583911,
2.48571877521554,2.52371378071088,2.53834977058261,2.5655065850755,2.56963265583248,
2.5721249092442,2.57405838426332,2.57615393187958,2.57950162033336,2.59070276111532,
2.60928557013674,2.66833801738852),.UNSPECIFIED.);
#1867=B_SPLINE_CURVE_WITH_KNOTS('',3,(#179521,#179522,#179523,#179524,#179525,
#179526,#179527,#179528,#179529,#179530,#179531,#179532,#179533,#179534,
#179535,#179536,#179537,#179538,#179539,#179540,#179541,#179542),
 .UNSPECIFIED.,.F.,.F.,(4,2,2,2,2,2,2,2,2,2,4),(0.000810717437210857,0.00554260819479371,
0.00881068906929704,0.0102445691543466,0.0113189779225148,0.0123417943062969,
0.013364996033305,0.0148060118696489,0.0186526098088544,0.02639099987356,
0.0750462537154924),.UNSPECIFIED.);
#1868=B_SPLINE_CURVE_WITH_KNOTS('',3,(#179547,#179548,#179549,#179550,#179551,
#179552,#179553,#179554,#179555,#179556,#179557,#179558,#179559,#179560,
#179561,#179562,#179563,#179564,#179565,#179566,#179567,#179568,#179569,
#179570,#179571,#179572,#179573,#179574,#179575,#179576,#179577,#179578,
#179579,#179580,#179581,#179582,#179583,#179584,#179585,#179586,#179587,
#179588,#179589,#179590,#179591,#179592,#179593,#179594,#179595,#179596,
#179597,#179598,#179599,#179600,#179601,#179602,#179603,#179604,#179605,
#179606,#179607,#179608,#179609,#179610,#179611,#179612,#179613,#179614,
#179615,#179616,#179617,#179618,#179619,#179620,#179621,#179622,#179623,
#179624,#179625,#179626,#179627,#179628,#179629,#179630,#179631,#179632,
#179633,#179634,#179635,#179636,#179637,#179638,#179639,#179640,#179641,
#179642,#179643,#179644,#179645,#179646,#179647,#179648,#179649,#179650,
#179651,#179652,#179653,#179654,#179655,#179656,#179657,#179658,#179659,
#179660,#179661,#179662,#179663,#179664,#179665,#179666,#179667,#179668,
#179669,#179670,#179671,#179672,#179673,#179674,#179675,#179676,#179677,
#179678,#179679,#179680,#179681,#179682,#179683,#179684,#179685,#179686,
#179687,#179688,#179689,#179690,#179691,#179692,#179693,#179694,#179695,
#179696,#179697,#179698,#179699,#179700,#179701,#179702,#179703,#179704,
#179705,#179706,#179707,#179708,#179709,#179710,#179711,#179712,#179713,
#179714,#179715,#179716,#179717,#179718,#179719,#179720,#179721,#179722,
#179723,#179724,#179725,#179726,#179727,#179728,#179729,#179730,#179731,
#179732,#179733,#179734,#179735,#179736,#179737,#179738,#179739,#179740,
#179741,#179742,#179743,#179744,#179745,#179746,#179747,#179748,#179749,
#179750,#179751,#179752,#179753,#179754,#179755,#179756,#179757,#179758,
#179759,#179760,#179761,#179762,#179763,#179764,#179765,#179766,#179767,
#179768,#179769,#179770,#179771,#179772,#179773,#179774,#179775,#179776),
 .UNSPECIFIED.,.F.,.F.,(4,2,2,2,2,2,2,2,2,2,2,2,2,2,2,2,2,2,2,2,2,2,2,2,
2,2,2,2,2,2,2,2,2,2,2,2,2,2,2,2,2,2,2,2,2,2,2,2,2,2,2,2,2,2,2,2,2,2,2,2,
2,2,2,2,2,2,2,2,2,2,2,2,2,2,2,2,2,2,2,2,2,2,2,2,2,2,2,2,2,2,2,2,2,2,2,2,
2,2,2,2,2,2,2,2,2,2,2,2,2,2,2,2,2,2,4),(1.25952994513294,1.26421488598236,
1.30515481544145,1.32763223119784,1.33029538162279,1.33163408266925,1.33260195983659,
1.33382544749752,1.33594775047286,1.34496553108,1.36294881533076,1.41315940227977,
1.4309613348525,1.43464041070228,1.43702379248317,1.43893908622121,1.44111762204123,
1.44484207719109,1.46024701804637,1.51157709626072,1.53925268004026,1.54215933447374,
1.54354650258749,1.54462123616883,1.54585019886904,1.54799722878005,1.55735197908928,
1.60661243391117,1.64183221861147,1.64612844434328,1.64866997749064,1.6506107221197,
1.65268391015098,1.65593198252428,1.66623739265292,1.68278903068098,1.71566752358765,
1.72911330028546,1.736696610636,1.75169296612739,1.75404224757913,1.75544430252706,
1.75652358368923,1.75772980714153,1.75977446645524,1.76781718180068,1.78295449543262,
1.82265124657729,1.8538880913086,1.85811304970662,1.86063381774351,1.86257115604171,
1.8646528892407,1.86794005869551,1.87859162512038,1.89591648917634,1.94411119254616,
1.9484064128245,1.95083887569047,1.96382573538939,1.96608014904842,1.96746910199456,
1.9685439839178,1.96977173596555,1.97191341784866,1.98119485777428,1.99999636799541,
2.04034065568394,2.05258399045552,2.06729683600943,2.07109426502402,2.07331120119358,
2.07522308690815,2.07755508258722,2.08199131224631,2.11242019220516,2.15453760179427,
2.15952788394103,2.17553328083814,2.17815268663513,2.17949994613809,2.18057125656893,
2.18182804021792,2.18410220413738,2.19543864623566,2.22146059245618,2.27437230825323,
2.28126892435235,2.28413586067807,2.28592883098994,2.28789019755062,2.29059712748133,
2.29702039834854,2.30588627237321,2.35712846618111,2.3871381137356,2.39005251520849,
2.39144118007698,2.39251606035343,2.39374405795638,2.39588674731219,2.40518147929141,
2.42402448743626,2.47021464779431,2.47167402645945,2.4906970588245,2.49445667183905,
2.49686485014865,2.49878240296042,2.50057963286904,2.50367219632359,2.51321649453698,
2.52821612536213,2.55050832517838,2.5930073351113),.UNSPECIFIED.);
#1869=B_SPLINE_CURVE_WITH_KNOTS('',3,(#179777,#179778,#179779,#179780,#179781,
#179782,#179783,#179784,#179785,#179786,#179787,#179788,#179789,#179790,
#179791,#179792,#179793,#179794,#179795,#179796,#179797,#179798,#179799,
#179800,#179801,#179802,#179803,#179804,#179805,#179806,#179807,#179808,
#179809,#179810,#179811,#179812,#179813,#179814,#179815,#179816,#179817,
#179818,#179819,#179820,#179821,#179822,#179823,#179824,#179825,#179826,
#179827,#179828,#179829,#179830,#179831,#179832,#179833,#179834,#179835,
#179836,#179837,#179838,#179839,#179840,#179841,#179842,#179843,#179844,
#179845,#179846,#179847,#179848,#179849,#179850,#179851,#179852,#179853,
#179854,#179855,#179856,#179857,#179858,#179859,#179860,#179861,#179862,
#179863,#179864,#179865,#179866,#179867,#179868,#179869,#179870,#179871,
#179872,#179873,#179874,#179875,#179876,#179877,#179878,#179879,#179880,
#179881,#179882,#179883,#179884,#179885,#179886,#179887,#179888,#179889,
#179890,#179891,#179892,#179893,#179894,#179895,#179896,#179897,#179898,
#179899,#179900,#179901,#179902,#179903,#179904,#179905,#179906,#179907,
#179908,#179909,#179910,#179911,#179912,#179913,#179914,#179915,#179916,
#179917,#179918,#179919,#179920,#179921,#179922,#179923,#179924,#179925,
#179926,#179927,#179928,#179929,#179930,#179931,#179932,#179933,#179934,
#179935,#179936,#179937,#179938,#179939,#179940,#179941,#179942,#179943,
#179944,#179945,#179946,#179947,#179948,#179949,#179950,#179951,#179952,
#179953,#179954,#179955,#179956,#179957,#179958,#179959,#179960,#179961,
#179962,#179963,#179964,#179965,#179966,#179967,#179968,#179969,#179970,
#179971,#179972,#179973,#179974,#179975,#179976,#179977,#179978,#179979,
#179980,#179981,#179982,#179983,#179984,#179985,#179986,#179987,#179988,
#179989,#179990,#179991,#179992,#179993,#179994,#179995,#179996,#179997,
#179998,#179999,#180000,#180001,#180002,#180003,#180004,#180005,#180006,
#180007,#180008,#180009,#180010,#180011,#180012),.UNSPECIFIED.,.F.,.F.,
(4,2,2,2,2,2,2,2,2,2,2,2,2,2,2,2,2,2,2,2,2,2,2,2,2,2,2,2,2,2,2,2,2,2,2,
2,2,2,2,2,2,2,2,2,2,2,2,2,2,2,2,2,2,2,2,2,2,2,2,2,2,2,2,2,2,2,2,2,2,2,2,
2,2,2,2,2,2,2,2,2,2,2,2,2,2,2,2,2,2,2,2,2,2,2,2,2,2,2,2,2,2,2,2,2,2,2,2,
2,2,2,2,2,2,2,2,2,2,4),(0.0750462537154924,0.0761256387381507,0.0989704599401781,
0.111902023384075,0.115419514704814,0.117551996243827,0.119474442395931,
0.121931582678128,0.125852746736523,0.147816198389106,0.207378558798831,
0.215844141380436,0.219418647549753,0.221351067985563,0.222624367089238,
0.22381832530777,0.22486186355796,0.226241575681799,0.229110441793543,0.264441139330251,
0.297386333548054,0.320271350619973,0.325968993619703,0.328548272074073,
0.330487894856251,0.332312144273875,0.334844970402375,0.34142889523907,
0.397818524492796,0.421525799092587,0.432252016242608,0.434490053279475,
0.43573897705894,0.436811042889057,0.438168812213042,0.440837179037049,
0.458109395767358,0.506984886462512,0.525221604404314,0.536273817059415,
0.539604938382228,0.541696425940234,0.543630459272732,0.546129470483122,
0.550279867378455,0.578398283385265,0.620497966164504,0.636274838914577,
0.644544264374919,0.646607926012674,0.647818420132488,0.648896767101814,
0.650291410266022,0.652615204121303,0.667014290583278,0.675576461617543,
0.688666349578805,0.721520054295096,0.744258604835183,0.749936812927187,
0.752512694959083,0.754451951899493,0.756277460950942,0.75881460231764,
0.765424704729817,0.821578218729879,0.8454455735475,0.856215800686848,0.858456695258177,
0.859706322545346,0.8607784416626,0.862135571516215,0.864800557564629,0.881974431453238,
0.927477837906839,0.955339008804063,0.961671787050835,0.964363585663553,
0.96632243793558,0.968118962517457,0.97100438967605,0.978011517918973,1.02935530668646,
1.05652792900927,1.06815196686868,1.07044262972475,1.07170310267479,1.07277428874515,
1.07411724023462,1.07671614900153,1.09222950274384,1.09880436863915,1.14018857818637,
1.16745745311394,1.17371819061984,1.17639772089854,1.17835445569228,1.18015378074087,
1.18305417638074,1.19015070267775,1.23978682627901,1.27816935568051,1.28175573391504,
1.28326688406574,1.28435953159511,1.28538507100967,1.28712572923928,1.29184140475802,
1.33225690507557,1.33414658502961,1.37797807156991,1.38520107324248,1.38812273809624,
1.38992601791968,1.39187979227601,1.3945422296185,1.40070386231283,1.40864677202052),
 .UNSPECIFIED.);
#1870=B_SPLINE_CURVE_WITH_KNOTS('',3,(#180018,#180019,#180020,#180021),
 .UNSPECIFIED.,.F.,.F.,(4,4),(152.105783788367,152.455231354966),
 .UNSPECIFIED.);
#1871=B_SPLINE_CURVE_WITH_KNOTS('',3,(#180022,#180023,#180024,#180025,#180026,
#180027,#180028,#180029,#180030,#180031,#180032,#180033,#180034,#180035,
#180036,#180037,#180038,#180039,#180040,#180041,#180042,#180043,#180044,
#180045,#180046,#180047,#180048,#180049,#180050,#180051,#180052,#180053,
#180054,#180055,#180056,#180057,#180058,#180059,#180060,#180061,#180062,
#180063,#180064,#180065,#180066,#180067,#180068,#180069,#180070,#180071,
#180072,#180073,#180074,#180075,#180076,#180077,#180078,#180079,#180080,
#180081,#180082,#180083,#180084,#180085,#180086,#180087,#180088,#180089,
#180090,#180091,#180092,#180093,#180094,#180095,#180096,#180097,#180098,
#180099,#180100,#180101,#180102,#180103,#180104,#180105,#180106,#180107,
#180108,#180109,#180110,#180111,#180112,#180113,#180114,#180115,#180116,
#180117,#180118,#180119,#180120,#180121,#180122,#180123,#180124,#180125,
#180126,#180127,#180128,#180129,#180130,#180131,#180132,#180133,#180134,
#180135,#180136,#180137,#180138,#180139,#180140,#180141,#180142,#180143,
#180144,#180145,#180146,#180147,#180148,#180149,#180150,#180151,#180152,
#180153,#180154,#180155,#180156,#180157,#180158,#180159,#180160,#180161,
#180162,#180163,#180164,#180165,#180166,#180167,#180168,#180169,#180170,
#180171,#180172,#180173,#180174,#180175,#180176,#180177,#180178,#180179,
#180180,#180181,#180182,#180183,#180184,#180185,#180186,#180187,#180188,
#180189,#180190,#180191,#180192,#180193,#180194,#180195,#180196,#180197,
#180198,#180199,#180200,#180201,#180202,#180203,#180204,#180205,#180206,
#180207,#180208,#180209,#180210,#180211,#180212,#180213,#180214,#180215,
#180216,#180217,#180218,#180219,#180220,#180221,#180222,#180223,#180224,
#180225,#180226,#180227,#180228,#180229,#180230,#180231,#180232,#180233,
#180234,#180235,#180236,#180237,#180238,#180239,#180240,#180241,#180242,
#180243,#180244,#180245,#180246,#180247),.UNSPECIFIED.,.F.,.F.,(4,2,2,2,
2,2,2,2,2,2,2,2,2,2,2,2,2,2,2,2,2,2,2,2,2,2,2,2,2,2,2,2,2,2,2,2,2,2,2,2,
2,2,2,2,2,2,2,2,2,2,2,2,2,2,2,2,2,2,2,2,2,2,2,2,2,2,2,2,2,2,2,2,2,2,2,2,
2,2,2,2,2,2,2,2,2,2,2,2,2,2,2,2,2,2,2,2,2,2,2,2,2,2,2,2,2,2,2,2,2,2,2,2,
4),(0.000629316459415605,0.0219107407500348,0.0544690400356165,0.058013446133146,
0.0595170939913138,0.0606081537861777,0.0616352682843622,0.0633851800392661,
0.0681640862994912,0.104196691217396,0.118264876043651,0.145382236097941,
0.159841449725047,0.163420463120145,0.165251746466431,0.167163469554063,
0.169379347146946,0.173172836430744,0.187843957056055,0.194634607030113,
0.232398675936394,0.257333668883158,0.268387954983155,0.270645518873576,
0.271898594097376,0.272970084500289,0.274321831658835,0.276453659046085,
0.287275067141506,0.291986924343857,0.292255738542014,0.299089676090735,
0.344016679468041,0.361673377650787,0.37247226116102,0.375775572990988,
0.37786076271535,0.379796649878384,0.38230890782771,0.386505067983572,0.416445511501366,
0.457610276871152,0.472691013384552,0.480712489556112,0.482755284556124,
0.483961048244808,0.485040368096117,0.486443047697802,0.488794591398675,
0.503847725139858,0.50417963064025,0.508484169232661,0.556501547347434,
0.580216269568659,0.586024222722498,0.588623458877811,0.590566149166089,
0.592384616724773,0.594895671029282,0.601345967063761,0.658910661578761,
0.681863226079149,0.692380929377794,0.69460594091003,0.69585197383282,0.696924280343102,
0.69828586238423,0.700449775966555,0.711789625384751,0.762836706960133,
0.791362040599131,0.797774181404231,0.800479162910151,0.802440117663382,
0.804233404117657,0.807102343025063,0.814011507442687,0.86678853168531,
0.892931787907377,0.904298204246441,0.906574054699768,0.907831176331421,
0.908902418230124,0.910249131646227,0.912866126801966,0.928828565608794,
0.929545427851628,0.973844302069392,1.00321075255303,1.00972273447401,1.01244458574824,
1.01440868736056,1.01619863283265,1.01904876395403,1.0258433586234,1.08004718552776,
1.10520899712734,1.11632331638331,1.11858464568805,1.11983864887484,1.120910222607,
1.12226116799733,1.12489765476065,1.14132677815376,1.19190998478661,1.20961968338314,
1.22044219744945,1.22374835298558,1.22583432822735,1.22777024940487,1.23028156702776,
1.23447399618861,1.25952994513294),.UNSPECIFIED.);
#1872=B_SPLINE_CURVE_WITH_KNOTS('',3,(#180249,#180250,#180251,#180252,#180253,
#180254,#180255,#180256,#180257,#180258,#180259,#180260,#180261,#180262,
#180263,#180264,#180265,#180266,#180267,#180268,#180269,#180270,#180271,
#180272,#180273,#180274,#180275,#180276,#180277,#180278,#180279,#180280,
#180281,#180282,#180283,#180284,#180285,#180286,#180287,#180288,#180289,
#180290,#180291,#180292,#180293,#180294,#180295,#180296,#180297,#180298,
#180299,#180300,#180301,#180302,#180303,#180304,#180305,#180306,#180307,
#180308,#180309,#180310,#180311,#180312,#180313,#180314,#180315,#180316,
#180317,#180318,#180319,#180320,#180321,#180322,#180323,#180324,#180325,
#180326,#180327,#180328,#180329,#180330,#180331,#180332,#180333,#180334,
#180335,#180336,#180337,#180338,#180339,#180340,#180341,#180342,#180343,
#180344,#180345,#180346,#180347,#180348,#180349,#180350,#180351,#180352,
#180353,#180354,#180355,#180356,#180357,#180358,#180359,#180360,#180361,
#180362,#180363,#180364,#180365,#180366,#180367,#180368,#180369,#180370,
#180371,#180372,#180373,#180374,#180375,#180376,#180377,#180378,#180379,
#180380,#180381,#180382,#180383,#180384,#180385,#180386,#180387,#180388,
#180389,#180390,#180391,#180392,#180393,#180394,#180395,#180396,#180397,
#180398,#180399,#180400,#180401,#180402,#180403,#180404,#180405,#180406,
#180407,#180408,#180409,#180410,#180411,#180412,#180413,#180414,#180415,
#180416,#180417,#180418,#180419,#180420,#180421,#180422,#180423,#180424,
#180425,#180426,#180427,#180428,#180429,#180430,#180431,#180432,#180433,
#180434,#180435,#180436,#180437,#180438,#180439,#180440,#180441,#180442,
#180443,#180444,#180445,#180446,#180447,#180448,#180449,#180450,#180451,
#180452,#180453,#180454,#180455,#180456,#180457,#180458,#180459,#180460,
#180461,#180462,#180463,#180464,#180465,#180466),.UNSPECIFIED.,.F.,.F.,
(4,2,2,2,2,2,2,2,2,2,2,2,2,2,2,2,2,2,2,2,2,2,2,2,2,2,2,2,2,2,2,2,2,2,2,
2,2,2,2,2,2,2,2,2,2,2,2,2,2,2,2,2,2,2,2,2,2,2,2,2,2,2,2,2,2,2,2,2,2,2,2,
2,2,2,2,2,2,2,2,2,2,2,2,2,2,2,2,2,2,2,2,2,2,2,2,2,2,2,2,2,2,2,2,2,2,2,2,
2,4),(1.40864677202052,1.42717364576226,1.46609541676906,1.47423845005591,
1.49151516819806,1.49418410944191,1.49554213256243,1.49661437793364,1.49786349370049,
1.50010182030058,1.51082885999856,1.53453385511464,1.56191062557594,1.59384737618265,
1.59808754277584,1.60061307280469,1.60255156194732,1.60463207368134,1.60791211342398,
1.61849509322632,1.6356638427404,1.68140178055422,1.68818809443002,1.70362499740722,
1.70599281398186,1.70740047378882,1.70848077396767,1.7096844891459,1.71171695329105,
1.71961256367361,1.73434144998214,1.76337580102843,1.80576310256087,1.81005680894429,
1.81259791662672,1.81453894986154,1.81661304119256,1.8198637714802,1.83018809678135,
1.84678009577227,1.8796966328426,1.8957088568118,1.89936901383237,1.91556025607603,
1.91818768760102,1.91953682008136,1.92060843647354,1.92186420908351,1.92413306833315,
1.93537222914556,1.96101030602208,2.01449202780544,2.02134631995769,2.0242066152825,
2.02599861757039,2.02796149101847,2.03067521466761,2.03713701056287,2.09109131045908,
2.12733130069677,2.13018646890341,2.13156373324646,2.13263766183573,2.13387345146592,
2.13605083075925,2.14583496536358,2.19473680294313,2.22986226626357,2.23415147433881,
2.23669122124905,2.2386319653576,2.24070647594637,2.24395938560466,2.25430350273394,
2.2709395883316,2.30389189654495,2.32204987328687,2.33956664036618,2.34224414499969,
2.34360397074656,2.34467632491935,2.34592406023346,2.34815617422359,2.35878323367491,
2.38212425015349,2.43905942078557,2.44557853004871,2.44810086625834,2.44992251969286,
2.45182509696711,2.4543389563836,2.45711929023671,2.47422092648888,2.50981441549534,
2.54858920483338,2.55333924153494,2.55508500962317,2.55611148224048,2.55720336957248,
2.55871061120539,2.56227466057451,2.59910852854178,2.64882446399773,2.65698836256091,
2.66005999003248,2.66189152253071,2.66373571134253,2.66602783958275,2.66809243247618),
 .UNSPECIFIED.);
#1873=B_SPLINE_CURVE_WITH_KNOTS('',3,(#180467,#180468,#180469,#180470,#180471,
#180472,#180473,#180474,#180475,#180476),.UNSPECIFIED.,.F.,.F.,(4,2,2,2,
4),(0.000823833555207768,0.00366228394810211,0.00932751687306586,0.0366377460792521,
0.0751066538684062),.UNSPECIFIED.);
#1874=B_SPLINE_CURVE_WITH_KNOTS('',3,(#180482,#180483,#180484,#180485,#180486,
#180487),.UNSPECIFIED.,.F.,.F.,(4,2,4),(2.59315592077889,2.60891629482103,
2.66742166566177),.UNSPECIFIED.);
#1875=B_SPLINE_CURVE_WITH_KNOTS('',3,(#180488,#180489,#180490,#180491,#180492,
#180493,#180494,#180495,#180496,#180497),.UNSPECIFIED.,.F.,.F.,(4,1,1,1,
1,1,1,4),(152.455231354966,152.821976844167,153.820813294129,154.819649744091,
155.818486194052,156.817322644014,157.816159093976,158.388969095546),
 .UNSPECIFIED.);
#1876=B_SPLINE_CURVE_WITH_KNOTS('',3,(#180498,#180499,#180500,#180501,#180502,
#180503,#180504,#180505,#180506,#180507,#180508,#180509,#180510,#180511,
#180512,#180513,#180514,#180515,#180516,#180517,#180518,#180519,#180520,
#180521,#180522,#180523,#180524,#180525,#180526,#180527,#180528,#180529,
#180530,#180531,#180532,#180533,#180534,#180535,#180536,#180537,#180538,
#180539,#180540,#180541,#180542,#180543,#180544,#180545,#180546,#180547,
#180548,#180549,#180550,#180551,#180552,#180553,#180554,#180555,#180556,
#180557,#180558,#180559,#180560,#180561,#180562,#180563,#180564,#180565,
#180566,#180567,#180568,#180569,#180570,#180571,#180572,#180573,#180574,
#180575,#180576,#180577,#180578,#180579,#180580,#180581,#180582,#180583,
#180584,#180585,#180586,#180587,#180588,#180589,#180590,#180591,#180592,
#180593,#180594,#180595,#180596,#180597,#180598,#180599,#180600,#180601,
#180602,#180603,#180604,#180605,#180606,#180607,#180608,#180609,#180610,
#180611,#180612,#180613,#180614,#180615,#180616,#180617,#180618,#180619,
#180620,#180621,#180622,#180623,#180624,#180625,#180626,#180627,#180628,
#180629,#180630,#180631,#180632,#180633,#180634,#180635,#180636,#180637,
#180638,#180639,#180640,#180641,#180642,#180643,#180644,#180645,#180646,
#180647,#180648,#180649,#180650,#180651,#180652,#180653,#180654,#180655,
#180656,#180657,#180658,#180659,#180660,#180661,#180662,#180663,#180664,
#180665,#180666,#180667,#180668,#180669,#180670,#180671,#180672,#180673,
#180674,#180675,#180676,#180677,#180678,#180679,#180680,#180681,#180682,
#180683,#180684,#180685,#180686,#180687,#180688,#180689,#180690,#180691,
#180692,#180693,#180694,#180695,#180696,#180697,#180698,#180699,#180700,
#180701,#180702,#180703,#180704,#180705,#180706,#180707,#180708,#180709,
#180710,#180711,#180712,#180713,#180714,#180715,#180716,#180717,#180718,
#180719,#180720,#180721,#180722,#180723,#180724,#180725,#180726,#180727,
#180728,#180729,#180730,#180731,#180732,#180733,#180734,#180735,#180736,
#180737,#180738,#180739,#180740,#180741,#180742,#180743,#180744,#180745),
 .UNSPECIFIED.,.F.,.F.,(4,2,2,2,2,2,2,2,2,2,2,2,2,2,2,2,2,2,2,2,2,2,2,2,
2,2,2,2,2,2,2,2,2,2,2,2,2,2,2,2,2,2,2,2,2,2,2,2,2,2,2,2,2,2,2,2,2,2,2,2,
2,2,2,2,2,2,2,2,2,2,2,2,2,2,2,2,2,2,2,2,2,2,2,2,2,2,2,2,2,2,2,2,2,2,2,2,
2,2,2,2,2,2,2,2,2,2,2,2,2,2,2,2,2,2,2,2,2,2,2,2,2,2,2,4),(0.0751066538684062,
0.0853464370458629,0.0970415719080759,0.0993358324161196,0.100596927831639,
0.101667827669287,0.103009388096851,0.105107785673461,0.115413356626747,
0.12067329748708,0.139468793162179,0.181309803440704,0.199977034375344,
0.202818257513735,0.205275670488441,0.207196708670981,0.208991016502369,
0.211865349820437,0.218790631706484,0.271285788687736,0.297629150870201,
0.309046253200314,0.311325043344881,0.312582827521975,0.313654051970842,
0.315000003570262,0.31761334854299,0.333490389110287,0.339268429871492,
0.378729182437409,0.407975659719928,0.414473668465978,0.417193258632019,
0.419157015533481,0.420947527455091,0.423800462764248,0.43061146404938,
0.484633539818862,0.509922005727839,0.521069529966652,0.523332882455269,
0.52458736213142,0.525658949069601,0.527009408273084,0.529136584894448,
0.539880483893609,0.545950872384997,0.549568907402696,0.595500673643667,
0.613961068927827,0.625110025414995,0.628451652918744,0.630545550707453,
0.632478962426192,0.634973176772787,0.639106945842207,0.666582324745711,
0.708929438223251,0.725014649531097,0.733392079130199,0.735464646410787,
0.736677168609629,0.737755144674835,0.739146485178004,0.741458868591958,
0.755618914432618,0.756947693765561,0.775377036237943,0.77771377382717,
0.810507456247192,0.83315022931624,0.838815680743529,0.841389321434246,
0.843328330608518,0.84515466292416,0.847694641618562,0.854322106688857,
0.910315161187398,0.93429138016885,0.945091386749922,0.947334196497143,
0.94858429027601,0.94965643833323,0.951013128343307,0.953160447902102,0.964222443799658,
1.01536897095973,1.0440936697049,1.05053028629531,1.05323977540908,1.05520188675337,
1.05699477868204,1.0598599266731,1.06674360217525,1.11988990105854,1.14579021437507,
1.15709595355743,1.15936870112171,1.16062532512125,1.16169688147637,1.16304493029893,
1.16566728427923,1.18171529530774,1.18582749280021,1.2015194330128,1.23440851705753,
1.25719722284593,1.26288266808008,1.26546015801674,1.26739994702939,1.26922545978457,
1.27176181064671,1.27836519705283,1.33460492043245,1.35355839492103,1.36856131134596,
1.37091144978739,1.37231399672715,1.37339364470637,1.3746002647154,1.37664556743915,
1.38469044903661,1.39983134679781,1.4087239097703),.UNSPECIFIED.);
#1877=B_SPLINE_CURVE_WITH_KNOTS('',3,(#180750,#180751,#180752,#180753,#180754,
#180755,#180756,#180757,#180758,#180759,#180760,#180761,#180762,#180763,
#180764,#180765,#180766,#180767,#180768,#180769,#180770,#180771,#180772,
#180773,#180774,#180775,#180776,#180777,#180778,#180779,#180780,#180781,
#180782,#180783,#180784,#180785,#180786,#180787,#180788,#180789,#180790,
#180791,#180792,#180793,#180794,#180795,#180796,#180797,#180798,#180799,
#180800,#180801,#180802,#180803,#180804,#180805,#180806,#180807,#180808,
#180809,#180810,#180811,#180812,#180813,#180814,#180815,#180816,#180817,
#180818,#180819,#180820,#180821,#180822,#180823,#180824,#180825,#180826,
#180827,#180828,#180829,#180830,#180831,#180832,#180833,#180834,#180835,
#180836,#180837,#180838,#180839,#180840,#180841,#180842,#180843,#180844,
#180845,#180846,#180847,#180848,#180849,#180850,#180851,#180852,#180853,
#180854,#180855,#180856,#180857,#180858,#180859,#180860,#180861,#180862,
#180863,#180864,#180865,#180866,#180867,#180868,#180869,#180870,#180871,
#180872,#180873,#180874,#180875,#180876,#180877,#180878,#180879,#180880,
#180881,#180882,#180883,#180884,#180885,#180886,#180887,#180888,#180889,
#180890,#180891,#180892,#180893,#180894,#180895,#180896,#180897,#180898,
#180899,#180900,#180901,#180902,#180903,#180904,#180905,#180906,#180907,
#180908,#180909,#180910,#180911,#180912,#180913,#180914,#180915,#180916,
#180917,#180918,#180919,#180920,#180921,#180922,#180923,#180924,#180925,
#180926,#180927,#180928,#180929,#180930,#180931,#180932,#180933,#180934,
#180935,#180936,#180937,#180938,#180939,#180940,#180941,#180942,#180943,
#180944,#180945,#180946,#180947,#180948,#180949,#180950,#180951,#180952,
#180953,#180954,#180955,#180956,#180957,#180958,#180959,#180960,#180961,
#180962,#180963,#180964,#180965,#180966,#180967,#180968,#180969,#180970,
#180971,#180972,#180973,#180974,#180975,#180976,#180977,#180978,#180979,
#180980,#180981,#180982,#180983),.UNSPECIFIED.,.F.,.F.,(4,2,2,2,2,2,2,2,
2,2,2,2,2,2,2,2,2,2,2,2,2,2,2,2,2,2,2,2,2,2,2,2,2,2,2,2,2,2,2,2,2,2,2,2,
2,2,2,2,2,2,2,2,2,2,2,2,2,2,2,2,2,2,2,2,2,2,2,2,2,2,2,2,2,2,2,2,2,2,2,2,
2,2,2,2,2,2,2,2,2,2,2,2,2,2,2,2,2,2,2,2,2,2,2,2,2,2,2,2,2,2,2,2,2,2,2,2,
4),(1.2596092854299,1.26784055751155,1.29070305347183,1.30119586103389,
1.30341928457475,1.30466495418703,1.3057372358087,1.30709916505989,1.30978755131927,
1.32763515166132,1.3337320471683,1.3757426351308,1.40292854294941,1.40705404625465,
1.40954560719511,1.41147833514597,1.413572861717,1.41691845641326,1.42810816206235,
1.44666703713446,1.49069768567924,1.49656848995899,1.51244824762357,1.515061588296,
1.51640744975573,1.51747862294526,1.51873640719983,1.52101504483251,1.53242879554278,
1.55875570591604,1.61123417420874,1.61816334580788,1.62103576852764,1.62282983345686,
1.62479052418754,1.62749309455207,1.63388986676,1.68178289775531,1.72137472810358,
1.72610769765945,1.72785089466736,1.72887687739298,1.7299690440267,1.73147806846267,
1.73505280596006,1.77424547541152,1.82298126420698,1.83011231019706,1.83301822396599,
1.83481837115166,1.8367739495846,1.83944819181053,1.84567960840533,1.87271680925558,
1.91343179187051,1.9361424106261,1.93899620386144,1.94037302386442,1.94144670813122,
1.94268232985773,1.94485968541373,1.95464821425903,2.00353413482948,2.03864072814747,
2.04293542352402,2.04547648503994,2.04741711898868,2.04949043046021,2.05273920036304,
2.06305106396055,2.07961707413574,2.11250732988003,2.12706654699959,2.1323852310817,
2.14842387306158,2.15104513512959,2.15239273817488,2.15346400914608,2.15472038860364,
2.15699287334563,2.16830152576631,2.19421530896038,2.24727738471828,2.2541619656418,
2.25702684114788,2.25881937754806,2.26078095698944,2.26348944196519,2.26992238015805,
2.29862621005349,2.34984861188788,2.36088133259416,2.36302657483499,2.36438248748561,
2.36545437861352,2.36670458817691,2.36894865199325,2.37977521518805,2.4038504481036,
2.45963405600161,2.46627495554774,2.46881672542427,2.47064329078775,2.47251929302347,
2.47500313974899,2.47774077498614,2.48229128053979,2.49161863124835,2.54225918008863,
2.57203620196739,2.57495057375471,2.57633918699828,2.57741401028942,2.57864192378382,
2.58078442024775,2.59007760248922,2.59315592077889),.UNSPECIFIED.);
#1878=B_SPLINE_CURVE_WITH_KNOTS('',3,(#180985,#180986,#180987,#180988,#180989,
#180990,#180991,#180992,#180993,#180994,#180995,#180996,#180997,#180998,
#180999,#181000,#181001,#181002,#181003,#181004,#181005,#181006,#181007,
#181008,#181009,#181010,#181011,#181012,#181013,#181014,#181015,#181016,
#181017,#181018,#181019,#181020,#181021,#181022,#181023,#181024,#181025,
#181026,#181027,#181028,#181029,#181030,#181031,#181032,#181033,#181034,
#181035,#181036,#181037,#181038,#181039,#181040,#181041,#181042,#181043,
#181044,#181045,#181046,#181047,#181048,#181049,#181050,#181051,#181052,
#181053,#181054,#181055,#181056,#181057,#181058,#181059,#181060,#181061,
#181062,#181063,#181064,#181065,#181066,#181067,#181068,#181069,#181070,
#181071,#181072,#181073,#181074,#181075,#181076,#181077,#181078,#181079,
#181080,#181081,#181082,#181083,#181084,#181085,#181086,#181087,#181088,
#181089,#181090,#181091,#181092,#181093,#181094,#181095,#181096,#181097,
#181098,#181099,#181100,#181101,#181102,#181103,#181104,#181105,#181106,
#181107,#181108,#181109,#181110,#181111,#181112,#181113,#181114,#181115,
#181116,#181117,#181118,#181119,#181120,#181121,#181122,#181123,#181124,
#181125,#181126,#181127,#181128,#181129,#181130,#181131,#181132,#181133,
#181134,#181135,#181136,#181137,#181138,#181139,#181140,#181141,#181142,
#181143,#181144,#181145,#181146,#181147,#181148,#181149,#181150,#181151,
#181152,#181153,#181154,#181155,#181156,#181157,#181158,#181159,#181160,
#181161,#181162,#181163,#181164,#181165,#181166,#181167,#181168,#181169,
#181170,#181171,#181172,#181173,#181174,#181175,#181176,#181177,#181178,
#181179,#181180,#181181,#181182,#181183,#181184,#181185,#181186,#181187,
#181188,#181189,#181190,#181191,#181192,#181193,#181194,#181195,#181196,
#181197,#181198,#181199,#181200,#181201,#181202,#181203,#181204,#181205,
#181206,#181207,#181208,#181209,#181210),.UNSPECIFIED.,.F.,.F.,(4,2,2,2,
2,2,2,2,2,2,2,2,2,2,2,2,2,2,2,2,2,2,2,2,2,2,2,2,2,2,2,2,2,2,2,2,2,2,2,2,
2,2,2,2,2,2,2,2,2,2,2,2,2,2,2,2,2,2,2,2,2,2,2,2,2,2,2,2,2,2,2,2,2,2,2,2,
2,2,2,2,2,2,2,2,2,2,2,2,2,2,2,2,2,2,2,2,2,2,2,2,2,2,2,2,2,2,2,2,2,2,2,2,
4),(1.4087239097703,1.43953310653064,1.4707906634425,1.47501726132828,1.47753894204538,
1.47947694358548,1.48155935196071,1.48484750803127,1.49550157222155,1.51282980903747,
1.55311717757715,1.58011104335949,1.58301346000418,1.58440002326499,1.58547494306089,
1.58670485223124,1.58885526017928,1.59825165920333,1.64749090277013,1.68271042221743,
1.68700767412,1.68954985110794,1.69149110854773,1.69356486489835,1.69681387046829,
1.7071226019063,1.72367991756045,1.75656825147938,1.77012258685533,1.77743785290147,
1.78179523708985,1.79296115305944,1.7951149407989,1.79647362262413,1.79754595605584,
1.79879467912652,1.80103106831506,1.81172554047372,1.83531077426319,1.89186564640622,
1.89843106897118,1.90096124141165,1.90278503575134,1.90472552121993,1.90730824366264,
1.91302294624607,1.93603367005409,1.96909147498953,1.99034868695485,2.0046763164207,
2.00699835131973,2.00839255421045,2.00947093981632,2.01068191140972,2.01274734029082,
2.02103661059078,2.03686696109282,2.07904331309759,2.10698563685207,2.1111315541083,
2.11362941753169,2.1155634687185,2.11765587684943,2.12099040864645,2.13207178847149,
2.15037766535872,2.19869324226627,2.21644768555504,2.2191335159248,2.22049512370589,
2.22156762814829,2.22281410102886,2.22504040537006,2.23557399195102,2.25857773083565,
2.31603906537968,2.32250093672487,2.32501419885246,2.32683348917125,2.32877633456139,
2.33137452002162,2.33717482919308,2.36083020557867,2.39173684265513,2.42827449457615,
2.43112334198816,2.4324992669988,2.43357296085789,2.43478455334195,2.43688094777454,
2.43946832806807,2.44484972478038,2.46014569794909,2.50065627361534,2.53090695350227,
2.53511069881581,2.53762547072958,2.5395620976429,2.54164690306083,2.54494708699777,
2.55571316586618,2.57329622979357,2.61947477386722,2.62780655258086,2.64081202452361,
2.64306759883811,2.64445699598947,2.64553204210694,2.64654087036144,2.64775405385555,
2.64954048691474,2.65527579181324,2.66794445739932),.UNSPECIFIED.);
#1879=B_SPLINE_CURVE_WITH_KNOTS('',3,(#181211,#181212,#181213,#181214,#181215,
#181216,#181217,#181218,#181219,#181220,#181221,#181222,#181223),
 .UNSPECIFIED.,.F.,.F.,(4,3,3,3,4),(-161.271232361061,-161.169466150914,
-161.067655442619,-160.965693965034,-160.920671713183),.UNSPECIFIED.);
#1880=B_SPLINE_CURVE_WITH_KNOTS('',3,(#181229,#181230,#181231,#181232,#181233,
#181234,#181235,#181236,#181237,#181238,#181239,#181240,#181241),
 .UNSPECIFIED.,.F.,.F.,(4,3,3,3,4),(170.955339710339,171.057208844779,171.158971097412,
171.260660135508,171.305836564222),.UNSPECIFIED.);
#1881=B_SPLINE_CURVE_WITH_KNOTS('',3,(#181242,#181243,#181244,#181245,#181246,
#181247,#181248,#181249,#181250,#181251,#181252,#181253,#181254,#181255,
#181256,#181257,#181258,#181259,#181260,#181261,#181262,#181263,#181264,
#181265,#181266,#181267,#181268,#181269,#181270,#181271,#181272,#181273,
#181274,#181275,#181276,#181277,#181278,#181279,#181280,#181281,#181282,
#181283,#181284,#181285,#181286,#181287,#181288,#181289,#181290,#181291,
#181292,#181293,#181294,#181295,#181296,#181297,#181298,#181299,#181300,
#181301,#181302,#181303,#181304,#181305,#181306,#181307,#181308,#181309,
#181310,#181311,#181312,#181313,#181314,#181315,#181316,#181317,#181318,
#181319,#181320,#181321,#181322,#181323,#181324,#181325,#181326,#181327,
#181328,#181329,#181330,#181331,#181332,#181333,#181334,#181335,#181336,
#181337,#181338,#181339,#181340,#181341,#181342,#181343,#181344,#181345,
#181346,#181347,#181348,#181349,#181350,#181351,#181352,#181353,#181354,
#181355,#181356,#181357,#181358,#181359,#181360,#181361,#181362,#181363,
#181364,#181365,#181366,#181367,#181368,#181369,#181370,#181371,#181372,
#181373,#181374,#181375,#181376,#181377,#181378,#181379,#181380,#181381,
#181382,#181383,#181384,#181385,#181386,#181387,#181388,#181389,#181390,
#181391,#181392,#181393,#181394,#181395,#181396,#181397,#181398,#181399,
#181400,#181401,#181402,#181403,#181404,#181405,#181406,#181407,#181408,
#181409,#181410,#181411,#181412,#181413,#181414,#181415,#181416,#181417,
#181418,#181419,#181420,#181421,#181422,#181423,#181424,#181425,#181426,
#181427,#181428,#181429,#181430,#181431,#181432,#181433,#181434,#181435,
#181436,#181437,#181438,#181439,#181440,#181441,#181442,#181443,#181444,
#181445,#181446,#181447,#181448,#181449,#181450,#181451,#181452,#181453,
#181454,#181455,#181456,#181457,#181458,#181459,#181460,#181461,#181462,
#181463),.UNSPECIFIED.,.F.,.F.,(4,2,2,2,2,2,2,2,2,2,2,2,2,2,2,2,2,2,2,2,
2,2,2,2,2,2,2,2,2,2,2,2,2,2,2,2,2,2,2,2,2,2,2,2,2,2,2,2,2,2,2,2,2,2,2,2,
2,2,2,2,2,2,2,2,2,2,2,2,2,2,2,2,2,2,2,2,2,2,2,2,2,2,2,2,2,2,2,2,2,2,2,2,
2,2,2,2,2,2,2,2,2,2,2,2,2,2,2,2,2,2,4),(0.000655553105071722,0.0215327022503399,
0.0285521141267371,0.0303960812882683,0.0316335720171466,0.0326484433143034,
0.0337175298956809,0.0350634467520839,0.0377856129526834,0.0559582137427058,
0.0616381071511329,0.0739377920509654,0.0845184420705206,0.106384465137635,
0.122977060357035,0.133286033526241,0.136520200021145,0.138580642265221,
0.140506650842285,0.143024722911443,0.147271547765017,0.192337554227069,
0.220917548979898,0.234450971820541,0.241868990982089,0.243841387940844,
0.244851109631307,0.245918148677256,0.247244764407309,0.249294095405719,
0.258883090837928,0.318505477136906,0.335297061926008,0.345718734013405,
0.348984761231629,0.351065048444871,0.353009420737682,0.35555141705698,
0.359839125091224,0.394233009182222,0.44343552787257,0.453287201291696,
0.455474777349829,0.456715751415926,0.457792016017413,0.459170679611106,
0.462028585192884,0.484806459207241,0.527329152876518,0.545904429014042,
0.557102195141594,0.560449714400349,0.562545379780961,0.564479121375145,
0.566971944221895,0.571099464639318,0.598278064866925,0.640347506189968,
0.656908029981825,0.66544956728105,0.667534904237756,0.66875003530653,0.669826485917343,
0.671211219103108,0.673503612986742,0.68728756877378,0.698620809126769,
0.737949711512445,0.764492303067573,0.770660366503347,0.773322007001096,
0.775273831587008,0.777074347835149,0.779989349136334,0.787184849384752,
0.833863017380337,0.856213770649654,0.870037647785498,0.875062775891369,
0.878645299588949,0.880154594737846,0.881246030472107,0.882271314704293,
0.884011288224965,0.888723642665489,0.929074950392337,0.977358991268938,
0.982966730790509,0.985529988135733,0.987467663862014,0.989297530270643,
0.991850143526969,0.998557329207836,1.05366061574855,1.07817670571631,1.08912119122043,
1.09137328851315,1.09262570504106,1.09369780575127,1.09505199526529,1.09779133641041,
1.1161497469021,1.16514969113898,1.18898303318183,1.19480675563528,1.19740896224039,
1.19935225338315,1.20117011145434,1.20367847276004,1.21011174277809,1.2596092854299),
 .UNSPECIFIED.);
#1882=B_SPLINE_CURVE_WITH_KNOTS('',3,(#181465,#181466,#181467,#181468,#181469,
#181470,#181471,#181472,#181473,#181474,#181475,#181476,#181477,#181478,
#181479,#181480,#181481,#181482,#181483,#181484,#181485,#181486,#181487,
#181488,#181489,#181490,#181491,#181492,#181493,#181494,#181495,#181496,
#181497,#181498,#181499,#181500,#181501,#181502,#181503,#181504,#181505,
#181506,#181507,#181508,#181509,#181510,#181511,#181512,#181513,#181514,
#181515,#181516,#181517,#181518,#181519,#181520,#181521,#181522,#181523,
#181524,#181525,#181526,#181527,#181528,#181529,#181530,#181531,#181532,
#181533,#181534,#181535,#181536,#181537,#181538,#181539,#181540,#181541,
#181542,#181543,#181544,#181545,#181546,#181547,#181548,#181549,#181550,
#181551,#181552,#181553,#181554,#181555,#181556,#181557,#181558,#181559,
#181560,#181561,#181562,#181563,#181564,#181565,#181566,#181567,#181568,
#181569,#181570,#181571,#181572,#181573,#181574,#181575,#181576,#181577,
#181578,#181579,#181580,#181581,#181582,#181583,#181584,#181585,#181586,
#181587,#181588,#181589,#181590,#181591,#181592,#181593,#181594,#181595,
#181596,#181597,#181598,#181599,#181600,#181601,#181602,#181603,#181604,
#181605,#181606,#181607,#181608,#181609,#181610,#181611,#181612,#181613,
#181614,#181615,#181616,#181617,#181618,#181619,#181620,#181621,#181622,
#181623,#181624,#181625,#181626,#181627,#181628,#181629,#181630,#181631,
#181632,#181633,#181634,#181635,#181636,#181637,#181638,#181639,#181640,
#181641,#181642,#181643,#181644,#181645),.UNSPECIFIED.,.F.,.F.,(4,3,3,3,
3,3,3,3,3,3,3,3,3,3,3,3,3,3,3,3,3,3,3,3,3,3,3,3,3,3,3,3,3,3,3,3,3,3,3,3,
3,3,3,3,3,3,3,3,3,3,3,3,3,3,3,3,3,3,3,3,4),(-167.203857019737,-167.089811057167,
-166.975344515757,-166.860315160037,-166.805687143633,-166.702287412998,
-166.599041100617,-166.495916074883,-166.392856430485,-166.289828137571,
-166.186797209444,-166.083659391335,-165.980465259865,-165.877088300924,
-165.806850693671,-165.703453680512,-165.600210065146,-165.497087692246,
-165.394030672044,-165.291004970728,-165.187976597605,-165.084841259846,
-164.981649570783,-164.878274965339,-164.808014243709,-164.70462213054,
-164.601383514262,-164.4982662645,-164.39521444117,-164.292194002951,-164.189170951718,
-164.08604098996,-163.982854715524,-163.879485527151,-163.809177793747,
-163.705782195438,-163.602540043866,-163.499419201028,-163.396363750916,
-163.293339657491,-163.190312927878,-163.087179277445,-162.983989302849,
-162.880616436887,-162.810341343786,-162.706946383752,-162.603704871948,
-162.500584667936,-162.39752985573,-162.294506398346,-162.191480301959,
-162.088347275963,-161.985157921851,-161.881785663032,-161.811504893824,
-161.709471729847,-161.607582180192,-161.505807287711,-161.404097849845,
-161.30240517996,-161.271232361061),.UNSPECIFIED.);
#1883=B_SPLINE_CURVE_WITH_KNOTS('',3,(#181646,#181647,#181648,#181649,#181650,
#181651,#181652,#181653,#181654,#181655,#181656,#181657,#181658),
 .UNSPECIFIED.,.F.,.F.,(4,3,3,3,4),(-167.553337655846,-167.448855737649,
-167.344457493798,-167.24011056783,-167.203857020092),.UNSPECIFIED.);
#1884=B_SPLINE_CURVE_WITH_KNOTS('',3,(#181664,#181665,#181666,#181667,#181668,
#181669,#181670,#181671,#181672,#181673),.UNSPECIFIED.,.F.,.F.,(4,3,3,4),
(7.5925217235916,7.70650211118153,7.82442142970536,7.9423407482292),
 .UNSPECIFIED.);
#1885=B_SPLINE_CURVE_WITH_KNOTS('',3,(#181675,#181676,#181677,#181678,#181679,
#181680,#181681,#181682,#181683,#181684,#181685,#181686,#181687,#181688,
#181689,#181690,#181691,#181692,#181693,#181694,#181695,#181696,#181697,
#181698,#181699,#181700,#181701,#181702,#181703,#181704,#181705,#181706,
#181707,#181708,#181709,#181710,#181711,#181712,#181713,#181714,#181715,
#181716,#181717,#181718,#181719,#181720,#181721,#181722,#181723,#181724,
#181725,#181726,#181727,#181728,#181729,#181730,#181731,#181732,#181733,
#181734,#181735,#181736,#181737,#181738,#181739,#181740,#181741,#181742,
#181743,#181744,#181745,#181746,#181747,#181748,#181749,#181750,#181751,
#181752,#181753,#181754,#181755,#181756,#181757,#181758,#181759,#181760,
#181761,#181762,#181763,#181764,#181765,#181766,#181767,#181768,#181769,
#181770,#181771,#181772,#181773,#181774,#181775,#181776,#181777,#181778,
#181779,#181780,#181781,#181782,#181783,#181784,#181785,#181786,#181787,
#181788,#181789,#181790,#181791,#181792,#181793,#181794,#181795,#181796,
#181797,#181798,#181799,#181800,#181801,#181802,#181803,#181804,#181805,
#181806,#181807,#181808,#181809,#181810,#181811,#181812,#181813,#181814,
#181815,#181816,#181817,#181818,#181819,#181820,#181821,#181822,#181823,
#181824,#181825,#181826,#181827,#181828,#181829,#181830,#181831,#181832,
#181833,#181834,#181835,#181836,#181837,#181838,#181839,#181840,#181841,
#181842,#181843),.UNSPECIFIED.,.F.,.F.,(4,3,3,3,3,3,3,3,3,3,3,3,3,3,3,3,
3,3,3,3,3,3,3,3,3,3,3,3,3,3,3,3,3,3,3,3,3,3,3,3,3,3,3,3,3,3,3,3,3,3,3,3,
3,3,3,3,4),(2.0087845179796,2.11210382153695,2.21526971314845,2.31831418782041,
2.42129345937132,2.52424167355639,2.62719293310599,2.73024899451789,2.83336205194679,
2.93665137518728,2.99650934988562,3.1000822938161,3.20350554280194,3.30681219802197,
3.41005626110442,3.51327148737703,3.6164915916683,3.71982072762223,3.82320766651892,
3.92677769686775,3.9953457998475,4.09860816546045,4.20171516905871,4.30469864795499,
4.40761543749361,4.51049977143286,4.61338583911071,4.71637840074725,4.81942682496833,
4.92265896654802,4.99418224980937,5.09760356589106,5.2008715269481,5.30401818826614,
5.40709944854822,5.51014930542212,5.61320171332599,5.71636073031363,5.81957593612843,
5.92297353214023,5.99301869977125,6.09643423322203,6.19969677808622,6.30283860095653,
6.40591538148351,6.50896112490232,6.61200979362756,6.71516567854847,6.81837808737288,
6.92177346211854,6.99185514973312,7.09670699527071,7.20139082935589,7.30591391683331,
7.41034217631691,7.5147117225697,7.59252172323623),.UNSPECIFIED.);
#1886=B_SPLINE_CURVE_WITH_KNOTS('',3,(#181847,#181848,#181849,#181850,#181851,
#181852,#181853,#181854,#181855,#181856,#181857,#181858,#181859,#181860,
#181861,#181862,#181863,#181864,#181865,#181866,#181867,#181868,#181869,
#181870,#181871,#181872,#181873,#181874,#181875,#181876,#181877,#181878,
#181879,#181880,#181881,#181882,#181883,#181884,#181885,#181886,#181887,
#181888,#181889,#181890,#181891,#181892,#181893,#181894,#181895,#181896,
#181897,#181898,#181899,#181900,#181901,#181902,#181903,#181904,#181905,
#181906,#181907,#181908,#181909,#181910,#181911,#181912,#181913,#181914,
#181915,#181916,#181917,#181918,#181919,#181920,#181921,#181922,#181923,
#181924,#181925,#181926,#181927,#181928,#181929,#181930,#181931,#181932,
#181933,#181934,#181935,#181936,#181937,#181938,#181939,#181940,#181941,
#181942,#181943,#181944,#181945,#181946,#181947,#181948,#181949,#181950,
#181951,#181952,#181953,#181954,#181955,#181956,#181957,#181958,#181959,
#181960,#181961,#181962,#181963,#181964),.UNSPECIFIED.,.F.,.F.,(4,3,3,3,
3,3,3,3,3,3,3,3,3,3,3,3,3,3,3,3,3,3,3,3,3,3,3,3,3,3,3,3,3,3,3,3,3,3,3,4),
(-3.8410390329882,-3.73547282260038,-3.63371534136024,-3.53202564994167,
-3.43036801697593,-3.32870675963968,-3.22694496840103,-3.12512265251928,
-3.02313914541121,-2.99650934988562,-2.89298805351485,-2.78961775740447,
-2.68636579627284,-2.58317747650149,-2.48001897640827,-2.37685651582112,
-2.27358608503736,-2.17025853571448,-2.06674838352885,-1.99767289992375,
-1.89536967835424,-1.79322051059792,-1.69118874726443,-1.58921969074132,
-1.48727797529671,-1.3853282756702,-1.28325622478001,-1.18112117613606,
-1.07878042700533,-0.998836449961875,-0.892562662128034,-0.78099232936203,
-0.675071864520977,-0.569250995903944,-0.463501983636266,-0.357797177553288,
-0.252079241114024,-0.146356223433945,-0.0405602493167351,0.),
 .UNSPECIFIED.);
#1887=B_SPLINE_CURVE_WITH_KNOTS('',3,(#181965,#181966,#181967,#181968,#181969,
#181970,#181971,#181972,#181973,#181974,#181975,#181976,#181977,#181978,
#181979,#181980,#181981,#181982,#181983,#181984,#181985,#181986,#181987,
#181988,#181989,#181990),.UNSPECIFIED.,.F.,.F.,(4,2,2,2,2,2,2,2,2,2,2,2,
4),(0.000655568072780243,0.0215326044780164,0.0285520611652364,0.0303960587346235,
0.0316335581114911,0.032648425183238,0.0337175017371922,0.0350633807412954,
0.0377853867802569,0.0559535320639813,0.0616384514068862,0.0739384345531311,
0.0747573385915169),.UNSPECIFIED.);
#1888=B_SPLINE_CURVE_WITH_KNOTS('',3,(#181996,#181997,#181998,#181999,#182000,
#182001,#182002,#182003,#182004,#182005,#182006,#182007,#182008,#182009,
#182010,#182011,#182012,#182013,#182014,#182015,#182016,#182017,#182018,
#182019),.UNSPECIFIED.,.F.,.F.,(4,2,2,2,2,2,2,2,2,2,2,4),(2.59366994486789,
2.61937244280716,2.62770429439083,2.64070987224822,2.64296546588963,2.64435487507994,
2.64542993062086,2.64643876778755,2.64765196207014,2.64943841110757,2.65517376483347,
2.66784253617411),.UNSPECIFIED.);
#1889=B_SPLINE_CURVE_WITH_KNOTS('',3,(#182020,#182021,#182022,#182023,#182024,
#182025,#182026,#182027,#182028,#182029,#182030,#182031,#182032,#182033,
#182034,#182035,#182036,#182037,#182038,#182039,#182040,#182041,#182042,
#182043,#182044,#182045,#182046,#182047,#182048,#182049,#182050,#182051,
#182052,#182053,#182054,#182055,#182056,#182057,#182058,#182059,#182060,
#182061,#182062,#182063,#182064,#182065,#182066,#182067,#182068,#182069,
#182070,#182071,#182072,#182073,#182074,#182075,#182076,#182077,#182078,
#182079,#182080,#182081,#182082,#182083,#182084,#182085,#182086,#182087,
#182088,#182089,#182090,#182091,#182092,#182093,#182094,#182095,#182096,
#182097,#182098,#182099,#182100,#182101,#182102,#182103,#182104,#182105,
#182106,#182107,#182108,#182109,#182110,#182111,#182112,#182113,#182114,
#182115,#182116,#182117,#182118,#182119,#182120,#182121,#182122,#182123,
#182124,#182125,#182126,#182127,#182128,#182129,#182130,#182131,#182132,
#182133,#182134,#182135,#182136,#182137,#182138,#182139,#182140,#182141,
#182142,#182143,#182144,#182145,#182146,#182147,#182148,#182149,#182150,
#182151,#182152,#182153,#182154,#182155,#182156,#182157,#182158,#182159,
#182160,#182161,#182162,#182163,#182164,#182165,#182166,#182167,#182168,
#182169,#182170,#182171,#182172,#182173,#182174,#182175,#182176,#182177,
#182178,#182179,#182180,#182181,#182182,#182183,#182184,#182185,#182186,
#182187,#182188,#182189,#182190,#182191,#182192,#182193,#182194,#182195,
#182196,#182197,#182198,#182199,#182200),.UNSPECIFIED.,.F.,.F.,(4,3,3,3,
3,3,3,3,3,3,3,3,3,3,3,3,3,3,3,3,3,3,3,3,3,3,3,3,3,3,3,3,3,3,3,3,3,3,3,3,
3,3,3,3,3,3,3,3,3,3,3,3,3,3,3,3,3,3,3,3,4),(7.9423407482292,7.99069159969499,
8.09409131510382,8.1973376121055,8.30046262230383,8.40352225107942,8.50655052830579,
8.6095814407028,8.71271924312554,8.81591335890946,8.91929030233818,8.98952804965687,
9.0929250599491,9.19616867235508,9.29929104216923,9.40234805920861,9.50537375729145,
9.60840212711332,9.71153746148904,9.81472914711778,9.91810374908263,9.98836449961874,
10.0917566194232,10.1949952424428,10.2981124990724,10.4011643293445,10.5041847745688,
10.6072078328613,10.7103378017146,10.813524083277,10.9168932787461,10.9872009495806,
11.0905965448759,11.1938386934009,11.2969595331577,11.40001498017,11.5030390704798,
11.6060657969671,11.7091994442799,11.8123894157543,11.9157622786263,11.9860373995425,
12.0894323592657,12.1926738707447,12.2957940744116,12.3988488862601,12.5018723432752,
12.6048984392812,12.708031464883,12.8112208185909,12.9145930769959,12.9848738495044,
13.0869196153942,13.1887917832796,13.2905669753687,13.3922809425427,13.4939693506563,
13.5957283288954,13.6975220044616,13.7994743438963,13.8757070301446),
 .UNSPECIFIED.);
#1890=B_SPLINE_CURVE_WITH_KNOTS('',3,(#182201,#182202,#182203,#182204,#182205,
#182206,#182207,#182208,#182209,#182210,#182211,#182212,#182213,#182214,
#182215,#182216,#182217,#182218,#182219,#182220,#182221,#182222,#182223,
#182224,#182225,#182226,#182227,#182228,#182229,#182230,#182231,#182232,
#182233,#182234,#182235,#182236,#182237,#182238,#182239,#182240,#182241,
#182242,#182243,#182244,#182245,#182246,#182247,#182248,#182249,#182250,
#182251,#182252,#182253,#182254,#182255,#182256,#182257,#182258,#182259,
#182260,#182261,#182262,#182263,#182264,#182265,#182266,#182267,#182268,
#182269,#182270,#182271,#182272,#182273,#182274,#182275,#182276,#182277,
#182278,#182279,#182280,#182281,#182282,#182283,#182284,#182285,#182286,
#182287,#182288,#182289,#182290,#182291,#182292,#182293,#182294,#182295,
#182296,#182297,#182298,#182299,#182300,#182301,#182302,#182303,#182304,
#182305,#182306,#182307,#182308,#182309,#182310,#182311,#182312,#182313,
#182314,#182315,#182316,#182317,#182318,#182319,#182320,#182321,#182322,
#182323,#182324,#182325,#182326,#182327,#182328,#182329,#182330,#182331,
#182332,#182333,#182334,#182335,#182336,#182337,#182338,#182339,#182340,
#182341,#182342,#182343,#182344,#182345,#182346,#182347,#182348,#182349,
#182350,#182351,#182352,#182353,#182354,#182355,#182356,#182357,#182358,
#182359,#182360,#182361,#182362,#182363,#182364,#182365,#182366,#182367,
#182368,#182369,#182370,#182371,#182372,#182373,#182374,#182375,#182376,
#182377,#182378,#182379,#182380,#182381,#182382,#182383,#182384,#182385,
#182386,#182387,#182388,#182389,#182390,#182391,#182392,#182393,#182394,
#182395,#182396,#182397,#182398,#182399,#182400,#182401,#182402,#182403,
#182404,#182405,#182406,#182407,#182408,#182409,#182410,#182411,#182412,
#182413,#182414,#182415,#182416,#182417,#182418,#182419,#182420,#182421,
#182422,#182423,#182424,#182425,#182426),.UNSPECIFIED.,.F.,.F.,(4,2,2,2,
2,2,2,2,2,2,2,2,2,2,2,2,2,2,2,2,2,2,2,2,2,2,2,2,2,2,2,2,2,2,2,2,2,2,2,2,
2,2,2,2,2,2,2,2,2,2,2,2,2,2,2,2,2,2,2,2,2,2,2,2,2,2,2,2,2,2,2,2,2,2,2,2,
2,2,2,2,2,2,2,2,2,2,2,2,2,2,2,2,2,2,2,2,2,2,2,2,2,2,2,2,2,2,2,2,2,2,2,2,
4),(0.0747573385915169,0.0845186660563088,0.106384825885023,0.122977264307818,
0.133286153510231,0.136520297104307,0.138580725314274,0.140506721079582,
0.14302477673237,0.147271574297925,0.192338068386794,0.220918198232181,
0.23445132046961,0.241869215344308,0.243841592621727,0.244851307008202,
0.245918344988499,0.247244964389105,0.249294304929312,0.258883412682225,
0.318505114363265,0.335297165839,0.345719059569437,0.348985119972811,0.351065419812425,
0.35300979800306,0.355551793623918,0.35983948206055,0.394231696268526,0.443432679699405,
0.453286801430609,0.455474553210324,0.456715570777116,0.457791834590142,
0.459170447891583,0.462028090662232,0.484795377877622,0.527329643639262,
0.545904467140845,0.557102035876837,0.56044953361568,0.562545193908041,
0.564478936499098,0.566971768575439,0.571099321372655,0.59827916816761,
0.640351409167709,0.656909155895798,0.665449741003629,0.667535000112857,
0.668750112633886,0.669826564784798,0.671211323074965,0.673503806328032,
0.687289664657288,0.69862343776508,0.737950307791625,0.764492433751154,
0.770660435514412,0.773322062769965,0.775273882640514,0.777074398031094,
0.779989405707813,0.787184959843073,0.833860461124851,0.856214196184002,
0.870037819475752,0.875062883147794,0.878645370113907,0.880154657585907,
0.881246091026226,0.882271376787971,0.88401135771577,0.888723760194312,
0.929076048762534,0.977359082455919,0.98296681558263,0.985530072725587,
0.98746774942837,0.989297617601982,0.991850234692957,0.998557439042445,
1.05366042498685,1.07817664904728,1.08912117123381,1.09137327239189,1.09262569060441,
1.09369779185165,1.09505198122705,1.09779132125902,1.11614969273561,1.16514965487027,
1.18898299316969,1.19480671436024,1.19740892035612,1.19935221102246,1.20117006862932,
1.20367842925972,1.21011169732687,1.26784057178093,1.29070305835673,1.30119586269071,
1.3034192852407,1.30466495423351,1.30573723528824,1.30709916372239,1.30978754800495,
1.32763511724923,1.33373204591263,1.37574265895549,1.40292854694586,1.40705404852227,
1.40817975905822),.UNSPECIFIED.);
#1891=B_SPLINE_CURVE_WITH_KNOTS('',3,(#182431,#182432,#182433,#182434,#182435,
#182436,#182437,#182438,#182439,#182440,#182441,#182442,#182443,#182444,
#182445,#182446,#182447,#182448,#182449,#182450,#182451,#182452,#182453,
#182454,#182455,#182456,#182457,#182458,#182459,#182460,#182461,#182462,
#182463,#182464,#182465,#182466,#182467,#182468,#182469,#182470,#182471,
#182472,#182473,#182474,#182475,#182476,#182477,#182478,#182479,#182480,
#182481,#182482,#182483,#182484,#182485,#182486,#182487,#182488,#182489,
#182490,#182491,#182492,#182493,#182494,#182495,#182496,#182497,#182498,
#182499,#182500,#182501,#182502,#182503,#182504,#182505,#182506,#182507,
#182508,#182509,#182510,#182511,#182512,#182513,#182514,#182515,#182516,
#182517,#182518,#182519,#182520,#182521,#182522,#182523,#182524,#182525,
#182526,#182527,#182528,#182529,#182530,#182531,#182532,#182533,#182534,
#182535,#182536,#182537,#182538,#182539,#182540,#182541,#182542,#182543,
#182544,#182545,#182546,#182547,#182548,#182549,#182550,#182551,#182552,
#182553,#182554,#182555,#182556,#182557,#182558,#182559,#182560,#182561,
#182562,#182563,#182564,#182565,#182566,#182567,#182568,#182569,#182570,
#182571,#182572,#182573,#182574,#182575,#182576,#182577,#182578,#182579,
#182580,#182581,#182582,#182583,#182584,#182585,#182586,#182587,#182588,
#182589,#182590,#182591,#182592,#182593,#182594,#182595,#182596,#182597,
#182598,#182599,#182600,#182601,#182602,#182603,#182604,#182605,#182606,
#182607,#182608,#182609,#182610,#182611,#182612,#182613,#182614,#182615,
#182616,#182617,#182618,#182619,#182620,#182621,#182622,#182623,#182624,
#182625,#182626,#182627,#182628,#182629,#182630,#182631,#182632,#182633,
#182634,#182635,#182636,#182637,#182638,#182639,#182640,#182641,#182642,
#182643,#182644,#182645,#182646,#182647,#182648,#182649,#182650,#182651,
#182652,#182653,#182654,#182655,#182656,#182657,#182658,#182659,#182660,
#182661,#182662,#182663,#182664,#182665,#182666,#182667,#182668,#182669,
#182670),.UNSPECIFIED.,.F.,.F.,(4,2,2,2,2,2,2,2,2,2,2,2,2,2,2,2,2,2,2,2,
2,2,2,2,2,2,2,2,2,2,2,2,2,2,2,2,2,2,2,2,2,2,2,2,2,2,2,2,2,2,2,2,2,2,2,2,
2,2,2,2,2,2,2,2,2,2,2,2,2,2,2,2,2,2,2,2,2,2,2,2,2,2,2,2,2,2,2,2,2,2,2,2,
2,2,2,2,2,2,2,2,2,2,2,2,2,2,2,2,2,2,2,2,2,2,2,2,2,2,2,4),(1.26001551649135,
1.26284451446193,1.26542193188058,1.26736166623112,1.26918712748262,1.27172340669052,
1.27832660600844,1.33456473152628,1.35351766662686,1.3685201584845,1.37087023057504,
1.3722727379463,1.37335235548607,1.37455894150873,1.37660418670428,1.38464884310749,
1.39978931893419,1.43948999071047,1.47074661031438,1.4749730877135,1.47749469695244,
1.47943264379949,1.48151499364467,1.48480305780564,1.49545682878334,1.51278459355559,
1.55307079622017,1.58006388566935,1.58296622023713,1.58435274436055,1.58542763385194,
1.58665750840069,1.5888078559456,1.59820399318063,1.64744184496253,1.68266035164975,
1.6869574819605,1.68949958715262,1.69144078984891,1.69351448780033,1.69676340204889,
1.70707184529562,1.72362869984322,1.75651610810682,1.77007085800938,1.77738388897131,
1.78171825412594,1.7929054640263,1.79506051127956,1.79641955692446,1.79749189118573,
1.7987402867533,1.80097527400743,1.81164770871794,1.83515299066214,1.89182920221108,
1.89838103212265,1.90090897907839,1.90273215532822,1.90467289611173,1.9072575226087,
1.91298289930623,1.93607392014222,1.97017197925383,1.99144317212453,2.00471566552533,
2.00698464570543,2.00836320108285,2.00943960284404,2.01065978181404,2.01276681091004,
2.02158118209909,2.03894711697881,2.088036472038,2.09416320705489,2.10833735473455,
2.11208659754359,2.11429251955556,2.11620533660696,2.11855166345124,2.12305607934971,
2.15614905299671,2.20248416037468,2.21664646325623,2.21895902652945,2.22035043524351,
2.22142844140827,2.22264098294256,2.22471353626541,2.23309050027175,2.24917193431417,
2.29150102610325,2.3189604848539,2.323093695616,2.32558780982689,2.32752127384201,
2.32961535701129,2.33295755780525,2.34411090339026,2.36258384167035,2.39106624725118,
2.42818853789256,2.43102581077384,2.43239946690034,2.43347296076776,2.43468607022011,
2.43678917277774,2.43938677858613,2.44479786710206,2.46022018619701,2.50129051292669,
2.53082929599935,2.53501930970744,2.53753008116393,2.53946609955538,2.54155269066825,
2.54486091369059,2.55569990330907,2.57344886292543,2.59366994486789),
 .UNSPECIFIED.);
#1892=B_SPLINE_CURVE_WITH_KNOTS('',3,(#182672,#182673,#182674,#182675,#182676,
#182677,#182678,#182679,#182680,#182681,#182682,#182683,#182684,#182685,
#182686,#182687,#182688,#182689,#182690,#182691,#182692,#182693,#182694,
#182695,#182696,#182697,#182698,#182699,#182700,#182701,#182702,#182703,
#182704,#182705,#182706,#182707,#182708,#182709,#182710,#182711,#182712,
#182713,#182714,#182715,#182716,#182717,#182718,#182719,#182720,#182721,
#182722,#182723,#182724,#182725,#182726,#182727,#182728,#182729,#182730,
#182731,#182732,#182733,#182734,#182735,#182736,#182737,#182738,#182739,
#182740,#182741,#182742,#182743,#182744,#182745,#182746,#182747,#182748,
#182749,#182750,#182751,#182752,#182753,#182754,#182755,#182756,#182757,
#182758,#182759,#182760,#182761,#182762,#182763,#182764,#182765,#182766,
#182767,#182768,#182769,#182770,#182771,#182772,#182773,#182774,#182775,
#182776,#182777,#182778,#182779,#182780,#182781,#182782,#182783,#182784,
#182785,#182786,#182787,#182788,#182789,#182790,#182791,#182792,#182793,
#182794,#182795,#182796,#182797,#182798,#182799,#182800,#182801,#182802,
#182803,#182804,#182805,#182806,#182807,#182808,#182809,#182810,#182811,
#182812,#182813,#182814,#182815,#182816,#182817,#182818,#182819,#182820,
#182821,#182822,#182823,#182824,#182825,#182826,#182827,#182828,#182829,
#182830,#182831,#182832,#182833,#182834,#182835,#182836,#182837,#182838,
#182839,#182840,#182841,#182842,#182843,#182844,#182845,#182846,#182847,
#182848,#182849,#182850,#182851,#182852,#182853,#182854,#182855,#182856,
#182857,#182858,#182859,#182860,#182861,#182862,#182863,#182864,#182865,
#182866,#182867,#182868,#182869,#182870,#182871,#182872,#182873,#182874,
#182875,#182876,#182877,#182878,#182879,#182880,#182881),.UNSPECIFIED.,
 .F.,.F.,(4,2,2,2,2,2,2,2,2,2,2,2,2,2,2,2,2,2,2,2,2,2,2,2,2,2,2,2,2,2,2,
2,2,2,2,2,2,2,2,2,2,2,2,2,2,2,2,2,2,2,2,2,2,2,2,2,2,2,2,2,2,2,2,2,2,2,2,
2,2,2,2,2,2,2,2,2,2,2,2,2,2,2,2,2,2,2,2,2,2,2,2,2,2,2,2,2,2,2,2,2,2,2,2,
2,4),(1.40817975905822,1.40954560836466,1.41147833542434,1.4135728609852,
1.4169184539589,1.42810815255206,1.44666701369632,1.49069805568445,1.49656816369503,
1.51244823619313,1.51506158397542,1.51640744662406,1.51747861959037,1.5187364022801,
1.52101503315593,1.53242866855974,1.55875512241244,1.6112342419393,1.61816336723805,
1.62103578226236,1.62282984573923,1.62479053757248,1.62749311437592,1.63388992499525,
1.68180129896859,1.72137451500311,1.72610764874689,1.72785087070757,1.7288768583589,
1.72996902180997,1.73147802835959,1.7350526619759,1.77422308970196,1.82298257769147,
1.83011269461674,1.83301845230588,1.8348185704141,1.83677417067401,1.83944853898156,
1.8456806887981,1.87272384959603,1.91345069505711,1.93614315338508,1.93899650061353,
1.94037323279208,1.94144690848067,1.94268258799221,1.94486020732928,1.95465260962522,
2.00353525341999,2.03864078667319,2.04293546732949,2.0454765242656,2.04741715709159,
2.04949046966397,2.05273924608953,2.06305117074383,2.07961731710115,2.11250768493825,
2.12707675561372,2.13238317907733,2.1484237110747,2.1510450917114,2.15239272010833,
2.15346399253881,2.15472035205142,2.1569927456024,2.16829981653343,2.19420740046896,
2.2472783874386,2.25416228532456,2.25702704823045,2.25881956398771,2.26078116089898,
2.26348974349135,2.26992326198122,2.29863196938254,2.34984137610625,2.36088058032047,
2.36302622378498,2.36438225858115,2.365454158525,2.36670427744037,2.36894792669211,
2.37976766044285,2.40381758281657,2.45963978372236,2.46627671827603,2.46881786574529,
2.47064426615729,2.47252035325782,2.47500472435949,2.47774309062016,2.48229537649571,
2.49162780734091,2.54226190779155,2.57203626856797,2.57495063884984,2.57633925129826,
2.57741407393816,2.57864198664061,2.58078448159155,2.59007765512967,2.60891632565383,
2.66742169168651),.UNSPECIFIED.);
#1893=B_SPLINE_CURVE_WITH_KNOTS('',3,(#182882,#182883,#182884,#182885),
 .UNSPECIFIED.,.F.,.F.,(4,4),(-16.7565928334374,-16.4074096477818),
 .UNSPECIFIED.);
#1894=B_SPLINE_CURVE_WITH_KNOTS('',3,(#182891,#182892,#182893,#182894,#182895,
#182896,#182897,#182898,#182899,#182900,#182901,#182902,#182903,#182904,
#182905,#182906),.UNSPECIFIED.,.F.,.F.,(4,2,2,2,2,2,2,4),(2.59336419963794,
2.64851730992168,2.65667985504919,2.65975097327022,2.66158220209397,2.66342608512958,
2.66571783163649,2.66778208221742),.UNSPECIFIED.);
#1895=B_SPLINE_CURVE_WITH_KNOTS('',3,(#182907,#182908,#182909,#182910,#182911,
#182912,#182913,#182914,#182915,#182916,#182917,#182918,#182919,#182920,
#182921,#182922,#182923,#182924,#182925,#182926,#182927,#182928,#182929,
#182930,#182931,#182932,#182933,#182934,#182935,#182936,#182937,#182938,
#182939,#182940,#182941,#182942,#182943,#182944,#182945,#182946,#182947,
#182948,#182949,#182950,#182951,#182952,#182953,#182954,#182955,#182956,
#182957,#182958,#182959,#182960,#182961,#182962,#182963,#182964,#182965,
#182966,#182967,#182968,#182969,#182970,#182971,#182972,#182973,#182974,
#182975,#182976,#182977,#182978,#182979,#182980,#182981,#182982,#182983,
#182984,#182985,#182986,#182987,#182988,#182989,#182990,#182991,#182992,
#182993,#182994,#182995,#182996,#182997,#182998,#182999,#183000,#183001,
#183002,#183003,#183004,#183005,#183006,#183007,#183008,#183009,#183010,
#183011,#183012,#183013,#183014,#183015,#183016,#183017,#183018,#183019,
#183020,#183021,#183022,#183023,#183024,#183025,#183026,#183027,#183028,
#183029,#183030,#183031,#183032,#183033,#183034,#183035,#183036,#183037,
#183038,#183039,#183040,#183041,#183042,#183043,#183044,#183045,#183046,
#183047,#183048,#183049,#183050,#183051,#183052,#183053,#183054,#183055,
#183056,#183057,#183058,#183059,#183060,#183061,#183062,#183063,#183064,
#183065,#183066,#183067,#183068,#183069,#183070,#183071,#183072,#183073,
#183074,#183075,#183076,#183077,#183078,#183079,#183080,#183081,#183082,
#183083,#183084,#183085,#183086,#183087,#183088,#183089,#183090,#183091,
#183092,#183093,#183094,#183095,#183096,#183097,#183098,#183099,#183100,
#183101,#183102,#183103,#183104,#183105,#183106,#183107,#183108,#183109,
#183110,#183111,#183112,#183113,#183114,#183115,#183116,#183117,#183118,
#183119,#183120,#183121,#183122,#183123,#183124,#183125,#183126,#183127,
#183128,#183129,#183130,#183131,#183132,#183133,#183134,#183135,#183136,
#183137,#183138,#183139,#183140,#183141,#183142,#183143,#183144,#183145,
#183146,#183147,#183148,#183149,#183150,#183151,#183152,#183153,#183154,
#183155,#183156),.UNSPECIFIED.,.F.,.F.,(4,2,2,2,2,2,2,2,2,2,2,2,2,2,2,2,
2,2,2,2,2,2,2,2,2,2,2,2,2,2,2,2,2,2,2,2,2,2,2,2,2,2,2,2,2,2,2,2,2,2,2,2,
2,2,2,2,2,2,2,2,2,2,2,2,2,2,2,2,2,2,2,2,2,2,2,2,2,2,2,2,2,2,2,2,2,2,2,2,
2,2,2,2,2,2,2,2,2,2,2,2,2,2,2,2,2,2,2,2,2,2,2,2,2,2,2,2,2,2,2,2,2,2,2,2,
4),(0.000823822472317207,0.00402591699170803,0.0105189260068452,0.0602232793173974,
0.0858540471813482,0.0970894386700358,0.0993576796542626,0.100613114722003,
0.10168444953284,0.103033229329788,0.105659981548195,0.121848831178235,
0.172512225735023,0.190330720635742,0.20120062365209,0.203653936590393,
0.20593359915671,0.205948682438116,0.205964392968151,0.20598077332524,0.205997870265091,
0.206015735165232,0.206034424666561,0.20605400146026,0.206074535004654,
0.206096102575133,0.206118790454896,0.206142695340538,0.206167925992387,
0.206194605303977,0.206222872714743,0.206252887251777,0.206284831231239,
0.206318914962662,0.206355382557691,0.208228529534964,0.210616080072911,
0.215085114556155,0.241811493627869,0.285244653545143,0.301115650922831,
0.309417858485812,0.311484081130193,0.312695075444056,0.313773183340093,
0.315166628301309,0.317486560700479,0.331786262924069,0.380028863003848,
0.40816513095325,0.414530534597715,0.417227561634384,0.419187052596701,
0.420981972978595,0.423860023918919,0.430824699012687,0.482805612174114,
0.509509434687927,0.521016544977097,0.523300338645433,0.524559168456589,
0.525630246915027,0.526974699096923,0.529581283887988,0.54528371603,0.551463612770259,
0.555216497853862,0.565595683086056,0.598425173069379,0.614951374796059,
0.625246303822338,0.628493163534855,0.630566086895852,0.632506942279414,
0.635049139215031,0.639347682473988,0.674733840529545,0.723911451889856,
0.733226330126461,0.735370560884082,0.736598931382085,0.737673810555959,
0.739062031216454,0.741973955552941,0.773378916617537,0.777667782332219,
0.810468023444918,0.833121868059516,0.838788741184759,0.841362599484792,
0.843301598716053,0.845127794038316,0.847667377626918,0.854292603213663,
0.910304071294489,0.934266497183649,0.945062648923812,0.947305179451994,
0.948555190850898,0.949627313461724,0.950984029300079,0.953131498578615,
0.964196586743705,1.0153361162577,1.04406147028494,1.05049807973324,1.05320752185898,
1.05516958322811,1.05696241852631,1.05982745218169,1.06671072952063,1.11985813809552,
1.14575589564192,1.15706084974852,1.15933350640645,1.16059008915057,1.16166161579937,
1.163009634232,1.16563194964916,1.18168004992619,1.1857909545577,1.20148300101392,
1.23437115886928,1.25715922870071,1.26001551649135),.UNSPECIFIED.);
#1896=B_SPLINE_CURVE_WITH_KNOTS('',3,(#183158,#183159,#183160,#183161,#183162,
#183163,#183164,#183165,#183166,#183167),.UNSPECIFIED.,.F.,.F.,(4,1,1,1,
1,1,1,4),(-22.6905949549614,-21.9744018991612,-20.9755654491994,-19.9767289992375,
-18.9778925492756,-17.9790560993137,-16.9802196493519,-16.7565928334374),
 .UNSPECIFIED.);
#1897=B_SPLINE_CURVE_WITH_KNOTS('',3,(#183168,#183169,#183170,#183171,#183172,
#183173,#183174,#183175,#183176,#183177,#183178,#183179,#183180,#183181,
#183182,#183183,#183184,#183185,#183186,#183187),.UNSPECIFIED.,.F.,.F.,
(4,2,2,2,2,2,2,2,2,4),(0.000629315580650519,0.0163202363040628,0.0544201888437156,
0.0580035127267242,0.0595138353816897,0.0606060562445949,0.0616313318818364,
0.0633718340587686,0.0680887842443331,0.0747327161871493),.UNSPECIFIED.);
#1898=B_SPLINE_CURVE_WITH_KNOTS('',3,(#183192,#183193,#183194,#183195,#183196,
#183197,#183198,#183199,#183200,#183201,#183202,#183203,#183204,#183205,
#183206,#183207,#183208,#183209,#183210,#183211,#183212,#183213,#183214,
#183215,#183216,#183217,#183218,#183219,#183220,#183221,#183222,#183223,
#183224,#183225,#183226,#183227,#183228,#183229,#183230,#183231,#183232,
#183233,#183234,#183235,#183236,#183237,#183238,#183239,#183240,#183241,
#183242,#183243,#183244,#183245,#183246,#183247,#183248,#183249,#183250,
#183251,#183252,#183253,#183254,#183255,#183256,#183257,#183258,#183259,
#183260,#183261,#183262,#183263,#183264,#183265,#183266,#183267,#183268,
#183269,#183270,#183271,#183272,#183273,#183274,#183275,#183276,#183277,
#183278,#183279,#183280,#183281,#183282,#183283,#183284,#183285,#183286,
#183287,#183288,#183289,#183290,#183291,#183292,#183293,#183294,#183295,
#183296,#183297,#183298,#183299,#183300,#183301,#183302,#183303,#183304,
#183305,#183306,#183307,#183308,#183309,#183310,#183311,#183312,#183313,
#183314,#183315,#183316,#183317,#183318,#183319,#183320,#183321,#183322,
#183323,#183324,#183325,#183326,#183327,#183328,#183329,#183330,#183331,
#183332,#183333,#183334,#183335,#183336,#183337,#183338,#183339,#183340,
#183341,#183342,#183343,#183344,#183345,#183346,#183347,#183348,#183349,
#183350,#183351,#183352,#183353,#183354,#183355,#183356,#183357,#183358,
#183359,#183360,#183361,#183362,#183363,#183364,#183365,#183366,#183367,
#183368,#183369,#183370,#183371,#183372,#183373,#183374,#183375,#183376,
#183377,#183378,#183379,#183380,#183381,#183382,#183383,#183384,#183385,
#183386,#183387,#183388,#183389,#183390,#183391,#183392,#183393,#183394,
#183395,#183396,#183397,#183398,#183399,#183400,#183401,#183402,#183403,
#183404,#183405,#183406,#183407,#183408,#183409,#183410,#183411,#183412,
#183413,#183414,#183415,#183416,#183417,#183418,#183419,#183420,#183421,
#183422,#183423,#183424,#183425,#183426,#183427,#183428,#183429,#183430,
#183431),.UNSPECIFIED.,.F.,.F.,(4,2,2,2,2,2,2,2,2,2,2,2,2,2,2,2,2,2,2,2,
2,2,2,2,2,2,2,2,2,2,2,2,2,2,2,2,2,2,2,2,2,2,2,2,2,2,2,2,2,2,2,2,2,2,2,2,
2,2,2,2,2,2,2,2,2,2,2,2,2,2,2,2,2,2,2,2,2,2,2,2,2,2,2,2,2,2,2,2,2,2,2,2,
2,2,2,2,2,2,2,2,2,2,2,2,2,2,2,2,2,2,2,2,2,2,2,2,2,2,2,4),(1.25983790857793,
1.27797720523257,1.28156303790082,1.28307395792435,1.28416643896761,1.28519182205558,
1.28693221482015,1.29164717042241,1.33205648703802,1.3339458948937,1.37777069272836,
1.38499259263956,1.387913812067,1.38971681704495,1.39167029368026,1.3943323254265,
1.40049301998838,1.42695877731456,1.46587466816546,1.47401787505932,1.49129054790315,
1.49395903095881,1.49531683613192,1.49638891725887,1.49763785070098,1.49987587301008,
1.51060187884258,1.53430546558711,1.56167740146777,1.59360713178078,1.59784660940097,
1.60037174209123,1.6023099338345,1.60439013380503,1.60766969773444,1.61825127924484,
1.63541789455111,1.68115828269663,1.6879204758484,1.70336710376258,1.70573503387373,
1.70714261744554,1.70822277246688,1.70942623007516,1.71145805126151,1.71934859563784,
1.73406464165688,1.76310434016164,1.80549060627848,1.80978360014269,1.81232430373996,
1.81426503845648,1.81633882064678,1.81958908698159,1.82991211246918,1.84650218830943,
1.8794142093178,1.89545946012091,1.89928711031461,1.91528402609327,1.91790301058041,
1.91925020518782,1.92032154387906,1.92157845326514,1.92385308013381,1.93519666654688,
1.96124611680367,2.01412103995842,2.0210210133345,2.02388855897214,2.02568168196252,
2.02764303205819,2.03034960299055,2.0367704311123,2.06537054533334,2.11662171043,
2.12774598260801,2.12989698711648,2.13125471052477,2.13232681754745,2.13357588503383,
2.13581440592864,2.1465476932325,2.17027746553897,2.22659602015694,2.23318401377596,
2.23571755929501,2.23754205871452,2.23948169940866,2.24206057070796,2.24775553250463,
2.27062223697597,2.30358524581222,2.32245679168493,2.3267697713123,2.33956211858517,
2.34180652401039,2.34319245835702,2.34426701265935,2.34549664057627,2.34764687852778,
2.35704757590243,2.40626454393015,2.44146541127269,2.44614418107161,2.44857826853674,
2.45044818795255,2.45253358762694,2.45471588495329,2.45793044457636,2.49302281158196,
2.54885369014608,2.55313420694314,2.55480687508637,2.55581911573968,2.5569212788574,
2.55848527009532,2.56239199961126,2.5815475823925,2.59336419963794),
 .UNSPECIFIED.);
#1899=B_SPLINE_CURVE_WITH_KNOTS('',3,(#183432,#183433,#183434,#183435,#183436,
#183437,#183438,#183439,#183440,#183441,#183442,#183443,#183444,#183445,
#183446,#183447,#183448,#183449,#183450,#183451,#183452,#183453,#183454,
#183455,#183456,#183457,#183458,#183459,#183460,#183461,#183462,#183463,
#183464,#183465,#183466,#183467,#183468,#183469,#183470,#183471,#183472,
#183473,#183474,#183475,#183476,#183477,#183478,#183479,#183480,#183481,
#183482,#183483,#183484,#183485,#183486,#183487,#183488,#183489,#183490,
#183491,#183492,#183493,#183494,#183495,#183496,#183497,#183498,#183499,
#183500,#183501,#183502,#183503,#183504,#183505,#183506,#183507,#183508,
#183509,#183510,#183511,#183512,#183513,#183514,#183515,#183516,#183517,
#183518,#183519,#183520,#183521,#183522,#183523,#183524,#183525,#183526,
#183527,#183528,#183529,#183530,#183531,#183532,#183533,#183534,#183535,
#183536,#183537,#183538,#183539,#183540,#183541,#183542,#183543,#183544,
#183545,#183546,#183547,#183548,#183549,#183550,#183551,#183552,#183553,
#183554,#183555,#183556,#183557,#183558,#183559,#183560,#183561,#183562,
#183563,#183564,#183565,#183566,#183567,#183568,#183569,#183570,#183571,
#183572,#183573,#183574,#183575,#183576,#183577,#183578,#183579,#183580,
#183581,#183582,#183583,#183584,#183585,#183586,#183587,#183588,#183589,
#183590,#183591,#183592,#183593,#183594,#183595,#183596,#183597,#183598,
#183599,#183600,#183601,#183602,#183603,#183604,#183605,#183606,#183607,
#183608,#183609,#183610,#183611,#183612,#183613,#183614,#183615,#183616,
#183617,#183618,#183619,#183620,#183621,#183622,#183623,#183624,#183625,
#183626,#183627,#183628,#183629,#183630,#183631,#183632,#183633,#183634,
#183635,#183636,#183637,#183638,#183639,#183640,#183641,#183642,#183643,
#183644,#183645,#183646,#183647),.UNSPECIFIED.,.F.,.F.,(4,2,2,2,2,2,2,2,
2,2,2,2,2,2,2,2,2,2,2,2,2,2,2,2,2,2,2,2,2,2,2,2,2,2,2,2,2,2,2,2,2,2,2,2,
2,2,2,2,2,2,2,2,2,2,2,2,2,2,2,2,2,2,2,2,2,2,2,2,2,2,2,2,2,2,2,2,2,2,2,2,
2,2,2,2,2,2,2,2,2,2,2,2,2,2,2,2,2,2,2,2,2,2,2,2,2,2,2,4),(0.0747327161871493,
0.112806263249665,0.136932016893629,0.151520374868938,0.160861100382372,
0.163933560938048,0.166006632969609,0.16794710999224,0.170488064463653,
0.174782832519329,0.209904538757292,0.258831792828393,0.26859796551639,
0.270773729244168,0.272008956847566,0.273082629072402,0.274459858393428,
0.277315979291488,0.30012692356418,0.345792858012144,0.362352409594568,
0.372662291999832,0.375910767549687,0.377983977490443,0.379924577789205,
0.382465685298002,0.386760693218058,0.421881873366653,0.470803718405356,
0.480580664350534,0.48275726154936,0.483992721111619,0.485066440616442,
0.486443528863192,0.489298663294989,0.512064187029572,0.524919300846613,
0.557770477962619,0.574321506103386,0.584627831901054,0.587876118415675,
0.589949431622159,0.591890285885263,0.594431952936962,0.598728415445979,
0.633929687462879,0.683101121258225,0.692593317730559,0.694750293473788,
0.69598151626546,0.697056006802251,0.698439932258856,0.700677296610982,
0.713330659266395,0.763174181018253,0.791498895283811,0.797887510368748,
0.800588778804796,0.802549308251866,0.80434376940163,0.807218000632127,
0.814157564220036,0.866538272552775,0.892970541954052,0.904410644615518,
0.906690959398448,0.907949177114371,0.909020523982913,0.910366315766807,
0.912978431743436,0.928753383487914,0.929617580563808,0.973975024025688,
1.003346825627,1.00985994589294,1.01258225926934,1.01454668941625,1.01633693092621,
1.01918752616203,1.0259831902078,1.08019676365256,1.10536228031066,1.11647832368368,
1.11874002194943,1.11999423222078,1.12106598442386,1.12241715673457,1.12505409203379,
1.14148619742741,1.19207769209147,1.2097902620344,1.22061454401318,1.2239212461215,
1.22600756770438,1.22794381133236,1.23045554869039,1.23464868172609,1.26439484972425,
1.30534135019042,1.32782242906259,1.33048602114964,1.33182494466666,1.33279298286869,
1.33401667433845,1.33613933140971,1.34515862481949,1.36314493821362,1.40835625272083),
 .UNSPECIFIED.);
#1900=B_SPLINE_CURVE_WITH_KNOTS('',3,(#183653,#183654,#183655,#183656,#183657,
#183658),.UNSPECIFIED.,.F.,.F.,(4,2,4),(2.59396194766411,2.60938231110621,
2.6684204151543),.UNSPECIFIED.);
#1901=B_SPLINE_CURVE_WITH_KNOTS('',3,(#183659,#183660,#183661,#183662,#183663,
#183664,#183665,#183666,#183667,#183668,#183669,#183670,#183671,#183672,
#183673,#183674,#183675,#183676,#183677,#183678,#183679,#183680,#183681,
#183682,#183683,#183684,#183685,#183686,#183687,#183688,#183689,#183690,
#183691,#183692,#183693,#183694,#183695,#183696,#183697,#183698,#183699,
#183700,#183701,#183702,#183703,#183704,#183705,#183706,#183707,#183708,
#183709,#183710,#183711,#183712,#183713,#183714,#183715,#183716,#183717,
#183718,#183719,#183720,#183721,#183722,#183723,#183724,#183725,#183726,
#183727,#183728,#183729,#183730,#183731,#183732,#183733,#183734,#183735,
#183736,#183737,#183738,#183739,#183740,#183741,#183742,#183743,#183744,
#183745,#183746,#183747,#183748,#183749,#183750,#183751,#183752,#183753,
#183754,#183755,#183756,#183757,#183758,#183759,#183760,#183761,#183762,
#183763,#183764,#183765,#183766,#183767,#183768,#183769,#183770,#183771,
#183772,#183773,#183774,#183775,#183776,#183777,#183778,#183779,#183780,
#183781,#183782,#183783,#183784,#183785,#183786,#183787,#183788,#183789,
#183790,#183791,#183792,#183793,#183794,#183795,#183796,#183797,#183798,
#183799,#183800,#183801,#183802,#183803,#183804,#183805,#183806,#183807,
#183808,#183809,#183810,#183811,#183812,#183813,#183814,#183815,#183816,
#183817,#183818,#183819,#183820,#183821,#183822,#183823,#183824,#183825,
#183826,#183827,#183828,#183829,#183830,#183831,#183832,#183833,#183834,
#183835,#183836,#183837,#183838,#183839,#183840,#183841,#183842,#183843,
#183844,#183845,#183846,#183847,#183848,#183849,#183850,#183851,#183852,
#183853,#183854,#183855,#183856,#183857,#183858,#183859,#183860,#183861,
#183862,#183863,#183864,#183865,#183866,#183867,#183868,#183869,#183870,
#183871,#183872,#183873,#183874,#183875,#183876,#183877,#183878,#183879,
#183880),.UNSPECIFIED.,.F.,.F.,(4,2,2,2,2,2,2,2,2,2,2,2,2,2,2,2,2,2,2,2,
2,2,2,2,2,2,2,2,2,2,2,2,2,2,2,2,2,2,2,2,2,2,2,2,2,2,2,2,2,2,2,2,2,2,2,2,
2,2,2,2,2,2,2,2,2,2,2,2,2,2,2,2,2,2,2,2,2,2,2,2,2,2,2,2,2,2,2,2,2,2,2,2,
2,2,2,2,2,2,2,2,2,2,2,2,2,2,2,2,2,2,4),(0.000810724389290951,0.00554261375580484,
0.00881069691195324,0.0102445769783141,0.011318985848088,0.0123418025241498,
0.0133650045898498,0.0148060212231952,0.0186526235771321,0.0263910153305198,
0.0811772808672639,0.107629387837393,0.113788020924836,0.116449253515829,
0.118402180529452,0.120204708031169,0.123125208371619,0.130345635359972,
0.174351807037448,0.207135137809993,0.215734594940256,0.219348857655954,
0.221296373882804,0.22257585593342,0.223774129654423,0.224825662411511,
0.226202815743788,0.229059222189351,0.265112317068062,0.29780688404151,
0.32030387335704,0.325948779676435,0.3285181613556,0.330456027760932,0.332282802427431,
0.334825834325865,0.341475778654321,0.397208499776815,0.421336622553385,
0.432176261672697,0.434420973828269,0.43567124200945,0.436742993562836,
0.438098481507766,0.440845295152296,0.459441566198162,0.508226353031946,
0.525602943175706,0.536278201585356,0.53956778574421,0.541649913854862,
0.543586834722163,0.546105943487939,0.550325687766331,0.581324838595276,
0.621242465250727,0.636423823917826,0.644481377707186,0.646527183489368,
0.647733593571336,0.648812709538806,0.650214101656203,0.652561315377136,
0.667512518906407,0.67511482761232,0.688554352914632,0.721406441682432,
0.744146843191376,0.749824902396771,0.75240052315621,0.754339504883303,
0.756164697307141,0.758701306467865,0.765309481953417,0.821463247846527,
0.845321199919284,0.856088220064211,0.858328677587908,0.859578093584948,
0.860650051457819,0.86200700293403,0.864671715982247,0.881846600474784,
0.927339625368517,0.9551961863153,0.961527955279621,0.964219336130375,0.966177888532615,
0.967974140966102,0.970859137333597,0.977865251631405,1.02920028612628,
1.05636942333767,1.06799185033315,1.07028217301201,1.07154245580033,1.07261347847955,
1.07395622287387,1.07655472432443,1.09206545116655,1.09863982300736,1.1400175365505,
1.16728220599751,1.17354198318758,1.17622110404514,1.17817754045073,1.17997659153028,
1.18287654647134,1.1899719991594,1.23960035131516,1.25983790857793),
 .UNSPECIFIED.);
#1902=B_SPLINE_CURVE_WITH_KNOTS('',3,(#183882,#183883,#183884,#183885,#183886,
#183887,#183888,#183889,#183890,#183891,#183892,#183893,#183894,#183895,
#183896,#183897,#183898,#183899,#183900,#183901,#183902,#183903,#183904,
#183905,#183906,#183907,#183908,#183909,#183910,#183911,#183912,#183913,
#183914,#183915,#183916,#183917,#183918,#183919,#183920,#183921,#183922,
#183923,#183924,#183925,#183926,#183927,#183928,#183929,#183930,#183931,
#183932,#183933,#183934,#183935,#183936,#183937,#183938,#183939,#183940,
#183941,#183942,#183943,#183944,#183945,#183946,#183947,#183948,#183949,
#183950,#183951,#183952,#183953,#183954,#183955,#183956,#183957,#183958,
#183959,#183960,#183961,#183962,#183963,#183964,#183965,#183966,#183967,
#183968,#183969,#183970,#183971,#183972,#183973,#183974,#183975,#183976,
#183977,#183978,#183979,#183980,#183981,#183982,#183983,#183984,#183985,
#183986,#183987,#183988,#183989,#183990,#183991,#183992,#183993,#183994,
#183995,#183996,#183997,#183998,#183999,#184000,#184001,#184002,#184003,
#184004,#184005,#184006,#184007,#184008,#184009,#184010,#184011,#184012,
#184013,#184014,#184015,#184016,#184017,#184018,#184019,#184020,#184021,
#184022,#184023,#184024,#184025,#184026,#184027,#184028,#184029,#184030,
#184031,#184032,#184033,#184034,#184035,#184036,#184037,#184038,#184039,
#184040,#184041,#184042,#184043,#184044,#184045,#184046,#184047,#184048,
#184049,#184050,#184051,#184052,#184053,#184054,#184055,#184056,#184057,
#184058,#184059,#184060,#184061,#184062,#184063,#184064,#184065,#184066,
#184067,#184068,#184069,#184070,#184071,#184072,#184073,#184074,#184075,
#184076,#184077,#184078,#184079,#184080,#184081,#184082,#184083,#184084,
#184085,#184086,#184087,#184088,#184089,#184090,#184091,#184092,#184093,
#184094,#184095,#184096,#184097,#184098,#184099,#184100,#184101,#184102,
#184103,#184104,#184105,#184106,#184107,#184108,#184109),.UNSPECIFIED.,
 .F.,.F.,(4,2,2,2,2,2,2,2,2,2,2,2,2,2,2,2,2,2,2,2,2,2,2,2,2,2,2,2,2,2,2,
2,2,2,2,2,2,2,2,2,2,2,2,2,2,2,2,2,2,2,2,2,2,2,2,2,2,2,2,2,2,2,2,2,2,2,2,
2,2,2,2,2,2,2,2,2,2,2,2,2,2,2,2,2,2,2,2,2,2,2,2,2,2,2,2,2,2,2,2,2,2,2,2,
2,2,2,2,2,2,2,2,2,2,4),(1.40835625272083,1.41336368806739,1.43116872566781,
1.43484842293011,1.43723220416798,1.43914781687456,1.4413267132969,1.44505177945364,
1.46045916759543,1.51179701767642,1.53947811685562,1.54238526115338,1.54377266130752,
1.54484757386111,1.546076740306,1.54822412401745,1.55758038234137,1.6068490786857,
1.64207475295534,1.64637169417152,1.6489136504204,1.65085471803946,1.65292825100875,
1.65617686359758,1.66648398593569,1.68303837202102,1.71592233387626,1.72936951776526,
1.73695626675539,1.75195389546679,1.75430351576105,1.75570578880263,1.75678524748666,
1.75799168003349,1.76003671720068,1.76808121533805,1.78322228438951,1.82293243544293,
1.85416626673713,1.85839175519206,1.86091289225587,1.86285054494295,1.8649326461682,
1.86822046079938,1.87887468072414,1.89620441513131,1.9444306171971,1.94873390689186,
1.95196293469188,1.96419552942283,1.96641049758499,1.96778768894949,1.96886155053835,
1.97009725167077,1.97227444775361,1.98205730690306,2.03095657979584,2.0660685568434,
2.07036387814959,2.0729053149221,2.07484623859035,2.0769198628265,2.08016913003967,
2.09048264193443,2.10705139361886,2.13994656134181,2.15456287475828,2.15981787996429,
2.17586545609174,2.17848752879942,2.17983542309108,2.18090685095587,2.18216332356894,
2.18443578445295,2.19574038045612,2.22163585464488,2.27473613504417,2.28161925106378,
2.28448410119294,2.28627679100996,2.28823867437865,2.29094782844773,2.29738353678552,
2.30627119379578,2.35748924472459,2.38749103980191,2.39040567361415,2.39179444617781,
2.39286940842842,2.3940974981232,2.39624034450607,2.40553570108986,2.4243798824607,
2.47057382382192,2.47203375715982,2.4910579469055,2.49481781987104,2.49722617337713,
2.4991438712783,2.50094123856844,2.50403405192422,2.51357919660978,2.52858022240595,
2.55087382072599,2.59692596171914,2.60157163495471,2.60330156075396,2.60432493251932,
2.6054188161644,2.60693747948808,2.61056863437898,2.6156799188112,2.62984817881187,
2.66748302574586),.UNSPECIFIED.);
#1903=B_SPLINE_CURVE_WITH_KNOTS('',3,(#184110,#184111,#184112,#184113,#184114,
#184115,#184116,#184117,#184118,#184119,#184120,#184121,#184122,#184123,
#184124,#184125,#184126,#184127,#184128,#184129),.UNSPECIFIED.,.F.,.F.,
(4,2,2,2,2,2,2,2,2,4),(0.000704184852116804,0.0257176022094043,0.0359848500666596,
0.0390635722060811,0.0411898678713681,0.0432710177822686,0.0452083783979804,
0.0477299820330082,0.0519581544184686,0.0751489451347217),.UNSPECIFIED.);
#1904=B_SPLINE_CURVE_WITH_KNOTS('',3,(#184134,#184135,#184136,#184137,#184138,
#184139,#184140,#184141,#184142,#184143,#184144,#184145,#184146,#184147,
#184148,#184149,#184150,#184151,#184152,#184153,#184154,#184155,#184156,
#184157,#184158,#184159,#184160,#184161,#184162,#184163,#184164,#184165,
#184166,#184167,#184168,#184169,#184170,#184171,#184172,#184173,#184174,
#184175,#184176,#184177,#184178,#184179,#184180,#184181,#184182,#184183,
#184184,#184185,#184186,#184187,#184188,#184189,#184190,#184191,#184192,
#184193,#184194,#184195,#184196,#184197,#184198,#184199,#184200,#184201,
#184202,#184203,#184204,#184205,#184206,#184207,#184208,#184209,#184210,
#184211,#184212,#184213,#184214,#184215,#184216,#184217,#184218,#184219,
#184220,#184221,#184222,#184223,#184224,#184225,#184226,#184227,#184228,
#184229,#184230,#184231,#184232,#184233,#184234,#184235,#184236,#184237,
#184238,#184239,#184240,#184241,#184242,#184243,#184244,#184245,#184246,
#184247,#184248,#184249,#184250,#184251,#184252,#184253,#184254,#184255,
#184256,#184257,#184258,#184259,#184260,#184261,#184262,#184263,#184264,
#184265,#184266,#184267,#184268,#184269,#184270,#184271,#184272,#184273,
#184274,#184275,#184276,#184277,#184278,#184279,#184280,#184281,#184282,
#184283,#184284,#184285,#184286,#184287,#184288,#184289,#184290,#184291,
#184292,#184293,#184294,#184295,#184296,#184297,#184298,#184299,#184300,
#184301,#184302,#184303,#184304,#184305,#184306,#184307,#184308,#184309,
#184310,#184311,#184312,#184313,#184314,#184315,#184316,#184317,#184318,
#184319,#184320,#184321,#184322,#184323,#184324,#184325,#184326,#184327,
#184328,#184329,#184330,#184331,#184332,#184333,#184334,#184335,#184336,
#184337,#184338,#184339,#184340,#184341,#184342,#184343,#184344,#184345,
#184346,#184347,#184348,#184349,#184350,#184351,#184352,#184353,#184354,
#184355,#184356,#184357,#184358,#184359,#184360,#184361,#184362,#184363,
#184364,#184365,#184366,#184367,#184368,#184369,#184370,#184371,#184372,
#184373,#184374,#184375,#184376,#184377,#184378,#184379,#184380,#184381,
#184382,#184383,#184384,#184385,#184386,#184387,#184388,#184389,#184390,
#184391,#184392,#184393,#184394,#184395,#184396,#184397,#184398,#184399,
#184400,#184401,#184402,#184403,#184404,#184405,#184406,#184407,#184408,
#184409),.UNSPECIFIED.,.F.,.F.,(4,2,2,2,2,2,2,2,2,2,2,2,2,2,2,2,2,2,2,2,
2,2,2,2,2,2,2,2,2,2,2,2,2,2,2,2,2,2,2,2,2,2,2,2,2,2,2,2,2,2,2,2,2,2,2,2,
2,2,2,2,2,2,2,2,2,2,2,2,2,2,2,2,2,2,2,2,2,2,2,2,2,2,2,2,2,2,2,2,2,2,2,2,
2,2,2,2,2,2,2,2,2,2,2,2,2,2,2,2,2,2,2,2,2,2,2,2,2,2,2,2,2,2,2,2,2,2,2,2,
2,2,2,2,2,2,2,2,2,4),(1.26015660703498,1.26850353839846,1.29388141845515,
1.29815223390653,1.30044982624054,1.30234294688901,1.30458374931348,1.30848301244928,
1.32439211594051,1.3346146286344,1.37390000555279,1.40248494808154,1.40539757889374,
1.4067861653548,1.40786133728485,1.40909006222754,1.41123494397423,1.42055345384096,
1.46973117631598,1.50510123298155,1.50940052081475,1.51194334691486,1.51388478037683,
1.51595841496646,1.51920658323939,1.52950721437933,1.54604634616807,1.57359384006365,
1.58973745550778,1.60082107001498,1.6150540366232,1.61737054723746,1.61876321784715,
1.61984151672186,1.62105362144081,1.62312371831444,1.63146796498687,1.64745439110005,
1.68977182301542,1.71738179358572,1.72151940303762,1.72401499119278,1.72594889825981,
1.72804276337901,1.73138310540736,1.74251617589424,1.76094094499302,1.80770403810387,
1.81238790076397,1.82704125409291,1.82937668556193,1.83077491997594,1.83185397143872,
1.83306295822877,1.83511895173284,1.84329148009806,1.85878990810227,1.90014881820821,
1.92932982664744,1.93350872854028,1.93601645369324,1.93795224668422,1.94004069592337,
1.9433563643061,1.95426036548847,1.97215678748334,2.02283065706109,2.03896711092047,
2.04159626732589,2.04294587667124,2.04401765752629,2.04527337487705,2.04754150624368,
2.05876435009312,2.08433662102447,2.13792608376044,2.14477313424653,2.14763247031026,
2.14942447106373,2.15138782627842,2.15410310544928,2.16057284687703,2.21477965760947,
2.22580484585943,2.25070462983722,2.25359339765226,2.25497732615041,2.25605200636901,
2.25728366581576,2.25944191075616,2.26894803191861,2.31809352045741,2.3532860024778,
2.35758302448765,2.36012517427007,2.36206647359919,2.36414033545589,2.36738963318007,
2.37770036072059,2.39426189888552,2.42798255702194,2.46276561958121,2.46564472786883,
2.46702673969045,2.46806957966137,2.46807433654214,2.46807900997116,2.46808360166098,
2.46808811350254,2.46809254731902,2.46809690480249,2.46810118785428,2.46810539778791,
2.46810953607837,2.4681136044994,2.46811760436237,2.46812153721469,2.46812540446117,
2.46812900140162,2.46813258499554,2.46813615516565,2.46813971186342,2.46814325546488,
2.46936716343783,2.47067885718657,2.47270356797895,2.47652077094661,2.48580997197465,
2.52380810757076,2.53846120539619,2.56559448357076,2.5697198083356,2.57221178784583,
2.57414515533493,2.57624069134386,2.57958858900748,2.59079256646039,2.59396194766411),
 .UNSPECIFIED.);
#1905=B_SPLINE_CURVE_WITH_KNOTS('',3,(#184410,#184411,#184412,#184413,#184414,
#184415,#184416,#184417,#184418,#184419,#184420,#184421,#184422,#184423,
#184424,#184425,#184426,#184427,#184428,#184429,#184430,#184431,#184432,
#184433,#184434,#184435,#184436,#184437,#184438,#184439,#184440,#184441,
#184442,#184443,#184444,#184445,#184446,#184447,#184448,#184449,#184450,
#184451,#184452,#184453,#184454,#184455,#184456,#184457,#184458,#184459,
#184460,#184461,#184462,#184463,#184464,#184465,#184466,#184467,#184468,
#184469,#184470,#184471,#184472,#184473,#184474,#184475,#184476,#184477,
#184478,#184479,#184480,#184481,#184482,#184483,#184484,#184485,#184486,
#184487,#184488,#184489,#184490,#184491,#184492,#184493,#184494,#184495,
#184496,#184497,#184498,#184499,#184500,#184501,#184502,#184503,#184504,
#184505,#184506,#184507,#184508,#184509,#184510,#184511,#184512,#184513,
#184514,#184515,#184516,#184517,#184518,#184519,#184520,#184521,#184522,
#184523,#184524,#184525,#184526,#184527,#184528,#184529,#184530,#184531,
#184532,#184533,#184534,#184535,#184536,#184537,#184538,#184539,#184540,
#184541,#184542,#184543,#184544,#184545,#184546,#184547,#184548,#184549,
#184550,#184551,#184552,#184553,#184554,#184555,#184556,#184557,#184558,
#184559,#184560,#184561,#184562,#184563,#184564,#184565,#184566,#184567,
#184568,#184569,#184570,#184571,#184572,#184573,#184574,#184575,#184576,
#184577,#184578,#184579,#184580,#184581,#184582,#184583,#184584,#184585,
#184586,#184587,#184588,#184589,#184590,#184591,#184592,#184593,#184594,
#184595,#184596,#184597,#184598,#184599,#184600,#184601,#184602,#184603,
#184604,#184605,#184606,#184607,#184608,#184609,#184610,#184611,#184612,
#184613,#184614,#184615,#184616,#184617,#184618,#184619,#184620,#184621,
#184622,#184623,#184624,#184625,#184626,#184627,#184628,#184629,#184630,
#184631,#184632,#184633,#184634,#184635,#184636,#184637,#184638,#184639),
 .UNSPECIFIED.,.F.,.F.,(4,2,2,2,2,2,2,2,2,2,2,2,2,2,2,2,2,2,2,2,2,2,2,2,
2,2,2,2,2,2,2,2,2,2,2,2,2,2,2,2,2,2,2,2,2,2,2,2,2,2,2,2,2,2,2,2,2,2,2,2,
2,2,2,2,2,2,2,2,2,2,2,2,2,2,2,2,2,2,2,2,2,2,2,2,2,2,2,2,2,2,2,2,2,2,2,2,
2,2,2,2,2,2,2,2,2,2,2,2,2,2,2,2,2,2,4),(0.0751489451347217,0.0833507687398273,
0.108693897814586,0.136627086573777,0.145910886645299,0.148052581554333,
0.149280244099893,0.150354989768126,0.151743679457158,0.153997484253236,
0.166976862044332,0.188667672851665,0.215384456391813,0.236981735410283,
0.245198580224,0.251207962177669,0.253835108106743,0.25579166492443,0.257590154255876,
0.260487716487645,0.267569839542336,0.317778483894999,0.355565284018007,
0.359164609079005,0.360677739990485,0.361770526142713,0.362795167290526,
0.364532111062224,0.369224987747128,0.410119178514221,0.4567277765047,0.463120318208575,
0.465821987649755,0.467782348658663,0.469576338621285,0.472449122864454,
0.479381619562274,0.531831153367774,0.558205057179414,0.569629706952713,
0.571908878575761,0.573166723471649,0.574237908965008,0.575583696383888,
0.578196384936595,0.594048605625068,0.598801103315708,0.614070826201948,
0.646946930371511,0.663528806028483,0.673848987832411,0.677098794684803,
0.679172394756504,0.681113037550354,0.683653735258197,0.687947007613558,
0.730347335586221,0.759403786114085,0.774125645839017,0.782017432494795,
0.784049295302067,0.785252716774208,0.786332803687113,0.787740237111621,
0.790107777879002,0.805548576264205,0.812259402678407,0.826060078339225,
0.858920786798176,0.875483084096869,0.88579453543023,0.889043430538638,
0.891116890278173,0.893057711776927,0.895599090725547,0.89989451662427,
0.935013736138574,0.98392289543762,0.993722764407131,0.995901100414189,
0.997137029899902,0.998210827162394,0.99958758320526,1.00244054459879,1.02510735550418,
1.0380664302586,1.07092235863773,1.08747644518285,1.09778448107669,1.10103320308503,
1.10310676938518,1.10504784309833,1.10758977231665,1.11188662146474,1.14708338049787,
1.19623182845181,1.20575825710308,1.20791781881272,1.20914969868785,1.21022423315029,
1.21160751962747,1.21384248950938,1.22644680162857,1.23298162269474,1.2381153243991,
1.27817836248789,1.30768223981042,1.31209267260043,1.3144196120831,1.31614670947385,
1.31830315004177,1.32192599615574,1.33437679389053,1.38533776653531,1.40863964716442),
 .UNSPECIFIED.);
#1906=B_SPLINE_CURVE_WITH_KNOTS('',3,(#184645,#184646,#184647,#184648,#184649,
#184650,#184651,#184652),.UNSPECIFIED.,.F.,.F.,(4,2,2,4),(2.59337744564721,
2.59680650631764,2.61639715086674,2.66756143788907),.UNSPECIFIED.);
#1907=B_SPLINE_CURVE_WITH_KNOTS('',3,(#184653,#184654,#184655,#184656,#184657,
#184658,#184659,#184660,#184661,#184662,#184663,#184664,#184665,#184666,
#184667,#184668,#184669,#184670,#184671,#184672,#184673,#184674,#184675,
#184676,#184677,#184678,#184679,#184680,#184681,#184682,#184683,#184684,
#184685,#184686,#184687,#184688,#184689,#184690,#184691,#184692,#184693,
#184694,#184695,#184696,#184697,#184698,#184699,#184700,#184701,#184702,
#184703,#184704,#184705,#184706,#184707,#184708,#184709,#184710,#184711,
#184712,#184713,#184714,#184715,#184716,#184717,#184718,#184719,#184720,
#184721,#184722,#184723,#184724,#184725,#184726,#184727,#184728,#184729,
#184730,#184731,#184732,#184733,#184734,#184735,#184736,#184737,#184738,
#184739,#184740,#184741,#184742,#184743,#184744,#184745,#184746,#184747,
#184748,#184749,#184750,#184751,#184752,#184753,#184754,#184755,#184756,
#184757,#184758,#184759,#184760,#184761,#184762,#184763,#184764,#184765,
#184766,#184767,#184768,#184769,#184770,#184771,#184772,#184773,#184774,
#184775,#184776,#184777,#184778,#184779,#184780,#184781,#184782,#184783,
#184784,#184785,#184786,#184787,#184788,#184789,#184790,#184791,#184792,
#184793,#184794,#184795,#184796,#184797,#184798,#184799,#184800,#184801,
#184802,#184803,#184804,#184805,#184806,#184807,#184808,#184809,#184810,
#184811,#184812,#184813,#184814,#184815,#184816,#184817,#184818,#184819,
#184820,#184821,#184822,#184823,#184824,#184825,#184826,#184827,#184828,
#184829,#184830,#184831,#184832,#184833,#184834,#184835,#184836,#184837,
#184838,#184839,#184840,#184841,#184842,#184843,#184844,#184845,#184846,
#184847,#184848,#184849,#184850,#184851,#184852,#184853,#184854,#184855,
#184856,#184857,#184858,#184859,#184860,#184861,#184862,#184863,#184864,
#184865,#184866,#184867,#184868,#184869,#184870,#184871,#184872,#184873,
#184874,#184875,#184876),.UNSPECIFIED.,.F.,.F.,(4,2,2,2,2,2,2,2,2,2,2,2,
2,2,2,2,2,2,2,2,2,2,2,2,2,2,2,2,2,2,2,2,2,2,2,2,2,2,2,2,2,2,2,2,2,2,2,2,
2,2,2,2,2,2,2,2,2,2,2,2,2,2,2,2,2,2,2,2,2,2,2,2,2,2,2,2,2,2,2,2,2,2,2,2,
2,2,2,2,2,2,2,2,2,2,2,2,2,2,2,2,2,2,2,2,2,2,2,2,2,2,2,4),(0.000768636763620859,
0.0217315066625405,0.0248344419133145,0.026970678143598,0.0287699104987455,
0.030685112795253,0.0330691762509115,0.0367508368038254,0.0545959714040407,
0.0730111911955766,0.121979341411483,0.131697019623042,0.133869453884699,
0.135103947685483,0.13617772341325,0.137556055272068,0.140417804717059,
0.176399538266315,0.20912347261868,0.225523292957851,0.232324810710104,
0.23749883879562,0.239968098028527,0.241807521593055,0.243632198876294,
0.246166562549093,0.252759959465985,0.30904444772813,0.341534533561398,
0.345079265193333,0.346583133134812,0.347674383575492,0.348701702253464,
0.350452015143498,0.355232321612756,0.391152806185594,0.39739207199896,
0.442580350157967,0.44899616353931,0.451701928678007,0.453663173029819,
0.455456532518391,0.458325170388865,0.465231446369641,0.518057677823919,
0.5441731883724,0.555533049805055,0.557808688954534,0.559065841323031,0.560137198814906,
0.561484171278437,0.56410200378966,0.58007672594858,0.585034177782859,0.629903192358926,
0.64841696001026,0.659588891152749,0.662932982927637,0.665027435070619,
0.666960685637237,0.669453750491491,0.673583575738223,0.700904603771456,
0.743187692304861,0.759434473118696,0.767867973449621,0.769945078183847,
0.771158612823763,0.772236373949629,0.773625993740701,0.775932507385694,
0.789974982568318,0.791314807245637,0.798324935592705,0.812001368770075,
0.84486321961538,0.861425190092134,0.871736702264145,0.874985757285821,
0.877059352906881,0.87900032535612,0.881541936250879,0.885837831041215,
0.920971040899617,0.969918659955791,0.979677946062808,0.981853622208183,
0.983089023191742,0.984162989001907,0.98554078169571,0.988398713743108,
1.01125863261046,1.02402504859358,1.056881633485,1.07343480107024,1.08374263051261,
1.08699148230587,1.08906517828756,1.09100640630897,1.09354858510047,1.09784596261914,
1.13306155671959,1.1822681476552,1.19173242436896,1.19388770653724,1.19511870002955,
1.19619346812021,1.19757837922565,1.19981856865074,1.21252021657982,1.23489839246917,
1.26015660703498),.UNSPECIFIED.);
#1908=B_SPLINE_CURVE_WITH_KNOTS('',3,(#184878,#184879,#184880,#184881,#184882,
#184883,#184884,#184885,#184886,#184887,#184888,#184889,#184890,#184891,
#184892,#184893,#184894,#184895,#184896,#184897,#184898,#184899,#184900,
#184901,#184902,#184903,#184904,#184905,#184906,#184907,#184908,#184909,
#184910,#184911,#184912,#184913,#184914,#184915,#184916,#184917,#184918,
#184919,#184920,#184921,#184922,#184923,#184924,#184925,#184926,#184927,
#184928,#184929,#184930,#184931,#184932,#184933,#184934,#184935,#184936,
#184937,#184938,#184939,#184940,#184941,#184942,#184943,#184944,#184945,
#184946,#184947,#184948,#184949,#184950,#184951,#184952,#184953,#184954,
#184955,#184956,#184957,#184958,#184959,#184960,#184961,#184962,#184963,
#184964,#184965,#184966,#184967,#184968,#184969,#184970,#184971,#184972,
#184973,#184974,#184975,#184976,#184977,#184978,#184979,#184980,#184981,
#184982,#184983,#184984,#184985,#184986,#184987,#184988,#184989,#184990,
#184991,#184992,#184993,#184994,#184995,#184996,#184997,#184998,#184999,
#185000,#185001,#185002,#185003,#185004,#185005,#185006,#185007,#185008,
#185009,#185010,#185011,#185012,#185013,#185014,#185015,#185016,#185017,
#185018,#185019,#185020,#185021,#185022,#185023,#185024,#185025,#185026,
#185027,#185028,#185029,#185030,#185031,#185032,#185033,#185034,#185035,
#185036,#185037,#185038,#185039,#185040,#185041,#185042,#185043,#185044,
#185045,#185046,#185047,#185048,#185049,#185050,#185051,#185052,#185053,
#185054,#185055,#185056,#185057,#185058,#185059,#185060,#185061,#185062,
#185063,#185064,#185065,#185066,#185067,#185068,#185069,#185070,#185071,
#185072,#185073,#185074,#185075,#185076,#185077,#185078,#185079,#185080,
#185081,#185082,#185083,#185084,#185085,#185086,#185087,#185088,#185089,
#185090,#185091,#185092,#185093,#185094,#185095,#185096,#185097),
 .UNSPECIFIED.,.F.,.F.,(4,2,2,2,2,2,2,2,2,2,2,2,2,2,2,2,2,2,2,2,2,2,2,2,
2,2,2,2,2,2,2,2,2,2,2,2,2,2,2,2,2,2,2,2,2,2,2,2,2,2,2,2,2,2,2,2,2,2,2,2,
2,2,2,2,2,2,2,2,2,2,2,2,2,2,2,2,2,2,2,2,2,2,2,2,2,2,2,2,2,2,2,2,2,2,2,2,
2,2,2,2,2,2,2,2,2,2,2,2,2,4),(1.40863964716442,1.41654764256288,1.41946083579173,
1.42084949652186,1.42192463669879,1.4231532255005,1.42529763564206,1.43461047793079,
1.48376965084431,1.51916016469688,1.52345953256328,1.52600232681551,1.52794369037978,
1.53001720613691,1.53326509608718,1.54356406874418,1.56009980019928,1.59297023326031,
1.60449595099036,1.61425420981712,1.61606748499759,1.62921211557533,1.63147488928389,
1.63286652026671,1.63394190601275,1.63516848294114,1.63730403115457,1.6464965067669,
1.66501716992407,1.70914927550554,1.7317840423409,1.73573479484222,1.73820143199043,
1.74012569885294,1.7422544710342,1.74575265982184,1.75846526716016,1.780743468298,
1.82624897292974,1.82856531591742,1.84126738070175,1.8435075189208,1.84489236067264,
1.84596705461519,1.8471979493487,1.84935301183245,1.85881590293729,1.90799408650132,
1.94319456261665,1.94749136408763,1.95003334092667,1.95197448372881,1.95404815465521,
1.95729710371859,1.96760630754901,1.98416500105289,2.01705344523302,2.05268901962376,
2.05555268303099,2.05693160328613,2.05800567766868,2.05924034322329,2.06141265659592,
2.07112319591955,2.12008653296455,2.15522023941421,2.15951603917115,2.1620576796872,
2.16399871326019,2.16607241060743,2.16932169986364,2.17963450169365,2.19620137045321,
2.22909593278143,2.26470526831109,2.26757139958074,2.26895077443178,2.27002485924053,
2.27125914938986,2.27342987863855,2.28311821756389,2.33209838589604,2.36723676947822,
2.37153249383134,2.37407406628394,2.37601503437213,2.37808864866394,2.38133778043728,
2.39164985193077,2.40821532813543,2.47085486389423,2.47221620671777,2.47838974893803,
2.48032809473012,2.4815108796201,2.48254253023337,2.48395558070157,2.48697057165287,
2.49106866309595,2.50134681013531,2.52416875318152,2.57588013443217,2.58286385829124,
2.58574568151114,2.58754174992021,2.58950153779053,2.59219722308898,2.59855126109664,
2.62658804342393,2.66827829265055),.UNSPECIFIED.);
#1909=B_SPLINE_CURVE_WITH_KNOTS('',3,(#185098,#185099,#185100,#185101,#185102,
#185103,#185104,#185105,#185106,#185107,#185108,#185109,#185110),
 .UNSPECIFIED.,.F.,.F.,(4,3,3,3,4),(-48.1740290121606,-48.0708041571688,
-47.9674104081966,-47.94414959817,-47.8233361836797),.UNSPECIFIED.);
#1910=B_SPLINE_CURVE_WITH_KNOTS('',3,(#185115,#185116,#185117,#185118,#185119,
#185120,#185121,#185122,#185123,#185124,#185125,#185126,#185127,#185128,
#185129,#185130,#185131,#185132,#185133,#185134,#185135,#185136,#185137,
#185138,#185139,#185140,#185141,#185142,#185143,#185144,#185145,#185146,
#185147,#185148,#185149,#185150,#185151,#185152,#185153,#185154,#185155,
#185156,#185157,#185158,#185159,#185160,#185161,#185162,#185163,#185164,
#185165,#185166,#185167,#185168,#185169,#185170,#185171,#185172,#185173,
#185174,#185175,#185176,#185177,#185178,#185179,#185180,#185181,#185182,
#185183,#185184,#185185,#185186,#185187,#185188,#185189,#185190,#185191,
#185192,#185193,#185194,#185195,#185196,#185197,#185198,#185199,#185200,
#185201,#185202,#185203,#185204,#185205,#185206,#185207,#185208,#185209,
#185210,#185211,#185212,#185213,#185214,#185215,#185216,#185217,#185218,
#185219,#185220,#185221,#185222,#185223,#185224,#185225,#185226,#185227,
#185228,#185229,#185230,#185231,#185232,#185233,#185234,#185235,#185236,
#185237,#185238,#185239,#185240,#185241,#185242,#185243,#185244,#185245,
#185246,#185247,#185248,#185249,#185250,#185251,#185252,#185253,#185254,
#185255,#185256,#185257,#185258,#185259,#185260,#185261,#185262,#185263,
#185264,#185265,#185266,#185267,#185268,#185269,#185270,#185271,#185272,
#185273,#185274,#185275,#185276,#185277,#185278,#185279,#185280,#185281,
#185282,#185283,#185284,#185285,#185286,#185287,#185288,#185289,#185290,
#185291,#185292,#185293,#185294,#185295,#185296,#185297,#185298,#185299,
#185300,#185301,#185302,#185303,#185304,#185305,#185306,#185307,#185308,
#185309,#185310,#185311,#185312,#185313,#185314,#185315,#185316,#185317,
#185318,#185319,#185320,#185321,#185322,#185323,#185324,#185325,#185326,
#185327,#185328,#185329,#185330,#185331,#185332,#185333,#185334,#185335,
#185336,#185337,#185338,#185339,#185340,#185341,#185342,#185343,#185344,
#185345,#185346,#185347,#185348,#185349,#185350),.UNSPECIFIED.,.F.,.F.,
(4,2,2,2,2,2,2,2,2,2,2,2,2,2,2,2,2,2,2,2,2,2,2,2,2,2,2,2,2,2,2,2,2,2,2,
2,2,2,2,2,2,2,2,2,2,2,2,2,2,2,2,2,2,2,2,2,2,2,2,2,2,2,2,2,2,2,2,2,2,2,2,
2,2,2,2,2,2,2,2,2,2,2,2,2,2,2,2,2,2,2,2,2,2,2,2,2,2,2,2,2,2,2,2,2,2,2,2,
2,2,2,2,2,2,2,2,2,2,4),(1.25968336163638,1.28150381246531,1.30395448572161,
1.31433170933636,1.31654811413045,1.31779240001811,1.31886512414195,1.32022971845643,
1.32240312854682,1.33389982900217,1.38263541667828,1.4158386985878,1.42010255276132,
1.42263484404187,1.42457426449047,1.42665161975916,1.42991793052054,1.44038099252285,
1.45728194656261,1.49511048235499,1.52518582864636,1.52810042018771,1.52948919693211,
1.53056417361026,1.5317922923127,1.53393521864119,1.54323137459793,1.5620779165218,
1.60247839108949,1.61474048513036,1.62934631863552,1.63313459603982,1.63534958558466,
1.63726184492923,1.63959687495713,1.64404679877848,1.67495955683427,1.72180673060197,
1.73760386952349,1.74021635035163,1.74156223435342,1.74263360368595,1.74389179423334,
1.74617191280761,1.75760854005322,1.78402413656162,1.83638761534834,1.8433260673072,
1.84620014829443,1.84799460847972,1.84995521711348,1.85265673353905,1.85904657224156,
1.88738472843888,1.93728359451395,1.94991432471917,1.95215062266111,1.95353426062917,
1.95460877032405,1.95584029620597,1.95799845335825,1.96750651575542,2.01664165675908,
2.05182794795962,2.05612430967836,2.05866607222441,2.0606070777984,2.06268062773747,
2.06592944071323,2.07623866340765,2.09279781615963,2.12568535844249,2.13955046141776,
2.14611527770527,2.16166393842342,2.16426431072071,2.16560753805181,2.16667868913047,
2.16793882946592,2.17022813003496,2.18182972273794,2.20890969275392,2.26033572295614,
2.26733473695747,2.27021873446957,2.27201493643966,2.27397389543504,2.27666666692741,
2.28300556590808,2.31092215394589,2.35691488170998,2.35827699595489,2.36020818559394,
2.37383569611647,2.37612212493758,2.37750582803373,2.37858284733383,2.37979989146837,
2.38189279084592,2.39052515500643,2.40734999387028,2.46578858300041,2.47791139323761,
2.48149830216692,2.48364647036996,2.48552293806941,2.48788387304251,2.49249150159489,
2.49839596174534,2.51181620654956,2.53423713378931,2.58327534874353,2.58750372343543,
2.58916795054713,2.5901785912019,2.59128218578855,2.59285357572233,2.59337744564721),
 .UNSPECIFIED.);
#1911=B_SPLINE_CURVE_WITH_KNOTS('',3,(#185352,#185353,#185354,#185355,#185356,
#185357,#185358,#185359,#185360,#185361,#185362,#185363,#185364,#185365,
#185366,#185367,#185368,#185369,#185370,#185371,#185372,#185373,#185374,
#185375,#185376,#185377,#185378,#185379,#185380,#185381,#185382,#185383,
#185384,#185385,#185386,#185387,#185388,#185389,#185390,#185391,#185392,
#185393,#185394,#185395,#185396,#185397,#185398,#185399,#185400,#185401,
#185402,#185403,#185404,#185405,#185406,#185407,#185408,#185409,#185410,
#185411,#185412,#185413,#185414,#185415,#185416,#185417,#185418,#185419,
#185420,#185421,#185422,#185423,#185424,#185425,#185426,#185427,#185428,
#185429,#185430,#185431,#185432,#185433,#185434,#185435,#185436,#185437,
#185438,#185439,#185440,#185441,#185442,#185443,#185444,#185445,#185446,
#185447,#185448,#185449,#185450,#185451,#185452,#185453,#185454,#185455,
#185456,#185457,#185458,#185459,#185460,#185461,#185462,#185463,#185464,
#185465,#185466,#185467,#185468,#185469,#185470,#185471,#185472,#185473,
#185474,#185475,#185476,#185477,#185478,#185479,#185480,#185481,#185482,
#185483,#185484,#185485,#185486,#185487,#185488,#185489,#185490,#185491,
#185492,#185493,#185494,#185495,#185496,#185497,#185498,#185499,#185500,
#185501,#185502,#185503,#185504,#185505,#185506,#185507,#185508,#185509,
#185510,#185511,#185512,#185513,#185514,#185515,#185516,#185517,#185518,
#185519,#185520,#185521,#185522,#185523,#185524,#185525,#185526,#185527,
#185528,#185529),.UNSPECIFIED.,.F.,.F.,(4,3,3,3,3,3,3,3,3,3,3,3,3,3,3,3,
3,3,3,3,3,3,3,3,3,3,3,3,3,3,3,3,3,3,3,3,3,3,3,3,3,3,3,3,3,3,3,3,3,3,3,3,
3,3,3,3,3,3,3,4),(-54.1065214908593,-53.9371682979412,-53.8337735608932,
-53.7305322787781,-53.6274123133857,-53.5243577451767,-53.4213345368189,
-53.3183086941465,-53.2151759273683,-53.1119868359584,-53.0086148425767,
-52.9383318479793,-52.8349371109314,-52.7316958288165,-52.6285758634243,
-52.5255212952155,-52.4224980868578,-52.3194722441853,-52.2163394774073,
-52.1131503859976,-52.009778392616,-51.9394953980175,-51.8361006609696,
-51.7328593788546,-51.6297394134623,-51.5266848452534,-51.4236616368957,
-51.3206357942232,-51.2175030274452,-51.1143139360354,-51.0109419426538,
-50.9406589480556,-50.8372642110076,-50.7340229288926,-50.6309029635003,
-50.5278483952913,-50.4248251869335,-50.321799344261,-50.2186665774828,
-50.115477486073,-50.0121054926913,-49.9418224980937,-49.8384277610458,
-49.7351864789307,-49.6320665135384,-49.5290119453295,-49.4259887369717,
-49.3229628942992,-49.2198301275211,-49.1166410361113,-49.0132690427297,
-48.9429860481318,-48.8396205066968,-48.7363953136982,-48.6332762150935,
-48.5302290794639,-48.4271932051552,-48.3241646395655,-48.2210652727443,
-48.1740290121606),.UNSPECIFIED.);
#1912=B_SPLINE_CURVE_WITH_KNOTS('',3,(#185530,#185531,#185532,#185533),
 .UNSPECIFIED.,.F.,.F.,(4,4),(-54.4565130283295,-54.1065275196936),
 .UNSPECIFIED.);
#1913=B_SPLINE_CURVE_WITH_KNOTS('',3,(#185539,#185540,#185541,#185542,#185543,
#185544,#185545,#185546,#185547,#185548,#185549,#185550,#185551,#185552,
#185553,#185554,#185555,#185556,#185557,#185558),.UNSPECIFIED.,.F.,.F.,
(4,2,2,2,2,2,2,2,2,4),(2.59313914980931,2.59886472833631,2.60312141898723,
2.60565120851499,2.60758972885503,2.60966711125076,2.61293555061346,2.61673849141341,
2.62400252838434,2.66762635786377),.UNSPECIFIED.);
#1914=B_SPLINE_CURVE_WITH_KNOTS('',3,(#185559,#185560,#185561,#185562,#185563,
#185564,#185565,#185566,#185567,#185568,#185569,#185570,#185571,#185572,
#185573,#185574,#185575,#185576,#185577,#185578,#185579,#185580,#185581,
#185582,#185583,#185584,#185585,#185586,#185587,#185588,#185589,#185590,
#185591,#185592,#185593,#185594,#185595,#185596,#185597,#185598,#185599,
#185600,#185601,#185602,#185603,#185604,#185605,#185606,#185607,#185608,
#185609,#185610,#185611,#185612,#185613,#185614,#185615,#185616,#185617,
#185618,#185619,#185620,#185621,#185622,#185623,#185624,#185625,#185626,
#185627,#185628,#185629,#185630,#185631,#185632,#185633,#185634,#185635,
#185636,#185637,#185638,#185639,#185640,#185641,#185642,#185643,#185644,
#185645,#185646,#185647,#185648,#185649,#185650,#185651,#185652,#185653,
#185654,#185655,#185656,#185657,#185658,#185659,#185660,#185661,#185662,
#185663,#185664,#185665,#185666,#185667,#185668,#185669,#185670,#185671,
#185672,#185673,#185674,#185675,#185676,#185677,#185678,#185679,#185680,
#185681,#185682,#185683,#185684,#185685,#185686,#185687,#185688,#185689,
#185690,#185691,#185692,#185693,#185694,#185695,#185696,#185697,#185698,
#185699,#185700,#185701,#185702,#185703,#185704,#185705,#185706,#185707,
#185708,#185709,#185710,#185711,#185712,#185713,#185714,#185715,#185716,
#185717,#185718,#185719,#185720,#185721,#185722,#185723,#185724,#185725,
#185726,#185727,#185728,#185729,#185730,#185731,#185732,#185733,#185734,
#185735,#185736,#185737,#185738,#185739,#185740,#185741,#185742,#185743,
#185744,#185745,#185746,#185747,#185748,#185749,#185750,#185751,#185752,
#185753,#185754,#185755,#185756,#185757,#185758,#185759,#185760,#185761,
#185762,#185763,#185764,#185765,#185766,#185767,#185768,#185769,#185770,
#185771,#185772),.UNSPECIFIED.,.F.,.F.,(4,2,2,2,2,2,2,2,2,2,2,2,2,2,2,2,
2,2,2,2,2,2,2,2,2,2,2,2,2,2,2,2,2,2,2,2,2,2,2,2,2,2,2,2,2,2,2,2,2,2,2,2,
2,2,2,2,2,2,2,2,2,2,2,2,2,2,2,2,2,2,2,2,2,2,2,2,2,2,2,2,2,2,2,2,2,2,2,2,
2,2,2,2,2,2,2,2,2,2,2,2,2,2,2,2,2,2,4),(0.00064999401870814,0.0375152740774843,
0.0412926072787783,0.0433020348222845,0.0446072165208979,0.0458444201689322,
0.0469177328032517,0.0482917920573788,0.0511320607526068,0.0879797143108778,
0.109399231159625,0.136182509301837,0.146436109229218,0.149706965971948,
0.151785053864551,0.153723653894635,0.156252719855537,0.160506384817164,
0.193189314060769,0.222561939900857,0.244175730037096,0.254295425612179,
0.256485313796723,0.257733442726415,0.258805446753902,0.260163935545637,
0.262836118809076,0.280220611714519,0.329264880991464,0.347306199028025,
0.354573879979304,0.360002618875832,0.36256780699064,0.364505140438897,
0.366333350100077,0.368881496653483,0.375563659495922,0.430964785842751,
0.455317985223457,0.466218325466524,0.46846680960563,0.469717953032539,
0.470789700695349,0.472144217413519,0.474885907083682,0.493327487968013,
0.537460170432788,0.565331791001386,0.571665310121053,0.574356949408836,
0.576315511294048,0.578111648649546,0.580996188318186,0.58799980762993,
0.639384966729156,0.666515578373941,0.678128416282107,0.680418165073668,
0.681678304585031,0.682749309311691,0.684092162770366,0.686691258230314,
0.702217026171755,0.708760852023979,0.7226338679729,0.75549393192625,0.772056435613488,
0.782367860376191,0.785616664699219,0.787690046705758,0.789630781543226,
0.792172026961885,0.796467182234275,0.831578294062515,0.880465431901704,
0.890288604243727,0.892468461492535,0.89370469305999,0.894778394330742,
0.896154559272692,0.899004689366724,0.935374535901499,0.989163003036879,
0.995619057843842,0.998331625955218,1.00029412019574,1.00208609363388,1.00494701982904,
1.01180629779494,1.06524490606319,1.09093514883092,1.1021865449968,1.10445596255679,
1.10571177114402,1.106783255761,1.10813200888855,1.11075807436306,1.12692226978114,
1.17758026273599,1.20199422941898,1.20789424776203,1.21051031179204,1.21245601008353,
1.21427040670099,1.21676501607254,1.22311486349749,1.25968336163638),
 .UNSPECIFIED.);
#1915=B_SPLINE_CURVE_WITH_KNOTS('',3,(#185774,#185775,#185776,#185777,#185778,
#185779,#185780,#185781,#185782,#185783),.UNSPECIFIED.,.F.,.F.,(4,1,1,1,
1,1,1,4),(-60.3897037700523,-59.9301869977125,-58.9313505477506,-57.9325140977887,
-56.9336776478268,-55.934841197865,-54.9360047479031,-54.4565130283295),
 .UNSPECIFIED.);
#1916=B_SPLINE_CURVE_WITH_KNOTS('',3,(#185784,#185785,#185786,#185787,#185788,
#185789,#185790,#185791,#185792,#185793,#185794,#185795,#185796,#185797,
#185798,#185799,#185800,#185801),.UNSPECIFIED.,.F.,.F.,(4,2,2,2,2,2,2,2,
4),(0.000658789691829873,0.0033297019412485,0.00592165923435953,0.00778879714723288,
0.00964368964025443,0.0114909186427276,0.0146445374997109,0.023361496180258,
0.0750717851778821),.UNSPECIFIED.);
#1917=B_SPLINE_CURVE_WITH_KNOTS('',3,(#185806,#185807,#185808,#185809,#185810,
#185811,#185812,#185813,#185814,#185815,#185816,#185817,#185818,#185819,
#185820,#185821,#185822,#185823,#185824,#185825,#185826,#185827,#185828,
#185829,#185830,#185831,#185832,#185833,#185834,#185835,#185836,#185837,
#185838,#185839,#185840,#185841,#185842,#185843,#185844,#185845,#185846,
#185847,#185848,#185849,#185850,#185851,#185852,#185853,#185854,#185855,
#185856,#185857,#185858,#185859,#185860,#185861,#185862,#185863,#185864,
#185865,#185866,#185867,#185868,#185869,#185870,#185871,#185872,#185873,
#185874,#185875,#185876,#185877,#185878,#185879,#185880,#185881,#185882,
#185883,#185884,#185885,#185886,#185887,#185888,#185889,#185890,#185891,
#185892,#185893,#185894,#185895,#185896,#185897,#185898,#185899,#185900,
#185901,#185902,#185903,#185904,#185905,#185906,#185907,#185908,#185909,
#185910,#185911,#185912,#185913,#185914,#185915,#185916,#185917,#185918,
#185919,#185920,#185921,#185922,#185923,#185924,#185925,#185926,#185927,
#185928,#185929,#185930,#185931,#185932,#185933,#185934,#185935,#185936,
#185937,#185938,#185939,#185940,#185941,#185942,#185943,#185944,#185945,
#185946,#185947,#185948,#185949,#185950,#185951,#185952,#185953,#185954,
#185955,#185956,#185957,#185958,#185959,#185960,#185961,#185962,#185963,
#185964,#185965,#185966,#185967,#185968,#185969,#185970,#185971,#185972,
#185973,#185974,#185975,#185976,#185977,#185978,#185979,#185980,#185981,
#185982,#185983,#185984,#185985,#185986,#185987,#185988,#185989,#185990,
#185991,#185992,#185993,#185994,#185995,#185996,#185997,#185998,#185999,
#186000,#186001,#186002,#186003,#186004,#186005,#186006,#186007,#186008,
#186009,#186010,#186011,#186012,#186013,#186014,#186015,#186016,#186017,
#186018,#186019,#186020,#186021,#186022,#186023),.UNSPECIFIED.,.F.,.F.,
(4,2,2,2,2,2,2,2,2,2,2,2,2,2,2,2,2,2,2,2,2,2,2,2,2,2,2,2,2,2,2,2,2,2,2,
2,2,2,2,2,2,2,2,2,2,2,2,2,2,2,2,2,2,2,2,2,2,2,2,2,2,2,2,2,2,2,2,2,2,2,2,
2,2,2,2,2,2,2,2,2,2,2,2,2,2,2,2,2,2,2,2,2,2,2,2,2,2,2,2,2,2,2,2,2,2,2,2,
2,4),(1.25981860719964,1.28582891022361,1.32659467423898,1.33166059105053,
1.33412005612525,1.33604290774328,1.33817439093442,1.34168688904338,1.35456200426643,
1.37726280817133,1.41585026003799,1.42084444542092,1.43685056924709,1.43946977576748,
1.4408168819241,1.44188804366973,1.44314462188987,1.44541833526764,1.45675091337238,
1.48276027920743,1.53567696855932,1.54257189208843,1.54543830569257,1.54723100163399,
1.54919211027279,1.55189876163002,1.55832173773744,1.58694424906269,1.63822351505355,
1.64928412896355,1.65143095725007,1.65278728562107,1.65385911841402,1.65510881737313,
1.65735083935026,1.66814601013867,1.69210638951572,1.74805404629795,1.75467929342998,
1.75721847962063,1.75904426635465,1.7609827183722,1.76355564981005,1.76921965307229,
1.79185993256202,1.82467490385176,1.82889898837517,1.86039111270683,1.8633024911439,
1.86469040503985,1.86576502144183,1.8669930726272,1.86913668712782,1.87844828159124,
1.92759392663568,1.96295408368725,1.96725123097806,1.96979276014188,1.97173318561002,
1.97380572632607,1.97705214516539,1.98734692570109,2.00387637583337,2.03673241895726,
2.04842499823039,2.05688773826077,2.0727339348878,2.07534613190607,2.07669163343502,
2.07776257369036,2.07902011570333,2.08129869010328,2.09271990509077,2.11908202301188,
2.17148524379948,2.17841603878784,2.1812881475847,2.1830817267577,2.18504165356763,
2.18774274371944,2.19413398865415,2.24049020802426,2.28167191070143,2.28635355340294,
2.28808858751266,2.28911271836411,2.29020548502977,2.29171944475299,2.2953247129901,
2.33382364959093,2.38313324211796,2.39030045978694,2.39321196698077,2.39501279634959,
2.39696692214965,2.39963523349187,2.40564810022727,2.41389768596798,2.46455540520303,
2.49625376527554,2.49916486350826,2.50055269798735,2.50162727784137,2.50285531516211,
2.50414746183214,2.50879710771578,2.53292412726831,2.55382470693563,2.59313914980931),
 .UNSPECIFIED.);
#1918=B_SPLINE_CURVE_WITH_KNOTS('',3,(#186024,#186025,#186026,#186027,#186028,
#186029,#186030,#186031,#186032,#186033,#186034,#186035,#186036,#186037,
#186038,#186039,#186040,#186041,#186042,#186043,#186044,#186045,#186046,
#186047,#186048,#186049,#186050,#186051,#186052,#186053,#186054,#186055,
#186056,#186057,#186058,#186059,#186060,#186061,#186062,#186063,#186064,
#186065,#186066,#186067,#186068,#186069,#186070,#186071,#186072,#186073,
#186074,#186075,#186076,#186077,#186078,#186079,#186080,#186081,#186082,
#186083,#186084,#186085,#186086,#186087,#186088,#186089,#186090,#186091,
#186092,#186093,#186094,#186095,#186096,#186097,#186098,#186099,#186100,
#186101,#186102,#186103,#186104,#186105,#186106,#186107,#186108,#186109,
#186110,#186111,#186112,#186113,#186114,#186115,#186116,#186117,#186118,
#186119,#186120,#186121,#186122,#186123,#186124,#186125,#186126,#186127,
#186128,#186129,#186130,#186131,#186132,#186133,#186134,#186135,#186136,
#186137,#186138,#186139,#186140,#186141,#186142,#186143,#186144,#186145,
#186146,#186147,#186148,#186149,#186150,#186151,#186152,#186153,#186154,
#186155,#186156,#186157,#186158,#186159,#186160,#186161,#186162,#186163,
#186164,#186165,#186166,#186167,#186168,#186169,#186170,#186171,#186172,
#186173,#186174,#186175,#186176,#186177,#186178,#186179,#186180,#186181,
#186182,#186183,#186184,#186185,#186186,#186187,#186188,#186189,#186190,
#186191,#186192,#186193,#186194,#186195,#186196,#186197,#186198,#186199,
#186200,#186201,#186202,#186203,#186204,#186205,#186206,#186207,#186208,
#186209,#186210,#186211,#186212,#186213,#186214,#186215,#186216,#186217,
#186218,#186219,#186220,#186221,#186222,#186223,#186224,#186225,#186226,
#186227,#186228,#186229,#186230,#186231,#186232,#186233,#186234,#186235,
#186236,#186237,#186238,#186239,#186240,#186241,#186242,#186243,#186244,
#186245,#186246,#186247,#186248,#186249,#186250,#186251,#186252,#186253,
#186254,#186255,#186256,#186257,#186258,#186259,#186260,#186261),
 .UNSPECIFIED.,.F.,.F.,(4,2,2,2,2,2,2,2,2,2,2,2,2,2,2,2,2,2,2,2,2,2,2,2,
2,2,2,2,2,2,2,2,2,2,2,2,2,2,2,2,2,2,2,2,2,2,2,2,2,2,2,2,2,2,2,2,2,2,2,2,
2,2,2,2,2,2,2,2,2,2,2,2,2,2,2,2,2,2,2,2,2,2,2,2,2,2,2,2,2,2,2,2,2,2,2,2,
2,2,2,2,2,2,2,2,2,2,2,2,2,2,2,2,2,2,2,2,2,2,4),(0.0750717851778821,0.0891453783474772,
0.1087192970361,0.112670157112163,0.114241193640968,0.115344696903057,0.116355376301621,
0.118019908363095,0.122250352987691,0.171173402583166,0.20895082471958,
0.213968579861932,0.216896951969535,0.219516741369516,0.221437752967846,
0.223232180483361,0.226106804357264,0.233033251402772,0.285519572440992,
0.311872492728247,0.323292252604327,0.325571279362092,0.326829154986186,
0.327900433628379,0.329246423208051,0.331859753701603,0.347731566056851,
0.352570265379959,0.367740061051498,0.400617568765758,0.417199257124334,
0.427519584284733,0.430769576126748,0.432843327658458,0.434784135670115,
0.437325083531694,0.441618854436347,0.476149367615986,0.496363447435444,
0.52357755700517,0.535211386266633,0.537502463284449,0.538762965732314,
0.539834057535949,0.541176739628813,0.54377468713262,0.559269099536909,
0.563494995426891,0.611468218857118,0.635181638865882,0.640989895303778,
0.643589461135923,0.645532474861167,0.647351300977577,0.649862938640005,
0.656315216532433,0.713883148579057,0.736844180074091,0.747364976192785,
0.749590459351435,0.750836730097221,0.751909224889602,0.753271024874312,
0.755957860227891,0.773745509226652,0.821985607898747,0.840287695048908,
0.851368557299992,0.854703013833243,0.856795400351583,0.858729449641452,
0.861227337197682,0.86537338167352,0.893311548684437,0.947028169980716,
0.959232734448808,0.961554775631366,0.962822073493619,0.963892853517728,
0.965227484351787,0.967302745495934,0.97725674140125,0.982892865066459,
0.992293088897469,1.00386246051483,1.0367091579207,1.05325022119457,1.06355259515346,
1.0668008364901,1.06887440950704,1.07081570981274,1.07335825373397,1.07765685492899,
1.11296692312606,1.16222109021709,1.17155869396154,1.17370493824424,1.17493394549453,
1.17600904522414,1.17739710677164,1.18030713251461,1.20843832112002,1.24812717812997,
1.26507257095043,1.27555724716827,1.27882646295807,1.2809047622708,1.28284443417117,
1.28537615186896,1.28963706461134,1.33463676212147,1.3796876555644,1.38441284821034,
1.38615514539917,1.38718113692288,1.38827383174263,1.38978433755491,1.39336594278135,
1.40879227668569),.UNSPECIFIED.);
#1919=B_SPLINE_CURVE_WITH_KNOTS('',3,(#186267,#186268,#186269,#186270,#186271),
 .UNSPECIFIED.,.F.,.F.,(4,1,4),(76.7075601022117,76.9104066470643,77.0584303621713),
 .UNSPECIFIED.);
#1920=B_SPLINE_CURVE_WITH_KNOTS('',3,(#186272,#186273,#186274,#186275,#186276,
#186277,#186278,#186279,#186280,#186281,#186282,#186283,#186284,#186285,
#186286,#186287,#186288,#186289,#186290,#186291,#186292,#186293,#186294,
#186295,#186296,#186297,#186298,#186299,#186300,#186301,#186302,#186303,
#186304,#186305,#186306,#186307,#186308,#186309,#186310,#186311,#186312,
#186313,#186314,#186315,#186316,#186317,#186318,#186319,#186320,#186321,
#186322,#186323,#186324,#186325,#186326,#186327,#186328,#186329,#186330,
#186331,#186332,#186333,#186334,#186335,#186336,#186337,#186338,#186339,
#186340,#186341,#186342,#186343,#186344,#186345,#186346,#186347,#186348,
#186349,#186350,#186351,#186352,#186353,#186354,#186355,#186356,#186357,
#186358,#186359,#186360,#186361,#186362,#186363,#186364,#186365,#186366,
#186367,#186368,#186369,#186370,#186371,#186372,#186373,#186374,#186375,
#186376,#186377,#186378,#186379,#186380,#186381,#186382,#186383,#186384,
#186385,#186386,#186387,#186388,#186389,#186390,#186391,#186392,#186393,
#186394,#186395,#186396,#186397,#186398,#186399,#186400,#186401,#186402,
#186403,#186404,#186405,#186406,#186407,#186408,#186409,#186410,#186411,
#186412,#186413,#186414,#186415,#186416,#186417,#186418,#186419,#186420,
#186421,#186422,#186423,#186424,#186425,#186426,#186427,#186428,#186429,
#186430,#186431,#186432,#186433,#186434,#186435,#186436,#186437,#186438,
#186439,#186440,#186441,#186442,#186443,#186444,#186445,#186446,#186447,
#186448,#186449,#186450,#186451,#186452,#186453,#186454,#186455,#186456,
#186457,#186458,#186459,#186460,#186461,#186462,#186463,#186464,#186465,
#186466,#186467,#186468,#186469,#186470,#186471,#186472,#186473,#186474,
#186475,#186476,#186477,#186478,#186479,#186480,#186481,#186482,#186483,
#186484,#186485,#186486,#186487,#186488,#186489,#186490,#186491,#186492,
#186493),.UNSPECIFIED.,.F.,.F.,(4,2,2,2,2,2,2,2,2,2,2,2,2,2,2,2,2,2,2,2,
2,2,2,2,2,2,2,2,2,2,2,2,2,2,2,2,2,2,2,2,2,2,2,2,2,2,2,2,2,2,2,2,2,2,2,2,
2,2,2,2,2,2,2,2,2,2,2,2,2,2,2,2,2,2,2,2,2,2,2,2,2,2,2,2,2,2,2,2,2,2,2,2,
2,2,2,2,2,2,2,2,2,2,2,2,2,2,2,2,2,2,4),(0.000629224533727324,0.0464126621687836,
0.0539626763531269,0.0578723762427416,0.0612145520135249,0.0633082415157978,
0.0652410855766748,0.0677340423634502,0.0718645896666564,0.0992472355725051,
0.113709321813746,0.129240598463086,0.154594556929824,0.16574178214956,
0.168010450595375,0.169268035226069,0.170339020864305,0.171684584897561,
0.174296920953314,0.190152334184,0.195974171156568,0.252803526465609,0.268941988849295,
0.272736140704197,0.27492968962085,0.276842832163743,0.279203717020773,
0.282811030182719,0.299535151121957,0.307018560652277,0.355524549263055,
0.370248675243035,0.378140658615438,0.380172201927849,0.381375365209586,
0.382455172270495,0.383862177879522,0.386228863793868,0.401659062722206,
0.405923222942093,0.448896318633739,0.476827918475772,0.483168208250224,
0.485860736611321,0.487819214716071,0.489614769057079,0.492497261265996,
0.499490239454971,0.551009931245716,0.578034136333571,0.589619962056034,
0.591907936138278,0.593167565483171,0.594238417515275,0.595581435666222,
0.598181887162465,0.61374689460685,0.620206441122678,0.661616806330857,
0.688886522740687,0.695146366432909,0.697825195494852,0.699781299801176,
0.701579962533769,0.704479107892417,0.711571657377543,0.76122499734123,
0.799535458073044,0.803139547680463,0.804653404254384,0.805746239795849,
0.806770550084666,0.808506131278771,0.813190663793015,0.854270227369256,
0.90069632129006,0.907087781284192,0.909789116784305,0.91174928044377,0.913543120827663,
0.916415733282814,0.923348165275279,0.975791238592437,1.00216327878638,
1.01358701357392,1.01586598151391,1.01712371118841,1.0181947968606,1.01954045672254,
1.02215289135757,1.03800315140485,1.04274645700524,1.05802368065071,1.09089683261881,
1.10747729817755,1.11779657959663,1.12104609091117,1.12311949953335,1.12505996113583,
1.12760041872033,1.13189327881161,1.17429056279923,1.20334593464797,1.22296047210307,
1.22691537197947,1.22848693012366,1.22959043091726,1.23060082410116,1.23226432129821,
1.23648912489059,1.25981860719964),.UNSPECIFIED.);
#1921=B_SPLINE_CURVE_WITH_KNOTS('',3,(#186495,#186496,#186497,#186498,#186499,
#186500,#186501,#186502,#186503,#186504,#186505,#186506,#186507,#186508,
#186509,#186510,#186511,#186512,#186513,#186514,#186515,#186516,#186517,
#186518,#186519,#186520,#186521,#186522,#186523,#186524,#186525,#186526,
#186527,#186528,#186529,#186530,#186531,#186532,#186533,#186534,#186535,
#186536,#186537,#186538,#186539,#186540,#186541,#186542,#186543,#186544,
#186545,#186546,#186547,#186548,#186549,#186550,#186551,#186552,#186553,
#186554,#186555,#186556,#186557,#186558,#186559,#186560,#186561,#186562,
#186563,#186564,#186565,#186566,#186567,#186568,#186569,#186570,#186571,
#186572,#186573,#186574,#186575,#186576,#186577,#186578,#186579,#186580,
#186581,#186582,#186583,#186584,#186585,#186586,#186587,#186588,#186589,
#186590,#186591,#186592,#186593,#186594,#186595,#186596,#186597,#186598,
#186599,#186600,#186601,#186602,#186603,#186604,#186605,#186606,#186607,
#186608,#186609,#186610,#186611,#186612,#186613,#186614,#186615,#186616,
#186617,#186618,#186619,#186620,#186621,#186622,#186623,#186624,#186625,
#186626,#186627,#186628,#186629,#186630,#186631,#186632,#186633,#186634,
#186635,#186636,#186637,#186638,#186639,#186640,#186641,#186642,#186643,
#186644,#186645,#186646,#186647,#186648,#186649,#186650,#186651,#186652,
#186653,#186654,#186655,#186656,#186657,#186658,#186659,#186660,#186661,
#186662,#186663,#186664,#186665,#186666,#186667,#186668,#186669,#186670,
#186671,#186672,#186673,#186674,#186675,#186676,#186677,#186678,#186679,
#186680,#186681,#186682,#186683,#186684,#186685,#186686,#186687,#186688,
#186689,#186690,#186691,#186692,#186693,#186694,#186695,#186696,#186697,
#186698,#186699,#186700,#186701,#186702,#186703,#186704,#186705,#186706,
#186707,#186708,#186709,#186710,#186711,#186712,#186713,#186714,#186715,
#186716,#186717,#186718),.UNSPECIFIED.,.F.,.F.,(4,2,2,2,2,2,2,2,2,2,2,2,
2,2,2,2,2,2,2,2,2,2,2,2,2,2,2,2,2,2,2,2,2,2,2,2,2,2,2,2,2,2,2,2,2,2,2,2,
2,2,2,2,2,2,2,2,2,2,2,2,2,2,2,2,2,2,2,2,2,2,2,2,2,2,2,2,2,2,2,2,2,2,2,2,
2,2,2,2,2,2,2,2,2,2,2,2,2,2,2,2,2,2,2,2,2,2,2,2,2,2,2,4),(1.40879227668569,
1.43100334476945,1.48142611167368,1.48848461841809,1.49137902606764,1.49317751608561,
1.49513563473351,1.4978212006631,1.50411510510166,1.53165386473917,1.56005743142361,
1.58238723262586,1.59509407049765,1.59733461345269,1.59871964715131,1.59979445276563,
1.60102543356578,1.603180548043,1.61264210716678,1.66182711478029,1.69703164539968,
1.70132887834435,1.70387110819822,1.70581244291945,1.7078863176153,1.71113558332165,
1.72144576985247,1.73800602081766,1.77089764691296,1.78463226584746,1.79150542719729,
1.79172194163246,1.79524178403218,1.80720044609824,1.80940049805829,1.81077325936907,
1.8118468169668,1.81308573798261,1.8152772015073,1.82526903226868,1.87400032445147,
1.90905752288329,1.91335254868163,1.91589404744955,1.91783515488805,1.9199091077548,
1.92315916620381,1.93347751982231,1.9500562679024,1.98296192190686,1.99814136604356,
2.00298749678178,2.01887889737035,2.02149317854504,2.02283948348095,2.02391092077113,
2.02516888112824,2.02744779212173,2.03886194855498,2.06518741968749,2.11768264226043,
2.12461220076899,2.12748488900246,2.12927914863838,2.1312400744361,2.13394300838327,
2.140340814811,2.18822154798705,2.2278321977224,2.23257803305534,2.23432327224965,
2.23534971398744,2.23644180490625,2.23794971234211,2.24151709177331,2.27899770614475,
2.32959370074135,2.33664136625753,2.33953364673658,2.34133151027224,2.34328949940916,
2.34597588921557,2.35227635373791,2.37987345685712,2.42202986271522,2.44273030124236,
2.44553853536011,2.44690652672951,2.44794318828084,2.44914403808312,2.45042586068833,
2.45237854022586,2.45600562423696,2.46464620226109,2.49771078806596,2.54136333775339,
2.54858725821568,2.55150906913563,2.55331236936547,2.55526611108923,2.55792840599244,
2.56408926771024,2.59055298369589,2.6480782413717,2.655950306731,2.65804641507783,
2.65927645566117,2.66033332044916,2.66137927037716,2.66272977103268,2.66518795266621,
2.66828177691447),.UNSPECIFIED.);
#1922=B_SPLINE_CURVE_WITH_KNOTS('',3,(#186719,#186720,#186721,#186722,#186723,
#186724),.UNSPECIFIED.,.F.,.F.,(4,2,4),(0.000817337931816071,0.0612279287495663,
0.0752219443712125),.UNSPECIFIED.);
#1923=B_SPLINE_CURVE_WITH_KNOTS('',3,(#186730,#186731,#186732,#186733,#186734,
#186735,#186736,#186737,#186738,#186739,#186740,#186741,#186742),
 .UNSPECIFIED.,.F.,.F.,(4,3,3,3,4),(82.9907456874214,83.0928761472026,83.194883423972,
83.2967928188117,83.3413404136697),.UNSPECIFIED.);
#1924=B_SPLINE_CURVE_WITH_KNOTS('',3,(#186743,#186744,#186745,#186746,#186747,
#186748,#186749,#186750,#186751,#186752),.UNSPECIFIED.,.F.,.F.,(4,1,1,1,
1,1,1,4),(77.0584303621713,77.9092430970262,78.9080795469881,79.9069159969499,
80.9057524469118,81.9045888968737,82.9034253468355,82.9907454093913),
 .UNSPECIFIED.);
#1925=B_SPLINE_CURVE_WITH_KNOTS('',3,(#186753,#186754,#186755,#186756,#186757,
#186758,#186759,#186760,#186761,#186762,#186763,#186764,#186765,#186766,
#186767,#186768,#186769,#186770,#186771,#186772,#186773,#186774,#186775,
#186776,#186777,#186778,#186779,#186780,#186781,#186782,#186783,#186784,
#186785,#186786,#186787,#186788,#186789,#186790,#186791,#186792,#186793,
#186794,#186795,#186796,#186797,#186798,#186799,#186800,#186801,#186802,
#186803,#186804,#186805,#186806,#186807,#186808,#186809,#186810,#186811,
#186812,#186813,#186814,#186815,#186816,#186817,#186818,#186819,#186820,
#186821,#186822,#186823,#186824,#186825,#186826,#186827,#186828,#186829,
#186830,#186831,#186832,#186833,#186834,#186835,#186836,#186837,#186838,
#186839,#186840,#186841,#186842,#186843,#186844,#186845,#186846,#186847,
#186848,#186849,#186850,#186851,#186852,#186853,#186854,#186855,#186856,
#186857,#186858,#186859,#186860,#186861,#186862,#186863,#186864,#186865,
#186866,#186867,#186868,#186869,#186870,#186871,#186872,#186873,#186874,
#186875,#186876,#186877,#186878,#186879,#186880,#186881,#186882,#186883,
#186884,#186885,#186886,#186887,#186888,#186889,#186890,#186891,#186892,
#186893,#186894,#186895,#186896,#186897,#186898,#186899,#186900,#186901,
#186902,#186903,#186904,#186905,#186906,#186907,#186908,#186909,#186910,
#186911,#186912,#186913,#186914,#186915,#186916,#186917,#186918,#186919,
#186920,#186921,#186922,#186923,#186924,#186925,#186926,#186927,#186928,
#186929,#186930,#186931,#186932,#186933,#186934,#186935,#186936,#186937,
#186938,#186939,#186940,#186941,#186942,#186943,#186944,#186945,#186946,
#186947,#186948,#186949,#186950,#186951,#186952,#186953,#186954,#186955,
#186956,#186957,#186958,#186959,#186960,#186961,#186962,#186963,#186964,
#186965,#186966,#186967,#186968,#186969,#186970,#186971,#186972,#186973,
#186974,#186975,#186976,#186977,#186978,#186979,#186980,#186981,#186982,
#186983,#186984,#186985,#186986,#186987,#186988,#186989,#186990,#186991,
#186992,#186993,#186994,#186995,#186996,#186997,#186998,#186999,#187000,
#187001,#187002,#187003,#187004,#187005,#187006,#187007,#187008,#187009,
#187010,#187011,#187012,#187013,#187014,#187015,#187016,#187017,#187018,
#187019,#187020,#187021,#187022,#187023,#187024,#187025,#187026,#187027,
#187028,#187029,#187030,#187031,#187032,#187033,#187034,#187035,#187036,
#187037,#187038,#187039,#187040,#187041,#187042,#187043,#187044,#187045,
#187046,#187047,#187048),.UNSPECIFIED.,.F.,.F.,(4,2,2,2,2,2,2,2,2,2,2,2,
2,2,2,2,2,2,2,2,2,2,2,2,2,2,2,2,2,2,2,2,2,2,2,2,2,2,2,2,2,2,2,2,2,2,2,2,
2,2,2,2,2,2,2,2,2,2,2,2,2,2,2,2,2,2,2,2,2,2,2,2,2,2,2,2,2,2,2,2,2,2,2,2,
2,2,2,2,2,2,2,2,2,2,2,2,2,2,2,2,2,2,2,2,2,2,2,2,2,2,2,2,2,2,2,2,2,2,2,2,
2,2,2,2,2,2,2,2,2,2,2,2,2,2,2,2,2,2,2,2,2,2,2,2,2,2,2,4),(0.0752219443712125,
0.0876741589246509,0.0938319992011081,0.0964930602826022,0.0984459259287984,
0.100248442114753,0.103169025493228,0.110390158188158,0.154176294194007,
0.195389487801746,0.199210492316058,0.201236328242508,0.202548271249196,
0.203772196473567,0.203775760638908,0.203779337406272,0.203782926793875,
0.203786752196306,0.203790639193609,0.203794588949303,0.203798602988633,
0.203802682582228,0.203806828968806,0.203811043788491,0.203815328656416,
0.203819685085049,0.203824114634023,0.203828618842948,0.20383319940526,
0.203837858157001,0.203842596887828,0.203847417344461,0.203852321440246,
0.203857311144556,0.203862388531956,0.203867555672481,0.203872814614456,
0.203878167614088,0.203883616968383,0.203889165102637,0.20389481435452,
0.203900567237911,0.204946646809773,0.20633648647122,0.208644419526527,
0.222699790354313,0.225486226583975,0.260904545343977,0.288832623753712,
0.303595725234263,0.307269947312214,0.30943720552109,0.311353669210471,
0.313753136775027,0.31748505469894,0.336116257030104,0.38037337776533,0.402096069778575,
0.412263463198908,0.414465903275958,0.415706920918454,0.416779704806643,
0.418148105791884,0.420959801995392,0.44205134961489,0.488505393083269,
0.512080552203394,0.517869970015435,0.520465800509764,0.522407891886507,
0.524227210683245,0.526741675709619,0.53321302692565,0.590596699260725,
0.61366136024826,0.624210159324676,0.626437064200589,0.627683484682615,
0.628755706021515,0.630116640354069,0.632800196507584,0.650505405323888,
0.698831972572652,0.717121417331737,0.728196142673682,0.73152948505618,
0.733621337627878,0.735555006061041,0.738052559850852,0.742198393831729,
0.770156025124721,0.823837018238989,0.836036730997686,0.838358160751868,
0.839625163885281,0.840695717955886,0.842030096170982,0.844105016945603,
0.85405834330488,0.859539959206553,0.85998801824992,0.866875720218246,0.88060109322453,
0.91346023515796,0.930021201358598,0.94033198236359,0.943580750552406,0.945654149542356,
0.947594928402469,0.950136272042241,0.954431684263708,0.989556857113646,
1.03848555421248,1.04826059725288,1.05043720290348,1.05167273380006,1.05274655787461,
1.05412383587971,1.05697955512463,1.07976013037356,1.09260331190984,1.12545738352177,
1.14200978542588,1.15231699138319,1.15556556846554,1.15763907029967,1.15958010336284,
1.16212200777224,1.16641887870625,1.20162447618504,1.25080410079112,1.26029292673091,
1.26244980068617,1.26368107044931,1.26475566998545,1.26613982522458,1.26903023718907,
1.29473233270021,1.33417764185622,1.3619000757016,1.36604053272241,1.36853691973143,
1.37047090166261,1.37256430523393,1.37590273724581,1.38701853300503,1.40540343092708,
1.40862562901102),.UNSPECIFIED.);
#1926=B_SPLINE_CURVE_WITH_KNOTS('',3,(#187054,#187055,#187056,#187057,#187058,
#187059,#187060,#187061,#187062,#187063,#187064,#187065,#187066,#187067,
#187068,#187069,#187070,#187071,#187072,#187073,#187074,#187075,#187076,
#187077,#187078,#187079),.UNSPECIFIED.,.F.,.F.,(4,2,2,2,2,2,2,2,2,2,2,2,
4),(2.59396462623471,2.61326336975643,2.62537967530848,2.62720696852797,
2.62820845138943,2.63689624976139,2.64004737281275,2.64189441921288,2.64374937154851,
2.64561742100235,2.64801886758359,2.65175877907383,2.66839194337532),
 .UNSPECIFIED.);
#1927=B_SPLINE_CURVE_WITH_KNOTS('',3,(#187080,#187081,#187082,#187083,#187084,
#187085,#187086,#187087,#187088,#187089,#187090,#187091,#187092,#187093,
#187094,#187095,#187096,#187097,#187098,#187099,#187100,#187101,#187102,
#187103,#187104,#187105,#187106,#187107,#187108,#187109,#187110,#187111,
#187112,#187113,#187114,#187115,#187116,#187117,#187118,#187119,#187120,
#187121,#187122,#187123,#187124,#187125,#187126,#187127,#187128,#187129,
#187130,#187131,#187132,#187133,#187134,#187135,#187136,#187137,#187138,
#187139,#187140,#187141,#187142,#187143,#187144,#187145,#187146,#187147,
#187148,#187149,#187150,#187151,#187152,#187153,#187154,#187155,#187156,
#187157,#187158,#187159,#187160,#187161,#187162,#187163,#187164,#187165,
#187166,#187167,#187168,#187169,#187170,#187171,#187172,#187173,#187174,
#187175,#187176,#187177,#187178,#187179,#187180,#187181,#187182,#187183,
#187184,#187185,#187186,#187187,#187188,#187189,#187190,#187191,#187192,
#187193,#187194,#187195,#187196,#187197,#187198,#187199,#187200,#187201,
#187202,#187203,#187204,#187205,#187206,#187207,#187208,#187209,#187210,
#187211,#187212,#187213,#187214,#187215,#187216,#187217,#187218,#187219,
#187220,#187221,#187222,#187223,#187224,#187225,#187226,#187227,#187228,
#187229,#187230,#187231,#187232,#187233,#187234,#187235,#187236,#187237,
#187238,#187239,#187240,#187241,#187242,#187243,#187244,#187245,#187246,
#187247,#187248,#187249,#187250,#187251,#187252,#187253,#187254,#187255,
#187256,#187257,#187258,#187259,#187260),.UNSPECIFIED.,.F.,.F.,(4,3,3,3,
3,3,3,3,3,3,3,3,3,3,3,3,3,3,3,3,3,3,3,3,3,3,3,3,3,3,3,3,3,3,3,3,3,3,3,3,
3,3,3,3,3,3,3,3,3,3,3,3,3,3,3,3,3,3,3,3,4),(83.3413404136697,83.4431910990492,
83.5450419838146,83.6469948549843,83.749004646587,83.8511877914694,83.9022617967974,
84.0056565338453,84.1088978159602,84.2120177813525,84.3150723495614,84.4180955579192,
84.5211214005918,84.6242541673699,84.7274432587797,84.8308152521614,84.9010982467593,
85.0044929838073,85.1077342659222,85.2108542313146,85.3139087995235,85.4169320078814,
85.5199578505541,85.6230906173322,85.726279708742,85.8296517021237,85.8999346967212,
86.0033294337691,86.1065707158841,86.2096906812763,86.3127452494852,86.4157684578429,
86.5187943005153,86.6219270672933,86.725116158703,86.8284881520847,86.898771146683,
87.0021658837309,87.1054071658459,87.2085271312383,87.3115816994472,87.4146049078051,
87.5176307504777,87.6207635172557,87.7239526086656,87.8273246020472,87.8976075966449,
88.0010023336927,88.1042436158081,88.2073635812004,88.3104181494092,88.4134413577669,
88.5164672004396,88.6195999672179,88.7227890586277,88.8261610520094,88.8964440466068,
89.013226996161,89.1295586830716,89.2451399878319,89.2739307161836),
 .UNSPECIFIED.);
#1928=B_SPLINE_CURVE_WITH_KNOTS('',3,(#187262,#187263,#187264,#187265,#187266,
#187267,#187268,#187269,#187270,#187271,#187272,#187273,#187274,#187275,
#187276,#187277,#187278,#187279,#187280,#187281,#187282,#187283,#187284,
#187285,#187286,#187287,#187288,#187289,#187290,#187291,#187292,#187293,
#187294,#187295,#187296,#187297,#187298,#187299,#187300,#187301,#187302,
#187303,#187304,#187305,#187306,#187307,#187308,#187309,#187310,#187311,
#187312,#187313,#187314,#187315,#187316,#187317,#187318,#187319,#187320,
#187321,#187322,#187323,#187324,#187325,#187326,#187327,#187328,#187329,
#187330,#187331,#187332,#187333,#187334,#187335,#187336,#187337,#187338,
#187339,#187340,#187341,#187342,#187343,#187344,#187345,#187346,#187347,
#187348,#187349,#187350,#187351,#187352,#187353,#187354,#187355,#187356,
#187357,#187358,#187359,#187360,#187361,#187362,#187363,#187364,#187365,
#187366,#187367,#187368,#187369,#187370,#187371,#187372,#187373,#187374,
#187375,#187376,#187377,#187378,#187379,#187380,#187381,#187382,#187383,
#187384,#187385,#187386,#187387,#187388,#187389,#187390,#187391,#187392,
#187393,#187394,#187395,#187396,#187397,#187398,#187399,#187400,#187401,
#187402,#187403,#187404,#187405,#187406,#187407,#187408,#187409,#187410,
#187411,#187412,#187413,#187414,#187415,#187416,#187417,#187418,#187419,
#187420,#187421,#187422,#187423,#187424,#187425,#187426,#187427,#187428,
#187429,#187430,#187431,#187432,#187433,#187434,#187435,#187436,#187437,
#187438,#187439,#187440,#187441,#187442,#187443,#187444,#187445,#187446,
#187447,#187448,#187449,#187450,#187451,#187452,#187453,#187454,#187455,
#187456,#187457,#187458,#187459,#187460,#187461,#187462,#187463,#187464,
#187465,#187466,#187467,#187468,#187469,#187470,#187471,#187472,#187473,
#187474,#187475,#187476,#187477,#187478,#187479,#187480,#187481,#187482,
#187483,#187484,#187485,#187486,#187487,#187488,#187489,#187490,#187491,
#187492,#187493,#187494,#187495,#187496,#187497,#187498,#187499,#187500,
#187501,#187502,#187503,#187504,#187505,#187506,#187507,#187508,#187509,
#187510,#187511,#187512,#187513,#187514,#187515,#187516,#187517,#187518,
#187519,#187520,#187521,#187522,#187523),.UNSPECIFIED.,.F.,.F.,(4,2,2,2,
2,2,2,2,2,2,2,2,2,2,2,2,2,2,2,2,2,2,2,2,2,2,2,2,2,2,2,2,2,2,2,2,2,2,2,2,
2,2,2,2,2,2,2,2,2,2,2,2,2,2,2,2,2,2,2,2,2,2,2,2,2,2,2,2,2,2,2,2,2,2,2,2,
2,2,2,2,2,2,2,2,2,2,2,2,2,2,2,2,2,2,2,2,2,2,2,2,2,2,2,2,2,2,2,2,2,2,2,2,
2,2,2,2,2,2,2,2,2,2,2,2,2,2,2,2,2,2,4),(1.40862562901102,1.45275465334309,
1.47131667206135,1.47406295265149,1.47541864509015,1.4764907850887,1.47774177390752,
1.47998843675736,1.49085062078179,1.51505365069752,1.55568297615944,1.57463747693525,
1.5783919344153,1.58079885741186,1.58271672890813,1.58488073561894,1.58853766675947,
1.60307206654821,1.63032533179596,1.67876836451512,1.68478514663889,1.68670426430569,
1.68788277604679,1.68897140844695,1.69045822973662,1.6939032895456,1.72313346562477,
1.74570987834384,1.78562285200694,1.79036910634731,1.79279768191903,1.79471784950775,
1.79686871775279,1.80046581033984,1.81427971855126,1.86523494593173,1.89514137108093,
1.89805696143434,1.89944616672057,1.90052145330931,1.90174990168535,1.90389334615704,
1.91319086897048,1.93203874251219,1.97244588542559,1.98470982990822,1.99933013990606,
2.00312041203308,2.00533624404761,2.00724903495114,2.00958446798186,2.01403440309192,
2.04490939879905,2.09135879679525,2.10759225452143,2.11022186822737,2.11157166359224,
2.11264356663356,2.11389939757671,2.11616765925701,2.12738963437662,2.1529565248882,
2.20656388285264,2.21341078381916,2.2162702887456,2.21806246255446,2.22002606159702,
2.22274177776183,2.22921303650886,2.283454208799,2.31941439185054,2.32227322542457,
2.32365141102349,2.32472566011931,2.3259613694899,2.32813753333291,2.33789844169634,
2.3868339999351,2.42195761873526,2.42625780458589,2.42880105388566,2.43074274832793,
2.43079405246234,2.43083662180819,2.43087314323725,2.43090447337441,2.43093134891346,
2.43095440282948,2.4309741786094,2.43099713623213,2.43101930521496,2.43104071477006,
2.43106139240282,2.43108136458104,2.43110065676173,2.4311192934721,2.43113729830345,
2.431154693942,2.43117150224622,2.43118774422328,2.43120344010428,2.43121860935849,
2.43123326905954,2.43124743556367,2.43126112922914,2.43127436672901,2.43347744507451,
2.43737358079612,2.44215984439604,2.45216496583788,2.48140966241379,2.52925235737917,
2.53360373449368,2.53528822805322,2.53630295226307,2.5374036461747,2.5389585551921,
2.54280720810928,2.56141800128267,2.61332592834438,2.62544453509487,2.62727217388184,
2.62827386152683,2.63696330633214,2.64011502741922,2.64196242458428,2.64381772922041,
2.64568613360734,2.64808803658774,2.65182865902094,2.66846498743977),
 .UNSPECIFIED.);
#1929=B_SPLINE_CURVE_WITH_KNOTS('',3,(#187524,#187525,#187526,#187527,#187528,
#187529,#187530,#187531,#187532,#187533),.UNSPECIFIED.,.F.,.F.,(4,3,3,4),
(-85.8723818947888,-85.7556989608338,-85.6390734939892,-85.5224480271446),
 .UNSPECIFIED.);
#1930=B_SPLINE_CURVE_WITH_KNOTS('',3,(#187538,#187539,#187540,#187541,#187542,
#187543,#187544,#187545,#187546,#187547,#187548,#187549,#187550,#187551,
#187552,#187553,#187554,#187555,#187556,#187557,#187558,#187559,#187560,
#187561,#187562,#187563,#187564,#187565,#187566,#187567,#187568,#187569,
#187570,#187571,#187572,#187573,#187574,#187575,#187576,#187577,#187578,
#187579,#187580,#187581,#187582,#187583,#187584,#187585,#187586,#187587,
#187588,#187589,#187590,#187591,#187592,#187593,#187594,#187595,#187596,
#187597,#187598,#187599,#187600,#187601,#187602,#187603,#187604,#187605,
#187606,#187607,#187608,#187609,#187610,#187611,#187612,#187613,#187614,
#187615,#187616,#187617,#187618,#187619,#187620,#187621,#187622,#187623,
#187624,#187625,#187626,#187627,#187628,#187629,#187630,#187631,#187632,
#187633,#187634,#187635,#187636,#187637,#187638,#187639,#187640,#187641,
#187642,#187643,#187644,#187645,#187646,#187647,#187648,#187649,#187650,
#187651,#187652,#187653,#187654,#187655,#187656,#187657,#187658,#187659,
#187660,#187661,#187662,#187663,#187664,#187665,#187666,#187667,#187668,
#187669,#187670,#187671,#187672,#187673,#187674,#187675,#187676,#187677,
#187678,#187679,#187680,#187681,#187682,#187683,#187684,#187685,#187686,
#187687,#187688,#187689,#187690,#187691,#187692,#187693,#187694,#187695,
#187696,#187697,#187698,#187699,#187700,#187701,#187702,#187703,#187704,
#187705,#187706,#187707,#187708,#187709,#187710,#187711,#187712,#187713,
#187714,#187715,#187716,#187717,#187718,#187719,#187720,#187721,#187722,
#187723,#187724,#187725,#187726,#187727,#187728,#187729,#187730,#187731,
#187732,#187733,#187734,#187735,#187736,#187737,#187738,#187739,#187740,
#187741,#187742,#187743,#187744,#187745,#187746,#187747,#187748,#187749,
#187750,#187751,#187752,#187753,#187754,#187755,#187756,#187757,#187758,
#187759,#187760,#187761,#187762,#187763,#187764,#187765,#187766,#187767,
#187768,#187769,#187770,#187771,#187772,#187773,#187774,#187775,#187776,
#187777,#187778,#187779,#187780,#187781,#187782,#187783,#187784,#187785,
#187786,#187787,#187788,#187789,#187790,#187791,#187792,#187793,#187794,
#187795,#187796,#187797,#187798,#187799,#187800,#187801,#187802,#187803,
#187804,#187805,#187806,#187807),.UNSPECIFIED.,.F.,.F.,(4,2,2,2,2,2,2,2,
2,2,2,2,2,2,2,2,2,2,2,2,2,2,2,2,2,2,2,2,2,2,2,2,2,2,2,2,2,2,2,2,2,2,2,2,
2,2,2,2,2,2,2,2,2,2,2,2,2,2,2,2,2,2,2,2,2,2,2,2,2,2,2,2,2,2,2,2,2,2,2,2,
2,2,2,2,2,2,2,2,2,2,2,2,2,2,2,2,2,2,2,2,2,2,2,2,2,2,2,2,2,2,2,2,2,2,2,2,
2,2,2,2,2,2,2,2,2,2,2,2,2,2,2,2,2,2,4),(1.26011167467531,1.26036620110984,
1.26252309759977,1.26375438023324,1.26482899100896,1.26621316074654,1.26910360307005,
1.2948059918053,1.33425167466812,1.36197439259648,1.36611489261192,1.36861130563355,
1.370545307773,1.37263873327601,1.37597720039364,1.38709311436655,1.40547820955506,
1.45282977752233,1.47139210604318,1.47413841893173,1.47549412626162,1.47656627752368,
1.47781727890539,1.48006396287666,1.49092622141433,1.51512936044351,1.55575920931139,
1.57471396780341,1.57846846917351,1.58087541875538,1.58279331043829,1.58495733886781,
1.5886143041484,1.60314880564022,1.63040221068751,1.67884451695401,1.68486249706948,
1.68678177571617,1.68796033119809,1.68904896250635,1.69053572317125,1.6939803842591,
1.72945135535193,1.78246408786581,1.78935678807242,1.79222364275473,1.79401701111302,
1.79597917410697,1.79868786515744,1.80511844941566,1.83379302284758,1.88510089038917,
1.89612188860234,1.89826694383392,1.89962305806149,1.9006953264991,1.90194622919679,
1.90419214778577,1.915039386318,1.93918522414623,1.99489369855084,2.00154884603247,
2.0040934196725,2.00592116805771,2.00785994413729,2.01043031510689,2.01607650279299,
2.03857613371646,2.07130937252344,2.1074095970491,2.11026970295025,2.11164800382076,
2.1127221089369,2.11395738884392,2.11613216586542,2.12587645497241,2.17481666259083,
2.20996024630414,2.21424769056579,2.21678703264344,2.21872783628879,2.22080276870796,
2.22405708904639,2.23441203774115,2.25107160559055,2.28404496995142,2.30299084398414,
2.30503213119893,2.30689970820413,2.3199977489731,2.32225818933318,2.32364912620884,
2.32472444563532,2.32595147163909,2.32808902506277,2.33730875288676,2.35591434346865,
2.40015966834944,2.42257657244587,2.42652189651186,2.42898690292306,2.43091098599602,
2.43093283747588,2.43095158235253,2.43097432285093,2.4309962825178,2.431017490333,
2.43103797350346,2.43105775823301,2.43107686974478,2.43109533224338,2.43111316913073,
2.43113040285866,2.43114705501466,2.43116314644866,2.43117869716484,2.43119372642108,
2.43120825105012,2.43122228711152,2.43123585496406,2.43124897111116,2.43345298341257,
2.43735447449341,2.44214904098073,2.45217907199654,2.48154435456666,2.52915549901937,
2.53354229444586,2.53523233117229,2.5362479929801,2.53734757336637,2.53889734934271,
2.54271553111527,2.56104983964384,2.59396462623471),.UNSPECIFIED.);
#1931=B_SPLINE_CURVE_WITH_KNOTS('',3,(#187809,#187810,#187811,#187812,#187813,
#187814,#187815,#187816,#187817,#187818,#187819,#187820,#187821,#187822,
#187823,#187824,#187825,#187826,#187827,#187828,#187829,#187830,#187831,
#187832,#187833,#187834,#187835,#187836,#187837,#187838,#187839,#187840,
#187841,#187842,#187843,#187844,#187845,#187846,#187847,#187848,#187849,
#187850,#187851,#187852,#187853,#187854,#187855,#187856,#187857,#187858,
#187859,#187860,#187861,#187862,#187863,#187864,#187865,#187866,#187867,
#187868,#187869,#187870,#187871,#187872,#187873,#187874,#187875,#187876,
#187877,#187878,#187879,#187880,#187881,#187882,#187883,#187884,#187885,
#187886,#187887,#187888,#187889,#187890,#187891,#187892,#187893,#187894,
#187895,#187896,#187897,#187898,#187899,#187900,#187901,#187902,#187903,
#187904,#187905,#187906,#187907,#187908,#187909,#187910,#187911,#187912,
#187913,#187914,#187915,#187916,#187917,#187918,#187919,#187920,#187921,
#187922,#187923,#187924,#187925,#187926,#187927,#187928,#187929,#187930,
#187931,#187932,#187933,#187934,#187935,#187936,#187937,#187938,#187939,
#187940,#187941,#187942,#187943,#187944,#187945,#187946,#187947,#187948,
#187949,#187950,#187951,#187952,#187953,#187954,#187955,#187956,#187957,
#187958,#187959,#187960,#187961,#187962,#187963,#187964,#187965,#187966,
#187967,#187968,#187969,#187970,#187971,#187972,#187973,#187974,#187975,
#187976,#187977,#187978,#187979,#187980,#187981,#187982,#187983,#187984,
#187985,#187986,#187987,#187988,#187989),.UNSPECIFIED.,.F.,.F.,(4,3,3,3,
3,3,3,3,3,3,3,3,3,3,3,3,3,3,3,3,3,3,3,3,3,3,3,3,3,3,3,3,3,3,3,3,3,3,3,3,
3,3,3,3,3,3,3,3,3,3,3,3,3,3,3,3,3,3,3,3,4),(-91.8056330559226,-91.703478392047,
-91.6014794906872,-91.4995669524813,-91.397705213372,-91.2958587787104,
-91.193920770489,-91.0919397623291,-90.9897717066981,-90.8941169465305,
-90.7907222094827,-90.6874809273678,-90.5843609619755,-90.4813063937666,
-90.3782831854088,-90.2752573427364,-90.1721245759583,-90.0689354845486,
-89.965563491167,-89.8952804965687,-89.7918857595209,-89.6886444774056,
-89.5855245120134,-89.4824699438045,-89.3794467354468,-89.2764208927745,
-89.1732881259964,-89.0700990345866,-88.966727041205,-88.8964440466068,
-88.7930493095589,-88.6898080274438,-88.5866880620515,-88.4836334938425,
-88.3806102854848,-88.2775844428123,-88.1744516760343,-88.0712625846244,
-87.9678905912427,-87.8976075966449,-87.794212859597,-87.6909715774818,
-87.5878516120896,-87.4847970438808,-87.3817738355231,-87.2787479928507,
-87.1756152260725,-87.0724261346628,-86.9690541412812,-86.898771146683,
-86.7953764096352,-86.69213512752,-86.5890151621277,-86.4859605939188,-86.382937385561,
-86.2799115428887,-86.1767787761105,-86.0735896847008,-85.9702176913191,
-85.8999346967212,-85.8723818947888),.UNSPECIFIED.);
#1932=B_SPLINE_CURVE_WITH_KNOTS('',3,(#187990,#187991,#187992,#187993,#187994),
 .UNSPECIFIED.,.F.,.F.,(4,1,4),(-92.1566391646458,-91.8929533964924,-91.8056333339369),
 .UNSPECIFIED.);
#1933=B_SPLINE_CURVE_WITH_KNOTS('',3,(#188000,#188001,#188002,#188003,#188004,
#188005,#188006,#188007,#188008,#188009,#188010,#188011,#188012,#188013,
#188014,#188015,#188016,#188017,#188018,#188019,#188020,#188021),
 .UNSPECIFIED.,.F.,.F.,(4,2,2,2,2,2,2,2,2,2,4),(2.59434030580712,2.6245953507381,
2.6484152592862,2.65628687327347,2.65838285903235,2.65961282848372,2.66066963231726,
2.66171552239248,2.66306594609527,2.66552398461768,2.6686176292093),
 .UNSPECIFIED.);
#1934=B_SPLINE_CURVE_WITH_KNOTS('',3,(#188022,#188023,#188024,#188025,#188026,
#188027,#188028,#188029,#188030,#188031,#188032,#188033,#188034,#188035,
#188036,#188037,#188038,#188039,#188040,#188041,#188042,#188043,#188044,
#188045,#188046,#188047,#188048,#188049,#188050,#188051,#188052,#188053,
#188054,#188055,#188056,#188057,#188058,#188059,#188060,#188061,#188062,
#188063,#188064,#188065,#188066,#188067,#188068,#188069,#188070,#188071,
#188072,#188073,#188074,#188075,#188076,#188077,#188078,#188079,#188080,
#188081,#188082,#188083,#188084,#188085,#188086,#188087,#188088,#188089,
#188090,#188091,#188092,#188093,#188094,#188095,#188096,#188097,#188098,
#188099,#188100,#188101,#188102,#188103,#188104,#188105,#188106,#188107,
#188108,#188109,#188110,#188111,#188112,#188113,#188114,#188115,#188116,
#188117,#188118,#188119,#188120,#188121,#188122,#188123,#188124,#188125,
#188126,#188127,#188128,#188129,#188130,#188131,#188132,#188133,#188134,
#188135,#188136,#188137,#188138,#188139,#188140,#188141,#188142,#188143,
#188144,#188145,#188146,#188147,#188148,#188149,#188150,#188151,#188152,
#188153,#188154,#188155,#188156,#188157,#188158,#188159,#188160,#188161,
#188162,#188163,#188164,#188165,#188166,#188167,#188168,#188169,#188170,
#188171,#188172,#188173,#188174,#188175,#188176,#188177,#188178,#188179,
#188180,#188181,#188182,#188183,#188184,#188185,#188186,#188187,#188188,
#188189,#188190,#188191,#188192,#188193,#188194,#188195,#188196,#188197,
#188198,#188199,#188200,#188201,#188202,#188203,#188204,#188205,#188206,
#188207,#188208,#188209,#188210,#188211,#188212,#188213,#188214,#188215,
#188216,#188217,#188218,#188219,#188220,#188221,#188222,#188223,#188224,
#188225,#188226,#188227,#188228,#188229,#188230,#188231,#188232,#188233,
#188234,#188235,#188236,#188237,#188238,#188239,#188240,#188241,#188242,
#188243,#188244,#188245,#188246,#188247,#188248,#188249,#188250,#188251,
#188252,#188253,#188254,#188255,#188256,#188257,#188258,#188259,#188260,
#188261,#188262,#188263),.UNSPECIFIED.,.F.,.F.,(4,2,2,2,2,2,2,2,2,2,2,2,
2,2,2,2,2,2,2,2,2,2,2,2,2,2,2,2,2,2,2,2,2,2,2,2,2,2,2,2,2,2,2,2,2,2,2,2,
2,2,2,2,2,2,2,2,2,2,2,2,2,2,2,2,2,2,2,2,2,2,2,2,2,2,2,2,2,2,2,2,2,2,2,2,
2,2,2,2,2,2,2,2,2,2,2,2,2,2,2,2,2,2,2,2,2,2,2,2,2,2,2,2,2,2,2,2,2,2,2,2,
4),(0.000817344774108441,0.0612254651869213,0.0876737802003372,0.0938318808098746,
0.0964929874989253,0.0984458613996463,0.100248367484044,0.10316889486537,
0.110389693522579,0.154248043816412,0.195394654296778,0.199212997128793,
0.201237831272896,0.202549359042334,0.203772991306706,0.203776558034222,
0.203780137465953,0.203783729587056,0.203787567161818,0.203791466614978,
0.203795429174728,0.203799456164751,0.203803549140782,0.20380770937905,
0.203811938279478,0.203816237472464,0.203820608422661,0.203825052813434,
0.203829572297477,0.203834168460689,0.203838843215121,0.203843598289257,
0.203848435483984,0.204892224678134,0.206274994503329,0.209159894927432,
0.24333536368996,0.277585018344356,0.294134253468309,0.304439228580753,
0.307686964814489,0.309759896851876,0.311700373268492,0.314241515163701,
0.318537021927793,0.353721240095344,0.402848914196404,0.412378986999385,
0.414538347548047,0.415769950810159,0.416844139401268,0.418226843280678,
0.421111008852201,0.445864786342485,0.488791041320977,0.512159280939036,
0.517921466523687,0.520512484215026,0.52245393171994,0.524274797102512,
0.52679481126563,0.533299398727068,0.590405896585106,0.613651227045902,
0.624250482074529,0.626480659006351,0.627727855653289,0.628800088943574,
0.630160194117394,0.632319147710258,0.643575675048509,0.694430300562819,
0.723203038571217,0.729644822313636,0.732354887197064,0.73431683582354,
0.736109180619974,0.738972588319888,0.745847597131116,0.799079313312624,
0.814907809651494,0.835599169805093,0.83822332834501,0.839554065022661,
0.840614463375584,0.841880332663877,0.844133041559424,0.853786512644175,
0.859625398223345,0.860058972458099,0.866943612928567,0.880670433562754,
0.913529926085419,0.93009107766879,0.940401971870878,0.943650774638628,
0.945724195442819,0.94766499454514,0.950206364438463,0.954501820478792,
0.989627292276999,1.03855634677172,1.04833167342516,1.05050831422143,1.05174386075997,
1.05281769567492,1.05419498399687,1.05705071230623,1.07983069381489,1.09267484391548,
1.12552926030726,1.14208184059342,1.15238915658118,1.15563776787846,1.15771129144662,
1.15965234478391,1.16219427564375,1.16649119107448,1.20169713841453,1.25087727607578,
1.26011167467531),.UNSPECIFIED.);
#1935=B_SPLINE_CURVE_WITH_KNOTS('',3,(#188265,#188266,#188267,#188268,#188269,
#188270,#188271,#188272,#188273,#188274),.UNSPECIFIED.,.F.,.F.,(4,1,1,1,
1,1,1,4),(-98.0888186411165,-97.8859720962637,-96.8871356463018,-95.8882991963399,
-94.889462746378,-93.8906262964162,-92.8917898464543,-92.1566391646458),
 .UNSPECIFIED.);
#1936=B_SPLINE_CURVE_WITH_KNOTS('',3,(#188275,#188276,#188277,#188278,#188279,
#188280,#188281,#188282,#188283,#188284,#188285,#188286,#188287,#188288,
#188289,#188290,#188291,#188292,#188293,#188294),.UNSPECIFIED.,.F.,.F.,
(4,2,2,2,2,2,2,2,2,4),(0.000629226904789768,0.0468422160482133,0.0541658165813541,
0.0579911959946999,0.0612752724550681,0.0633561448110693,0.0652934439714124,
0.0678152483376244,0.0720443780039375,0.07510365538255),.UNSPECIFIED.);
#1937=B_SPLINE_CURVE_WITH_KNOTS('',3,(#188299,#188300,#188301,#188302,#188303,
#188304,#188305,#188306,#188307,#188308,#188309,#188310,#188311,#188312,
#188313,#188314,#188315,#188316,#188317,#188318,#188319,#188320,#188321,
#188322,#188323,#188324,#188325,#188326,#188327,#188328,#188329,#188330,
#188331,#188332,#188333,#188334,#188335,#188336,#188337,#188338,#188339,
#188340,#188341,#188342,#188343,#188344,#188345,#188346,#188347,#188348,
#188349,#188350,#188351,#188352,#188353,#188354,#188355,#188356,#188357,
#188358,#188359,#188360,#188361,#188362,#188363,#188364,#188365,#188366,
#188367,#188368,#188369,#188370,#188371,#188372,#188373,#188374,#188375,
#188376,#188377,#188378,#188379,#188380,#188381,#188382,#188383,#188384,
#188385,#188386,#188387,#188388,#188389,#188390,#188391,#188392,#188393,
#188394,#188395,#188396,#188397,#188398,#188399,#188400,#188401,#188402,
#188403,#188404,#188405,#188406,#188407,#188408,#188409,#188410,#188411,
#188412,#188413,#188414,#188415,#188416,#188417,#188418,#188419,#188420,
#188421,#188422,#188423,#188424,#188425,#188426,#188427,#188428,#188429,
#188430,#188431,#188432,#188433,#188434,#188435,#188436,#188437,#188438,
#188439,#188440,#188441,#188442,#188443,#188444,#188445,#188446,#188447,
#188448,#188449,#188450,#188451,#188452,#188453,#188454,#188455,#188456,
#188457,#188458,#188459,#188460,#188461,#188462,#188463,#188464,#188465,
#188466,#188467,#188468,#188469,#188470,#188471,#188472,#188473,#188474,
#188475,#188476,#188477,#188478,#188479,#188480,#188481,#188482,#188483,
#188484,#188485,#188486,#188487,#188488,#188489,#188490,#188491,#188492,
#188493,#188494,#188495,#188496,#188497,#188498,#188499,#188500,#188501,
#188502,#188503,#188504,#188505,#188506,#188507,#188508,#188509,#188510,
#188511,#188512,#188513,#188514,#188515,#188516,#188517,#188518,#188519,
#188520,#188521,#188522,#188523,#188524,#188525,#188526,#188527,#188528,
#188529,#188530,#188531,#188532,#188533,#188534,#188535,#188536),
 .UNSPECIFIED.,.F.,.F.,(4,2,2,2,2,2,2,2,2,2,2,2,2,2,2,2,2,2,2,2,2,2,2,2,
2,2,2,2,2,2,2,2,2,2,2,2,2,2,2,2,2,2,2,2,2,2,2,2,2,2,2,2,2,2,2,2,2,2,2,2,
2,2,2,2,2,2,2,2,2,2,2,2,2,2,2,2,2,2,2,2,2,2,2,2,2,2,2,2,2,2,2,2,2,2,2,2,
2,2,2,2,2,2,2,2,2,2,2,2,2,2,2,2,2,2,2,2,2,2,4),(1.26027877606838,1.26524564787062,
1.27573161663081,1.27900123511885,1.28107979036348,1.28301970107747,1.2855517304173,
1.289813167522,1.3348183954334,1.3798748277065,1.38460060111834,1.38634311267145,
1.38736923049169,1.38846205987685,1.38997275181412,1.39355479886493,1.43119698698182,
1.4816257776398,1.4886851614224,1.49157992677149,1.4933786384757,1.49533699802944,
1.49802289353801,1.50431756659891,1.53185966588531,1.56026675308619,1.58259932665336,
1.59530772341971,1.59754854193088,1.59893374606931,1.60000868401374,1.601239816457,
1.60339519662903,1.61285792564873,1.6620489837926,1.69725782955956,1.70155559116883,
1.70409813391085,1.70603970764331,1.708113837747,1.7113635037859,1.72167496212459,
1.7382372576002,1.77113293498692,1.78487000733137,1.79174219333639,1.79195138979034,
1.79528676880761,1.80742214727915,1.80963215745186,1.81100801789834,1.81208197721038,
1.8133190746358,1.81550181014409,1.82536090297181,1.8742096216054,1.90930927696582,
1.91360534002856,1.91614729827708,1.91808866777881,1.92016281446589,1.92341299668222,
1.9337302254574,1.95030572194142,1.98321101347395,1.99803204453847,2.00309193599487,
2.01913276619391,2.0217547938998,2.02310286376967,2.02417453564695,2.02543141545218,
2.0277049202389,2.03902099952282,2.06495714148558,2.11802004762081,2.12490878320021,
2.12777496727722,2.12956820019529,2.1315304434071,2.13423966414903,2.14067349122147,
2.16937555772329,2.22064733913027,2.23167081379126,2.23381600625513,2.23517215443313,
2.23624441445118,2.2374952667592,2.23974099354813,2.25058535783602,2.27472070108179,
2.33044405824917,2.33709758063341,2.3396418834895,2.34146954722493,2.3434083345115,
2.34597889199367,2.35162618747065,2.37413421066519,2.40687263517928,2.44295971787812,
2.44581771749361,2.44719559579556,2.44823499175961,2.44943036425619,2.45070437258797,
2.45263807730776,2.45621530280002,2.46468816980605,2.52438370686324,2.54621101977488,
2.55012782909812,2.55258417318313,2.55450718821749,2.55664152460183,2.56016490711316,
2.573150222639,2.59434030580712),.UNSPECIFIED.);
#1938=B_SPLINE_CURVE_WITH_KNOTS('',3,(#188537,#188538,#188539,#188540,#188541,
#188542,#188543,#188544,#188545,#188546,#188547,#188548,#188549,#188550,
#188551,#188552,#188553,#188554,#188555,#188556,#188557,#188558,#188559,
#188560,#188561,#188562,#188563,#188564,#188565,#188566,#188567,#188568,
#188569,#188570,#188571,#188572,#188573,#188574,#188575,#188576,#188577,
#188578,#188579,#188580,#188581,#188582,#188583,#188584,#188585,#188586,
#188587,#188588,#188589,#188590,#188591,#188592,#188593,#188594,#188595,
#188596,#188597,#188598,#188599,#188600,#188601,#188602,#188603,#188604,
#188605,#188606,#188607,#188608,#188609,#188610,#188611,#188612,#188613,
#188614,#188615,#188616,#188617,#188618,#188619,#188620,#188621,#188622,
#188623,#188624,#188625,#188626,#188627,#188628,#188629,#188630,#188631,
#188632,#188633,#188634,#188635,#188636,#188637,#188638,#188639,#188640,
#188641,#188642,#188643,#188644,#188645,#188646,#188647,#188648,#188649,
#188650,#188651,#188652,#188653,#188654,#188655,#188656,#188657,#188658,
#188659,#188660,#188661,#188662,#188663,#188664,#188665,#188666,#188667,
#188668,#188669,#188670,#188671,#188672,#188673,#188674,#188675,#188676,
#188677,#188678,#188679,#188680,#188681,#188682,#188683,#188684,#188685,
#188686,#188687,#188688,#188689,#188690,#188691,#188692,#188693,#188694,
#188695,#188696,#188697,#188698,#188699,#188700,#188701,#188702,#188703,
#188704,#188705,#188706,#188707,#188708,#188709,#188710,#188711,#188712,
#188713,#188714,#188715,#188716,#188717,#188718,#188719,#188720,#188721,
#188722,#188723,#188724,#188725,#188726,#188727,#188728,#188729,#188730,
#188731,#188732,#188733,#188734,#188735,#188736,#188737,#188738,#188739,
#188740,#188741,#188742,#188743,#188744,#188745,#188746,#188747,#188748,
#188749,#188750,#188751,#188752,#188753,#188754,#188755,#188756,#188757,
#188758),.UNSPECIFIED.,.F.,.F.,(4,2,2,2,2,2,2,2,2,2,2,2,2,2,2,2,2,2,2,2,
2,2,2,2,2,2,2,2,2,2,2,2,2,2,2,2,2,2,2,2,2,2,2,2,2,2,2,2,2,2,2,2,2,2,2,2,
2,2,2,2,2,2,2,2,2,2,2,2,2,2,2,2,2,2,2,2,2,2,2,2,2,2,2,2,2,2,2,2,2,2,2,2,
2,2,2,2,2,2,2,2,2,2,2,2,2,2,2,2,2,2,4),(0.07510365538255,0.118699139152014,
0.138790157978397,0.156962085014619,0.16602189526956,0.16806255948916,0.169315637659534,
0.170387061309427,0.17173863570937,0.174378777665775,0.190911462663399,
0.199764478504622,0.243740970988521,0.259906867840923,0.269996178958814,
0.27324363747737,0.275316468634537,0.277256904275559,0.279798070205302,
0.284093791180943,0.319303404930741,0.368518684618085,0.37794588264825,
0.380097921466115,0.381327889660885,0.382402299070527,0.383787453978794,
0.386029423626997,0.398777710807198,0.401649171323257,0.405936049248987,
0.448926926547703,0.476866462847058,0.48320809679262,0.485901063361633,
0.487859811477717,0.48965557961469,0.492538340964345,0.499531593624987,
0.551068240041451,0.57808859415,0.589674108944058,0.591962278701603,0.59322204955337,
0.594293042224718,0.595636262538031,0.598237180575012,0.613807233449575,
0.620261548200421,0.661679496467052,0.688953302732904,0.69521402633163,
0.697893214611427,0.699849574778535,0.701648468285654,0.704547975669279,
0.711641360810562,0.761303033561479,0.799616738266917,0.803221278945533,
0.804735329128075,0.805828305971827,0.806852749917557,0.808588560148625,
0.81327372579607,0.854357786507452,0.900790720169797,0.907183012256262,
0.909884698727915,0.911845116798863,0.913639189823246,0.916512174419259,
0.92344550237546,0.97589545436355,1.00227087738279,1.01369608503042,1.01597534814017,
1.01723324088855,1.01830446553677,1.01965030011911,1.02226307429011,1.03811541458428,
1.04285979830379,1.05813854118807,1.09101595881515,1.10759857242159,1.11791919142461,
1.12116912421312,1.12324280182285,1.12518351520449,1.12772430247277,1.13201771977366,
1.17442051842454,1.20347967363437,1.22309674950585,1.22705216189747,1.2286239238493,
1.22972756779993,1.23073809209405,1.23240180520209,1.23662715741319,1.28597339651562,
1.32674441864755,1.33181099193912,1.33427077596588,1.33619387704901,1.33832563687611,
1.3418385910895,1.35471538062677,1.37741913899921,1.40857222162858),
 .UNSPECIFIED.);
#1939=B_SPLINE_CURVE_WITH_KNOTS('',3,(#188764,#188765,#188766,#188767),
 .UNSPECIFIED.,.F.,.F.,(4,4),(114.406674973133,114.756144625377),
 .UNSPECIFIED.);
#1940=B_SPLINE_CURVE_WITH_KNOTS('',3,(#188768,#188769,#188770,#188771,#188772,
#188773,#188774,#188775,#188776,#188777,#188778,#188779,#188780,#188781,
#188782,#188783,#188784,#188785,#188786,#188787,#188788,#188789,#188790,
#188791,#188792,#188793,#188794,#188795,#188796,#188797,#188798,#188799,
#188800,#188801,#188802,#188803,#188804,#188805,#188806,#188807,#188808,
#188809,#188810,#188811,#188812,#188813,#188814,#188815,#188816,#188817,
#188818,#188819,#188820,#188821,#188822,#188823,#188824,#188825,#188826,
#188827,#188828,#188829,#188830,#188831,#188832,#188833,#188834,#188835,
#188836,#188837,#188838,#188839,#188840,#188841,#188842,#188843,#188844,
#188845,#188846,#188847,#188848,#188849,#188850,#188851,#188852,#188853,
#188854,#188855,#188856,#188857,#188858,#188859,#188860,#188861,#188862,
#188863,#188864,#188865,#188866,#188867,#188868,#188869,#188870,#188871,
#188872,#188873,#188874,#188875,#188876,#188877,#188878,#188879,#188880,
#188881,#188882,#188883,#188884,#188885,#188886,#188887,#188888,#188889,
#188890,#188891,#188892,#188893,#188894,#188895,#188896,#188897,#188898,
#188899,#188900,#188901,#188902,#188903,#188904,#188905,#188906,#188907,
#188908,#188909,#188910,#188911,#188912,#188913,#188914,#188915,#188916,
#188917,#188918,#188919,#188920,#188921,#188922,#188923,#188924,#188925,
#188926,#188927,#188928,#188929,#188930,#188931,#188932,#188933,#188934,
#188935,#188936,#188937,#188938,#188939,#188940,#188941,#188942,#188943,
#188944,#188945,#188946,#188947,#188948,#188949,#188950,#188951,#188952,
#188953,#188954,#188955,#188956,#188957,#188958,#188959,#188960,#188961,
#188962,#188963,#188964,#188965,#188966,#188967,#188968,#188969,#188970,
#188971,#188972,#188973,#188974,#188975,#188976,#188977,#188978,#188979,
#188980,#188981,#188982,#188983),.UNSPECIFIED.,.F.,.F.,(4,2,2,2,2,2,2,2,
2,2,2,2,2,2,2,2,2,2,2,2,2,2,2,2,2,2,2,2,2,2,2,2,2,2,2,2,2,2,2,2,2,2,2,2,
2,2,2,2,2,2,2,2,2,2,2,2,2,2,2,2,2,2,2,2,2,2,2,2,2,2,2,2,2,2,2,2,2,2,2,2,
2,2,2,2,2,2,2,2,2,2,2,2,2,2,2,2,2,2,2,2,2,2,2,2,2,2,2,4),(0.000658788637333733,
0.00332970111957805,0.00592165798483083,0.0077887962721166,0.00964368910378566,
0.0114909184364534,0.0146445377755957,0.0233614973535325,0.0917305383706879,
0.109072658587112,0.11278023260465,0.114311678894522,0.115407806628788,
0.116427795994408,0.118140544916847,0.122673808701606,0.169412955505319,
0.208756977489166,0.213872139697951,0.216839912671708,0.218921119844328,
0.220936314295769,0.222824215644402,0.225366501659542,0.229665126650277,
0.264781240463593,0.313699435168169,0.323487525706099,0.325665035363407,
0.326900771559257,0.327974577129087,0.329351574097245,0.332205826048581,
0.368431090342151,0.401082247997168,0.423502301778862,0.42913761828349,
0.431705733361184,0.433643908600663,0.435471904780948,0.438018132669157,
0.444685431694998,0.50028231196104,0.507358872502943,0.526258691274849,
0.535571224662673,0.537715472399808,0.538943942213686,0.540018966728738,
0.541407452178281,0.544320203781764,0.575418056595013,0.612230822589427,
0.635386119473837,0.641120659152872,0.643707074772631,0.645648217483469,
0.647471088553852,0.649997525125904,0.656539227443313,0.713347962515895,
0.73680029409589,0.747457798552966,0.749692019981419,0.750940309815345,
0.75201275803801,0.753372203310128,0.756047454830763,0.773495653696656,
0.823321313642927,0.840834961354449,0.85157199955984,0.854869286014235,
0.856953659334793,0.858890851091243,0.86140772925105,0.865618046493869,
0.896124831263709,0.94741967598083,0.959389844840715,0.96169968808587,0.962964446605137,
0.964035530772473,0.965373629313709,0.967459886864002,0.977570751556628,
0.983042494056251,0.992430706109514,1.00400338717725,1.0368541374581,1.05339725147272,
1.06370090016748,1.06694954215721,1.06902337064208,1.07096490991329,1.07350776651685,
1.07780689570321,1.11312122396326,1.1623815072661,1.1717202766068,1.17386678628622,
1.17509594511129,1.17617117717746,1.17755940925831,1.18046979137668,1.20860412800414,
1.24829816471492,1.26027877606838),.UNSPECIFIED.);
#1941=B_SPLINE_CURVE_WITH_KNOTS('',3,(#188985,#188986,#188987,#188988,#188989,
#188990,#188991,#188992,#188993,#188994,#188995,#188996,#188997,#188998,
#188999,#189000,#189001,#189002,#189003,#189004,#189005,#189006,#189007,
#189008,#189009,#189010,#189011,#189012,#189013,#189014,#189015,#189016,
#189017,#189018,#189019,#189020,#189021,#189022,#189023,#189024,#189025,
#189026,#189027,#189028,#189029,#189030,#189031,#189032,#189033,#189034,
#189035,#189036,#189037,#189038,#189039,#189040,#189041,#189042,#189043,
#189044,#189045,#189046,#189047,#189048,#189049,#189050,#189051,#189052,
#189053,#189054,#189055,#189056,#189057,#189058,#189059,#189060,#189061,
#189062,#189063,#189064,#189065,#189066,#189067,#189068,#189069,#189070,
#189071,#189072,#189073,#189074,#189075,#189076,#189077,#189078,#189079,
#189080,#189081,#189082,#189083,#189084,#189085,#189086,#189087,#189088,
#189089,#189090,#189091,#189092,#189093,#189094,#189095,#189096,#189097,
#189098,#189099,#189100,#189101,#189102,#189103,#189104,#189105,#189106,
#189107,#189108,#189109,#189110,#189111,#189112,#189113,#189114,#189115,
#189116,#189117,#189118,#189119,#189120,#189121,#189122,#189123,#189124,
#189125,#189126,#189127,#189128,#189129,#189130,#189131,#189132,#189133,
#189134,#189135,#189136,#189137,#189138,#189139,#189140,#189141,#189142,
#189143,#189144,#189145,#189146,#189147,#189148,#189149,#189150,#189151,
#189152,#189153,#189154,#189155,#189156,#189157,#189158,#189159,#189160,
#189161,#189162,#189163,#189164,#189165,#189166,#189167,#189168,#189169,
#189170,#189171,#189172,#189173,#189174,#189175,#189176,#189177,#189178,
#189179,#189180,#189181,#189182,#189183,#189184,#189185,#189186,#189187,
#189188,#189189,#189190,#189191,#189192,#189193,#189194,#189195,#189196,
#189197,#189198,#189199,#189200,#189201,#189202,#189203,#189204,#189205,
#189206),.UNSPECIFIED.,.F.,.F.,(4,2,2,2,2,2,2,2,2,2,2,2,2,2,2,2,2,2,2,2,
2,2,2,2,2,2,2,2,2,2,2,2,2,2,2,2,2,2,2,2,2,2,2,2,2,2,2,2,2,2,2,2,2,2,2,2,
2,2,2,2,2,2,2,2,2,2,2,2,2,2,2,2,2,2,2,2,2,2,2,2,2,2,2,2,2,2,2,2,2,2,2,2,
2,2,2,2,2,2,2,2,2,2,2,2,2,2,2,2,2,2,4),(1.40857222162858,1.41601196621291,
1.42100658421054,1.437014651322,1.43963419002885,1.44098146932286,1.44205276994169,
1.44330951245523,1.44558352661543,1.45691767558778,1.48293080959558,1.5358538196761,
1.54274968095228,1.54561647356978,1.54740940340059,1.54937076536781,1.55207776171094,
1.55850153445692,1.58712745059703,1.63841311802035,1.64947573332078,1.65162287516071,
1.65297939018676,1.6540513628493,1.65530121610225,1.65754349297141,1.66833947213673,
1.69230077033749,1.74825904843145,1.75488481309453,1.75742427486285,1.75925028425679,
1.76118899524557,1.76376230885916,1.76942731039186,1.79207247719862,1.82489295865303,
1.82941820035558,1.86060916484884,1.86352135013834,1.8649095267517,1.86598429042938,
1.86721244711463,1.8693560986222,1.87866557813956,1.92780721490209,1.96318573935499,
1.96748360549925,1.97002551010166,1.97196619358772,1.97403898214715,1.9772857313156,
1.98758107209317,2.00411095854136,2.036969830897,2.04848618686941,2.05827421766093,
2.0596014028723,2.07316111869237,2.07544388020458,2.07682634267758,2.07790300662812,
2.079120337492,2.08121529030947,2.08987792153073,2.10679402429725,2.1487078611603,
2.17542931454792,2.17954288869872,2.18203092316495,2.18396310590975,2.18605923602294,
2.18941216618977,2.20067145355606,2.21939330033796,2.25481219237785,2.28447589334949,
2.28738994761945,2.28877841742604,2.2898531330865,2.29108092737305,2.29322322625946,
2.30251571352589,2.321353270603,2.36913766416976,2.3880417326222,2.39179138356116,
2.3941963025708,2.39611327166443,2.39827699939892,2.4019352539455,2.41628127405657,
2.46674259933934,2.49644247359409,2.49935661878363,2.50074512832049,2.50181987308139,
2.50304769876655,2.5043394976538,2.50898384579415,2.53311915742372,2.55402308522148,
2.59906813594801,2.60332525106049,2.6058552950734,2.60779401170569,2.60987160570751,
2.61314038063283,2.61694371300853,2.62420850232443,2.66783673935143),
 .UNSPECIFIED.);
#1942=B_SPLINE_CURVE_WITH_KNOTS('',3,(#189207,#189208,#189209,#189210,#189211,
#189212,#189213,#189214,#189215,#189216,#189217,#189218,#189219,#189220,
#189221,#189222,#189223,#189224,#189225,#189226),.UNSPECIFIED.,.F.,.F.,
(4,2,2,2,2,2,2,2,2,4),(0.000649987196025464,0.0375152697788105,0.0412926014893609,
0.0433020283636711,0.0446072096947876,0.0458444130242866,0.0469177254605004,
0.0482917845512197,0.0511320532093311,0.0747588704862031),.UNSPECIFIED.);
#1943=B_SPLINE_CURVE_WITH_KNOTS('',3,(#189232,#189233,#189234,#189235,#189236,
#189237,#189238,#189239,#189240,#189241),.UNSPECIFIED.,.F.,.F.,(4,3,3,4),
(120.689857252469,120.859210445387,120.9625796252,121.040543934877),
 .UNSPECIFIED.);
#1944=B_SPLINE_CURVE_WITH_KNOTS('',3,(#189242,#189243,#189244,#189245,#189246,
#189247,#189248,#189249,#189250,#189251),.UNSPECIFIED.,.F.,.F.,(4,1,1,1,
1,1,1,4),(114.756144625377,114.866191745616,115.865028195577,116.863864645539,
117.862701095501,118.861537545463,119.860373995425,120.689851222923),
 .UNSPECIFIED.);
#1945=B_SPLINE_CURVE_WITH_KNOTS('',3,(#189252,#189253,#189254,#189255,#189256,
#189257,#189258,#189259,#189260,#189261,#189262,#189263,#189264,#189265,
#189266,#189267,#189268,#189269,#189270,#189271,#189272,#189273,#189274,
#189275,#189276,#189277,#189278,#189279,#189280,#189281,#189282,#189283,
#189284,#189285,#189286,#189287,#189288,#189289,#189290,#189291,#189292,
#189293,#189294,#189295,#189296,#189297,#189298,#189299,#189300,#189301,
#189302,#189303,#189304,#189305,#189306,#189307,#189308,#189309,#189310,
#189311,#189312,#189313,#189314,#189315,#189316,#189317,#189318,#189319,
#189320,#189321,#189322,#189323,#189324,#189325,#189326,#189327,#189328,
#189329,#189330,#189331,#189332,#189333,#189334,#189335,#189336,#189337,
#189338,#189339,#189340,#189341,#189342,#189343,#189344,#189345,#189346,
#189347,#189348,#189349,#189350,#189351,#189352,#189353,#189354,#189355,
#189356,#189357,#189358,#189359,#189360,#189361,#189362,#189363,#189364,
#189365,#189366,#189367,#189368,#189369,#189370,#189371,#189372,#189373,
#189374,#189375,#189376,#189377,#189378,#189379,#189380,#189381,#189382,
#189383,#189384,#189385,#189386,#189387,#189388,#189389,#189390,#189391,
#189392,#189393,#189394,#189395,#189396,#189397,#189398,#189399,#189400,
#189401,#189402,#189403,#189404,#189405,#189406,#189407,#189408,#189409,
#189410,#189411,#189412,#189413,#189414,#189415,#189416,#189417,#189418,
#189419,#189420,#189421,#189422,#189423,#189424,#189425,#189426,#189427,
#189428,#189429,#189430,#189431,#189432,#189433,#189434,#189435,#189436,
#189437,#189438,#189439,#189440,#189441,#189442,#189443,#189444,#189445,
#189446,#189447,#189448,#189449,#189450,#189451,#189452,#189453,#189454,
#189455,#189456,#189457,#189458,#189459,#189460,#189461,#189462,#189463,
#189464,#189465,#189466,#189467,#189468,#189469),.UNSPECIFIED.,.F.,.F.,
(4,2,2,2,2,2,2,2,2,2,2,2,2,2,2,2,2,2,2,2,2,2,2,2,2,2,2,2,2,2,2,2,2,2,2,
2,2,2,2,2,2,2,2,2,2,2,2,2,2,2,2,2,2,2,2,2,2,2,2,2,2,2,2,2,2,2,2,2,2,2,2,
2,2,2,2,2,2,2,2,2,2,2,2,2,2,2,2,2,2,2,2,2,2,2,2,2,2,2,2,2,2,2,2,2,2,2,2,
2,4),(0.0747588704862031,0.0879796875914506,0.109399103567414,0.136182009928896,
0.146436010033092,0.149706911363353,0.151785008802629,0.153723604647455,
0.156252646399797,0.160506228968039,0.193184802618462,0.222554041233268,
0.24417378241774,0.254295211425213,0.256485211339123,0.257733365014667,
0.258805366163536,0.260163820267166,0.262835841752181,0.280215848789155,
0.329253311598265,0.347302167883071,0.354571947452605,0.360001949741997,
0.3625673735979,0.364504742840328,0.366332881450401,0.368880760219933,0.375561192794359,
0.430979853898787,0.455321450902922,0.466218687923793,0.468466985392535,
0.469718088090325,0.470789839695392,0.472144411134277,0.474886373864345,
0.493336504876162,0.537461488735937,0.565332010852523,0.571665396941172,
0.574357013475187,0.576315571226138,0.578111713398295,0.580996279706098,
0.588000060041619,0.639382620642811,0.666515110320237,0.678128410191859,
0.680418184617347,0.681678329648746,0.6827493338966,0.684092180189308,0.686691242659467,
0.70221623881318,0.708761595209357,0.722633932417734,0.755493994171886,
0.772056492469513,0.782367914809658,0.785616718771579,0.787690100637495,
0.789630835404042,0.792172080814284,0.796467236253541,0.831578359363654,
0.880465479843008,0.890288671174311,0.892468529653024,0.893704761456567,
0.894778462633567,0.89615462705336,0.899004754680048,0.935374706201895,
0.989163090681777,0.995619143227736,0.998331710887372,1.00029420497743,
1.00208617839788,1.00494710482001,1.01180638461694,1.06524498728573,1.09093524438299,
1.10218664443679,1.10445606215777,1.10571187074455,1.10678335530417,1.10813210827461,
1.11075817318423,1.12692235584457,1.1775803507223,1.20199434029795,1.20789436156687,
1.21051042605123,1.21245612434676,1.21427052072673,1.21676512939122,1.22311497297649,
1.28150396590647,1.30395462180309,1.3143318406434,1.31654824507083,1.31779253084383,
1.31886525492234,1.32022984923615,1.32240325942883,1.33389996252107,1.38263556947134,
1.40832429865576),.UNSPECIFIED.);
#1946=B_SPLINE_CURVE_WITH_KNOTS('',3,(#189475,#189476,#189477,#189478,#189479,
#189480,#189481,#189482),.UNSPECIFIED.,.F.,.F.,(4,2,2,4),(2.59381054906569,
2.59855973280992,2.62659690643914,2.66829332114253),.UNSPECIFIED.);
#1947=B_SPLINE_CURVE_WITH_KNOTS('',3,(#189483,#189484,#189485,#189486,#189487,
#189488,#189489,#189490,#189491,#189492,#189493,#189494,#189495,#189496,
#189497,#189498,#189499,#189500,#189501,#189502,#189503,#189504,#189505,
#189506,#189507,#189508,#189509,#189510,#189511,#189512,#189513,#189514,
#189515,#189516,#189517,#189518,#189519,#189520,#189521,#189522,#189523,
#189524,#189525,#189526,#189527,#189528,#189529,#189530,#189531,#189532,
#189533,#189534,#189535,#189536,#189537,#189538,#189539,#189540,#189541,
#189542,#189543,#189544,#189545,#189546,#189547,#189548,#189549,#189550,
#189551,#189552,#189553,#189554,#189555,#189556,#189557,#189558,#189559,
#189560,#189561,#189562,#189563,#189564,#189565,#189566,#189567,#189568,
#189569,#189570,#189571,#189572,#189573,#189574,#189575,#189576,#189577,
#189578,#189579,#189580,#189581,#189582,#189583,#189584,#189585,#189586,
#189587,#189588,#189589,#189590,#189591,#189592,#189593,#189594,#189595,
#189596,#189597,#189598,#189599,#189600,#189601,#189602,#189603,#189604,
#189605,#189606,#189607,#189608,#189609,#189610,#189611,#189612,#189613,
#189614,#189615,#189616,#189617,#189618,#189619,#189620,#189621,#189622,
#189623,#189624,#189625,#189626,#189627,#189628,#189629,#189630,#189631,
#189632,#189633,#189634,#189635,#189636,#189637,#189638,#189639,#189640,
#189641,#189642,#189643,#189644,#189645,#189646,#189647,#189648,#189649,
#189650,#189651,#189652,#189653,#189654,#189655,#189656,#189657,#189658,
#189659,#189660),.UNSPECIFIED.,.F.,.F.,(4,3,3,3,3,3,3,3,3,3,3,3,3,3,3,3,
3,3,3,3,3,3,3,3,3,3,3,3,3,3,3,3,3,3,3,3,3,3,3,3,3,3,3,3,3,3,3,3,3,3,3,3,
3,3,3,3,3,3,3,4),(121.040543934877,121.143685143129,121.246752596576,121.34978034831,
121.452802399964,121.555926023838,121.659098486548,121.76246199832,121.858046895349,
121.961441632397,122.064682914512,122.167802879905,122.270857448114,122.373880656472,
122.476906499145,122.580039265923,122.683228357333,122.786600350715,122.856883345311,
122.960278082359,123.063519364473,123.166639329865,123.269693898074,123.372717106431,
123.475742949104,123.578875715881,123.682064807291,123.785436800672,123.855719795272,
123.95911453232,124.062355814435,124.165475779827,124.268530348036,124.371553556394,
124.474579399066,124.577712165844,124.680901257254,124.784273250635,124.854556245234,
124.957950982282,125.061192264397,125.16431222979,125.267366797999,125.370390006357,
125.473415849029,125.576548615808,125.679737707218,125.7831097006,125.853392695196,
125.956787432244,126.060028714359,126.163148679752,126.266203247961,126.369226456318,
126.472252298991,126.575385065769,126.678574157179,126.781946150561,126.852229145158,
126.973042559648),.UNSPECIFIED.);
#1948=B_SPLINE_CURVE_WITH_KNOTS('',3,(#189662,#189663,#189664,#189665,#189666,
#189667,#189668,#189669,#189670,#189671,#189672,#189673,#189674,#189675,
#189676,#189677,#189678,#189679,#189680,#189681,#189682,#189683,#189684,
#189685,#189686,#189687,#189688,#189689,#189690,#189691,#189692,#189693,
#189694,#189695,#189696,#189697,#189698,#189699,#189700,#189701,#189702,
#189703,#189704,#189705,#189706,#189707,#189708,#189709,#189710,#189711,
#189712,#189713,#189714,#189715,#189716,#189717,#189718,#189719,#189720,
#189721,#189722,#189723,#189724,#189725,#189726,#189727,#189728,#189729,
#189730,#189731,#189732,#189733,#189734,#189735,#189736,#189737,#189738,
#189739,#189740,#189741,#189742,#189743,#189744,#189745,#189746,#189747,
#189748,#189749,#189750,#189751,#189752,#189753,#189754,#189755,#189756,
#189757,#189758,#189759,#189760,#189761,#189762,#189763,#189764,#189765,
#189766,#189767,#189768,#189769,#189770,#189771,#189772,#189773,#189774,
#189775,#189776,#189777,#189778,#189779,#189780,#189781,#189782,#189783,
#189784,#189785,#189786,#189787,#189788,#189789,#189790,#189791,#189792,
#189793,#189794,#189795,#189796,#189797,#189798,#189799,#189800,#189801,
#189802,#189803,#189804,#189805,#189806,#189807,#189808,#189809,#189810,
#189811,#189812,#189813,#189814,#189815,#189816,#189817,#189818,#189819,
#189820,#189821,#189822,#189823,#189824,#189825,#189826,#189827,#189828,
#189829,#189830,#189831,#189832,#189833,#189834,#189835,#189836,#189837,
#189838,#189839,#189840,#189841,#189842,#189843,#189844,#189845,#189846,
#189847,#189848,#189849,#189850,#189851,#189852,#189853,#189854,#189855,
#189856,#189857,#189858,#189859,#189860,#189861,#189862,#189863,#189864,
#189865,#189866,#189867,#189868,#189869,#189870,#189871,#189872,#189873,
#189874,#189875,#189876,#189877,#189878,#189879),.UNSPECIFIED.,.F.,.F.,
(4,2,2,2,2,2,2,2,2,2,2,2,2,2,2,2,2,2,2,2,2,2,2,2,2,2,2,2,2,2,2,2,2,2,2,
2,2,2,2,2,2,2,2,2,2,2,2,2,2,2,2,2,2,2,2,2,2,2,2,2,2,2,2,2,2,2,2,2,2,2,2,
2,2,2,2,2,2,2,2,2,2,2,2,2,2,2,2,2,2,2,2,2,2,2,2,2,2,2,2,2,2,2,2,2,2,2,2,
2,4),(1.40832429865576,1.41583884495366,1.42010269900384,1.42263499019131,
1.42457441055375,1.42665176571331,1.42991807626368,1.44038113715901,1.45728208869256,
1.49511037488455,1.52518599045843,1.52810058168737,1.52948935833352,1.53056433495725,
1.53179245361094,1.53393537987583,1.5432315357883,1.56207807729296,1.60247855317451,
1.61474064742621,1.62934649342146,1.63313477184721,1.63534976156614,1.63726202080289,
1.63959705037182,1.64404697230231,1.67495966336917,1.72180621505924,1.73760405313658,
1.74021653802424,1.74156242286277,1.74263379219851,1.74389198196789,1.74617209712654,
1.75760866537589,1.78402402621373,1.83638785391721,1.84332628260559,1.84620035967748,
1.8479948190856,1.84995542820426,1.85265694773325,1.85904680520332,1.88738511825063,
1.93728516006437,1.94991466861279,1.95215090234824,1.95353452095267,1.95460902866221,
1.95584056691653,1.95799878037093,1.96750764192813,2.01664208994934,2.05182819066386,
2.0561245499724,2.05866631176982,2.06060731715934,2.0626808672741,2.06592968129853,
2.0762389137514,2.09279808800999,2.12568565054142,2.13955221159419,2.14611376194883,
2.16166407760683,2.16426452046228,2.1656077630128,2.16667891497163,2.16793904323441,
2.17022828823725,2.18182888435915,2.20890480585537,2.2603364903594,2.26733515714113,
2.27021909701194,2.27201528838317,2.27397425599951,2.27666707605165,2.2830062603409,
2.31092520737643,2.35694097730278,2.35794187149938,2.37366921516647,2.37627720144427,
2.37762207054712,2.37869331907723,2.37995216593099,2.38223551275641,2.39373092527518,
2.42038248370029,2.47238243700029,2.47936146681885,2.48224214585815,2.48403773500581,
2.48585833958336,2.48841277472039,2.49401322600401,2.50153647292751,2.52050598213682,
2.54851777748622,2.58534456122477,2.58818630672239,2.58956080069349,2.59063431748126,
2.59187161139157,2.5940563912719,2.60395325166763,2.65275138022529,2.66750909677174),
 .UNSPECIFIED.);
#1949=B_SPLINE_CURVE_WITH_KNOTS('',3,(#189880,#189881,#189882,#189883,#189884,
#189885,#189886,#189887,#189888,#189889,#189890,#189891,#189892,#189893,
#189894,#189895,#189896,#189897,#189898,#189899,#189900,#189901),
 .UNSPECIFIED.,.F.,.F.,(4,2,2,2,2,2,2,2,2,2,4),(0.000768647970570284,0.0217309695992682,
0.0248341065116262,0.0269704254049385,0.0287696705523692,0.0306848619291281,
0.0330687978124981,0.0367500452676532,0.0545887181713197,0.072975494517195,
0.0751664090908324),.UNSPECIFIED.);
#1950=B_SPLINE_CURVE_WITH_KNOTS('',3,(#189906,#189907,#189908,#189909,#189910,
#189911,#189912,#189913,#189914,#189915,#189916,#189917,#189918,#189919,
#189920,#189921,#189922,#189923,#189924,#189925,#189926,#189927,#189928,
#189929,#189930,#189931,#189932,#189933,#189934,#189935,#189936,#189937,
#189938,#189939,#189940,#189941,#189942,#189943,#189944,#189945,#189946,
#189947,#189948,#189949,#189950,#189951,#189952,#189953,#189954,#189955,
#189956,#189957,#189958,#189959,#189960,#189961,#189962,#189963,#189964,
#189965,#189966,#189967,#189968,#189969,#189970,#189971,#189972,#189973,
#189974,#189975,#189976,#189977,#189978,#189979,#189980,#189981,#189982,
#189983,#189984,#189985,#189986,#189987,#189988,#189989,#189990,#189991,
#189992,#189993,#189994,#189995,#189996,#189997,#189998,#189999,#190000,
#190001,#190002,#190003,#190004,#190005,#190006,#190007,#190008,#190009,
#190010,#190011,#190012,#190013,#190014,#190015,#190016,#190017,#190018,
#190019,#190020,#190021,#190022,#190023,#190024,#190025,#190026,#190027,
#190028,#190029,#190030,#190031,#190032,#190033,#190034,#190035,#190036,
#190037,#190038,#190039,#190040,#190041,#190042,#190043,#190044,#190045,
#190046,#190047,#190048,#190049,#190050,#190051,#190052,#190053,#190054,
#190055,#190056,#190057,#190058,#190059,#190060,#190061,#190062,#190063,
#190064,#190065,#190066,#190067,#190068,#190069,#190070,#190071,#190072,
#190073,#190074,#190075,#190076,#190077,#190078,#190079,#190080,#190081,
#190082,#190083,#190084,#190085,#190086,#190087,#190088,#190089,#190090,
#190091,#190092,#190093,#190094,#190095,#190096,#190097,#190098,#190099,
#190100,#190101,#190102,#190103,#190104,#190105,#190106,#190107,#190108,
#190109,#190110,#190111,#190112,#190113,#190114,#190115,#190116,#190117,
#190118,#190119,#190120,#190121,#190122,#190123,#190124,#190125,#190126,
#190127,#190128,#190129,#190130,#190131,#190132,#190133,#190134,#190135,
#190136,#190137,#190138,#190139,#190140,#190141,#190142,#190143),
 .UNSPECIFIED.,.F.,.F.,(4,2,2,2,2,2,2,2,2,2,2,2,2,2,2,2,2,2,2,2,2,2,2,2,
2,2,2,2,2,2,2,2,2,2,2,2,2,2,2,2,2,2,2,2,2,2,2,2,2,2,2,2,2,2,2,2,2,2,2,2,
2,2,2,2,2,2,2,2,2,2,2,2,2,2,2,2,2,2,2,2,2,2,2,2,2,2,2,2,2,2,2,2,2,2,2,2,
2,2,2,2,2,2,2,2,2,2,2,2,2,2,2,2,2,2,2,2,2,2,4),(1.25997183052399,1.27817567886033,
1.30767952852,1.31208995429294,1.31441688987609,1.31614398429107,1.31830042104015,
1.32192326049702,1.33437403324548,1.38533491188035,1.41654472381099,1.41945791182565,
1.42084657011798,1.42192170843108,1.42315029513985,1.42529470172456,1.43460753016451,
1.48376662632684,1.51915704870962,1.52345640857122,1.52599919825571,1.52794055843185,
1.530014070669,1.53326195531548,1.54356091300877,1.56009662248404,1.59296700102857,
1.60449381399583,1.6142450350421,1.61616610662091,1.62921742622787,1.63147548843054,
1.63286570439141,1.63394093797432,1.63516839264351,1.6373079222005,1.64655496320553,
1.66524609360828,1.70943437688544,1.73180205662411,1.73574128667566,1.73820443755014,
1.74012828189235,1.74225893361626,1.74576560970272,1.75856932078564,1.78108185957412,
1.82960357948144,1.84136212302166,1.84355430743698,1.84492468045176,1.84599801655695,
1.84723855163952,1.84943739922561,1.8595409327925,1.88103622391695,1.89337486426171,
1.93941064742755,1.94661835591445,1.94953755001237,1.95134045154839,1.95329471689711,
1.95595943690022,1.96213363241734,1.98870292006014,2.02808114368097,2.03941483875518,
2.05318730589606,2.05548100874553,2.05686696227646,2.05794439586525,2.05916040305897,
2.06124811942227,2.06981204916858,2.08643464813904,2.12835895507403,2.15549366223038,
2.15961898976107,2.16211095757247,2.16404430804365,2.1661398176675,2.16948765594565,
2.18069127297986,2.19928025092611,2.24261624307531,2.26472797766188,2.26756700696273,
2.26894112952305,2.2700148019016,2.27125277976661,2.2734399821749,2.28336833585192,
2.33215167780638,2.3672266941228,2.37152191997075,2.37406346338802,2.37600456246437,
2.37807846521967,2.38132835914815,2.39164546519976,2.4082215187391,2.47085804352185,
2.47221932342294,2.47838898108063,2.48032696053338,2.48150973046551,2.48254141104951,
2.48395478344332,2.48697107807225,2.49107129277855,2.50135666515076,2.52417539952219,
2.57588652624925,2.58287117880116,2.58575330931771,2.58754954685035,2.58950950137706,
2.59220538333982,2.59381054906569),.UNSPECIFIED.);
#1951=B_SPLINE_CURVE_WITH_KNOTS('',3,(#190144,#190145,#190146,#190147,#190148,
#190149,#190150,#190151,#190152,#190153,#190154,#190155,#190156,#190157,
#190158,#190159,#190160,#190161,#190162,#190163,#190164,#190165,#190166,
#190167,#190168,#190169,#190170,#190171,#190172,#190173,#190174,#190175,
#190176,#190177,#190178,#190179,#190180,#190181,#190182,#190183,#190184,
#190185,#190186,#190187,#190188,#190189,#190190,#190191,#190192,#190193,
#190194,#190195,#190196,#190197,#190198,#190199,#190200,#190201,#190202,
#190203,#190204,#190205,#190206,#190207,#190208,#190209,#190210,#190211,
#190212,#190213,#190214,#190215,#190216,#190217,#190218,#190219,#190220,
#190221,#190222,#190223,#190224,#190225,#190226,#190227,#190228,#190229,
#190230,#190231,#190232,#190233,#190234,#190235,#190236,#190237,#190238,
#190239,#190240,#190241,#190242,#190243,#190244,#190245,#190246,#190247,
#190248,#190249,#190250,#190251,#190252,#190253,#190254,#190255,#190256,
#190257,#190258,#190259,#190260,#190261,#190262,#190263,#190264,#190265,
#190266,#190267,#190268,#190269,#190270,#190271,#190272,#190273,#190274,
#190275,#190276,#190277,#190278,#190279,#190280,#190281,#190282,#190283,
#190284,#190285,#190286,#190287,#190288,#190289,#190290,#190291,#190292,
#190293,#190294,#190295,#190296,#190297,#190298,#190299,#190300,#190301,
#190302,#190303,#190304,#190305,#190306,#190307,#190308,#190309,#190310,
#190311,#190312,#190313,#190314,#190315,#190316,#190317,#190318,#190319,
#190320,#190321,#190322,#190323,#190324,#190325,#190326,#190327,#190328,
#190329,#190330,#190331,#190332,#190333,#190334,#190335,#190336,#190337,
#190338,#190339,#190340,#190341,#190342,#190343,#190344,#190345,#190346,
#190347,#190348,#190349,#190350,#190351,#190352,#190353,#190354,#190355,
#190356,#190357,#190358,#190359,#190360,#190361,#190362,#190363,#190364,
#190365,#190366,#190367,#190368,#190369,#190370,#190371,#190372,#190373,
#190374,#190375,#190376,#190377),.UNSPECIFIED.,.F.,.F.,(4,2,2,2,2,2,2,2,
2,2,2,2,2,2,2,2,2,2,2,2,2,2,2,2,2,2,2,2,2,2,2,2,2,2,2,2,2,2,2,2,2,2,2,2,
2,2,2,2,2,2,2,2,2,2,2,2,2,2,2,2,2,2,2,2,2,2,2,2,2,2,2,2,2,2,2,2,2,2,2,2,
2,2,2,2,2,2,2,2,2,2,2,2,2,2,2,2,2,2,2,2,2,2,2,2,2,2,2,2,2,2,2,2,2,2,2,2,
4),(0.0751664090908324,0.121837060794992,0.131681154580003,0.133862218936931,
0.135098609348292,0.136172112973235,0.137547586555477,0.14039478308759,
0.176867593743613,0.209428589603404,0.225633494276976,0.232378372999333,
0.237517835267561,0.239980362266982,0.24182160906685,0.243648984947873,
0.24619358731576,0.252852041300881,0.308507478827018,0.332697662164898,
0.343554696200585,0.345800715641859,0.347051391175338,0.348123294323277,
0.349478720652284,0.351622253527715,0.362626804254524,0.413891793790983,
0.442557477613195,0.448986593123129,0.451694562979244,0.453656168813981,
0.455449007921287,0.45831496133963,0.465205183335653,0.51824131493154,0.544208668875459,
0.555530763501977,0.557804197079648,0.559060850781458,0.560132220078928,
0.561479763280902,0.564100338996175,0.580124041799767,0.585198357313938,
0.62988200363044,0.648403689166925,0.659578942020468,0.662923333421311,
0.665017817799912,0.666950992464238,0.669443811657874,0.673572910091847,
0.700868879448593,0.743120553968538,0.759406863082676,0.767853959244599,
0.769932121744742,0.771145872170893,0.772223552155801,0.773612714392369,
0.775917733466,0.789930520496486,0.791300161058096,0.798313730845986,0.81198834179328,
0.844849354606316,0.861410892866797,0.871722138504353,0.874971110813799,
0.877044653944802,0.878985577468383,0.881527124593694,0.885822912254324,
0.920955318573848,0.969901902909867,0.979660706696958,0.981836311782615,
0.983071678036541,0.984145617251088,0.985523380514225,0.988381267646278,
1.01124168745723,1.0240066975221,1.05686244976068,1.07341519163896,1.08372275748767,
1.08697152690445,1.08904517046851,1.09098634953222,1.09352846436847,1.09782573412167,
1.13304047776493,1.18224589602785,1.19170985580366,1.19386507805123,1.1950960392592,
1.19617078041621,1.19755565845216,1.19979579758883,1.21249724423315,1.23487538868016,
1.26847905280066,1.29385628229564,1.29812698963818,1.30042452392246,1.30231759679482,
1.30455834273101,1.30845750771934,1.32436621245914,1.3345884709149,1.37387287164785,
1.40245709083406,1.40536964828917,1.40675819973767,1.40783334453758,1.40876522934455),
 .UNSPECIFIED.);
#1952=B_SPLINE_CURVE_WITH_KNOTS('',3,(#190383,#190384,#190385,#190386,#190387,
#190388,#190389,#190390,#190391,#190392,#190393,#190394,#190395,#190396,
#190397,#190398,#190399,#190400,#190401,#190402,#190403,#190404),
 .UNSPECIFIED.,.F.,.F.,(4,2,2,2,2,2,2,2,2,2,4),(2.59301342310063,2.59652018861172,
2.60119783305151,2.60293253192801,2.60395677895129,2.60504993697695,2.60656487605862,
2.61017450132261,2.61524686047379,2.62925650837804,2.66711449156562),
 .UNSPECIFIED.);
#1953=B_SPLINE_CURVE_WITH_KNOTS('',3,(#190405,#190406,#190407,#190408,#190409,
#190410,#190411,#190412,#190413,#190414,#190415,#190416,#190417,#190418,
#190419,#190420,#190421,#190422,#190423,#190424,#190425,#190426,#190427,
#190428,#190429,#190430,#190431,#190432,#190433,#190434,#190435,#190436,
#190437,#190438,#190439,#190440,#190441,#190442,#190443,#190444,#190445,
#190446,#190447,#190448,#190449,#190450,#190451,#190452,#190453,#190454,
#190455,#190456,#190457,#190458,#190459,#190460,#190461,#190462,#190463,
#190464,#190465,#190466,#190467,#190468,#190469,#190470,#190471,#190472,
#190473,#190474,#190475,#190476,#190477,#190478,#190479,#190480,#190481,
#190482,#190483,#190484,#190485,#190486,#190487,#190488,#190489,#190490,
#190491,#190492,#190493,#190494,#190495,#190496,#190497,#190498,#190499,
#190500,#190501,#190502,#190503,#190504,#190505,#190506,#190507,#190508,
#190509,#190510,#190511,#190512,#190513,#190514,#190515,#190516,#190517,
#190518,#190519,#190520,#190521,#190522,#190523,#190524,#190525,#190526,
#190527,#190528,#190529,#190530,#190531,#190532,#190533,#190534,#190535,
#190536,#190537,#190538,#190539,#190540,#190541,#190542,#190543,#190544,
#190545,#190546,#190547,#190548,#190549,#190550,#190551,#190552,#190553,
#190554,#190555,#190556,#190557,#190558,#190559,#190560,#190561,#190562,
#190563,#190564,#190565,#190566,#190567,#190568,#190569,#190570,#190571,
#190572,#190573,#190574,#190575,#190576,#190577,#190578,#190579,#190580,
#190581,#190582,#190583,#190584,#190585,#190586,#190587,#190588,#190589,
#190590,#190591,#190592,#190593,#190594,#190595,#190596,#190597,#190598,
#190599,#190600,#190601,#190602,#190603,#190604,#190605,#190606,#190607,
#190608,#190609,#190610,#190611,#190612,#190613,#190614,#190615,#190616,
#190617,#190618,#190619,#190620,#190621,#190622,#190623,#190624,#190625,
#190626,#190627,#190628,#190629,#190630,#190631,#190632),.UNSPECIFIED.,
 .F.,.F.,(4,2,2,2,2,2,2,2,2,2,2,2,2,2,2,2,2,2,2,2,2,2,2,2,2,2,2,2,2,2,2,
2,2,2,2,2,2,2,2,2,2,2,2,2,2,2,2,2,2,2,2,2,2,2,2,2,2,2,2,2,2,2,2,2,2,2,2,
2,2,2,2,2,2,2,2,2,2,2,2,2,2,2,2,2,2,2,2,2,2,2,2,2,2,2,2,2,2,2,2,2,2,2,2,
2,2,2,2,2,2,2,2,2,2,4),(0.00070417365456507,0.0257174857516651,0.0359847480784371,
0.0390635037060503,0.0411898132628437,0.0432709727765218,0.0452083303494675,
0.047729912948974,0.0519580123236602,0.0833470854812081,0.108660532403853,
0.136506496715738,0.145896845031396,0.148046207237502,0.149275561060278,
0.150350028422841,0.151736041141806,0.153980938539433,0.166786704522338,
0.188793015005292,0.215577358353407,0.23704354853604,0.245226816600629,
0.251216700447995,0.253840413141923,0.255796348256697,0.257595616110479,
0.260497421472034,0.267604938409068,0.317187172083802,0.355583624564653,
0.35916926711615,0.360680067198888,0.361772446643604,0.362797722533406,
0.364537908087725,0.369252155315286,0.409787642162989,0.456725506184692,
0.463118884531493,0.465820692809186,0.467781076220977,0.469575032644453,
0.472447645198868,0.479379118298607,0.531842815258053,0.558206612602061,
0.569628710827241,0.571907734651659,0.573165546103371,0.574236732239752,
0.575582557494768,0.578195428008421,0.59405582464407,0.598862688444337,
0.614071685277517,0.646946957225565,0.663527873732877,0.673847616726631,
0.67709736954593,0.679170955349841,0.681111598982654,0.683652318260893,
0.687945672940657,0.730339605970443,0.759384712515066,0.774118772814738,
0.782015001040382,0.784047244550115,0.785250749405223,0.786330812000847,
0.787738083619861,0.790105073647513,0.805531936840359,0.812269412497604,
0.826058617288149,0.858919141486843,0.875481262202823,0.885792628402886,
0.88904150998083,0.891114964285735,0.893055782947641,0.895597161431638,
0.8998925938382,0.935012840958341,0.983925279081658,0.993721128804179,0.995899188165928,
0.997135055486108,0.998208859356632,0.999585703072175,1.00243911823943,
1.02512457408904,1.03806473222202,1.07092042002931,1.08747426149498,1.09778218132457,
1.10103088630441,1.1031044464417,1.10504551769378,1.10758744846606,1.1118843109584,
1.14708264797785,1.19623652119962,1.20575655406218,1.20791566285735,1.20914744164461,
1.21022198959788,1.21160542700361,1.21384090211796,1.22645486852707,1.23298050298514,
1.23811264297844,1.25997183052399),.UNSPECIFIED.);
#1954=B_SPLINE_CURVE_WITH_KNOTS('',3,(#190634,#190635,#190636,#190637,#190638,
#190639,#190640,#190641,#190642,#190643,#190644,#190645,#190646,#190647,
#190648,#190649,#190650,#190651,#190652,#190653,#190654,#190655,#190656,
#190657,#190658,#190659,#190660,#190661,#190662,#190663,#190664,#190665,
#190666,#190667,#190668,#190669,#190670,#190671,#190672,#190673,#190674,
#190675,#190676,#190677,#190678,#190679,#190680,#190681,#190682,#190683,
#190684,#190685,#190686,#190687,#190688,#190689,#190690,#190691,#190692,
#190693,#190694,#190695,#190696,#190697,#190698,#190699,#190700,#190701,
#190702,#190703,#190704,#190705,#190706,#190707,#190708,#190709,#190710,
#190711,#190712,#190713,#190714,#190715,#190716,#190717,#190718,#190719,
#190720,#190721,#190722,#190723,#190724,#190725,#190726,#190727,#190728,
#190729,#190730,#190731,#190732,#190733,#190734,#190735,#190736,#190737,
#190738,#190739,#190740,#190741,#190742,#190743,#190744,#190745,#190746,
#190747,#190748,#190749,#190750,#190751,#190752,#190753,#190754,#190755,
#190756,#190757,#190758,#190759,#190760,#190761,#190762,#190763,#190764,
#190765,#190766,#190767,#190768,#190769,#190770,#190771,#190772,#190773,
#190774,#190775,#190776,#190777,#190778,#190779,#190780,#190781,#190782,
#190783,#190784,#190785,#190786,#190787,#190788,#190789,#190790,#190791,
#190792,#190793,#190794,#190795,#190796,#190797,#190798,#190799,#190800,
#190801,#190802,#190803,#190804,#190805,#190806,#190807,#190808,#190809,
#190810,#190811,#190812,#190813,#190814,#190815,#190816,#190817,#190818,
#190819,#190820,#190821,#190822,#190823,#190824,#190825,#190826,#190827,
#190828,#190829,#190830,#190831,#190832,#190833,#190834,#190835,#190836,
#190837,#190838,#190839,#190840,#190841,#190842,#190843,#190844,#190845,
#190846,#190847,#190848,#190849,#190850,#190851,#190852,#190853,#190854,
#190855,#190856,#190857,#190858,#190859,#190860,#190861,#190862,#190863),
 .UNSPECIFIED.,.F.,.F.,(4,2,2,2,2,2,2,2,2,2,2,2,2,2,2,2,2,2,2,2,2,2,2,2,
2,2,2,2,2,2,2,2,2,2,2,2,2,2,2,2,2,2,2,2,2,2,2,2,2,2,2,2,2,2,2,2,2,2,2,2,
2,2,2,2,2,2,2,2,2,2,2,2,2,2,2,2,2,2,2,2,2,2,2,2,2,2,2,2,2,2,2,2,2,2,2,2,
2,2,2,2,2,2,2,2,2,2,2,2,2,2,2,2,2,2,4),(1.40876522934455,1.40906203844239,
1.41120686592205,1.42052513857405,1.46970161231669,1.50507080576657,1.50936998566118,
1.51191274775594,1.51385413225212,1.51592771444487,1.51917580043562,1.52947616880855,
1.54601487666193,1.57356167837748,1.58970409347244,1.600784706932,1.61502053685379,
1.61733716480446,1.6187298518975,1.61980813026777,1.62102017469625,1.62309008558368,
1.63143247862436,1.64741379441942,1.68972807553654,1.71734565740105,1.72148337964582,
1.72397896862389,1.72591283649619,1.72800661944552,1.73134674439907,1.74247829120265,
1.76089970967477,1.80770742523714,1.81252956966111,1.82701168344094,1.82934218372271,
1.83073895560801,1.83181778964995,1.83302754926357,1.83508710443475,1.84330297118474,
1.85892394604438,1.90067235665691,1.92931450646513,1.93347935906925,1.93598293615531,
1.93791805149379,1.94000827353765,1.94333213529409,1.95431205570459,1.97238290730774,
2.02252301941893,2.0389114593475,2.04154695669813,2.04289790616715,2.04396974959826,
2.04522438244351,2.04748762883996,2.05862750092203,2.08387991806958,2.13793358711759,
2.14474145305826,2.14759426382349,2.14938504870012,2.15134939482114,2.15407032808689,
2.16057405870037,2.18986706413482,2.23045248167066,2.25076712538338,2.25356035354298,
2.25492541685537,2.25599829628312,2.25724252614575,2.25945823948905,2.26982198919262,
2.2922207410463,2.35066402619404,2.35700471302507,2.35949796515481,2.36131215931685,
2.36325837857622,2.36587642437814,2.37178639337514,2.39627727351485,2.44388131991961,
2.46288674951732,2.46565098712122,2.46701024350062,2.46805186727489,2.46805591400501,
2.46805989278188,2.4680638049572,2.46806765199019,2.46807124430431,2.46807482310213,
2.46807838865476,2.46808194093323,2.46930494281057,2.47061534797828,2.47263693893703,
2.47644584213214,2.48570633250583,2.52347010312493,2.5337534772937,2.56534492805526,
2.56957833020121,2.57210195237765,2.57404021221258,2.57612168825699,2.57940580955971,
2.59002433475977,2.60727269931124,2.6683774093147),.UNSPECIFIED.);
#1955=B_SPLINE_CURVE_WITH_KNOTS('',3,(#190864,#190865,#190866,#190867,#190868,
#190869,#190870,#190871,#190872,#190873,#190874,#190875,#190876,#190877,
#190878,#190879,#190880,#190881,#190882,#190883,#190884,#190885,#190886,
#190887),.UNSPECIFIED.,.F.,.F.,(4,2,2,2,2,2,2,2,2,2,2,4),(0.000810717560574591,
0.00554260829355552,0.00881068920855145,0.010244569293212,0.0113189780628067,
0.0123417944517917,0.0133649961849808,0.0148060120350927,0.0186526100510774,
0.0263910001425551,0.0473308873917541,0.0750288866695304),.UNSPECIFIED.);
#1956=B_SPLINE_CURVE_WITH_KNOTS('',3,(#190892,#190893,#190894,#190895,#190896,
#190897,#190898,#190899,#190900,#190901,#190902,#190903,#190904,#190905,
#190906,#190907,#190908,#190909,#190910,#190911,#190912,#190913,#190914,
#190915,#190916,#190917,#190918,#190919,#190920,#190921,#190922,#190923,
#190924,#190925,#190926,#190927,#190928,#190929,#190930,#190931,#190932,
#190933,#190934,#190935,#190936,#190937,#190938,#190939,#190940,#190941,
#190942,#190943,#190944,#190945,#190946,#190947,#190948,#190949,#190950,
#190951,#190952,#190953,#190954,#190955,#190956,#190957,#190958,#190959,
#190960,#190961,#190962,#190963,#190964,#190965,#190966,#190967,#190968,
#190969,#190970,#190971,#190972,#190973,#190974,#190975,#190976,#190977,
#190978,#190979,#190980,#190981,#190982,#190983,#190984,#190985,#190986,
#190987,#190988,#190989,#190990,#190991,#190992,#190993,#190994,#190995,
#190996,#190997,#190998,#190999,#191000,#191001,#191002,#191003,#191004,
#191005,#191006,#191007,#191008,#191009,#191010,#191011,#191012,#191013,
#191014,#191015,#191016,#191017,#191018,#191019,#191020,#191021,#191022,
#191023,#191024,#191025,#191026,#191027,#191028,#191029,#191030,#191031,
#191032,#191033,#191034,#191035,#191036,#191037,#191038,#191039,#191040,
#191041,#191042,#191043,#191044,#191045,#191046,#191047,#191048,#191049,
#191050,#191051,#191052,#191053,#191054,#191055,#191056,#191057,#191058,
#191059,#191060,#191061,#191062,#191063,#191064,#191065,#191066,#191067,
#191068,#191069,#191070,#191071,#191072,#191073,#191074,#191075,#191076,
#191077,#191078,#191079,#191080,#191081,#191082,#191083,#191084,#191085,
#191086,#191087,#191088,#191089,#191090,#191091,#191092,#191093,#191094,
#191095,#191096,#191097,#191098,#191099,#191100,#191101,#191102,#191103,
#191104,#191105,#191106,#191107,#191108,#191109,#191110,#191111,#191112,
#191113,#191114,#191115,#191116,#191117,#191118,#191119,#191120,#191121,
#191122,#191123,#191124,#191125,#191126,#191127),.UNSPECIFIED.,.F.,.F.,
(4,2,2,2,2,2,2,2,2,2,2,2,2,2,2,2,2,2,2,2,2,2,2,2,2,2,2,2,2,2,2,2,2,2,2,
2,2,2,2,2,2,2,2,2,2,2,2,2,2,2,2,2,2,2,2,2,2,2,2,2,2,2,2,2,2,2,2,2,2,2,2,
2,2,2,2,2,2,2,2,2,2,2,2,2,2,2,2,2,2,2,2,2,2,2,2,2,2,2,2,2,2,2,2,2,2,2,2,
2,2,2,2,2,2,2,2,2,2,4),(1.25961098705092,1.26429589096183,1.30523587040568,
1.32771330738116,1.3303764594605,1.33171516128731,1.33268303899733,1.33390652731652,
1.33602883137143,1.34504661564238,1.36302990581967,1.4132405423344,1.43104246885246,
1.43472154572487,1.43710492851623,1.43902022329457,1.44119876054537,1.44492321875558,
1.46032818122401,1.51165837432783,1.53933387157848,1.54224052694126,1.54362769569379,
1.5447024298606,1.54593139333262,1.54807842483266,1.55743318582157,1.60669366318553,
1.64191346431821,1.64620969238522,1.6487512269324,1.65069197264094,1.65276516183558,
1.65601323605462,1.66631865223905,1.68287030021161,1.7157488117304,1.72919468933446,
1.73677775908984,1.75177426042052,1.75412354904193,1.75552560648424,1.75660488848266,
1.7578111116667,1.7598557678916,1.76789843774536,1.78303562077719,1.82273162969494,
1.85396941562139,1.85819439583057,1.86071517094643,1.86265251122501,1.86473424315566,
1.86802140340636,1.878672876719,1.89599752699931,1.94418960827059,1.94848458820401,
1.95083866934147,1.96390018632466,1.96615838982003,1.96754848096143,1.96862348349695,
1.9698505241838,1.9719889813816,1.98122602067255,1.99988824328324,2.04403206465749,
2.06645691093807,2.07039789313005,2.07286127560859,2.07478476557204,2.07691447785506,
2.08041834899328,2.09319772888885,2.11565000635428,2.15606158561172,2.16038645969957,
2.16186163765369,2.17577409847162,2.17807413266991,2.17946175981933,2.18053916068743,
2.18175363234102,2.18383533974423,2.1923284498817,2.20874672700626,2.25239703387108,
2.26464294689534,2.2793373993013,2.28313315344194,2.28534967396721,2.28726154038849,
2.28959393805035,2.29403223713569,2.32453851236181,2.36816434175097,2.37249180629,
2.37697490893965,2.38801865868004,2.39016459163177,2.39152071783719,2.39259263339461,
2.39384270772542,2.39608609885265,2.40690117302882,2.43093356853466,2.47256911358986,
2.49080658172696,2.49451338717382,2.49690533514595,2.49882139043036,2.500620088583,
2.50374313045043,2.51354125425459,2.5290804575828,2.55074369450569,2.59301342310063),
 .UNSPECIFIED.);
#1957=B_SPLINE_CURVE_WITH_KNOTS('',3,(#191128,#191129,#191130,#191131,#191132,
#191133,#191134,#191135,#191136,#191137,#191138,#191139,#191140,#191141,
#191142,#191143,#191144,#191145,#191146,#191147,#191148,#191149,#191150,
#191151,#191152,#191153,#191154,#191155,#191156,#191157,#191158,#191159,
#191160,#191161,#191162,#191163,#191164,#191165,#191166,#191167,#191168,
#191169,#191170,#191171,#191172,#191173,#191174,#191175,#191176,#191177,
#191178,#191179,#191180,#191181,#191182,#191183,#191184,#191185,#191186,
#191187,#191188,#191189,#191190,#191191,#191192,#191193,#191194,#191195,
#191196,#191197,#191198,#191199,#191200,#191201,#191202,#191203,#191204,
#191205,#191206,#191207,#191208,#191209,#191210,#191211,#191212,#191213,
#191214,#191215,#191216,#191217,#191218,#191219,#191220,#191221,#191222,
#191223,#191224,#191225,#191226,#191227,#191228,#191229,#191230,#191231,
#191232,#191233,#191234,#191235,#191236,#191237,#191238,#191239,#191240,
#191241,#191242,#191243,#191244,#191245,#191246,#191247,#191248,#191249,
#191250,#191251,#191252,#191253,#191254,#191255,#191256,#191257,#191258,
#191259,#191260,#191261,#191262,#191263,#191264,#191265,#191266,#191267,
#191268,#191269,#191270,#191271,#191272,#191273,#191274,#191275,#191276,
#191277,#191278,#191279,#191280,#191281,#191282,#191283,#191284,#191285,
#191286,#191287,#191288,#191289,#191290,#191291,#191292,#191293,#191294,
#191295,#191296,#191297,#191298,#191299,#191300,#191301,#191302,#191303,
#191304,#191305,#191306,#191307,#191308,#191309,#191310,#191311,#191312,
#191313,#191314,#191315,#191316,#191317,#191318,#191319,#191320,#191321,
#191322,#191323,#191324,#191325,#191326,#191327,#191328,#191329,#191330,
#191331,#191332,#191333,#191334,#191335,#191336,#191337,#191338,#191339,
#191340,#191341,#191342,#191343,#191344,#191345,#191346,#191347,#191348,
#191349,#191350,#191351,#191352,#191353,#191354,#191355,#191356,#191357,
#191358,#191359,#191360,#191361),.UNSPECIFIED.,.F.,.F.,(4,2,2,2,2,2,2,2,
2,2,2,2,2,2,2,2,2,2,2,2,2,2,2,2,2,2,2,2,2,2,2,2,2,2,2,2,2,2,2,2,2,2,2,2,
2,2,2,2,2,2,2,2,2,2,2,2,2,2,2,2,2,2,2,2,2,2,2,2,2,2,2,2,2,2,2,2,2,2,2,2,
2,2,2,2,2,2,2,2,2,2,2,2,2,2,2,2,2,2,2,2,2,2,2,2,2,2,2,2,2,2,2,2,2,2,2,2,
4),(0.0750288866695304,0.0988476388128419,0.111888896017187,0.115416384720813,
0.117551062967879,0.119473010908271,0.121926095772893,0.125833939336574,
0.147507513631184,0.207360988300454,0.215841413740865,0.219420342090852,
0.22135444545707,0.222628435301558,0.223822876379554,0.22486635864107,0.226245269920354,
0.22911009984437,0.264693456090149,0.297552629213783,0.320303169519504,
0.325982681899396,0.328558619925288,0.330497701947557,0.332322887219393,
0.334859323854595,0.341466097082073,0.397637306257989,0.421485895038357,
0.432250515347694,0.434490879017361,0.435740299795249,0.436812297051355,
0.438169343668719,0.440834379545483,0.458016218533738,0.507006516340784,
0.525230085590314,0.536276560196135,0.539607032913761,0.541698357521891,
0.543632406986323,0.546131673348657,0.550283003557895,0.578438583117287,
0.620515650582936,0.636279916483226,0.644544869789676,0.646608143657294,
0.647818540634769,0.648896890235033,0.650291652681477,0.652615888696389,
0.667025439902318,0.675569301872245,0.688665470740753,0.72151875655042,
0.744257070647802,0.749935208688195,0.75251105545168,0.754450284425893,
0.756275766114474,0.758812867790212,0.76542285705599,0.821575709471048,
0.845442611629954,0.856212653187838,0.858453513296996,0.859703121951681,
0.860775225443443,0.862132335981215,0.864797285493635,0.881970973850752,
0.92747365336257,0.955334410640888,0.961667095567586,0.964358854716377,
0.966317678344622,0.96811417670787,0.9709995618696,0.978006588705994,1.02934961057856,
1.05652184770716,1.06814571862572,1.07043634817434,1.07169680274305,1.0727679731605,
1.07411090498551,1.07670977558034,1.09222289794396,1.09879767692896,1.14018127845367,
1.16744975409078,1.17371040001649,1.17638989112832,1.17834659733112,1.18014589609658,
1.1830462493864,1.19014267214712,1.23977806686569,1.27816003863628,1.28174636449284,
1.28325749256897,1.28435012413588,1.28537564856719,1.28711628136227,1.29183188796299,
1.33224679737648,1.3341364500098,1.37796729601687,1.38519019214418,1.38811181430934,
1.38991506778615,1.39186881359856,1.39453121204554,1.40069275473419,1.40863554629314),
 .UNSPECIFIED.);
#1958=B_SPLINE_CURVE_WITH_KNOTS('',3,(#191367,#191368,#191369,#191370),
 .UNSPECIFIED.,.F.,.F.,(4,4),(152.105783788367,152.455231345441),
 .UNSPECIFIED.);
#1959=B_SPLINE_CURVE_WITH_KNOTS('',3,(#191371,#191372,#191373,#191374,#191375,
#191376,#191377,#191378,#191379,#191380,#191381,#191382,#191383,#191384,
#191385,#191386,#191387,#191388,#191389,#191390,#191391,#191392,#191393,
#191394,#191395,#191396,#191397,#191398,#191399,#191400,#191401,#191402,
#191403,#191404,#191405,#191406,#191407,#191408,#191409,#191410,#191411,
#191412,#191413,#191414,#191415,#191416,#191417,#191418,#191419,#191420,
#191421,#191422,#191423,#191424,#191425,#191426,#191427,#191428,#191429,
#191430,#191431,#191432,#191433,#191434,#191435,#191436,#191437,#191438,
#191439,#191440,#191441,#191442,#191443,#191444,#191445,#191446,#191447,
#191448,#191449,#191450,#191451,#191452,#191453,#191454,#191455,#191456,
#191457,#191458,#191459,#191460,#191461,#191462,#191463,#191464,#191465,
#191466,#191467,#191468,#191469,#191470,#191471,#191472,#191473,#191474,
#191475,#191476,#191477,#191478,#191479,#191480,#191481,#191482,#191483,
#191484,#191485,#191486,#191487,#191488,#191489,#191490,#191491,#191492,
#191493,#191494,#191495,#191496,#191497,#191498,#191499,#191500,#191501,
#191502,#191503,#191504,#191505,#191506,#191507,#191508,#191509,#191510,
#191511,#191512,#191513,#191514,#191515,#191516,#191517,#191518,#191519,
#191520,#191521,#191522,#191523,#191524,#191525,#191526,#191527,#191528,
#191529,#191530,#191531,#191532,#191533,#191534,#191535,#191536,#191537,
#191538,#191539,#191540,#191541,#191542,#191543,#191544,#191545,#191546,
#191547,#191548,#191549,#191550,#191551,#191552,#191553,#191554,#191555,
#191556,#191557,#191558,#191559,#191560,#191561,#191562,#191563,#191564,
#191565,#191566,#191567,#191568,#191569,#191570,#191571,#191572,#191573,
#191574,#191575,#191576,#191577,#191578,#191579,#191580,#191581,#191582,
#191583,#191584,#191585,#191586,#191587,#191588),.UNSPECIFIED.,.F.,.F.,
(4,2,2,2,2,2,2,2,2,2,2,2,2,2,2,2,2,2,2,2,2,2,2,2,2,2,2,2,2,2,2,2,2,2,2,
2,2,2,2,2,2,2,2,2,2,2,2,2,2,2,2,2,2,2,2,2,2,2,2,2,2,2,2,2,2,2,2,2,2,2,2,
2,2,2,2,2,2,2,2,2,2,2,2,2,2,2,2,2,2,2,2,2,2,2,2,2,2,2,2,2,2,2,2,2,2,2,2,
2,4),(0.000629330332896467,0.0481836283120002,0.0539124780237477,0.05787733475668,
0.0594504871787808,0.0605543059052947,0.0615643737818521,0.0632261135679029,
0.0674397512461144,0.117074899313782,0.145099746889406,0.159868702049087,
0.163472396047961,0.165305888284628,0.167218128087233,0.169427168350128,
0.173190872934244,0.187528077164309,0.194033219199103,0.231119072317868,
0.257108362976473,0.268435364721626,0.270708846750274,0.271965401439233,
0.273036609959852,0.274383853772958,0.277003561627561,0.293016737546607,
0.298054532289369,0.342300494321789,0.361132349055645,0.368618138341636,
0.374241455022956,0.376807011926189,0.378744445959156,0.380572619411744,
0.383120504417729,0.389800695683808,0.445225322817334,0.469564715247018,
0.480461488353643,0.482709803765115,0.483960932279112,0.485032715746576,
0.486387339952193,0.489041178184703,0.505923813355234,0.551390667602991,
0.582460329300252,0.586913729254806,0.589249257675527,0.591161254183334,
0.59337518483369,0.597159812813965,0.611728909326192,0.624007001074787,
0.664457786380243,0.683309566177892,0.692606095844698,0.69474884985209,
0.695976816916883,0.697051631759554,0.698440150294487,0.701354043952059,
0.731367395207987,0.782632281234815,0.791458724027022,0.79786005323276,
0.800563206648733,0.802523831735161,0.804317502987526,0.807188554083247,
0.814110550750721,0.86671263000008,0.892978558835595,0.904375992282532,
0.90665361251085,0.907911118757985,0.908982329221137,0.910328546421638,
0.912943237382301,0.928861144804925,0.929632069519631,0.973925248757589,
1.00329166350919,1.00980364292021,1.01252549468196,1.01448959719813,1.01627954387186,
1.01912967772102,1.02592428305164,1.0801280585937,1.10528993829633,1.1164042778108,
1.11866560919824,1.1199196132617,1.1209911875743,1.12234213348133,1.12497862061388,
1.14140772532225,1.19199097466867,1.20970069163456,1.22052321544298,1.22382937322598,
1.22591534971842,1.2278512719421,1.23036259075949,1.23455502155928,1.25961098705092),
 .UNSPECIFIED.);
#1960=B_SPLINE_CURVE_WITH_KNOTS('',3,(#191590,#191591,#191592,#191593,#191594,
#191595,#191596,#191597,#191598,#191599,#191600,#191601,#191602,#191603,
#191604,#191605,#191606,#191607,#191608,#191609,#191610,#191611,#191612,
#191613,#191614,#191615,#191616,#191617,#191618,#191619,#191620,#191621,
#191622,#191623,#191624,#191625,#191626,#191627,#191628,#191629,#191630,
#191631,#191632,#191633,#191634,#191635,#191636,#191637,#191638,#191639,
#191640,#191641,#191642,#191643,#191644,#191645,#191646,#191647,#191648,
#191649,#191650,#191651,#191652,#191653,#191654,#191655,#191656,#191657,
#191658,#191659,#191660,#191661,#191662,#191663,#191664,#191665,#191666,
#191667,#191668,#191669,#191670,#191671,#191672,#191673,#191674,#191675,
#191676,#191677,#191678,#191679,#191680,#191681,#191682,#191683,#191684,
#191685,#191686,#191687,#191688,#191689,#191690,#191691,#191692,#191693,
#191694,#191695,#191696,#191697,#191698,#191699,#191700,#191701,#191702,
#191703,#191704,#191705,#191706,#191707,#191708,#191709,#191710,#191711,
#191712,#191713,#191714,#191715,#191716,#191717,#191718,#191719,#191720,
#191721,#191722,#191723,#191724,#191725,#191726,#191727,#191728,#191729,
#191730,#191731,#191732,#191733,#191734,#191735,#191736,#191737,#191738,
#191739,#191740,#191741,#191742,#191743,#191744,#191745,#191746,#191747,
#191748,#191749,#191750,#191751,#191752,#191753,#191754,#191755,#191756,
#191757,#191758,#191759,#191760,#191761,#191762,#191763,#191764,#191765,
#191766,#191767,#191768,#191769,#191770,#191771,#191772,#191773,#191774,
#191775,#191776,#191777,#191778,#191779,#191780,#191781,#191782,#191783,
#191784,#191785,#191786,#191787,#191788,#191789,#191790,#191791,#191792,
#191793,#191794,#191795,#191796,#191797,#191798,#191799,#191800,#191801,
#191802,#191803,#191804,#191805,#191806,#191807,#191808,#191809),
 .UNSPECIFIED.,.F.,.F.,(4,2,2,2,2,2,2,2,2,2,2,2,2,2,2,2,2,2,2,2,2,2,2,2,
2,2,2,2,2,2,2,2,2,2,2,2,2,2,2,2,2,2,2,2,2,2,2,2,2,2,2,2,2,2,2,2,2,2,2,2,
2,2,2,2,2,2,2,2,2,2,2,2,2,2,2,2,2,2,2,2,2,2,2,2,2,2,2,2,2,2,2,2,2,2,2,2,
2,2,2,2,2,2,2,2,2,2,2,2,2,4),(1.40863554629314,1.42716215159709,1.46608335485054,
1.4742262937387,1.49150273493638,1.49417163629359,1.49552963938261,1.49660186907406,
1.49785096673155,1.50008926127109,1.51081615469342,1.53452084178693,1.56189720077975,
1.59383344740408,1.59807355130827,1.60059904422423,1.60253750501244,1.60461798644391,
1.60789797868523,1.61848080760563,1.6356493146767,1.68138674762876,1.68817256117372,
1.70360944883121,1.7059772390797,1.70738488073162,1.70846516546746,1.70966886176828,
1.71170129041267,1.71959671810318,1.73432520447475,1.76335930174742,1.80574607868969,
1.81003972128601,1.81258079153819,1.81452179636653,1.81659585752303,1.81984654089242,
1.83017072034651,1.84676248796964,1.8796785532681,1.89569119122154,1.89935457602018,
1.91554186909053,1.9181691129569,1.9195181936139,1.92058979219937,1.9218455709776,
1.92411450987405,1.93535545373384,1.96100072805648,2.01447068945007,2.02132576778302,
2.02418616726865,2.02597816979551,2.02794099109555,2.03065454626968,2.03711548181607,
2.09104317996443,2.12731082282962,2.13016509347575,2.1315421696298,2.13261606659975,
2.13385194986308,2.1360298053932,2.14582124223785,2.19471609134631,2.22983738282057,
2.23412739389796,2.23666735477647,2.23860811162243,2.24068248949139,2.24393488508621,
2.25427477893621,2.27090160239157,2.30384594427632,2.32163773658148,2.3395210915158,
2.34221127405255,2.34357378887543,2.34464634307932,2.3458921140461,2.3481152904112,
2.35859967555724,2.38142776393167,2.41099672670033,2.44190937607125,2.44650855264558,
2.44892542349954,2.45079410007683,2.4528901947448,2.45508756247662,2.4583380477175,
2.49660981719125,2.53859758144543,2.55185006429499,2.55411817912451,2.55549653647139,
2.55657299018092,2.55779346303841,2.55990153224842,2.56872789661443,2.58612906951568,
2.64880086677163,2.65696471589238,2.66003632479818,2.66186784621627,2.66371202387013,
2.66600413821752,2.66806871862646),.UNSPECIFIED.);
#1961=B_SPLINE_CURVE_WITH_KNOTS('',3,(#191810,#191811,#191812,#191813,#191814,
#191815,#191816,#191817,#191818,#191819),.UNSPECIFIED.,.F.,.F.,(4,2,2,2,
4),(0.000823833599433129,0.00391834426972108,0.0101607531916337,0.0637296745559499,
0.07512477121657),.UNSPECIFIED.);
#1962=B_SPLINE_CURVE_WITH_KNOTS('',3,(#191825,#191826,#191827,#191828,#191829,
#191830),.UNSPECIFIED.,.F.,.F.,(4,2,4),(2.59315591655363,2.60891629140922,
2.66742166236768),.UNSPECIFIED.);
#1963=B_SPLINE_CURVE_WITH_KNOTS('',3,(#191831,#191832,#191833,#191834,#191835,
#191836,#191837,#191838,#191839,#191840),.UNSPECIFIED.,.F.,.F.,(4,1,1,1,
1,1,1,4),(152.455231345441,152.821976844167,153.820813294129,154.81964974409,
155.818486194052,156.817322644014,157.816159093976,158.388969095546),
 .UNSPECIFIED.);
#1964=B_SPLINE_CURVE_WITH_KNOTS('',3,(#191841,#191842,#191843,#191844,#191845,
#191846,#191847,#191848,#191849,#191850,#191851,#191852,#191853,#191854,
#191855,#191856,#191857,#191858,#191859,#191860,#191861,#191862,#191863,
#191864,#191865,#191866,#191867,#191868,#191869,#191870,#191871,#191872,
#191873,#191874,#191875,#191876,#191877,#191878,#191879,#191880,#191881,
#191882,#191883,#191884,#191885,#191886,#191887,#191888,#191889,#191890,
#191891,#191892,#191893,#191894,#191895,#191896,#191897,#191898,#191899,
#191900,#191901,#191902,#191903,#191904,#191905,#191906,#191907,#191908,
#191909,#191910,#191911,#191912,#191913,#191914,#191915,#191916,#191917,
#191918,#191919,#191920,#191921,#191922,#191923,#191924,#191925,#191926,
#191927,#191928,#191929,#191930,#191931,#191932,#191933,#191934,#191935,
#191936,#191937,#191938,#191939,#191940,#191941,#191942,#191943,#191944,
#191945,#191946,#191947,#191948,#191949,#191950,#191951,#191952,#191953,
#191954,#191955,#191956,#191957,#191958,#191959,#191960,#191961,#191962,
#191963,#191964,#191965,#191966,#191967,#191968,#191969,#191970,#191971,
#191972,#191973,#191974,#191975,#191976,#191977,#191978,#191979,#191980,
#191981,#191982,#191983,#191984,#191985,#191986,#191987,#191988,#191989,
#191990,#191991,#191992,#191993,#191994,#191995,#191996,#191997,#191998,
#191999,#192000,#192001,#192002,#192003,#192004,#192005,#192006,#192007,
#192008,#192009,#192010,#192011,#192012,#192013,#192014,#192015,#192016,
#192017,#192018,#192019,#192020,#192021,#192022,#192023,#192024,#192025,
#192026,#192027,#192028,#192029,#192030,#192031,#192032,#192033,#192034,
#192035,#192036,#192037,#192038,#192039,#192040,#192041,#192042,#192043,
#192044,#192045,#192046,#192047,#192048,#192049,#192050,#192051,#192052,
#192053,#192054,#192055,#192056,#192057,#192058,#192059,#192060,#192061,
#192062,#192063,#192064,#192065,#192066,#192067,#192068,#192069,#192070,
#192071,#192072,#192073,#192074),.UNSPECIFIED.,.F.,.F.,(4,2,2,2,2,2,2,2,
2,2,2,2,2,2,2,2,2,2,2,2,2,2,2,2,2,2,2,2,2,2,2,2,2,2,2,2,2,2,2,2,2,2,2,2,
2,2,2,2,2,2,2,2,2,2,2,2,2,2,2,2,2,2,2,2,2,2,2,2,2,2,2,2,2,2,2,2,2,2,2,2,
2,2,2,2,2,2,2,2,2,2,2,2,2,2,2,2,2,2,2,2,2,2,2,2,2,2,2,2,2,2,2,2,2,2,2,2,
4),(0.07512477121657,0.0866656614041577,0.0971787061917909,0.0994034139875145,
0.100649374983133,0.101721680739751,0.103083340651343,0.105770202884318,
0.123569836670099,0.183744945029975,0.200301942100647,0.203058816148262,
0.205554098781904,0.207453881261889,0.209279756454386,0.211819138400779,
0.218445141181668,0.274398200532703,0.298387415254804,0.309189818023144,
0.311432362033971,0.312682200516078,0.313754063516151,0.315110307992711,
0.317771871894378,0.334863658205109,0.380432706677751,0.408296195764049,
0.414628676252824,0.417320108936067,0.419278606857167,0.42107474541533,
0.423959418499773,0.430964032001749,0.48232321654618,0.509471790058244,
0.521088952724782,0.523378911923478,0.524639083027632,0.525710063956928,
0.527052823367524,0.52965154984707,0.545169501854001,0.592242170237513,
0.620259136846318,0.626610255077,0.629304907007226,0.631264021391924,0.633059530301395,
0.635940570563124,0.642922975181822,0.694639667019797,0.721533832947211,
0.733088375071281,0.735374885605499,0.736634330149682,0.737705399270661,
0.739049164328244,0.741652445975924,0.757275925677643,0.775418506847907,
0.777790870533834,0.810581386111433,0.833222084705453,0.838886993974625,
0.841460381041518,0.843399196152501,0.845225343494201,0.847765061428206,
0.854391825377458,0.910379596898951,0.934353181570827,0.945152042035031,
0.947394622720328,0.948644590082684,0.949716630493261,0.951073185283515,
0.95322029269039,0.964281235493402,1.01542252771507,1.04414436575984,1.05058033864303,
1.05328955602246,1.05525147030904,1.05704418198381,1.05990904150288,1.06679202178475,
1.11993302602103,1.1458307050905,1.15713530015814,1.15940781889123,1.16066431652466,
1.16173576521977,1.16308367872507,1.16570576983221,1.18175217783023,1.18586394160893,
1.20155431469556,1.23444009412102,1.25722651025384,1.26291138423872,1.26548861519639,
1.26742820930306,1.26925353863326,1.27178963464469,1.27839235753856,1.33462642983714,
1.35357799982722,1.36857940875808,1.37092931106035,1.37233171707441,1.37341125657246,
1.37461775534265,1.37666285255934,1.38470692584711,1.39984630235978,1.40873796955923),
 .UNSPECIFIED.);
#1965=B_SPLINE_CURVE_WITH_KNOTS('',3,(#192079,#192080,#192081,#192082,#192083,
#192084,#192085,#192086,#192087,#192088,#192089,#192090,#192091,#192092,
#192093,#192094,#192095,#192096,#192097,#192098,#192099,#192100,#192101,
#192102,#192103,#192104,#192105,#192106,#192107,#192108,#192109,#192110,
#192111,#192112,#192113,#192114,#192115,#192116,#192117,#192118,#192119,
#192120,#192121,#192122,#192123,#192124,#192125,#192126,#192127,#192128,
#192129,#192130,#192131,#192132,#192133,#192134,#192135,#192136,#192137,
#192138,#192139,#192140,#192141,#192142,#192143,#192144,#192145,#192146,
#192147,#192148,#192149,#192150,#192151,#192152,#192153,#192154,#192155,
#192156,#192157,#192158,#192159,#192160,#192161,#192162,#192163,#192164,
#192165,#192166,#192167,#192168,#192169,#192170,#192171,#192172,#192173,
#192174,#192175,#192176,#192177,#192178,#192179,#192180,#192181,#192182,
#192183,#192184,#192185,#192186,#192187,#192188,#192189,#192190,#192191,
#192192,#192193,#192194,#192195,#192196,#192197,#192198,#192199,#192200,
#192201,#192202,#192203,#192204,#192205,#192206,#192207,#192208,#192209,
#192210,#192211,#192212,#192213,#192214,#192215,#192216,#192217,#192218,
#192219,#192220,#192221,#192222,#192223,#192224,#192225,#192226,#192227,
#192228,#192229,#192230,#192231,#192232,#192233,#192234,#192235,#192236,
#192237,#192238,#192239,#192240,#192241,#192242,#192243,#192244,#192245,
#192246,#192247,#192248,#192249,#192250,#192251,#192252,#192253,#192254,
#192255,#192256,#192257,#192258,#192259,#192260,#192261,#192262,#192263,
#192264,#192265,#192266,#192267,#192268,#192269,#192270,#192271,#192272,
#192273,#192274,#192275,#192276,#192277,#192278,#192279,#192280,#192281,
#192282,#192283,#192284,#192285,#192286,#192287,#192288,#192289,#192290,
#192291,#192292,#192293,#192294,#192295,#192296,#192297,#192298,#192299,
#192300,#192301,#192302,#192303,#192304,#192305,#192306,#192307,#192308,
#192309,#192310,#192311,#192312),.UNSPECIFIED.,.F.,.F.,(4,2,2,2,2,2,2,2,
2,2,2,2,2,2,2,2,2,2,2,2,2,2,2,2,2,2,2,2,2,2,2,2,2,2,2,2,2,2,2,2,2,2,2,2,
2,2,2,2,2,2,2,2,2,2,2,2,2,2,2,2,2,2,2,2,2,2,2,2,2,2,2,2,2,2,2,2,2,2,2,2,
2,2,2,2,2,2,2,2,2,2,2,2,2,2,2,2,2,2,2,2,2,2,2,2,2,2,2,2,2,2,2,2,2,2,2,2,
4),(1.25960928709908,1.26784055573431,1.2907030527357,1.30119586065487,
1.3034192843059,1.3046649539869,1.30573723567159,1.3070991650138,1.30978755149372,
1.32763515531548,1.33373204709831,1.37574263222815,1.40292854225494,1.40705404575204,
1.4095456068141,1.41147833486376,1.41357286154704,1.41691845643489,1.42810816287076,
1.44666703949846,1.49069764380321,1.49656852631586,1.51244824860124,1.51506158847437,
1.51640744979989,1.51747862301405,1.51873640744419,1.52101504583588,1.53242880949112,
1.55875577111714,1.61123416629037,1.6181633430875,1.62103576667108,1.62282983176323,
1.62479052237024,1.62749309201263,1.63388985990958,1.68178083519589,1.72137474943336,
1.72610770227625,1.7278508967438,1.72887687896778,1.72996904592675,1.73147807218518,
1.73505282026033,1.77424775366377,1.82298113051944,1.83011227083648,1.83301820045556,
1.83481835059661,1.83677392681743,1.83944815625023,1.84567949843769,1.87271609449124,
1.91342988717374,1.93614233522075,1.93899617344875,1.9403730023126,1.94144668744679,
1.94268230334877,1.94485963231244,1.95464777071552,2.00353402176072,2.0386407217033,
2.04293541856535,2.04547648054644,2.04741711461237,2.0494904259782,2.05273919523384,
2.06305105273228,2.07961704929546,2.11250729383114,2.12706552683484,2.13238544468093,
2.14842388940541,2.15104513914485,2.15239273955484,2.15346401037507,2.15472039190784,
2.156992886137,2.1683017030916,2.19421613130566,2.24727727988239,2.25416193182608,
2.25702681904081,2.25881935758839,2.26078093521539,2.2634894100444,2.26992228791662,
2.29862561082173,2.34984929424604,2.36088140272063,2.36302660706477,2.36438250817935,
2.36545439847882,2.3667046166138,2.36894871961712,2.37977592854959,2.40385355560873,
2.45963351474795,2.46627478844487,2.46881661701892,2.47064319794461,2.47251919219428,
2.47500298951852,2.47774055588461,2.4822908937083,2.49161776582798,2.54225892254908,
2.57203619480185,2.57495056673749,2.57633918006039,2.57741400341707,2.57864191699185,
2.58078441361074,2.59007759676306,2.59315591655363),.UNSPECIFIED.);
#1966=B_SPLINE_CURVE_WITH_KNOTS('',3,(#192314,#192315,#192316,#192317,#192318,
#192319,#192320,#192321,#192322,#192323,#192324,#192325,#192326,#192327,
#192328,#192329,#192330,#192331,#192332,#192333,#192334,#192335,#192336,
#192337,#192338,#192339,#192340,#192341,#192342,#192343,#192344,#192345,
#192346,#192347,#192348,#192349,#192350,#192351,#192352,#192353,#192354,
#192355,#192356,#192357,#192358,#192359,#192360,#192361,#192362,#192363,
#192364,#192365,#192366,#192367,#192368,#192369,#192370,#192371,#192372,
#192373,#192374,#192375,#192376,#192377,#192378,#192379,#192380,#192381,
#192382,#192383,#192384,#192385,#192386,#192387,#192388,#192389,#192390,
#192391,#192392,#192393,#192394,#192395,#192396,#192397,#192398,#192399,
#192400,#192401,#192402,#192403,#192404,#192405,#192406,#192407,#192408,
#192409,#192410,#192411,#192412,#192413,#192414,#192415,#192416,#192417,
#192418,#192419,#192420,#192421,#192422,#192423,#192424,#192425,#192426,
#192427,#192428,#192429,#192430,#192431,#192432,#192433,#192434,#192435,
#192436,#192437,#192438,#192439,#192440,#192441,#192442,#192443,#192444,
#192445,#192446,#192447,#192448,#192449,#192450,#192451,#192452,#192453,
#192454,#192455,#192456,#192457,#192458,#192459,#192460,#192461,#192462,
#192463,#192464,#192465,#192466,#192467,#192468,#192469,#192470,#192471,
#192472,#192473,#192474,#192475,#192476,#192477,#192478,#192479,#192480,
#192481,#192482,#192483,#192484,#192485,#192486,#192487,#192488,#192489,
#192490,#192491,#192492,#192493,#192494,#192495,#192496,#192497,#192498,
#192499,#192500,#192501,#192502,#192503,#192504,#192505,#192506,#192507,
#192508,#192509,#192510,#192511,#192512,#192513,#192514,#192515,#192516,
#192517,#192518,#192519,#192520,#192521,#192522,#192523,#192524,#192525,
#192526,#192527,#192528,#192529,#192530,#192531,#192532,#192533,#192534,
#192535,#192536,#192537,#192538,#192539,#192540,#192541),.UNSPECIFIED.,
 .F.,.F.,(4,2,2,2,2,2,2,2,2,2,2,2,2,2,2,2,2,2,2,2,2,2,2,2,2,2,2,2,2,2,2,
2,2,2,2,2,2,2,2,2,2,2,2,2,2,2,2,2,2,2,2,2,2,2,2,2,2,2,2,2,2,2,2,2,2,2,2,
2,2,2,2,2,2,2,2,2,2,2,2,2,2,2,2,2,2,2,2,2,2,2,2,2,2,2,2,2,2,2,2,2,2,2,2,
2,2,2,2,2,2,2,2,2,2,4),(1.40873796955923,1.43954407347186,1.47079848867483,
1.4750246618546,1.47754608919005,1.47948389600165,1.48156609514269,1.48485392083813,
1.49550691464887,1.51283341063729,1.55311673063461,1.58010788384515,1.58301000885525,
1.58439643279473,1.58547124458416,1.58670103017614,1.58885122205798,1.59824667699909,
1.64748097300911,1.68269695329597,1.68699377340832,1.68953569495947,1.69147675734442,
1.69355030532848,1.69679898444777,1.70710668012022,1.7236623322147,1.75654736158497,
1.77010034868505,1.7774148449482,1.78177139990558,1.79293656332903,1.79509015725136,
1.79644870944042,1.79752093565588,1.79876952824895,1.80100566978832,1.811698694541,
1.83528019688316,1.89183149432246,1.89839602867847,1.90092591023938,1.90274951167987,
1.90468980742426,1.90727230391559,1.91298661612148,1.93599639997058,1.96905175821786,
1.99032132737911,2.00463237470267,2.00695314822479,2.0083469093453,2.00942514706726,
2.01063616926891,2.01270216615563,2.02100007169377,2.03685582517001,2.07906214793458,
2.10693287600035,2.11107655852846,2.11357363721655,2.11550741321349,2.11759985474868,
2.12093515510041,2.1320257106873,2.15035357269575,2.19838987285337,2.21636746232778,
2.21906065773651,2.22042375214956,2.22149627852515,2.22274146334813,2.22496223156422,
2.23541039286213,2.25811056621867,2.31604731638538,2.32244996429073,2.32495328846761,
2.32676986813482,2.32871401257197,2.33132120656349,2.33717234850553,2.36121619394524,
2.39060946057178,2.42822159314567,2.43104799992162,2.43241941944457,2.43349260124657,
2.43470695411841,2.43681596775364,2.43942266769537,2.44486047009304,2.46039785712345,
2.5018936809362,2.51079094849619,2.51723003235368,2.5321772650075,2.5359953013133,
2.5382170021158,2.5401286335118,2.54245486592691,2.54686349993011,2.57633055051127,
2.61936098785009,2.62769189673351,2.64069601077808,2.6429513496057,2.64434060170266,
2.64541553558637,2.64642425852135,2.6476373153628,2.64942356192591,2.65515826803913,
2.66782561093684),.UNSPECIFIED.);
#1967=B_SPLINE_CURVE_WITH_KNOTS('',3,(#192542,#192543,#192544,#192545,#192546,
#192547,#192548,#192549,#192550,#192551,#192552,#192553,#192554),
 .UNSPECIFIED.,.F.,.F.,(4,3,3,3,4),(-161.271232351587,-161.169466141419,
-161.067655433098,-160.96569395549,-160.920671713183),.UNSPECIFIED.);
#1968=B_SPLINE_CURVE_WITH_KNOTS('',3,(#192560,#192561,#192562,#192563,#192564,
#192565,#192566,#192567,#192568,#192569,#192570,#192571,#192572),
 .UNSPECIFIED.,.F.,.F.,(4,3,3,3,4),(170.955339710339,171.057208844183,171.158971096373,
171.260660134248,171.305836553012),.UNSPECIFIED.);
#1969=B_SPLINE_CURVE_WITH_KNOTS('',3,(#192573,#192574,#192575,#192576,#192577,
#192578,#192579,#192580,#192581,#192582,#192583,#192584,#192585,#192586,
#192587,#192588,#192589,#192590,#192591,#192592,#192593,#192594,#192595,
#192596,#192597,#192598,#192599,#192600,#192601,#192602,#192603,#192604,
#192605,#192606,#192607,#192608,#192609,#192610,#192611,#192612,#192613,
#192614,#192615,#192616,#192617,#192618,#192619,#192620,#192621,#192622,
#192623,#192624,#192625,#192626,#192627,#192628,#192629,#192630,#192631,
#192632,#192633,#192634,#192635,#192636,#192637,#192638,#192639,#192640,
#192641,#192642,#192643,#192644,#192645,#192646,#192647,#192648,#192649,
#192650,#192651,#192652,#192653,#192654,#192655,#192656,#192657,#192658,
#192659,#192660,#192661,#192662,#192663,#192664,#192665,#192666,#192667,
#192668,#192669,#192670,#192671,#192672,#192673,#192674,#192675,#192676,
#192677,#192678,#192679,#192680,#192681,#192682,#192683,#192684,#192685,
#192686,#192687,#192688,#192689,#192690,#192691,#192692,#192693,#192694,
#192695,#192696,#192697,#192698,#192699,#192700,#192701,#192702,#192703,
#192704,#192705,#192706,#192707,#192708,#192709,#192710,#192711,#192712,
#192713,#192714,#192715,#192716,#192717,#192718,#192719,#192720,#192721,
#192722,#192723,#192724,#192725,#192726,#192727,#192728,#192729,#192730,
#192731,#192732,#192733,#192734,#192735,#192736,#192737,#192738,#192739,
#192740,#192741,#192742,#192743,#192744,#192745,#192746,#192747,#192748,
#192749,#192750,#192751,#192752,#192753,#192754,#192755,#192756,#192757,
#192758,#192759,#192760,#192761,#192762,#192763,#192764,#192765,#192766,
#192767,#192768,#192769,#192770,#192771,#192772,#192773,#192774,#192775,
#192776,#192777,#192778,#192779,#192780,#192781,#192782,#192783,#192784,
#192785,#192786,#192787,#192788,#192789,#192790,#192791,#192792,#192793,
#192794),.UNSPECIFIED.,.F.,.F.,(4,2,2,2,2,2,2,2,2,2,2,2,2,2,2,2,2,2,2,2,
2,2,2,2,2,2,2,2,2,2,2,2,2,2,2,2,2,2,2,2,2,2,2,2,2,2,2,2,2,2,2,2,2,2,2,2,
2,2,2,2,2,2,2,2,2,2,2,2,2,2,2,2,2,2,2,2,2,2,2,2,2,2,2,2,2,2,2,2,2,2,2,2,
2,2,2,2,2,2,2,2,2,2,2,2,2,2,2,2,2,2,4),(0.000655551428707671,0.0215327131636358,
0.0285521200326831,0.0303960837974268,0.0316335735611994,0.032648445331859,
0.0337175330357083,0.035063454125746,0.0377856382359734,0.0559587373523061,
0.0616380686718176,0.0739377203228541,0.0845184170710276,0.106384424938896,
0.12297703761806,0.133286020145618,0.136520189199687,0.138580633014089,
0.140506643026182,0.143024716935975,0.147271544853911,0.192337496499189,
0.220917475857183,0.234450932701798,0.241868965911147,0.243841365085469,
0.244851087594292,0.245918126759799,0.247244742074754,0.249294071989488,
0.258883054629126,0.318505517323277,0.335297050192059,0.345718697613677,
0.348984721134232,0.351065006938216,0.353009378570062,0.355551374960315,
0.359839085161449,0.394233154429761,0.443435840109631,0.453287245382845,
0.455474802171122,0.456715771455664,0.457792036134616,0.459170705228411,
0.462028639566066,0.48480767131069,0.527329099661624,0.545904425390008,
0.55710221315087,0.560449734769267,0.562545400708846,0.564479142195401,
0.56697196403246,0.571099480905268,0.598277944722438,0.640347082526372,
0.656907907771879,0.66544954843179,0.667534893846574,0.668750026935094,
0.66982647738543,0.671211207856338,0.673503592060509,0.687287341627991,
0.698620516742917,0.737949645182713,0.764492288535883,0.770660358832987,
0.773322000804491,0.775273825915658,0.777074342259877,0.779989342853213,
0.787184837110465,0.833863301118626,0.856213723393924,0.870037628643727,
0.875062763886551,0.878645291653255,0.880154587653599,0.881246023642936,
0.882271307705382,0.884011280405899,0.888723629530098,0.929074828428406,
0.977358980984542,0.982966721211285,0.985529978576998,0.98746765419356,
0.989297520405304,0.991850133235058,0.998557316842197,1.05366063683498,
1.07817671190707,1.08912119333522,1.09137329019702,1.09262570653631,1.09369780718571,
1.09505199671401,1.09779133798081,1.11614975276579,1.16514969504523,1.18898303750825,
1.19480676010273,1.19740896677571,1.1993522579715,1.20117011609438,1.20367847747491,
1.21011174770897,1.25960928709908),.UNSPECIFIED.);
#1970=B_SPLINE_CURVE_WITH_KNOTS('',3,(#192796,#192797,#192798,#192799,#192800,
#192801,#192802,#192803,#192804,#192805,#192806,#192807,#192808,#192809,
#192810,#192811,#192812,#192813,#192814,#192815,#192816,#192817,#192818,
#192819,#192820,#192821,#192822,#192823,#192824,#192825,#192826,#192827,
#192828,#192829,#192830,#192831,#192832,#192833,#192834,#192835,#192836,
#192837,#192838,#192839,#192840,#192841,#192842,#192843,#192844,#192845,
#192846,#192847,#192848,#192849,#192850,#192851,#192852,#192853,#192854,
#192855,#192856,#192857,#192858,#192859,#192860,#192861,#192862,#192863,
#192864,#192865,#192866,#192867,#192868,#192869,#192870,#192871,#192872,
#192873,#192874,#192875,#192876,#192877,#192878,#192879,#192880,#192881,
#192882,#192883,#192884,#192885,#192886,#192887,#192888,#192889,#192890,
#192891,#192892,#192893,#192894,#192895,#192896,#192897,#192898,#192899,
#192900,#192901,#192902,#192903,#192904,#192905,#192906,#192907,#192908,
#192909,#192910,#192911,#192912,#192913,#192914,#192915,#192916,#192917,
#192918,#192919,#192920,#192921,#192922,#192923,#192924,#192925,#192926,
#192927,#192928,#192929,#192930,#192931,#192932,#192933,#192934,#192935,
#192936,#192937,#192938,#192939,#192940,#192941,#192942,#192943,#192944,
#192945,#192946,#192947,#192948,#192949,#192950,#192951,#192952,#192953,
#192954,#192955,#192956,#192957,#192958,#192959,#192960,#192961,#192962,
#192963,#192964,#192965,#192966,#192967,#192968,#192969,#192970,#192971,
#192972,#192973,#192974,#192975,#192976),.UNSPECIFIED.,.F.,.F.,(4,3,3,3,
3,3,3,3,3,3,3,3,3,3,3,3,3,3,3,3,3,3,3,3,3,3,3,3,3,3,3,3,3,3,3,3,3,3,3,3,
3,3,3,3,3,3,3,3,3,3,3,3,3,3,3,3,3,3,3,3,4),(-167.203857019737,-167.08981105619,
-166.975344513777,-166.860315157044,-166.805687143633,-166.702287413269,
-166.599041101161,-166.495916075704,-166.392856431583,-166.289828138948,
-166.186797211101,-166.083659393271,-165.98046526208,-165.877088303416,
-165.806850693671,-165.703453680563,-165.60021006525,-165.497087692404,
-165.394030672259,-165.291004971,-165.187976597935,-165.084841260237,-164.981649571235,
-164.878274965853,-164.808014243709,-164.704622130422,-164.601383514024,
-164.49826626414,-164.395214440686,-164.292194002343,-164.189170950985,
-164.086040989101,-163.982854714538,-163.879485526039,-163.809177793747,
-163.705782195491,-163.602540043973,-163.49941920119,-163.396363751132,
-163.293339657762,-163.190312928204,-163.087179277827,-162.983989303286,
-162.880616437379,-162.810341343785,-162.706946383757,-162.603704871958,
-162.500584667953,-162.397529855753,-162.294506398376,-162.191480301996,
-162.088347276007,-161.985157921902,-161.881785663091,-161.811504893824,
-161.70947172983,-161.607582180158,-161.505807287657,-161.404097849771,
-161.302405179864,-161.271232351587),.UNSPECIFIED.);
#1971=B_SPLINE_CURVE_WITH_KNOTS('',3,(#192977,#192978,#192979,#192980,#192981,
#192982,#192983,#192984,#192985,#192986,#192987,#192988,#192989),
 .UNSPECIFIED.,.F.,.F.,(4,3,3,3,4),(-167.553337646663,-167.448855727829,
-167.344457483332,-167.240110556711,-167.203857020092),.UNSPECIFIED.);
#1972=B_SPLINE_CURVE_WITH_KNOTS('',3,(#192995,#192996,#192997,#192998,#192999,
#193000,#193001,#193002,#193003,#193004),.UNSPECIFIED.,.F.,.F.,(4,3,3,4),
(7.59252172359161,7.70650209815482,7.82442144397709,7.94234078979936),
 .UNSPECIFIED.);
#1973=B_SPLINE_CURVE_WITH_KNOTS('',3,(#193006,#193007,#193008,#193009,#193010,
#193011,#193012,#193013,#193014,#193015,#193016,#193017,#193018,#193019,
#193020,#193021,#193022,#193023,#193024,#193025,#193026,#193027,#193028,
#193029,#193030,#193031,#193032,#193033,#193034,#193035,#193036,#193037,
#193038,#193039,#193040,#193041,#193042,#193043,#193044,#193045,#193046,
#193047,#193048,#193049,#193050,#193051,#193052,#193053,#193054,#193055,
#193056,#193057,#193058,#193059,#193060,#193061,#193062,#193063,#193064,
#193065,#193066,#193067,#193068,#193069,#193070,#193071,#193072,#193073,
#193074,#193075,#193076,#193077,#193078,#193079,#193080,#193081,#193082,
#193083,#193084,#193085,#193086,#193087,#193088,#193089,#193090,#193091,
#193092,#193093,#193094,#193095,#193096,#193097,#193098,#193099,#193100,
#193101,#193102,#193103,#193104,#193105,#193106,#193107,#193108,#193109,
#193110,#193111,#193112,#193113,#193114,#193115,#193116,#193117,#193118,
#193119,#193120,#193121,#193122,#193123,#193124,#193125,#193126,#193127,
#193128,#193129,#193130,#193131,#193132,#193133,#193134,#193135,#193136,
#193137,#193138,#193139,#193140,#193141,#193142,#193143,#193144,#193145,
#193146,#193147,#193148,#193149,#193150,#193151,#193152,#193153,#193154,
#193155,#193156,#193157,#193158,#193159,#193160,#193161,#193162,#193163,
#193164,#193165,#193166,#193167,#193168,#193169,#193170,#193171,#193172,
#193173,#193174),.UNSPECIFIED.,.F.,.F.,(4,3,3,3,3,3,3,3,3,3,3,3,3,3,3,3,
3,3,3,3,3,3,3,3,3,3,3,3,3,3,3,3,3,3,3,3,3,3,3,3,3,3,3,3,3,3,3,3,3,3,3,3,
3,3,3,3,4),(2.00878451764821,2.11210391279692,2.21526989698117,2.31831446525096,
2.42129383098617,2.52424213980858,2.62719349431534,2.73024965054147,2.83336280284661,
2.93665222006101,2.99650934988563,3.10008230986109,3.20350557536163,3.30681224772116,
3.4100563283188,3.51327157245755,3.61649169494142,3.71982084946894,3.82320780718055,
3.92677785652903,3.99534579984751,4.09860812441835,4.2017150863826,4.30469852295217,
4.40761526975675,4.51049956061293,4.61338558491655,4.71637810302099,4.81942648355166,
4.92265858166643,4.99418224980938,5.09760358352983,5.20087156240154,5.30401824171002,
5.40709952008129,5.51014939511661,5.61320182122769,5.71636085636684,5.81957608032993,
5.92297369428319,5.99301869977126,6.09643423755244,6.19969678686738,6.30283861434793,
6.40591539958098,6.50896114779516,6.61200982139876,6.71516571129313,6.81837812515205,
6.9217735049757,6.99185514973314,7.0967069869202,7.20139081251388,7.30591389133753,
7.41034214208164,7.51471167951793,7.59252172323623),.UNSPECIFIED.);
#1974=B_SPLINE_CURVE_WITH_KNOTS('',3,(#193178,#193179,#193180,#193181,#193182,
#193183,#193184,#193185,#193186,#193187,#193188,#193189,#193190,#193191,
#193192,#193193,#193194,#193195,#193196,#193197,#193198,#193199,#193200,
#193201,#193202,#193203,#193204,#193205,#193206,#193207,#193208,#193209,
#193210,#193211,#193212,#193213,#193214,#193215,#193216,#193217,#193218,
#193219,#193220,#193221,#193222,#193223,#193224,#193225,#193226,#193227,
#193228,#193229,#193230,#193231,#193232,#193233,#193234,#193235,#193236,
#193237,#193238,#193239,#193240,#193241,#193242,#193243,#193244,#193245,
#193246,#193247,#193248,#193249,#193250,#193251,#193252,#193253,#193254,
#193255,#193256,#193257,#193258,#193259,#193260,#193261,#193262,#193263,
#193264,#193265,#193266,#193267,#193268,#193269,#193270,#193271,#193272,
#193273,#193274,#193275,#193276,#193277,#193278,#193279,#193280,#193281,
#193282,#193283,#193284,#193285,#193286,#193287,#193288,#193289,#193290,
#193291,#193292,#193293,#193294,#193295),.UNSPECIFIED.,.F.,.F.,(4,3,3,3,
3,3,3,3,3,3,3,3,3,3,3,3,3,3,3,3,3,3,3,3,3,3,3,3,3,3,3,3,3,3,3,3,3,3,3,4),
(-3.84103903298818,-3.73547282260036,-3.63371534451888,-3.53202565477874,
-3.43036802202408,-3.3287067634427,-3.22694496884903,-3.12512264837507,
-3.02313913493882,-2.99650934988562,-2.89298838415395,-2.7896184205715,
-2.68636679313977,-2.58317880759893,-2.48002064176421,-2.37685851496106,
-2.27358841489219,-2.17026119505925,-2.06675136672922,-1.99767289992375,
-1.89536901188924,-1.79321917542629,-1.69118674247093,-1.58921701577407,
-1.48727463022112,-1.3853242611676,-1.28325154596761,-1.18111583450438,
-1.07877443242794,-0.998836449961874,-0.892563151715309,-0.780992757750895,
-0.675072785964147,-0.569252409114428,-0.463503885892126,-0.357799564693429,
-0.252082102978388,-0.146359553840664,-0.0405640348441741,0.),
 .UNSPECIFIED.);
#1975=B_SPLINE_CURVE_WITH_KNOTS('',3,(#193296,#193297,#193298,#193299,#193300,
#193301,#193302,#193303,#193304,#193305,#193306,#193307,#193308,#193309,
#193310,#193311,#193312,#193313,#193314,#193315,#193316,#193317,#193318,
#193319,#193320,#193321),.UNSPECIFIED.,.F.,.F.,(4,2,2,2,2,2,2,2,2,2,2,2,
4),(0.000655554096865791,0.0215326957973204,0.028552110634771,0.0303960798049156,
0.0316335711042768,0.0326484421215227,0.0337175280396046,0.0350634423926314,
0.0377855980008208,0.0559579040604788,0.0616381299228464,0.0739378344818628,
0.0747573278913931),.UNSPECIFIED.);
#1976=B_SPLINE_CURVE_WITH_KNOTS('',3,(#193327,#193328,#193329,#193330,#193331,
#193332,#193333,#193334,#193335,#193336,#193337,#193338,#193339,#193340,
#193341,#193342,#193343,#193344,#193345,#193346,#193347,#193348,#193349,
#193350),.UNSPECIFIED.,.F.,.F.,(4,2,2,2,2,2,2,2,2,2,2,4),(2.59392175456229,
2.61962491033593,2.62795697204938,2.64096287978827,2.64321853041206,2.64460797466987,
2.64568305731841,2.64669191990705,2.64790514474502,2.64969163875382,2.65542713745129,
2.66809622952257),.UNSPECIFIED.);
#1977=B_SPLINE_CURVE_WITH_KNOTS('',3,(#193351,#193352,#193353,#193354,#193355,
#193356,#193357,#193358,#193359,#193360,#193361,#193362,#193363,#193364,
#193365,#193366,#193367,#193368,#193369,#193370,#193371,#193372,#193373,
#193374,#193375,#193376,#193377,#193378,#193379,#193380,#193381,#193382,
#193383,#193384,#193385,#193386,#193387,#193388,#193389,#193390,#193391,
#193392,#193393,#193394,#193395,#193396,#193397,#193398,#193399,#193400,
#193401,#193402,#193403,#193404,#193405,#193406,#193407,#193408,#193409,
#193410,#193411,#193412,#193413,#193414,#193415,#193416,#193417,#193418,
#193419,#193420,#193421,#193422,#193423,#193424,#193425,#193426,#193427,
#193428,#193429,#193430,#193431,#193432,#193433,#193434,#193435,#193436,
#193437,#193438,#193439,#193440,#193441,#193442,#193443,#193444,#193445,
#193446,#193447,#193448,#193449,#193450,#193451,#193452,#193453,#193454,
#193455,#193456,#193457,#193458,#193459,#193460,#193461,#193462,#193463,
#193464,#193465,#193466,#193467,#193468,#193469,#193470,#193471,#193472,
#193473,#193474,#193475,#193476,#193477,#193478,#193479,#193480,#193481,
#193482,#193483,#193484,#193485,#193486,#193487,#193488,#193489,#193490,
#193491,#193492,#193493,#193494,#193495,#193496,#193497,#193498,#193499,
#193500,#193501,#193502,#193503,#193504,#193505,#193506,#193507,#193508,
#193509,#193510,#193511,#193512,#193513,#193514,#193515,#193516,#193517,
#193518,#193519,#193520,#193521,#193522,#193523,#193524,#193525,#193526,
#193527,#193528,#193529,#193530,#193531),.UNSPECIFIED.,.F.,.F.,(4,3,3,3,
3,3,3,3,3,3,3,3,3,3,3,3,3,3,3,3,3,3,3,3,3,3,3,3,3,3,3,3,3,3,3,3,3,3,3,3,
3,3,3,3,3,3,3,3,3,3,3,3,3,3,3,3,3,3,3,3,4),(7.94234078979936,7.99069159969502,
8.0940913187467,8.19733761942809,8.30046263334334,8.4035222658568,8.50655054683657,
8.60958146299715,8.71271926917291,8.8159133887099,8.91929033584984,8.98952804965688,
9.09292506063529,9.19616867374971,9.29929104430254,9.40234806209879,9.50537376095564,
9.60840213156772,9.71153746675316,9.81472915320384,9.9181037560014,9.98836449961875,
10.0917566178357,10.1949952392422,10.2981124942289,10.4011643228401,10.5041847663884,
10.6072078229917,10.7103377901475,10.8135240700051,10.9168932637763,10.9872009495806,
11.0905965455969,11.1938386948507,11.2969595353445,11.4000149830984,11.5030390741534,
11.6060658013884,11.7091994494476,11.8123894216688,11.91576228528,11.9860373995425,
12.0894323593401,12.192673870897,12.2957940746466,12.3988488865806,12.5018723436841,
12.6048984397812,12.7080314654776,12.8112208192822,12.9145930777863,12.9848738495044,
13.0869196151459,13.1887917827773,13.2905669746092,13.3922809415229,13.4939693493735,
13.5957283273467,13.697522002645,13.7994743418109,13.8757070301447),
 .UNSPECIFIED.);
#1978=B_SPLINE_CURVE_WITH_KNOTS('',3,(#193532,#193533,#193534,#193535,#193536,
#193537,#193538,#193539,#193540,#193541,#193542,#193543,#193544,#193545,
#193546,#193547,#193548,#193549,#193550,#193551,#193552,#193553,#193554,
#193555,#193556,#193557,#193558,#193559,#193560,#193561,#193562,#193563,
#193564,#193565,#193566,#193567,#193568,#193569,#193570,#193571,#193572,
#193573,#193574,#193575,#193576,#193577,#193578,#193579,#193580,#193581,
#193582,#193583,#193584,#193585,#193586,#193587,#193588,#193589,#193590,
#193591,#193592,#193593,#193594,#193595,#193596,#193597,#193598,#193599,
#193600,#193601,#193602,#193603,#193604,#193605,#193606,#193607,#193608,
#193609,#193610,#193611,#193612,#193613,#193614,#193615,#193616,#193617,
#193618,#193619,#193620,#193621,#193622,#193623,#193624,#193625,#193626,
#193627,#193628,#193629,#193630,#193631,#193632,#193633,#193634,#193635,
#193636,#193637,#193638,#193639,#193640,#193641,#193642,#193643,#193644,
#193645,#193646,#193647,#193648,#193649,#193650,#193651,#193652,#193653,
#193654,#193655,#193656,#193657,#193658,#193659,#193660,#193661,#193662,
#193663,#193664,#193665,#193666,#193667,#193668,#193669,#193670,#193671,
#193672,#193673,#193674,#193675,#193676,#193677,#193678,#193679,#193680,
#193681,#193682,#193683,#193684,#193685,#193686,#193687,#193688,#193689,
#193690,#193691,#193692,#193693,#193694,#193695,#193696,#193697,#193698,
#193699,#193700,#193701,#193702,#193703,#193704,#193705,#193706,#193707,
#193708,#193709,#193710,#193711,#193712,#193713,#193714,#193715,#193716,
#193717,#193718,#193719,#193720,#193721,#193722,#193723,#193724,#193725,
#193726,#193727,#193728,#193729,#193730,#193731,#193732,#193733,#193734,
#193735,#193736,#193737,#193738,#193739,#193740,#193741,#193742,#193743,
#193744,#193745,#193746,#193747,#193748,#193749,#193750,#193751,#193752,
#193753,#193754,#193755,#193756,#193757),.UNSPECIFIED.,.F.,.F.,(4,2,2,2,
2,2,2,2,2,2,2,2,2,2,2,2,2,2,2,2,2,2,2,2,2,2,2,2,2,2,2,2,2,2,2,2,2,2,2,2,
2,2,2,2,2,2,2,2,2,2,2,2,2,2,2,2,2,2,2,2,2,2,2,2,2,2,2,2,2,2,2,2,2,2,2,2,
2,2,2,2,2,2,2,2,2,2,2,2,2,2,2,2,2,2,2,2,2,2,2,2,2,2,2,2,2,2,2,2,2,2,2,2,
4),(0.0747573278913931,0.0845184568723634,0.106384488924799,0.122977073836737,
0.133286041480215,0.136520206462886,0.138580647778778,0.14050665550755,
0.14302472648801,0.147271549528457,0.192337588514278,0.220917592465344,
0.234450995086863,0.241869005899496,0.243841401544,0.244851122749664,0.245918161725359,
0.247244777703299,0.249294109348943,0.258883112422578,0.318505453636211,
0.335297069016963,0.345718755640732,0.348984785040333,0.35106507308597,
0.35300944577025,0.355551442051943,0.359839148817527,0.39423292416601,0.44343534651272,
0.453287175653806,0.455474762914013,0.456715739764428,0.457792004326271,
0.45917066473234,0.462028553635301,0.484805755916712,0.527329183667635,
0.545904430961908,0.557102184503488,0.560449702389093,0.562545367444631,
0.564479109101443,0.566971932534784,0.571099455013165,0.598278134504166,
0.64034775302055,0.656908101261101,0.665449578366819,0.667534910396288,
0.668750040287345,0.669826490989463,0.671211225752069,0.673503625263376,
0.687287701042015,0.69862097868883,0.737949750063071,0.764492311579503,
0.770660371029709,0.773322010667461,0.775273834943801,0.777074351130886,
0.77998935283224,0.787184856519674,0.833862854130476,0.856213797873246,
0.870037658861674,0.875062782863863,0.878645304219324,0.880154598875101,
0.881246034459896,0.882271318788963,0.884011292777907,0.888723650256947,
0.929075020144451,0.977358997253004,0.982966736376446,0.985529993712516,
0.987467669503632,0.989297536027248,0.99185014953113,0.998557336409075,
1.05366060343261,1.07817670201039,1.0891211898708,1.0913732874147,1.09262570405227,
1.09369780479726,1.09505199430249,1.09779133537881,1.11614974346584,1.16514968870468,
1.18898303046794,1.19480675283253,1.19740895939576,1.19935225050625,1.20117010854636,
1.20367846980671,1.21011173969497,1.26784055833987,1.29070305368072,1.30119586102782,
1.30341928450233,1.30466495407273,1.30573723565602,1.30709916485218,1.30978755097911,
1.32763514925058,1.33373204695253,1.37574263655658,1.40292854304668,1.40705404623529,
1.40817977152992),.UNSPECIFIED.);
#1979=B_SPLINE_CURVE_WITH_KNOTS('',3,(#193762,#193763,#193764,#193765,#193766,
#193767,#193768,#193769,#193770,#193771,#193772,#193773,#193774,#193775,
#193776,#193777,#193778,#193779,#193780,#193781,#193782,#193783,#193784,
#193785,#193786,#193787,#193788,#193789,#193790,#193791,#193792,#193793,
#193794,#193795,#193796,#193797,#193798,#193799,#193800,#193801,#193802,
#193803,#193804,#193805,#193806,#193807,#193808,#193809,#193810,#193811,
#193812,#193813,#193814,#193815,#193816,#193817,#193818,#193819,#193820,
#193821,#193822,#193823,#193824,#193825,#193826,#193827,#193828,#193829,
#193830,#193831,#193832,#193833,#193834,#193835,#193836,#193837,#193838,
#193839,#193840,#193841,#193842,#193843,#193844,#193845,#193846,#193847,
#193848,#193849,#193850,#193851,#193852,#193853,#193854,#193855,#193856,
#193857,#193858,#193859,#193860,#193861,#193862,#193863,#193864,#193865,
#193866,#193867,#193868,#193869,#193870,#193871,#193872,#193873,#193874,
#193875,#193876,#193877,#193878,#193879,#193880,#193881,#193882,#193883,
#193884,#193885,#193886,#193887,#193888,#193889,#193890,#193891,#193892,
#193893,#193894,#193895,#193896,#193897,#193898,#193899,#193900,#193901,
#193902,#193903,#193904,#193905,#193906,#193907,#193908,#193909,#193910,
#193911,#193912,#193913,#193914,#193915,#193916,#193917,#193918,#193919,
#193920,#193921,#193922,#193923,#193924,#193925,#193926,#193927,#193928,
#193929,#193930,#193931,#193932,#193933,#193934,#193935,#193936,#193937,
#193938,#193939,#193940,#193941,#193942,#193943,#193944,#193945,#193946,
#193947,#193948,#193949,#193950,#193951,#193952,#193953,#193954,#193955,
#193956,#193957,#193958,#193959,#193960,#193961,#193962,#193963,#193964,
#193965,#193966,#193967,#193968,#193969,#193970,#193971,#193972,#193973,
#193974,#193975,#193976,#193977,#193978,#193979,#193980,#193981,#193982,
#193983,#193984,#193985,#193986,#193987,#193988,#193989,#193990,#193991,
#193992,#193993,#193994,#193995,#193996,#193997,#193998,#193999),
 .UNSPECIFIED.,.F.,.F.,(4,2,2,2,2,2,2,2,2,2,2,2,2,2,2,2,2,2,2,2,2,2,2,2,
2,2,2,2,2,2,2,2,2,2,2,2,2,2,2,2,2,2,2,2,2,2,2,2,2,2,2,2,2,2,2,2,2,2,2,2,
2,2,2,2,2,2,2,2,2,2,2,2,2,2,2,2,2,2,2,2,2,2,2,2,2,2,2,2,2,2,2,2,2,2,2,2,
2,2,2,2,2,2,2,2,2,2,2,2,2,2,2,2,2,2,2,2,2,2,4),(1.26014529339144,1.26297464047121,
1.26555236723457,1.26749233441503,1.2693180147951,1.27185459848015,1.27845859063422,
1.33470346965188,1.35365868098231,1.36866297404335,1.37101332824703,1.37241600397414,
1.37349575110534,1.37470248195186,1.37674797261363,1.38479359426047,1.39993588627135,
1.43964131592529,1.47090170089244,1.47512868593201,1.47765059794279,1.47958877742304,
1.48167137717811,1.48495983582815,1.49561488389859,1.5129447246226,1.55323577024489,
1.58023210347049,1.58313478647756,1.5845214770423,1.5855964955573,1.58682651772072,
1.58897712332772,1.5983743876709,1.64761815055298,1.6828408894392,1.6871385356592,
1.68968094602136,1.69162238173212,1.69369632858282,1.696945632746,1.70725531277231,
1.72381415334077,1.7567055088474,1.77026169396841,1.77757609119675,1.78191649753897,
1.79309983972583,1.79525482756751,1.7966139394648,1.79768639494436,1.79893501072878,
1.80117058855457,1.81184953177432,1.83537668589542,1.89203012686887,1.89858598361363,
1.90111475535078,1.90293828754355,1.90487918603592,1.90746364353385,1.91318707955642,
1.93626122682681,1.96949461915746,1.99168668419642,2.00493620480639,2.00720423123931,
2.00858258859569,2.00965907517461,2.01087962134308,2.01298790445359,2.02181641686492,
2.03922372257643,2.0891080218214,2.10792309328548,2.11166728769388,2.11407096925926,
2.11598841192212,2.11815423043834,2.12181980478344,2.13646359084584,2.16403801057788,
2.19307511410123,2.21638807851245,2.21924821682677,2.22062641212825,2.22170037777364,
2.22293543219521,2.22510965790808,2.23484893066339,2.28378537384592,2.31891048836793,
2.32320602849357,2.32574754257893,2.32768849518688,2.3297621211283,2.33301132997924,
2.34332414180407,2.35989128493126,2.39134215898152,2.4284352304507,2.43127319634106,
2.43264700949187,2.4337205416077,2.43493360054744,2.43703639558514,2.43963351673771,
2.44504314187052,2.46045902525304,2.50150255754408,2.53107943269,2.53526960368001,
2.53778045354652,2.53971652310281,2.54180316017597,2.5451114364364,2.55595042400506,
2.57369920292217,2.59392175456229),.UNSPECIFIED.);
#1980=B_SPLINE_CURVE_WITH_KNOTS('',3,(#194001,#194002,#194003,#194004,#194005,
#194006,#194007,#194008,#194009,#194010,#194011,#194012,#194013,#194014,
#194015,#194016,#194017,#194018,#194019,#194020,#194021,#194022,#194023,
#194024,#194025,#194026,#194027,#194028,#194029,#194030,#194031,#194032,
#194033,#194034,#194035,#194036,#194037,#194038,#194039,#194040,#194041,
#194042,#194043,#194044,#194045,#194046,#194047,#194048,#194049,#194050,
#194051,#194052,#194053,#194054,#194055,#194056,#194057,#194058,#194059,
#194060,#194061,#194062,#194063,#194064,#194065,#194066,#194067,#194068,
#194069,#194070,#194071,#194072,#194073,#194074,#194075,#194076,#194077,
#194078,#194079,#194080,#194081,#194082,#194083,#194084,#194085,#194086,
#194087,#194088,#194089,#194090,#194091,#194092,#194093,#194094,#194095,
#194096,#194097,#194098,#194099,#194100,#194101,#194102,#194103,#194104,
#194105,#194106,#194107,#194108,#194109,#194110,#194111,#194112,#194113,
#194114,#194115,#194116,#194117,#194118,#194119,#194120,#194121,#194122,
#194123,#194124,#194125,#194126,#194127,#194128,#194129,#194130,#194131,
#194132,#194133,#194134,#194135,#194136,#194137,#194138,#194139,#194140,
#194141,#194142,#194143,#194144,#194145,#194146,#194147,#194148,#194149,
#194150,#194151,#194152,#194153,#194154,#194155,#194156,#194157,#194158,
#194159,#194160,#194161,#194162,#194163,#194164,#194165,#194166,#194167,
#194168,#194169,#194170,#194171,#194172,#194173,#194174,#194175,#194176,
#194177,#194178,#194179,#194180,#194181,#194182,#194183,#194184,#194185,
#194186,#194187,#194188,#194189,#194190,#194191,#194192,#194193,#194194,
#194195,#194196,#194197,#194198,#194199,#194200,#194201,#194202,#194203,
#194204,#194205,#194206,#194207,#194208,#194209,#194210),.UNSPECIFIED.,
 .F.,.F.,(4,2,2,2,2,2,2,2,2,2,2,2,2,2,2,2,2,2,2,2,2,2,2,2,2,2,2,2,2,2,2,
2,2,2,2,2,2,2,2,2,2,2,2,2,2,2,2,2,2,2,2,2,2,2,2,2,2,2,2,2,2,2,2,2,2,2,2,
2,2,2,2,2,2,2,2,2,2,2,2,2,2,2,2,2,2,2,2,2,2,2,2,2,2,2,2,2,2,2,2,2,2,2,2,
2,4),(1.40817977152992,1.40954560710164,1.41147833499254,1.41357286149577,
1.41691845607658,1.42810816125348,1.446667035395,1.49069771000593,1.49656846812303,
1.51244824665426,1.51506158779642,1.51640744933461,1.51747862250971,1.51873640666159,
1.52101504384949,1.53242878693592,1.55875566711102,1.61123417855208,1.61816334709237,
1.6210357693046,1.62282983413917,1.62479052494421,1.62749309573695,1.63388987049344,
1.68178411506865,1.72137471504812,1.72610769463321,1.72785089316597,1.72887687619305,
1.72996904263184,1.73147806597397,1.73505279712531,1.77424410856813,1.8229813441372,
1.83011233352274,1.83301823777969,1.83481838319174,1.83677396295087,1.83944821285175,
1.84567967409462,1.87271723788112,1.91343293580722,1.93614245550613,1.93899622171256,
1.94037303639201,1.94144672013567,1.94268234535814,1.94485971688534,1.95464848026898,
2.00353420224454,2.03864073142966,2.04293542590678,2.04547648713978,2.04741712101568,
2.04949043254769,2.0527392028345,2.06305107008396,2.07961708842125,2.11250735084954,
2.12706716039433,2.13238510253001,2.14842386248627,2.1510451319288,2.15239273654899,
2.15346400760861,2.15472038582165,2.15699286488075,2.1683014188057,2.19421481590956,
2.24727744647852,2.25416198487916,2.25702685337156,2.25881938848315,2.26078096900714,
2.2634894600511,2.26992243433805,2.29862656765248,2.34984819605326,2.3608812887332,
2.36302655399557,2.36438247365213,2.36545436528211,2.36670456963672,2.36894860964171,
2.37977478053233,2.40384855905286,2.45963438345724,2.4662750556321,2.4688167898324,
2.47064334573534,2.47251935282139,2.47500322956724,2.47774090665828,2.48229151414849,
2.49161915572466,2.54225933502191,2.57203620462721,2.57495057631857,2.57633918951182,
2.57741401276103,2.57864192620402,2.58078442257017,2.59007760424531,2.60891629515257,
2.66742166574813),.UNSPECIFIED.);
#1981=B_SPLINE_CURVE_WITH_KNOTS('',3,(#194211,#194212,#194213,#194214),
 .UNSPECIFIED.,.F.,.F.,(4,4),(-16.7565928758252,-16.4074096477818),
 .UNSPECIFIED.);
#1982=B_SPLINE_CURVE_WITH_KNOTS('',3,(#194220,#194221,#194222,#194223,#194224,
#194225,#194226,#194227,#194228,#194229,#194230,#194231,#194232,#194233,
#194234,#194235),.UNSPECIFIED.,.F.,.F.,(4,2,2,2,2,2,2,4),(2.5939427763898,
2.64911100496539,2.65727579111078,2.66034775251964,2.66217948411756,2.66402387340263,
2.66631624952862,2.66838106686199),.UNSPECIFIED.);
#1983=B_SPLINE_CURVE_WITH_KNOTS('',3,(#194236,#194237,#194238,#194239,#194240,
#194241,#194242,#194243,#194244,#194245,#194246,#194247,#194248,#194249,
#194250,#194251,#194252,#194253,#194254,#194255,#194256,#194257,#194258,
#194259,#194260,#194261,#194262,#194263,#194264,#194265,#194266,#194267,
#194268,#194269,#194270,#194271,#194272,#194273,#194274,#194275,#194276,
#194277,#194278,#194279,#194280,#194281,#194282,#194283,#194284,#194285,
#194286,#194287,#194288,#194289,#194290,#194291,#194292,#194293,#194294,
#194295,#194296,#194297,#194298,#194299,#194300,#194301,#194302,#194303,
#194304,#194305,#194306,#194307,#194308,#194309,#194310,#194311,#194312,
#194313,#194314,#194315,#194316,#194317,#194318,#194319,#194320,#194321,
#194322,#194323,#194324,#194325,#194326,#194327,#194328,#194329,#194330,
#194331,#194332,#194333,#194334,#194335,#194336,#194337,#194338,#194339,
#194340,#194341,#194342,#194343,#194344,#194345,#194346,#194347,#194348,
#194349,#194350,#194351,#194352,#194353,#194354,#194355,#194356,#194357,
#194358,#194359,#194360,#194361,#194362,#194363,#194364,#194365,#194366,
#194367,#194368,#194369,#194370,#194371,#194372,#194373,#194374,#194375,
#194376,#194377,#194378,#194379,#194380,#194381,#194382,#194383,#194384,
#194385,#194386,#194387,#194388,#194389,#194390,#194391,#194392,#194393,
#194394,#194395,#194396,#194397,#194398,#194399,#194400,#194401,#194402,
#194403,#194404,#194405,#194406,#194407,#194408,#194409,#194410,#194411,
#194412,#194413,#194414,#194415,#194416,#194417,#194418,#194419,#194420,
#194421,#194422,#194423,#194424,#194425,#194426,#194427,#194428,#194429,
#194430,#194431,#194432,#194433,#194434,#194435,#194436,#194437,#194438,
#194439,#194440,#194441,#194442,#194443,#194444,#194445,#194446,#194447,
#194448,#194449,#194450,#194451,#194452,#194453,#194454,#194455,#194456,
#194457,#194458,#194459,#194460,#194461,#194462,#194463,#194464,#194465,
#194466,#194467,#194468,#194469,#194470,#194471,#194472,#194473,#194474,
#194475,#194476,#194477,#194478,#194479,#194480,#194481,#194482,#194483,
#194484,#194485,#194486,#194487),.UNSPECIFIED.,.F.,.F.,(4,2,2,2,2,2,2,2,
2,2,2,2,2,2,2,2,2,2,2,2,2,2,2,2,2,2,2,2,2,2,2,2,2,2,2,2,2,2,2,2,2,2,2,2,
2,2,2,2,2,2,2,2,2,2,2,2,2,2,2,2,2,2,2,2,2,2,2,2,2,2,2,2,2,2,2,2,2,2,2,2,
2,2,2,2,2,2,2,2,2,2,2,2,2,2,2,2,2,2,2,2,2,2,2,2,2,2,2,2,2,2,2,2,2,2,2,2,
2,2,2,2,2,2,2,2,2,4),(0.000823825197108989,0.00400945008563605,0.0104637827734715,
0.0609493693956797,0.0860173114433529,0.0971066951178503,0.0993664141855828,
0.100619998727938,0.101691504613244,0.103042734738811,0.105680874999083,
0.122156709361488,0.172105754414404,0.190189888152416,0.201175646680102,
0.203636604208991,0.205921753369301,0.205936334788996,0.205951510161678,
0.205967318969076,0.205983804396929,0.206001013822833,0.206018999431138,
0.206037818701473,0.2060575352396,0.206078219659453,0.206099950534169,0.206122815608128,
0.206146913284508,0.20617235431584,0.206199263901127,0.206227784226489,
0.206258077562141,0.206290330162048,0.206324757003612,0.20636160834815,
0.206401176938608,0.206443806358067,0.208321239629732,0.210755229228764,
0.215433670312416,0.250555505648697,0.29950005778079,0.309248472817553,
0.311423081347828,0.312658085391576,0.313731840173607,0.315109537400538,
0.317967874933001,0.353828595109926,0.386598389472844,0.409207048056845,
0.414867595734132,0.417440163230724,0.419378833009472,0.421205190150472,
0.423745755827132,0.430378023195683,0.486305361914658,0.510318387916333,
0.521127860127566,0.523371066138102,0.524621160516376,0.525693173261203,
0.52704951776782,0.529711009742722,0.546792814120082,0.555102456937598,
0.565638158030108,0.59847270441242,0.615002218808887,0.625298987067793,
0.628546307193363,0.630619495712637,0.632560579126951,0.635103045533725,
0.639401978915324,0.674781700322757,0.723973283194637,0.733291858361445,
0.735436533521945,0.736665093209176,0.737740095302287,0.739128418474605,
0.742040359487207,0.773906432611635,0.777744915834216,0.810547269846879,
0.833200978877344,0.838868146716202,0.841442243238062,0.843381464312925,
0.845207899677868,0.847747866938959,0.854374387878647,0.910387711871419,
0.934356207047114,0.94515451905543,0.947397371356511,0.948647544277521,
0.949719794415094,0.95107665750154,0.953224333347304,0.964289920602169,
1.01543693676616,1.04416538621516,1.05060272632574,1.05331248660352,1.05527478220288,
1.05706783416788,1.05993321980338,1.06681737249372,1.1199705330045,1.14587183848024,
1.15717826179401,1.15945119770653,1.16070793268664,1.1617795878345,1.16312776624361,
1.16575038791887,1.18180028426588,1.18591196532136,1.20160576350127,1.23449786883911,
1.25728867247218,1.26014529339144),.UNSPECIFIED.);
#1984=B_SPLINE_CURVE_WITH_KNOTS('',3,(#194489,#194490,#194491,#194492,#194493,
#194494,#194495,#194496,#194497,#194498),.UNSPECIFIED.,.F.,.F.,(4,1,1,1,
1,1,1,4),(-22.6905949549614,-21.9744018991612,-20.9755654491994,-19.9767289992375,
-18.9778925492756,-17.9790560993137,-16.9802196493519,-16.7565928758252),
 .UNSPECIFIED.);
#1985=B_SPLINE_CURVE_WITH_KNOTS('',3,(#194499,#194500,#194501,#194502,#194503,
#194504,#194505,#194506,#194507,#194508,#194509,#194510,#194511,#194512,
#194513,#194514,#194515,#194516,#194517,#194518),.UNSPECIFIED.,.F.,.F.,
(4,2,2,2,2,2,2,2,2,4),(0.000629330687125576,0.0481769840684086,0.0539096608571859,
0.0578765520360831,0.0594500272904705,0.0605539083195781,0.0615639069530703,
0.0632252827349632,0.0674368411984206,0.0747600637111309),.UNSPECIFIED.);
#1986=B_SPLINE_CURVE_WITH_KNOTS('',3,(#194523,#194524,#194525,#194526,#194527,
#194528,#194529,#194530,#194531,#194532,#194533,#194534,#194535,#194536,
#194537,#194538,#194539,#194540,#194541,#194542,#194543,#194544,#194545,
#194546,#194547,#194548,#194549,#194550,#194551,#194552,#194553,#194554,
#194555,#194556,#194557,#194558,#194559,#194560,#194561,#194562,#194563,
#194564,#194565,#194566,#194567,#194568,#194569,#194570,#194571,#194572,
#194573,#194574,#194575,#194576,#194577,#194578,#194579,#194580,#194581,
#194582,#194583,#194584,#194585,#194586,#194587,#194588,#194589,#194590,
#194591,#194592,#194593,#194594,#194595,#194596,#194597,#194598,#194599,
#194600,#194601,#194602,#194603,#194604,#194605,#194606,#194607,#194608,
#194609,#194610,#194611,#194612,#194613,#194614,#194615,#194616,#194617,
#194618,#194619,#194620,#194621,#194622,#194623,#194624,#194625,#194626,
#194627,#194628,#194629,#194630,#194631,#194632,#194633,#194634,#194635,
#194636,#194637,#194638,#194639,#194640,#194641,#194642,#194643,#194644,
#194645,#194646,#194647,#194648,#194649,#194650,#194651,#194652,#194653,
#194654,#194655,#194656,#194657,#194658,#194659,#194660,#194661,#194662,
#194663,#194664,#194665,#194666,#194667,#194668,#194669,#194670,#194671,
#194672,#194673,#194674,#194675,#194676,#194677,#194678,#194679,#194680,
#194681,#194682,#194683,#194684,#194685,#194686,#194687,#194688,#194689,
#194690,#194691,#194692,#194693,#194694,#194695,#194696,#194697,#194698,
#194699,#194700,#194701,#194702,#194703,#194704,#194705,#194706,#194707,
#194708,#194709,#194710,#194711,#194712,#194713,#194714,#194715,#194716,
#194717,#194718,#194719,#194720,#194721,#194722,#194723,#194724,#194725,
#194726,#194727,#194728,#194729,#194730,#194731,#194732,#194733,#194734,
#194735,#194736,#194737,#194738,#194739,#194740,#194741,#194742,#194743,
#194744,#194745,#194746,#194747,#194748,#194749,#194750,#194751,#194752,
#194753,#194754,#194755,#194756,#194757,#194758),.UNSPECIFIED.,.F.,.F.,
(4,2,2,2,2,2,2,2,2,2,2,2,2,2,2,2,2,2,2,2,2,2,2,2,2,2,2,2,2,2,2,2,2,2,2,
2,2,2,2,2,2,2,2,2,2,2,2,2,2,2,2,2,2,2,2,2,2,2,2,2,2,2,2,2,2,2,2,2,2,2,2,
2,2,2,2,2,2,2,2,2,2,2,2,2,2,2,2,2,2,2,2,2,2,2,2,2,2,2,2,2,2,2,2,2,2,2,2,
2,2,2,2,2,2,2,2,2,2,4),(1.26007673425044,1.27822034854057,1.28180703240457,
1.28331831114579,1.28441105158424,1.28543667815149,1.28717748420687,1.2918935596457,
1.33231247703275,1.33420232974193,1.37803753563163,1.3852611505755,1.38818306366884,
1.38998649676569,1.39194043723396,1.39460310102582,1.40076525819235,1.42723729776746,
1.46616241659447,1.4743072172829,1.49158433063981,1.49425345966724,1.49561158988127,
1.49668392576704,1.49793315382893,1.50017169869674,1.51090010700594,1.53460879252624,
1.56198738678538,1.593925215884,1.5981657104196,1.6006914456784,1.60263009810805,
1.60471079073515,1.60799112759627,1.61857517009446,1.63574574563707,1.68149473027648,
1.68826406879547,1.70371146986738,1.70607984863648,1.70748773331768,1.70856814014955,
1.70977190125538,1.71180428465049,1.71969762708589,1.7344197029257,1.76346395810338,
1.80585899123358,1.81015301786832,1.81269432862232,1.81463552477766,1.81670979776849,
1.81996082859284,1.83028624203308,1.84688011726286,1.87979983748303,1.89584072437233,
1.89963267018512,1.91567456110945,1.91829658453125,1.91964461961337,1.92071624670885,
1.92197305414485,1.92424637760147,1.93556052225193,1.9614898725518,2.01455864423808,
2.02144645474548,2.02431241178301,2.02610554847049,2.02806772322619,2.03077691704051,
2.0372110005296,2.06591631435643,2.11717680274213,2.12820320396987,2.13034851468667,
2.13170466851684,2.13277688686089,2.13402763747206,2.136273049107,2.14711334411419,
2.17123427606813,2.22697591490186,2.2336268322301,2.23617066276573,2.23799815152965,
2.23993690430015,2.24250767285752,2.24815647689199,2.27067646789451,2.30342178835782,
2.33947784842715,2.3423392854123,2.34371780249772,2.34479187658871,2.34602689572929,
2.34820067608323,2.35793165099402,2.40687999208181,2.44200406854333,2.44668309419899,
2.4491176244479,2.45098803547697,2.45307413470562,2.45525721240222,2.45847309220987,
2.49361008414377,2.54942123335573,2.55370206928047,2.5553750573199,2.55638754917169,
2.55749003764377,2.55905457790401,2.56296312587904,2.58213095395406,2.5939427763898),
 .UNSPECIFIED.);
#1987=B_SPLINE_CURVE_WITH_KNOTS('',3,(#194759,#194760,#194761,#194762,#194763,
#194764,#194765,#194766,#194767,#194768,#194769,#194770,#194771,#194772,
#194773,#194774,#194775,#194776,#194777,#194778,#194779,#194780,#194781,
#194782,#194783,#194784,#194785,#194786,#194787,#194788,#194789,#194790,
#194791,#194792,#194793,#194794,#194795,#194796,#194797,#194798,#194799,
#194800,#194801,#194802,#194803,#194804,#194805,#194806,#194807,#194808,
#194809,#194810,#194811,#194812,#194813,#194814,#194815,#194816,#194817,
#194818,#194819,#194820,#194821,#194822,#194823,#194824,#194825,#194826,
#194827,#194828,#194829,#194830,#194831,#194832,#194833,#194834,#194835,
#194836,#194837,#194838,#194839,#194840,#194841,#194842,#194843,#194844,
#194845,#194846,#194847,#194848,#194849,#194850,#194851,#194852,#194853,
#194854,#194855,#194856,#194857,#194858,#194859,#194860,#194861,#194862,
#194863,#194864,#194865,#194866,#194867,#194868,#194869,#194870,#194871,
#194872,#194873,#194874,#194875,#194876,#194877,#194878,#194879,#194880,
#194881,#194882,#194883,#194884,#194885,#194886,#194887,#194888,#194889,
#194890,#194891,#194892,#194893,#194894,#194895,#194896,#194897,#194898,
#194899,#194900,#194901,#194902,#194903,#194904,#194905,#194906,#194907,
#194908,#194909,#194910,#194911,#194912,#194913,#194914,#194915,#194916,
#194917,#194918,#194919,#194920,#194921,#194922,#194923,#194924,#194925,
#194926,#194927,#194928,#194929,#194930,#194931,#194932,#194933,#194934,
#194935,#194936,#194937,#194938,#194939,#194940,#194941,#194942,#194943,
#194944,#194945,#194946,#194947,#194948,#194949,#194950,#194951,#194952,
#194953,#194954,#194955,#194956,#194957,#194958,#194959,#194960,#194961,
#194962,#194963,#194964,#194965,#194966,#194967,#194968,#194969,#194970,
#194971,#194972,#194973,#194974,#194975,#194976,#194977,#194978,#194979,
#194980),.UNSPECIFIED.,.F.,.F.,(4,2,2,2,2,2,2,2,2,2,2,2,2,2,2,2,2,2,2,2,
2,2,2,2,2,2,2,2,2,2,2,2,2,2,2,2,2,2,2,2,2,2,2,2,2,2,2,2,2,2,2,2,2,2,2,2,
2,2,2,2,2,2,2,2,2,2,2,2,2,2,2,2,2,2,2,2,2,2,2,2,2,2,2,2,2,2,2,2,2,2,2,2,
2,2,2,2,2,2,2,2,2,2,2,2,2,2,2,2,2,2,4),(0.0747600637111309,0.117105823764469,
0.145108411734536,0.159869859461584,0.16347296292742,0.16566682895406,0.167580337587679,
0.169941789263497,0.173550182604974,0.190283437410746,0.199048912005449,
0.246254159454364,0.260993802292196,0.268891893502176,0.270924206361464,
0.272127675912181,0.273207653512253,0.274614744444762,0.276981280881599,
0.29239964380829,0.299150922851425,0.344056021383004,0.36175381554568,0.372570961798037,
0.375876428823309,0.377962188704936,0.379898060862263,0.382409528472346,
0.386602676660348,0.416067874415692,0.457611867419546,0.472769410626551,
0.480818684089956,0.482863929807413,0.484070292057608,0.485149560672342,
0.486551406420661,0.488899922187192,0.503878521982589,0.524489506496471,
0.557486860936813,0.580451769821037,0.58616027768988,0.588741624185283,
0.590681652017809,0.592505441437672,0.595036286062315,0.601607314702554,
0.65812356269269,0.681751986031374,0.692456895567904,0.694693709519191,
0.695942407056806,0.697014561073142,0.698372805011686,0.700525489831871,
0.711677463574072,0.762882474824384,0.791461703959685,0.797880624094858,
0.800586935681674,0.802548298428888,0.804341574969612,0.807209663694989,
0.814112460989114,0.866991338859081,0.893070554381798,0.904421271813461,
0.90669640945359,0.90795346303484,0.909024844442683,0.91037198451393,0.912990546788288,
0.928978157107934,0.929666273628093,0.973973556302938,1.0033433745717,1.0098561001038,
1.01257826128358,1.0145425861999,1.01633273495281,1.01918318927731,1.02597855199891,
1.08018858644684,1.10535322543206,1.11646879937416,1.1187303851603,1.11998453074097,
1.12105622625253,1.12240732529864,1.12504411230898,1.14147511903859,1.19206406517171,
1.20977577121625,1.22059951292097,1.22390604391618,1.2259922561474,1.2279283973344,
1.23044000045437,1.23463290643626,1.26437719762356,1.30532176334021,1.32780172822321,
1.33046518117726,1.33180403432858,1.33277202147971,1.33399564818647,1.336118192394,
1.34513699855699,1.3631223287937,1.40833130187303),.UNSPECIFIED.);
#1988=B_SPLINE_CURVE_WITH_KNOTS('',3,(#194986,#194987,#194988,#194989,#194990,
#194991),.UNSPECIFIED.,.F.,.F.,(4,2,4),(2.59391834687278,2.60763875198809,
2.66839545987335),.UNSPECIFIED.);
#1989=B_SPLINE_CURVE_WITH_KNOTS('',3,(#194992,#194993,#194994,#194995,#194996,
#194997,#194998,#194999,#195000,#195001,#195002,#195003,#195004,#195005,
#195006,#195007,#195008,#195009,#195010,#195011,#195012,#195013,#195014,
#195015,#195016,#195017,#195018,#195019,#195020,#195021,#195022,#195023,
#195024,#195025,#195026,#195027,#195028,#195029,#195030,#195031,#195032,
#195033,#195034,#195035,#195036,#195037,#195038,#195039,#195040,#195041,
#195042,#195043,#195044,#195045,#195046,#195047,#195048,#195049,#195050,
#195051,#195052,#195053,#195054,#195055,#195056,#195057,#195058,#195059,
#195060,#195061,#195062,#195063,#195064,#195065,#195066,#195067,#195068,
#195069,#195070,#195071,#195072,#195073,#195074,#195075,#195076,#195077,
#195078,#195079,#195080,#195081,#195082,#195083,#195084,#195085,#195086,
#195087,#195088,#195089,#195090,#195091,#195092,#195093,#195094,#195095,
#195096,#195097,#195098,#195099,#195100,#195101,#195102,#195103,#195104,
#195105,#195106,#195107,#195108,#195109,#195110,#195111,#195112,#195113,
#195114,#195115,#195116,#195117,#195118,#195119,#195120,#195121,#195122,
#195123,#195124,#195125,#195126,#195127,#195128,#195129,#195130,#195131,
#195132,#195133,#195134,#195135,#195136,#195137,#195138,#195139,#195140,
#195141,#195142,#195143,#195144,#195145,#195146,#195147,#195148,#195149,
#195150,#195151,#195152,#195153,#195154,#195155,#195156,#195157,#195158,
#195159,#195160,#195161,#195162,#195163,#195164,#195165,#195166,#195167,
#195168,#195169,#195170,#195171,#195172,#195173,#195174,#195175,#195176,
#195177,#195178,#195179,#195180,#195181,#195182,#195183,#195184,#195185,
#195186,#195187,#195188,#195189,#195190,#195191,#195192,#195193,#195194,
#195195,#195196,#195197,#195198,#195199,#195200,#195201,#195202,#195203,
#195204,#195205,#195206,#195207,#195208,#195209,#195210,#195211,#195212,
#195213),.UNSPECIFIED.,.F.,.F.,(4,2,2,2,2,2,2,2,2,2,2,2,2,2,2,2,2,2,2,2,
2,2,2,2,2,2,2,2,2,2,2,2,2,2,2,2,2,2,2,2,2,2,2,2,2,2,2,2,2,2,2,2,2,2,2,2,
2,2,2,2,2,2,2,2,2,2,2,2,2,2,2,2,2,2,2,2,2,2,2,2,2,2,2,2,2,2,2,2,2,2,2,2,
2,2,2,2,2,2,2,2,2,2,2,2,2,2,2,2,2,2,4),(0.0008107227228681,0.00554261242357023,
0.00881069503303161,0.0102445751035381,0.0113189839483436,0.012341800553414,
0.0133650025371135,0.014806018979062,0.0186526202746868,0.026391011620125,
0.0473065533864827,0.0988382636989564,0.111887535807851,0.115415754172655,
0.117550594294732,0.119472508732425,0.121925303839554,0.12583219147926,
0.147488757626182,0.20735969504481,0.215841010091871,0.219420204375171,
0.221354409470144,0.222628441523035,0.223822912393626,0.224866392342224,
0.226245257493794,0.229109851175418,0.264707789076383,0.297562034167569,
0.314119270433323,0.324428098518561,0.327676447986507,0.329749626993424,
0.331690233133116,0.334231398498342,0.33852661675391,0.373664432788686,
0.422637795107076,0.432353676390653,0.434526083989274,0.435760620706204,
0.436834471006619,0.438212947314881,0.441075164761016,0.476694454306604,
0.509546977118821,0.526099969467085,0.536407142453932,0.539655495914197,
0.541728803770686,0.543669619249225,0.546211186771581,0.550507371783156,
0.585691561362842,0.634807294936188,0.644362958176063,0.646524378943076,
0.647756569447583,0.648830890689694,0.650213267092093,0.652445523957233,
0.665002294744506,0.667475806801245,0.675300191938136,0.688659867077617,
0.721518942104245,0.744263466509966,0.749942701890795,0.752518902691156,
0.754458339937502,0.756283974968964,0.758821221381019,0.765431186706561,
0.821596171725762,0.845461172322981,0.856231124784658,0.858472137223952,
0.859721854892126,0.86079406678,0.862151333628002,0.864816647440531,0.881994739114714,
0.927499393522673,0.95536265623051,0.961695939243892,0.964387960957094,
0.966346978728991,0.968143657278269,0.971029336522855,0.978037101431352,
1.02938454832566,1.05655997917679,1.06818512727908,1.07047599163981,1.07173657321053,
1.07280785023142,1.07415091403497,1.07675003518382,1.09226450802658,1.09884031895341,
1.14022790278774,1.16749905800728,1.17376032302885,1.17644008028276,1.17839698127643,
1.18019645947063,1.18309710267183,1.19019423823624,1.2398344240603,1.26007673425044),
 .UNSPECIFIED.);
#1990=B_SPLINE_CURVE_WITH_KNOTS('',3,(#195215,#195216,#195217,#195218,#195219,
#195220,#195221,#195222,#195223,#195224,#195225,#195226,#195227,#195228,
#195229,#195230,#195231,#195232,#195233,#195234,#195235,#195236,#195237,
#195238,#195239,#195240,#195241,#195242,#195243,#195244,#195245,#195246,
#195247,#195248,#195249,#195250,#195251,#195252,#195253,#195254,#195255,
#195256,#195257,#195258,#195259,#195260,#195261,#195262,#195263,#195264,
#195265,#195266,#195267,#195268,#195269,#195270,#195271,#195272,#195273,
#195274,#195275,#195276,#195277,#195278,#195279,#195280,#195281,#195282,
#195283,#195284,#195285,#195286,#195287,#195288,#195289,#195290,#195291,
#195292,#195293,#195294,#195295,#195296,#195297,#195298,#195299,#195300,
#195301,#195302,#195303,#195304,#195305,#195306,#195307,#195308,#195309,
#195310,#195311,#195312,#195313,#195314,#195315,#195316,#195317,#195318,
#195319,#195320,#195321,#195322,#195323,#195324,#195325,#195326,#195327,
#195328,#195329,#195330,#195331,#195332,#195333,#195334,#195335,#195336,
#195337,#195338,#195339,#195340,#195341,#195342,#195343,#195344,#195345,
#195346,#195347,#195348,#195349,#195350,#195351,#195352,#195353,#195354,
#195355,#195356,#195357,#195358,#195359,#195360,#195361,#195362,#195363,
#195364,#195365,#195366,#195367,#195368,#195369,#195370,#195371,#195372,
#195373,#195374,#195375,#195376,#195377,#195378,#195379,#195380,#195381,
#195382,#195383,#195384,#195385,#195386,#195387,#195388,#195389,#195390,
#195391,#195392,#195393,#195394,#195395,#195396,#195397,#195398,#195399,
#195400,#195401,#195402,#195403,#195404,#195405,#195406,#195407,#195408,
#195409,#195410,#195411,#195412,#195413,#195414,#195415,#195416,#195417,
#195418,#195419,#195420,#195421,#195422,#195423,#195424,#195425,#195426,
#195427,#195428,#195429,#195430,#195431,#195432,#195433,#195434,#195435,
#195436,#195437,#195438),.UNSPECIFIED.,.F.,.F.,(4,2,2,2,2,2,2,2,2,2,2,2,
2,2,2,2,2,2,2,2,2,2,2,2,2,2,2,2,2,2,2,2,2,2,2,2,2,2,2,2,2,2,2,2,2,2,2,2,
2,2,2,2,2,2,2,2,2,2,2,2,2,2,2,2,2,2,2,2,2,2,2,2,2,2,2,2,2,2,2,2,2,2,2,2,
2,2,2,2,2,2,2,2,2,2,2,2,2,2,2,2,2,2,2,2,2,2,2,2,2,2,2,4),(1.40833130187303,
1.41333860865638,1.43114257366929,1.43482206820683,1.43720572101494,1.43912123241566,
1.44130001566784,1.44502489346626,1.46043157714509,1.51176743708484,1.53944622634268,
1.54235321148717,1.54374053731288,1.54481539303127,1.54604449533572,1.54819176899699,
1.55754757911024,1.60681363467,1.64203742354281,1.6463341375209,1.6488759594911,
1.65081692466258,1.65289034828071,1.65613878973532,1.66644537075952,1.68299888924696,
1.71588111821047,1.7293283675807,1.73691268454139,1.75191066282938,1.75426020777919,
1.75566242103971,1.75674182470983,1.75794818579049,1.75999307995436,1.76803673881456,
1.78317585486001,1.82287756918822,1.85411741708831,1.85834284408661,1.86086389521879,
1.86280145313762,1.86488342433604,1.86817097386406,1.87882380930297,1.89615077429853,
1.94435252076409,1.94864842885042,1.95112875598218,1.96407178724157,1.96632414641052,
1.96771256316774,1.96878749452924,1.97001582243435,1.97215972501833,1.98146955642855,
2.00035926908347,2.00776456608895,2.06294338563554,2.06964714341179,2.07219886232132,
2.07402821229395,2.07596544998899,2.07852829557183,2.08413575635093,2.13242239267253,
2.17281407016494,2.177527201763,2.17926736761458,2.18029273973336,2.18138531358962,
2.18289653073126,2.18648385809957,2.22413173272559,2.2745053461978,2.28156397574394,
2.28445789874098,2.2862559270563,2.28821341550438,2.29089788613927,2.29718815722413,
2.32470420092858,2.36836192529645,2.37267676935115,2.37428700871004,2.38806817866148,
2.3903620520745,2.39174794657588,2.39282523361029,2.39404096214363,2.39612794461472,
2.40468534623343,2.42129014270033,2.46980351346381,2.49084056335534,2.49471304239968,
2.49715576049242,2.49907699874299,2.50087179399015,2.50390421111817,2.51296412135939,
2.52695566757823,2.55048381538279,2.59701886873766,2.6015925093705,2.60331145398766,
2.60433267489801,2.60542800132095,2.60695482500546,2.6106345351413,2.62772793363314,
2.66748530878275),.UNSPECIFIED.);
#1991=B_SPLINE_CURVE_WITH_KNOTS('',3,(#195439,#195440,#195441,#195442,#195443,
#195444,#195445,#195446,#195447,#195448,#195449,#195450,#195451,#195452,
#195453,#195454,#195455,#195456,#195457,#195458),.UNSPECIFIED.,.F.,.F.,
(4,2,2,2,2,2,2,2,2,4),(0.00070417545084543,0.0257174469115552,0.0359847153183718,
0.0390634835596431,0.0411897982603028,0.0432709612661059,0.0452083174595604,
0.0477298916634498,0.0519579623696429,0.0751489416222558),.UNSPECIFIED.);
#1992=B_SPLINE_CURVE_WITH_KNOTS('',3,(#195463,#195464,#195465,#195466,#195467,
#195468,#195469,#195470,#195471,#195472,#195473,#195474,#195475,#195476,
#195477,#195478,#195479,#195480,#195481,#195482,#195483,#195484,#195485,
#195486,#195487,#195488,#195489,#195490,#195491,#195492,#195493,#195494,
#195495,#195496,#195497,#195498,#195499,#195500,#195501,#195502,#195503,
#195504,#195505,#195506,#195507,#195508,#195509,#195510,#195511,#195512,
#195513,#195514,#195515,#195516,#195517,#195518,#195519,#195520,#195521,
#195522,#195523,#195524,#195525,#195526,#195527,#195528,#195529,#195530,
#195531,#195532,#195533,#195534,#195535,#195536,#195537,#195538,#195539,
#195540,#195541,#195542,#195543,#195544,#195545,#195546,#195547,#195548,
#195549,#195550,#195551,#195552,#195553,#195554,#195555,#195556,#195557,
#195558,#195559,#195560,#195561,#195562,#195563,#195564,#195565,#195566,
#195567,#195568,#195569,#195570,#195571,#195572,#195573,#195574,#195575,
#195576,#195577,#195578,#195579,#195580,#195581,#195582,#195583,#195584,
#195585,#195586,#195587,#195588,#195589,#195590,#195591,#195592,#195593,
#195594,#195595,#195596,#195597,#195598,#195599,#195600,#195601,#195602,
#195603,#195604,#195605,#195606,#195607,#195608,#195609,#195610,#195611,
#195612,#195613,#195614,#195615,#195616,#195617,#195618,#195619,#195620,
#195621,#195622,#195623,#195624,#195625,#195626,#195627,#195628,#195629,
#195630,#195631,#195632,#195633,#195634,#195635,#195636,#195637,#195638,
#195639,#195640,#195641,#195642,#195643,#195644,#195645,#195646,#195647,
#195648,#195649,#195650,#195651,#195652,#195653,#195654,#195655,#195656,
#195657,#195658,#195659,#195660,#195661,#195662,#195663,#195664,#195665,
#195666,#195667,#195668,#195669,#195670,#195671,#195672,#195673,#195674,
#195675,#195676,#195677,#195678,#195679,#195680,#195681,#195682,#195683,
#195684,#195685,#195686,#195687,#195688,#195689,#195690,#195691,#195692,
#195693,#195694,#195695,#195696,#195697,#195698,#195699,#195700,#195701,
#195702,#195703,#195704,#195705,#195706,#195707,#195708,#195709,#195710,
#195711,#195712,#195713,#195714,#195715,#195716,#195717,#195718,#195719,
#195720),.UNSPECIFIED.,.F.,.F.,(4,2,2,2,2,2,2,2,2,2,2,2,2,2,2,2,2,2,2,2,
2,2,2,2,2,2,2,2,2,2,2,2,2,2,2,2,2,2,2,2,2,2,2,2,2,2,2,2,2,2,2,2,2,2,2,2,
2,2,2,2,2,2,2,2,2,2,2,2,2,2,2,2,2,2,2,2,2,2,2,2,2,2,2,2,2,2,2,2,2,2,2,2,
2,2,2,2,2,2,2,2,2,2,2,2,2,2,2,2,2,2,2,2,2,2,2,2,2,2,2,2,2,2,2,2,2,2,2,2,
4),(1.2601389384112,1.26848571120951,1.29386306512029,1.2981337923634,1.30043133727047,
1.30232441885463,1.30456517505604,1.30846435779437,1.32437313367788,1.3345954363477,
1.37388000634629,1.40246435856348,1.40537692931074,1.40676548712629,1.40784063687077,
1.40906933645133,1.41121417390558,1.42053249098821,1.46970919683015,1.50507853084996,
1.50937773010662,1.51192050377761,1.51386189718617,1.51593548897102,1.51918359014323,
1.52948400804535,1.54602279695485,1.57356972315891,1.5897128114394,1.60079553270927,
1.61502899303413,1.61734549874146,1.61873815321135,1.61981643147212,1.62102850393194,
1.6230985254543,1.63144219898204,1.64742714650239,1.68974320820639,1.71735462586705,
1.72149220266191,1.72398775480773,1.72592162430201,1.72801543909652,1.73135567996895,
1.74248821906649,1.76091190748415,1.8076851920583,1.81240084874524,1.82701499017415,
1.8293486927043,1.83074640602968,1.83182536946033,1.83303460775215,1.83509180229052,
1.84327911877606,1.85881939573537,1.90032284238502,1.90898218140034,1.92987234476664,
1.93373698633006,1.93617756852023,1.93809889334153,1.94024238244839,1.94380667224902,
1.9572455905208,2.00851502522241,2.03853791306167,2.04145317401922,2.04284224972012,
2.04391744859541,2.04514581085012,2.04728913803729,2.05658666094371,2.07543536632353,
2.11584208852909,2.12810600527748,2.14271919054542,2.14650863200771,2.14872416546594,
2.15063681173404,2.15297221032833,2.15742251698649,2.18832193837449,2.23500482746476,
2.25098959188883,2.25360846515385,2.25495588708897,2.25602755630807,2.25728502709826,
2.25956111160132,2.27092105265357,2.29702895963914,2.34984912367748,2.35675668707532,
2.35962603713395,2.36141989626524,2.36338173658721,2.36608840694338,2.37250674280563,
2.40107789247664,2.44548993980825,2.4629725876277,2.46564626818871,2.46700542908534,
2.46804717172061,2.46805121058445,2.46805518170384,2.46805908643056,2.46806269178163,
2.46806628367417,2.46806986207604,2.46807342706223,2.46807697897155,2.46930022720019,
2.47061092653101,2.47263307888466,2.47644326979725,2.48570770035342,2.52349861205201,
2.53472391591848,2.56538710396664,2.56960118010839,2.57211933555201,2.5740569329087,
2.57614117350816,2.57943703814588,2.59015860341032,2.59391834687278),
 .UNSPECIFIED.);
#1993=B_SPLINE_CURVE_WITH_KNOTS('',3,(#195721,#195722,#195723,#195724,#195725,
#195726,#195727,#195728,#195729,#195730,#195731,#195732,#195733,#195734,
#195735,#195736,#195737,#195738,#195739,#195740,#195741,#195742,#195743,
#195744,#195745,#195746,#195747,#195748,#195749,#195750,#195751,#195752,
#195753,#195754,#195755,#195756,#195757,#195758,#195759,#195760,#195761,
#195762,#195763,#195764,#195765,#195766,#195767,#195768,#195769,#195770,
#195771,#195772,#195773,#195774,#195775,#195776,#195777,#195778,#195779,
#195780,#195781,#195782,#195783,#195784,#195785,#195786,#195787,#195788,
#195789,#195790,#195791,#195792,#195793,#195794,#195795,#195796,#195797,
#195798,#195799,#195800,#195801,#195802,#195803,#195804,#195805,#195806,
#195807,#195808,#195809,#195810,#195811,#195812,#195813,#195814,#195815,
#195816,#195817,#195818,#195819,#195820,#195821,#195822,#195823,#195824,
#195825,#195826,#195827,#195828,#195829,#195830,#195831,#195832,#195833,
#195834,#195835,#195836,#195837,#195838,#195839,#195840,#195841,#195842,
#195843,#195844,#195845,#195846,#195847,#195848,#195849,#195850,#195851,
#195852,#195853,#195854,#195855,#195856,#195857,#195858,#195859,#195860,
#195861,#195862,#195863,#195864,#195865,#195866,#195867,#195868,#195869,
#195870,#195871,#195872,#195873,#195874,#195875,#195876,#195877,#195878,
#195879,#195880,#195881,#195882,#195883,#195884,#195885,#195886,#195887,
#195888,#195889,#195890,#195891,#195892,#195893,#195894,#195895,#195896,
#195897,#195898,#195899,#195900,#195901,#195902,#195903,#195904,#195905,
#195906,#195907,#195908,#195909,#195910,#195911,#195912,#195913,#195914,
#195915,#195916,#195917,#195918,#195919,#195920,#195921,#195922,#195923,
#195924,#195925,#195926,#195927,#195928,#195929,#195930,#195931,#195932,
#195933,#195934,#195935,#195936,#195937,#195938,#195939,#195940,#195941,
#195942,#195943,#195944,#195945,#195946,#195947,#195948,#195949,#195950),
 .UNSPECIFIED.,.F.,.F.,(4,2,2,2,2,2,2,2,2,2,2,2,2,2,2,2,2,2,2,2,2,2,2,2,
2,2,2,2,2,2,2,2,2,2,2,2,2,2,2,2,2,2,2,2,2,2,2,2,2,2,2,2,2,2,2,2,2,2,2,2,
2,2,2,2,2,2,2,2,2,2,2,2,2,2,2,2,2,2,2,2,2,2,2,2,2,2,2,2,2,2,2,2,2,2,2,2,
2,2,2,2,2,2,2,2,2,2,2,2,2,2,2,2,2,2,4),(0.0751489416222558,0.0833456594865257,
0.10864754221125,0.136459750324486,0.145891457113087,0.148043769077378,
0.149273773130638,0.150348135853102,0.151733127922358,0.153974632457574,
0.166714949664848,0.188867173562766,0.21569261338959,0.23708058275434,0.245243765604029,
0.251221974994586,0.253843628386387,0.255799191562491,0.257598929644745,
0.260503294718212,0.267626112344298,0.316798134455025,0.355579236560289,
0.359167498122403,0.360678743855942,0.36177120001151,0.362796352525048,
0.36453591197414,0.369246038175862,0.409869321215986,0.456725005652046,
0.463118173385777,0.46581994484496,0.467780320578642,0.469574283108175,
0.472446934110405,0.47937864805976,0.531838843734116,0.558205065453623,
0.569627770358348,0.571906827484897,0.573164645626753,0.574235830387382,
0.575581644921237,0.578194468266733,0.59405289917602,0.598851304524438,
0.614070411229687,0.646945788474424,0.663526847683016,0.67384665322596,
0.677096411766376,0.679169997864278,0.681110639415376,0.683651352568231,
0.687944689278822,0.730339610113684,0.759386513383232,0.774118595635768,
0.782014101378475,0.784046281633098,0.785249771881767,0.78632983731581,
0.787737133559872,0.790104209803694,0.805533296041103,0.812266491300551,
0.826057518178759,0.858918039330953,0.875480171901036,0.885791541513573,
0.889040422040249,0.891113875162427,0.893054692357583,0.895596068400749,
0.899891495514801,0.935011543440762,0.983923408155616,0.993719891617363,
0.995897993119582,0.997133869170045,0.99820767091787,0.999584499228307,
1.00243783889395,1.02512028941744,1.03806346126668,1.070919155012,1.08747301926967,
1.09778094744985,1.10102965193598,1.10310321100586,1.10504428073002,1.10758620873773,
1.11188306484463,1.14708111471412,1.19623407094332,1.20575511777427,1.20791429692606,
1.2091460906737,1.21022063540107,1.2116040472708,1.21383943927351,1.22645184678908,
1.23297894613478,1.23811133127399,1.27817432782865,1.30767815269563,1.31208857522361,
1.31441550912619,1.31614260230727,1.31829903753282,1.321921874469,1.33437263889487,
1.38533348213424,1.40863530833717),.UNSPECIFIED.);
#1994=B_SPLINE_CURVE_WITH_KNOTS('',3,(#195956,#195957,#195958,#195959,#195960,
#195961,#195962,#195963,#195964,#195965),.UNSPECIFIED.,.F.,.F.,(4,2,2,2,
4),(2.59328305732938,2.5941665037565,2.60558384395807,2.63192422606051,
2.66742998661749),.UNSPECIFIED.);
#1995=B_SPLINE_CURVE_WITH_KNOTS('',3,(#195966,#195967,#195968,#195969,#195970,
#195971,#195972,#195973,#195974,#195975,#195976,#195977,#195978,#195979,
#195980,#195981,#195982,#195983,#195984,#195985,#195986,#195987,#195988,
#195989,#195990,#195991,#195992,#195993,#195994,#195995,#195996,#195997,
#195998,#195999,#196000,#196001,#196002,#196003,#196004,#196005,#196006,
#196007,#196008,#196009,#196010,#196011,#196012,#196013,#196014,#196015,
#196016,#196017,#196018,#196019,#196020,#196021,#196022,#196023,#196024,
#196025,#196026,#196027,#196028,#196029,#196030,#196031,#196032,#196033,
#196034,#196035,#196036,#196037,#196038,#196039,#196040,#196041,#196042,
#196043,#196044,#196045,#196046,#196047,#196048,#196049,#196050,#196051,
#196052,#196053,#196054,#196055,#196056,#196057,#196058,#196059,#196060,
#196061,#196062,#196063,#196064,#196065,#196066,#196067,#196068,#196069,
#196070,#196071,#196072,#196073,#196074,#196075,#196076,#196077,#196078,
#196079,#196080,#196081,#196082,#196083,#196084,#196085,#196086,#196087,
#196088,#196089,#196090,#196091,#196092,#196093,#196094,#196095,#196096,
#196097,#196098,#196099,#196100,#196101,#196102,#196103,#196104,#196105,
#196106,#196107,#196108,#196109,#196110,#196111,#196112,#196113,#196114,
#196115,#196116,#196117,#196118,#196119,#196120,#196121,#196122,#196123,
#196124,#196125,#196126,#196127,#196128,#196129,#196130,#196131,#196132,
#196133,#196134,#196135,#196136,#196137,#196138,#196139,#196140,#196141,
#196142,#196143,#196144,#196145,#196146,#196147,#196148,#196149,#196150,
#196151,#196152,#196153,#196154,#196155,#196156,#196157,#196158,#196159,
#196160,#196161,#196162,#196163,#196164,#196165,#196166,#196167,#196168,
#196169,#196170,#196171,#196172,#196173,#196174,#196175,#196176,#196177,
#196178,#196179,#196180,#196181,#196182,#196183,#196184,#196185,#196186,
#196187,#196188,#196189),.UNSPECIFIED.,.F.,.F.,(4,2,2,2,2,2,2,2,2,2,2,2,
2,2,2,2,2,2,2,2,2,2,2,2,2,2,2,2,2,2,2,2,2,2,2,2,2,2,2,2,2,2,2,2,2,2,2,2,
2,2,2,2,2,2,2,2,2,2,2,2,2,2,2,2,2,2,2,2,2,2,2,2,2,2,2,2,2,2,2,2,2,2,2,2,
2,2,2,2,2,2,2,2,2,2,2,2,2,2,2,2,2,2,2,2,2,2,2,2,2,2,2,4),(0.000768639498582023,
0.0217315272484726,0.0248344558655061,0.0269706893309883,0.0287699211802129,
0.0306851237252918,0.0330691911455451,0.0367508647498313,0.0545962054436122,
0.0730123204296272,0.121983893617493,0.131697533992236,0.133869690408933,
0.13510412307762,0.136177907691802,0.137556332154594,0.140418553991821,
0.17638729847915,0.209115490703129,0.225520420771702,0.232323419581674,
0.237498350490654,0.239967785147863,0.241807161787133,0.243631769465946,
0.246165868724782,0.25275760261694,0.309057718971785,0.332826434072779,
0.343569477766903,0.345808576049655,0.347057746247984,0.348129809803604,
0.349487301641194,0.351637596511629,0.362751428367892,0.413981553905409,
0.442572966181543,0.448993238362901,0.451699723192618,0.4536610672632,0.455454227428409,
0.458321913792698,0.465222622597656,0.518120530857191,0.544184625364757,
0.555531343195069,0.557806196561707,0.559063162439451,0.560134511170677,
0.56148166368482,0.56410040741,0.580092334180435,0.585074834321935,0.629895188471682,
0.648410768165046,0.659583411777325,0.662927535039469,0.665021966225238,
0.666955169792683,0.66944813535519,0.673577712389402,0.700891800706749,
0.743167029156377,0.759423241930254,0.767859946964166,0.769937280659886,
0.771150850592922,0.772228576249864,0.773618063844585,0.77592417791237,
0.789959189497695,0.791306288115643,0.798317156209952,0.811992946079054,
0.844854116707176,0.861415741952725,0.871727039809902,0.874976027613441,
0.877049580407818,0.878990512820406,0.88153207136188,0.885827877823962,
0.920960383050237,0.969907041110738,0.97966606817553,0.98184169548107,0.983077070104677,
0.984151013877942,0.985528779446391,0.988386659169844,1.01124636969443,
1.02401225745664,1.05686816352699,1.07342098760334,1.083728603505,1.08697738816565,
1.0890510413373,1.09099222931086,1.09353435569534,1.09783164470785,1.13304652148973,
1.18225211388281,1.19171617632965,1.19387141268155,1.19510238047612,1.19617712643471,
1.19756200941938,1.19980215413631,1.21250356894832,1.23488141388171,1.2601389384112),
 .UNSPECIFIED.);
#1996=B_SPLINE_CURVE_WITH_KNOTS('',3,(#196191,#196192,#196193,#196194,#196195,
#196196,#196197,#196198,#196199,#196200,#196201,#196202,#196203,#196204,
#196205,#196206,#196207,#196208,#196209,#196210,#196211,#196212,#196213,
#196214,#196215,#196216,#196217,#196218,#196219,#196220,#196221,#196222,
#196223,#196224,#196225,#196226,#196227,#196228,#196229,#196230,#196231,
#196232,#196233,#196234,#196235,#196236,#196237,#196238,#196239,#196240,
#196241,#196242,#196243,#196244,#196245,#196246,#196247,#196248,#196249,
#196250,#196251,#196252,#196253,#196254,#196255,#196256,#196257,#196258,
#196259,#196260,#196261,#196262,#196263,#196264,#196265,#196266,#196267,
#196268,#196269,#196270,#196271,#196272,#196273,#196274,#196275,#196276,
#196277,#196278,#196279,#196280,#196281,#196282,#196283,#196284,#196285,
#196286,#196287,#196288,#196289,#196290,#196291,#196292,#196293,#196294,
#196295,#196296,#196297,#196298,#196299,#196300,#196301,#196302,#196303,
#196304,#196305,#196306,#196307,#196308,#196309,#196310,#196311,#196312,
#196313,#196314,#196315,#196316,#196317,#196318,#196319,#196320,#196321,
#196322,#196323,#196324,#196325,#196326,#196327,#196328,#196329,#196330,
#196331,#196332,#196333,#196334,#196335,#196336,#196337,#196338,#196339,
#196340,#196341,#196342,#196343,#196344,#196345,#196346,#196347,#196348,
#196349,#196350,#196351,#196352,#196353,#196354,#196355,#196356,#196357,
#196358,#196359,#196360,#196361,#196362,#196363,#196364,#196365,#196366,
#196367,#196368,#196369,#196370,#196371,#196372,#196373,#196374,#196375,
#196376,#196377,#196378,#196379,#196380,#196381,#196382,#196383,#196384,
#196385,#196386,#196387,#196388,#196389,#196390,#196391,#196392,#196393,
#196394,#196395,#196396,#196397,#196398,#196399,#196400,#196401,#196402,
#196403,#196404,#196405,#196406,#196407,#196408),.UNSPECIFIED.,.F.,.F.,
(4,2,2,2,2,2,2,2,2,2,2,2,2,2,2,2,2,2,2,2,2,2,2,2,2,2,2,2,2,2,2,2,2,2,2,
2,2,2,2,2,2,2,2,2,2,2,2,2,2,2,2,2,2,2,2,2,2,2,2,2,2,2,2,2,2,2,2,2,2,2,2,
2,2,2,2,2,2,2,2,2,2,2,2,2,2,2,2,2,2,2,2,2,2,2,2,2,2,2,2,2,2,2,2,2,2,2,2,
2,4),(1.40863530833717,1.41654327343824,1.41945645940367,1.42084511671204,
1.42192025425947,1.42314884008716,1.42529324511845,1.43460606655398,1.48376512633104,
1.51915552835373,1.52345488524099,1.52599767313947,1.52793903193626,1.53001254268434,
1.53326042496439,1.54355937485508,1.56009507147325,1.59296542620313,1.6044920513517,
1.61424439728623,1.61613908864028,1.62921366902091,1.63147290717544,1.63286347558798,
1.63393874585811,1.6351659789608,1.63730450730202,1.64653781557121,1.6651859669194,
1.70931649426577,1.73179166900342,1.73573551362933,1.73820005947526,1.74012407025685,
1.74225396332416,1.74575722135842,1.75852419286517,1.78094207404634,1.81740719247911,
1.84064309321391,1.84350353440371,1.84488182184277,1.84595583435793,1.84719091509848,
1.84936512010164,1.85910320012664,1.90804312104045,1.943169257887,1.9474649539807,
1.95000656307348,1.95194758987745,1.95402129669984,1.95727063569175,1.96758388959959,
1.98415176478964,2.01704714078391,2.05265713538824,2.05552123552805,2.05690021147769,
2.0579742567883,2.05920880723788,2.0613807232419,2.07108629227125,2.12005175519484,
2.15518541461582,2.15948107319897,2.16202262533062,2.16396358860998,2.16603720815051,
2.16928636983893,2.17959871921695,2.19616481611943,2.22905803412187,2.2646664616157,
2.26753247890526,2.26891180148466,2.2699858468023,2.27122009294505,2.2733907480846,
2.28307881002717,2.33205711820898,2.36719417910864,2.37148974556877,2.37403122479423,
2.37597212179823,2.37804566025863,2.38129467344734,2.39160637063835,2.40817124775688,
2.47080847239665,2.47216976513443,2.47834307322888,2.48028134707058,2.48146408844023,
2.48249570117241,2.48390870028928,2.48692358285226,2.49102152766931,2.50129931076411,
2.52412040595402,2.57582987066577,2.58281333893934,2.58569505666905,2.58749105932933,
2.5894507754562,2.59214636207253,2.5985001675002,2.62653592440016,2.66822463298926),
 .UNSPECIFIED.);
#1997=B_SPLINE_CURVE_WITH_KNOTS('',3,(#196409,#196410,#196411,#196412,#196413,
#196414,#196415,#196416,#196417,#196418,#196419,#196420,#196421),
 .UNSPECIFIED.,.F.,.F.,(4,3,3,3,4),(-48.1740290551459,-48.0708042001896,
-47.9674104512405,-47.94414959817,-47.8233361836797),.UNSPECIFIED.);
#1998=B_SPLINE_CURVE_WITH_KNOTS('',3,(#196426,#196427,#196428,#196429,#196430,
#196431,#196432,#196433,#196434,#196435,#196436,#196437,#196438,#196439,
#196440,#196441,#196442,#196443,#196444,#196445,#196446,#196447,#196448,
#196449,#196450,#196451,#196452,#196453,#196454,#196455,#196456,#196457,
#196458,#196459,#196460,#196461,#196462,#196463,#196464,#196465,#196466,
#196467,#196468,#196469,#196470,#196471,#196472,#196473,#196474,#196475,
#196476,#196477,#196478,#196479,#196480,#196481,#196482,#196483,#196484,
#196485,#196486,#196487,#196488,#196489,#196490,#196491,#196492,#196493,
#196494,#196495,#196496,#196497,#196498,#196499,#196500,#196501,#196502,
#196503,#196504,#196505,#196506,#196507,#196508,#196509,#196510,#196511,
#196512,#196513,#196514,#196515,#196516,#196517,#196518,#196519,#196520,
#196521,#196522,#196523,#196524,#196525,#196526,#196527,#196528,#196529,
#196530,#196531,#196532,#196533,#196534,#196535,#196536,#196537,#196538,
#196539,#196540,#196541,#196542,#196543,#196544,#196545,#196546,#196547,
#196548,#196549,#196550,#196551,#196552,#196553,#196554,#196555,#196556,
#196557,#196558,#196559,#196560,#196561,#196562,#196563,#196564,#196565,
#196566,#196567,#196568,#196569,#196570,#196571,#196572,#196573,#196574,
#196575,#196576,#196577,#196578,#196579,#196580,#196581,#196582,#196583,
#196584,#196585,#196586,#196587,#196588,#196589,#196590,#196591,#196592,
#196593,#196594,#196595,#196596,#196597,#196598,#196599,#196600,#196601,
#196602,#196603,#196604,#196605,#196606,#196607,#196608,#196609,#196610,
#196611,#196612,#196613,#196614,#196615,#196616,#196617,#196618,#196619,
#196620,#196621,#196622,#196623,#196624,#196625,#196626,#196627,#196628,
#196629,#196630,#196631,#196632,#196633,#196634,#196635,#196636,#196637,
#196638,#196639,#196640,#196641,#196642,#196643,#196644,#196645,#196646,
#196647,#196648,#196649,#196650,#196651,#196652,#196653,#196654,#196655,
#196656,#196657,#196658,#196659,#196660,#196661,#196662,#196663,#196664,
#196665,#196666,#196667,#196668,#196669,#196670,#196671,#196672,#196673,
#196674,#196675,#196676,#196677,#196678,#196679,#196680,#196681,#196682,
#196683,#196684,#196685,#196686,#196687,#196688,#196689,#196690,#196691,
#196692,#196693,#196694,#196695,#196696,#196697,#196698,#196699,#196700,
#196701,#196702,#196703,#196704,#196705,#196706,#196707),.UNSPECIFIED.,
 .F.,.F.,(4,2,2,2,2,2,2,2,2,2,2,2,2,2,2,2,2,2,2,2,2,2,2,2,2,2,2,2,2,2,2,
2,2,2,2,2,2,2,2,2,2,2,2,2,2,2,2,2,2,2,2,2,2,2,2,2,2,2,2,2,2,2,2,2,2,2,2,
2,2,2,2,2,2,2,2,2,2,2,2,2,2,2,2,2,2,2,2,2,2,2,2,2,2,2,2,2,2,2,2,2,2,2,2,
2,2,2,2,2,2,2,2,2,2,2,2,2,2,2,2,2,2,2,2,2,2,2,2,2,2,2,2,2,2,2,2,2,2,2,2,
2,4),(1.2596833809502,1.28150384854047,1.30395451750715,1.31433173993329,
1.31654814463258,1.31779243049033,1.31886515460167,1.32022974891393,1.32240315902596,
1.33389986010932,1.38263545242697,1.41583873271762,1.42010258685452,1.42263487810839,
1.42457429853268,1.4266516537708,1.42991796447472,1.4403810261871,1.45728197958185,
1.49511045407783,1.52518586637426,1.52810045783411,1.52948923455204,1.53056421121483,
1.53179232990309,1.53393525621241,1.5432314121433,1.56207795393584,1.60247842875927,
1.61474052283203,1.62934635935748,1.63313463700421,1.63534962658737,1.63726188590197,
1.63959691581375,1.64404683916555,1.67495958082077,1.72180660270239,1.73760391223777,
1.74021639403696,1.74156227823741,1.74263364756808,1.74389183792505,1.74617195567225,
1.75760856869607,1.78402410843133,1.83638767113452,1.84332611747916,1.84620019751758,
1.84799465751142,1.84995526625725,1.85265678342283,1.8590466266238,1.88738482047263,
1.93728396907904,1.94991440563756,1.9521506881435,1.95353432145482,1.95460883066996,
1.955840359522,1.95799853019891,1.9675067846179,2.0166417589585,2.05182800437473,
2.05612436550452,2.05866612786458,2.06060713338944,2.06268068336504,2.06592949658284,
2.0762387215821,2.09279787942866,2.12568542647966,2.13955087604799,2.1461149157402,
2.16166397004852,2.16426435912158,2.1656075900694,2.16667874135438,2.1679388788144,
2.17022816615922,2.18182952175351,2.20890852853831,2.26033590383901,2.26733483524746,
2.27021881904326,2.27201501848728,2.27397397952619,2.27666676255737,2.28300572936343,
2.31092287826035,2.35692108319348,2.35819339220091,2.37368534805368,2.37628329366009,
2.37762599359105,2.37869710933368,2.3799576565317,2.38224884747986,2.39388454785365,
2.42110341098997,2.44129017406253,2.47581019414818,2.48009734153408,2.48263641752228,
2.48457696573734,2.48466516121913,2.48471829642163,2.48475072620655,2.48479303665328,
2.48483143129011,2.48486632749208,2.48489808952065,2.48492703666271,2.4849534516183,
2.48497758299186,2.48499965097878,2.48501985112025,2.48503835757562,2.4850553259572,
2.48507089555338,2.48509352481743,2.48511573443406,2.48513753572401,2.48515894352915,
2.48517997050377,2.48520062880447,2.48522093010883,2.48747137199418,2.49155610432155,
2.49664786551223,2.50755454423486,2.53220185164321,2.55229775944963,2.56494070528658,
2.56972246127871,2.58559872972517,2.58821236335305,2.58955843526454,2.59062974008095,
2.59188760638825,2.59328305732938),.UNSPECIFIED.);
#1999=B_SPLINE_CURVE_WITH_KNOTS('',3,(#196709,#196710,#196711,#196712,#196713,
#196714,#196715,#196716,#196717,#196718,#196719,#196720,#196721,#196722,
#196723,#196724,#196725,#196726,#196727,#196728,#196729,#196730,#196731,
#196732,#196733,#196734,#196735,#196736,#196737,#196738,#196739,#196740,
#196741,#196742,#196743,#196744,#196745,#196746,#196747,#196748,#196749,
#196750,#196751,#196752,#196753,#196754,#196755,#196756,#196757,#196758,
#196759,#196760,#196761,#196762,#196763,#196764,#196765,#196766,#196767,
#196768,#196769,#196770,#196771,#196772,#196773,#196774,#196775,#196776,
#196777,#196778,#196779,#196780,#196781,#196782,#196783,#196784,#196785,
#196786,#196787,#196788,#196789,#196790,#196791,#196792,#196793,#196794,
#196795,#196796,#196797,#196798,#196799,#196800,#196801,#196802,#196803,
#196804,#196805,#196806,#196807,#196808,#196809,#196810,#196811,#196812,
#196813,#196814,#196815,#196816,#196817,#196818,#196819,#196820,#196821,
#196822,#196823,#196824,#196825,#196826,#196827,#196828,#196829,#196830,
#196831,#196832,#196833,#196834,#196835,#196836,#196837,#196838,#196839,
#196840,#196841,#196842,#196843,#196844,#196845,#196846,#196847,#196848,
#196849,#196850,#196851,#196852,#196853,#196854,#196855,#196856,#196857,
#196858,#196859,#196860,#196861,#196862,#196863,#196864,#196865,#196866,
#196867,#196868,#196869,#196870,#196871,#196872,#196873,#196874,#196875,
#196876,#196877,#196878,#196879,#196880,#196881,#196882,#196883,#196884,
#196885,#196886),.UNSPECIFIED.,.F.,.F.,(4,3,3,3,3,3,3,3,3,3,3,3,3,3,3,3,
3,3,3,3,3,3,3,3,3,3,3,3,3,3,3,3,3,3,3,3,3,3,3,3,3,3,3,3,3,3,3,3,3,3,3,3,
3,3,3,3,3,3,3,4),(-54.1065214908593,-53.9371682979412,-53.8337735608932,
-53.7305322787781,-53.6274123133858,-53.5243577451767,-53.4213345368189,
-53.3183086941464,-53.2151759273682,-53.1119868359583,-53.0086148425766,
-52.9383318479793,-52.8349371109314,-52.7316958288165,-52.6285758634242,
-52.5255212952153,-52.4224980868577,-52.3194722441852,-52.2163394774072,
-52.1131503859974,-52.0097783926158,-51.9394953980175,-51.8361006609696,
-51.7328593788546,-51.6297394134623,-51.5266848452534,-51.4236616368957,
-51.3206357942231,-51.2175030274451,-51.1143139360353,-51.0109419426537,
-50.9406589480556,-50.8372642110076,-50.7340229288926,-50.6309029635003,
-50.5278483952914,-50.4248251869336,-50.3217993442611,-50.218666577483,
-50.1154774860732,-50.0121054926915,-49.9418224980937,-49.8384277610457,
-49.7351864789307,-49.6320665135383,-49.5290119453294,-49.4259887369716,
-49.322962894299,-49.2198301275209,-49.1166410361111,-49.0132690427294,
-48.9429860481318,-48.8396205066934,-48.7363953136927,-48.6332762150873,
-48.530229079458,-48.4271932051592,-48.3241646395798,-48.2210652727916,
-48.1740290551459),.UNSPECIFIED.);
#2000=B_SPLINE_CURVE_WITH_KNOTS('',3,(#196887,#196888,#196889,#196890),
 .UNSPECIFIED.,.F.,.F.,(4,4),(-54.4565130710325,-54.1065275202913),
 .UNSPECIFIED.);
#2001=B_SPLINE_CURVE_WITH_KNOTS('',3,(#196896,#196897,#196898,#196899,#196900,
#196901,#196902,#196903,#196904,#196905,#196906,#196907,#196908,#196909,
#196910,#196911,#196912,#196913,#196914,#196915),.UNSPECIFIED.,.F.,.F.,
(4,2,2,2,2,2,2,2,2,4),(2.59294800260859,2.59867319176495,2.60292963635251,
2.60545927305944,2.60739767247906,2.60947492156612,2.61274314334304,2.61654582757013,
2.62380936125772,2.66743053820994),.UNSPECIFIED.);
#2002=B_SPLINE_CURVE_WITH_KNOTS('',3,(#196916,#196917,#196918,#196919,#196920,
#196921,#196922,#196923,#196924,#196925,#196926,#196927,#196928,#196929,
#196930,#196931,#196932,#196933,#196934,#196935,#196936,#196937,#196938,
#196939,#196940,#196941,#196942,#196943,#196944,#196945,#196946,#196947,
#196948,#196949,#196950,#196951,#196952,#196953,#196954,#196955,#196956,
#196957,#196958,#196959,#196960,#196961,#196962,#196963,#196964,#196965,
#196966,#196967,#196968,#196969,#196970,#196971,#196972,#196973,#196974,
#196975,#196976,#196977,#196978,#196979,#196980,#196981,#196982,#196983,
#196984,#196985,#196986,#196987,#196988,#196989,#196990,#196991,#196992,
#196993,#196994,#196995,#196996,#196997,#196998,#196999,#197000,#197001,
#197002,#197003,#197004,#197005,#197006,#197007,#197008,#197009,#197010,
#197011,#197012,#197013,#197014,#197015,#197016,#197017,#197018,#197019,
#197020,#197021,#197022,#197023,#197024,#197025,#197026,#197027,#197028,
#197029,#197030,#197031,#197032,#197033,#197034,#197035,#197036,#197037,
#197038,#197039,#197040,#197041,#197042,#197043,#197044,#197045,#197046,
#197047,#197048,#197049,#197050,#197051,#197052,#197053,#197054,#197055,
#197056,#197057,#197058,#197059,#197060,#197061,#197062,#197063,#197064,
#197065,#197066,#197067,#197068,#197069,#197070,#197071,#197072,#197073,
#197074,#197075,#197076,#197077,#197078,#197079,#197080,#197081,#197082,
#197083,#197084,#197085,#197086,#197087,#197088,#197089,#197090,#197091,
#197092,#197093,#197094,#197095,#197096,#197097,#197098,#197099,#197100,
#197101,#197102,#197103,#197104,#197105,#197106,#197107,#197108,#197109,
#197110,#197111,#197112,#197113,#197114,#197115,#197116,#197117,#197118,
#197119,#197120,#197121,#197122,#197123,#197124,#197125,#197126,#197127,
#197128,#197129),.UNSPECIFIED.,.F.,.F.,(4,2,2,2,2,2,2,2,2,2,2,2,2,2,2,2,
2,2,2,2,2,2,2,2,2,2,2,2,2,2,2,2,2,2,2,2,2,2,2,2,2,2,2,2,2,2,2,2,2,2,2,2,
2,2,2,2,2,2,2,2,2,2,2,2,2,2,2,2,2,2,2,2,2,2,2,2,2,2,2,2,2,2,2,2,2,2,2,2,
2,2,2,2,2,2,2,2,2,2,2,2,2,2,2,2,2,2,4),(0.000649992353746962,0.0375152730307587,
0.0412926058670708,0.0433020332466888,0.0446072148554326,0.0458444184253734,
0.0469177310104482,0.0482917902236038,0.0511320589090229,0.0879797077658783,
0.109399199895957,0.136182386948439,0.146436084907939,0.149706952573172,
0.151785042804177,0.153723641808267,0.156252701837223,0.160506346611089,
0.193188208656405,0.222560004176568,0.244175252655833,0.254295373048069,
0.256485288615895,0.257733423610194,0.258805426931146,0.260163907219127,
0.262836050825874,0.280219443950589,0.329262044005941,0.347305210354065,
0.354573405901029,0.360002454598206,0.362567700521536,0.364505042744284,
0.366333234975281,0.368881315843799,0.375563054186285,0.430968485007962,
0.455318835720252,0.466218414143172,0.468466852460497,0.469717985888873,
0.470789734517694,0.472144264664318,0.474886021346641,0.493329699716654,
0.537460493337828,0.565331844487407,0.571665330974489,0.574356964678557,
0.576315525547254,0.57811166408164,0.580996210279416,0.587999869069225,
0.639384390969122,0.666515463046019,0.678128414208415,0.680418169282219,
0.681678310145061,0.682749314752906,0.684092166452974,0.686691253820673,
0.702216832496513,0.708761033683465,0.722633883146357,0.755493946524701,
0.772056448871761,0.782367873029121,0.785616677260266,0.787690059230241,
0.789630794048282,0.792172039462032,0.796467194770158,0.831578309325013,
0.880465442872731,0.890288619835252,0.892468477381447,0.893704709005219,
0.894778410251878,0.89615457506459,0.899004704552178,0.935374576654408,
0.989163023546042,0.995619077791897,0.998331645788874,1.00029413998966,
1.00208611342134,1.00494703966778,1.01180631807051,1.06524492489252,1.09093517112184,
1.1021865682203,1.10445598581578,1.10571179440077,1.10678327900165,1.10813203208798,
1.11075809741942,1.12692228968746,1.1775802830176,1.20199425525246,1.20789427429974,
1.21051033843575,1.21245603672437,1.21427043328026,1.2167650424735,1.2231148889465,
1.2596833809502),.UNSPECIFIED.);
#2003=B_SPLINE_CURVE_WITH_KNOTS('',3,(#197131,#197132,#197133,#197134,#197135,
#197136,#197137,#197138,#197139,#197140),.UNSPECIFIED.,.F.,.F.,(4,1,1,1,
1,1,1,4),(-60.389703770172,-59.9301869977125,-58.9313505477506,-57.9325140977887,
-56.9336776478268,-55.934841197865,-54.9360047479031,-54.4565130710325),
 .UNSPECIFIED.);
#2004=B_SPLINE_CURVE_WITH_KNOTS('',3,(#197141,#197142,#197143,#197144,#197145,
#197146,#197147,#197148,#197149,#197150,#197151,#197152,#197153,#197154,
#197155,#197156,#197157,#197158),.UNSPECIFIED.,.F.,.F.,(4,2,2,2,2,2,2,2,
4),(0.000658788806491579,0.00332970125175962,0.00592165818523893,0.00778879641236155,
0.00964368919009544,0.01149091846978,0.0146445377313671,0.0233614971653259,
0.0750737837299188),.UNSPECIFIED.);
#2005=B_SPLINE_CURVE_WITH_KNOTS('',3,(#197163,#197164,#197165,#197166,#197167,
#197168,#197169,#197170,#197171,#197172,#197173,#197174,#197175,#197176,
#197177,#197178,#197179,#197180,#197181,#197182,#197183,#197184,#197185,
#197186,#197187,#197188,#197189,#197190,#197191,#197192,#197193,#197194,
#197195,#197196,#197197,#197198,#197199,#197200,#197201,#197202,#197203,
#197204,#197205,#197206,#197207,#197208,#197209,#197210,#197211,#197212,
#197213,#197214,#197215,#197216,#197217,#197218,#197219,#197220,#197221,
#197222,#197223,#197224,#197225,#197226,#197227,#197228,#197229,#197230,
#197231,#197232,#197233,#197234,#197235,#197236,#197237,#197238,#197239,
#197240,#197241,#197242,#197243,#197244,#197245,#197246,#197247,#197248,
#197249,#197250,#197251,#197252,#197253,#197254,#197255,#197256,#197257,
#197258,#197259,#197260,#197261,#197262,#197263,#197264,#197265,#197266,
#197267,#197268,#197269,#197270,#197271,#197272,#197273,#197274,#197275,
#197276,#197277,#197278,#197279,#197280,#197281,#197282,#197283,#197284,
#197285,#197286,#197287,#197288,#197289,#197290,#197291,#197292,#197293,
#197294,#197295,#197296,#197297,#197298,#197299,#197300,#197301,#197302,
#197303,#197304,#197305,#197306,#197307,#197308,#197309,#197310,#197311,
#197312,#197313,#197314,#197315,#197316,#197317,#197318,#197319,#197320,
#197321,#197322,#197323,#197324,#197325,#197326,#197327,#197328,#197329,
#197330,#197331,#197332,#197333,#197334,#197335,#197336,#197337,#197338,
#197339,#197340,#197341,#197342,#197343,#197344,#197345,#197346,#197347,
#197348,#197349,#197350,#197351,#197352,#197353,#197354,#197355,#197356,
#197357,#197358,#197359,#197360,#197361,#197362,#197363,#197364,#197365,
#197366,#197367,#197368,#197369,#197370,#197371,#197372,#197373,#197374,
#197375,#197376,#197377,#197378,#197379,#197380,#197381,#197382,#197383,
#197384,#197385,#197386),.UNSPECIFIED.,.F.,.F.,(4,2,2,2,2,2,2,2,2,2,2,2,
2,2,2,2,2,2,2,2,2,2,2,2,2,2,2,2,2,2,2,2,2,2,2,2,2,2,2,2,2,2,2,2,2,2,2,2,
2,2,2,2,2,2,2,2,2,2,2,2,2,2,2,2,2,2,2,2,2,2,2,2,2,2,2,2,2,2,2,2,2,2,2,2,
2,2,2,2,2,2,2,2,2,2,2,2,2,2,2,2,2,2,2,2,2,2,2,2,2,2,2,4),(1.25979359209778,
1.28580300251789,1.32656732777334,1.33163306653606,1.33409244522673,1.33601522933325,
1.33814663771316,1.34165901259573,1.35453367672641,1.37723368586608,1.41581987132213,
1.42081382980198,1.43681935977937,1.43943847251636,1.44078553098614,1.44185665510057,
1.44311318950585,1.44538682444043,1.45671902871575,1.48272757550874,1.53564227689878,
1.54253696868306,1.54540328335372,1.54719591666714,1.5491569561889,1.55186351104198,
1.55828625287392,1.58690768546855,1.63818509137097,1.64924545213547,1.65139221340895,
1.65274849671124,1.65382029206697,1.65506994527921,1.65731187995249,1.66810653038302,
1.69206554581996,1.74801204116381,1.75463697406073,1.75717605825111,1.75900177749123,
1.760940163237,1.7635130158854,1.76917688315898,1.79181683313003,1.82463095132139,
1.8289272421944,1.86034481835078,1.86325618395962,1.86464406631995,1.86571864660028,
1.86694664341057,1.86909013231011,1.87840070649366,1.92754245650627,1.96290424795715,
1.96720127802684,1.96974272745421,1.97168308605368,1.97375554954224,1.97700183529579,
1.9872960918038,2.00382460357321,2.03667919229329,2.04833442764834,2.05711079036982,
2.0726980307875,2.07529928991339,2.07664240285785,2.07771315941398,2.078972482818,
2.08125939474524,2.0928296954143,2.11979059720346,2.17134758805847,2.17833456471907,
2.18121589188431,2.18301110847835,2.18496953370372,2.18766255595841,2.19400663568412,
2.22197568769335,2.26488366547887,2.26905299832699,2.28462530638709,2.28722588622606,
2.28856883530343,2.28963956022194,2.29089896157927,2.2931863102912,2.30476507748831,
2.33176070845578,2.35233787454996,2.3867184315042,2.39100143075182,2.3935387725903,
2.39547841236837,2.39755245493155,2.40080612135813,2.41096065816617,2.4272680217722,
2.46879947995584,2.49608085887807,2.49898393281528,2.50037015595383,2.50144451003423,
2.50267343373536,2.50396687137187,2.50863278756087,2.53274153999305,2.5536372827895,
2.59294800260859),.UNSPECIFIED.);
#2006=B_SPLINE_CURVE_WITH_KNOTS('',3,(#197387,#197388,#197389,#197390,#197391,
#197392,#197393,#197394,#197395,#197396,#197397,#197398,#197399,#197400,
#197401,#197402,#197403,#197404,#197405,#197406,#197407,#197408,#197409,
#197410,#197411,#197412,#197413,#197414,#197415,#197416,#197417,#197418,
#197419,#197420,#197421,#197422,#197423,#197424,#197425,#197426,#197427,
#197428,#197429,#197430,#197431,#197432,#197433,#197434,#197435,#197436,
#197437,#197438,#197439,#197440,#197441,#197442,#197443,#197444,#197445,
#197446,#197447,#197448,#197449,#197450,#197451,#197452,#197453,#197454,
#197455,#197456,#197457,#197458,#197459,#197460,#197461,#197462,#197463,
#197464,#197465,#197466,#197467,#197468,#197469,#197470,#197471,#197472,
#197473,#197474,#197475,#197476,#197477,#197478,#197479,#197480,#197481,
#197482,#197483,#197484,#197485,#197486,#197487,#197488,#197489,#197490,
#197491,#197492,#197493,#197494,#197495,#197496,#197497,#197498,#197499,
#197500,#197501,#197502,#197503,#197504,#197505,#197506,#197507,#197508,
#197509,#197510,#197511,#197512,#197513,#197514,#197515,#197516,#197517,
#197518,#197519,#197520,#197521,#197522,#197523,#197524,#197525,#197526,
#197527,#197528,#197529,#197530,#197531,#197532,#197533,#197534,#197535,
#197536,#197537,#197538,#197539,#197540,#197541,#197542,#197543,#197544,
#197545,#197546,#197547,#197548,#197549,#197550,#197551,#197552,#197553,
#197554,#197555,#197556,#197557,#197558,#197559,#197560,#197561,#197562,
#197563,#197564,#197565,#197566,#197567,#197568,#197569,#197570,#197571,
#197572,#197573,#197574,#197575,#197576,#197577,#197578,#197579,#197580,
#197581,#197582,#197583,#197584,#197585,#197586,#197587,#197588,#197589,
#197590,#197591,#197592,#197593,#197594,#197595,#197596,#197597,#197598,
#197599,#197600,#197601,#197602,#197603,#197604,#197605,#197606,#197607,
#197608,#197609,#197610,#197611,#197612,#197613,#197614,#197615,#197616,
#197617,#197618,#197619,#197620,#197621,#197622,#197623,#197624),
 .UNSPECIFIED.,.F.,.F.,(4,2,2,2,2,2,2,2,2,2,2,2,2,2,2,2,2,2,2,2,2,2,2,2,
2,2,2,2,2,2,2,2,2,2,2,2,2,2,2,2,2,2,2,2,2,2,2,2,2,2,2,2,2,2,2,2,2,2,2,2,
2,2,2,2,2,2,2,2,2,2,2,2,2,2,2,2,2,2,2,2,2,2,2,2,2,2,2,2,2,2,2,2,2,2,2,2,
2,2,2,2,2,2,2,2,2,2,2,2,2,2,2,2,2,2,2,2,2,2,4),(0.0750737837299188,0.0897196818521214,
0.108795497230402,0.112693442247156,0.114256020592199,0.115357910077045,
0.116370459886175,0.118044759042156,0.12233532342493,0.170549693967141,
0.208879267552393,0.213931672917246,0.216874072207978,0.219503902802471,
0.221426789661721,0.223219057645675,0.226081713437894,0.232939565419232,
0.286353451360456,0.312059786394583,0.323315248293243,0.325584878079516,
0.32684072198318,0.327912186782429,0.329260851318762,0.331886556676403,
0.348042510349904,0.398689539703308,0.41655022562366,0.427439013049778,
0.430752521188773,0.432840181379354,0.434775636168728,0.43728347963043,
0.441463826026978,0.470473280170901,0.51196695415327,0.527505395662312,
0.535690782065472,0.537747559764025,0.538956555931311,0.540035311791355,
0.54143275341975,0.543765990741589,0.55837822406314,0.566577061161562,0.579798205438069,
0.612654542865741,0.629210578832585,0.639519319013962,0.642767991785144,
0.644841461486117,0.646782398989346,0.649324083771974,0.653620371647605,
0.688792552375121,0.737864776517521,0.747475569035496,0.749640943621061,
0.750874055446313,0.751948321104482,0.753329499684386,0.755557624182768,
0.768034521137767,0.772703615145575,0.823043088942335,0.840662357913241,
0.851445598070382,0.854747754737872,0.856833053483619,0.858769619820171,
0.86128357839281,0.865484378975842,0.895589004174204,0.947253201791336,
0.959259754409079,0.961571364824705,0.962836423381644,0.963907364194148,
0.965244782554016,0.967329069461115,0.977413353750753,0.982911559660835,
0.992300890531631,1.00387203193161,1.036719271018,1.0532606152779,1.06356316211411,
1.06681145690083,1.06888506379014,1.07082639563468,1.07336898061614,1.07766765068432,
1.11297821999515,1.16223323195852,1.17157100098013,1.17371728114146,1.17494630860135,
1.17602142579438,1.17740950961519,1.18031958109539,1.20845096251774,1.24814071125033,
1.26508638309759,1.27557123127229,1.27884050040433,1.28091883356835,1.28285853702239,
1.28539029585084,1.28965127770395,1.33465169887647,1.37970331859847,1.38442858727116,
1.38617091267851,1.38719692087222,1.38828963349461,1.38980016400639,1.39338182821556,
1.40880841792372),.UNSPECIFIED.);
#2007=B_SPLINE_CURVE_WITH_KNOTS('',3,(#197630,#197631,#197632,#197633,#197634),
 .UNSPECIFIED.,.F.,.F.,(4,1,4),(76.7075601022117,76.9104066470643,77.0584304051426),
 .UNSPECIFIED.);
#2008=B_SPLINE_CURVE_WITH_KNOTS('',3,(#197635,#197636,#197637,#197638,#197639,
#197640,#197641,#197642,#197643,#197644,#197645,#197646,#197647,#197648,
#197649,#197650,#197651,#197652,#197653,#197654,#197655,#197656,#197657,
#197658,#197659,#197660,#197661,#197662,#197663,#197664,#197665,#197666,
#197667,#197668,#197669,#197670,#197671,#197672,#197673,#197674,#197675,
#197676,#197677,#197678,#197679,#197680,#197681,#197682,#197683,#197684,
#197685,#197686,#197687,#197688,#197689,#197690,#197691,#197692,#197693,
#197694,#197695,#197696,#197697,#197698,#197699,#197700,#197701,#197702,
#197703,#197704,#197705,#197706,#197707,#197708,#197709,#197710,#197711,
#197712,#197713,#197714,#197715,#197716,#197717,#197718,#197719,#197720,
#197721,#197722,#197723,#197724,#197725,#197726,#197727,#197728,#197729,
#197730,#197731,#197732,#197733,#197734,#197735,#197736,#197737,#197738,
#197739,#197740,#197741,#197742,#197743,#197744,#197745,#197746,#197747,
#197748,#197749,#197750,#197751,#197752,#197753,#197754,#197755,#197756,
#197757,#197758,#197759,#197760,#197761,#197762,#197763,#197764,#197765,
#197766,#197767,#197768,#197769,#197770,#197771,#197772,#197773,#197774,
#197775,#197776,#197777,#197778,#197779,#197780,#197781,#197782,#197783,
#197784,#197785,#197786,#197787,#197788,#197789,#197790,#197791,#197792,
#197793,#197794,#197795,#197796,#197797,#197798,#197799,#197800,#197801,
#197802,#197803,#197804,#197805,#197806,#197807,#197808,#197809,#197810,
#197811,#197812,#197813,#197814,#197815,#197816,#197817,#197818,#197819,
#197820,#197821,#197822,#197823,#197824,#197825,#197826,#197827,#197828,
#197829,#197830,#197831,#197832,#197833,#197834,#197835,#197836,#197837,
#197838,#197839,#197840,#197841,#197842,#197843,#197844,#197845,#197846,
#197847,#197848,#197849,#197850,#197851,#197852,#197853,#197854,#197855,
#197856),.UNSPECIFIED.,.F.,.F.,(4,2,2,2,2,2,2,2,2,2,2,2,2,2,2,2,2,2,2,2,
2,2,2,2,2,2,2,2,2,2,2,2,2,2,2,2,2,2,2,2,2,2,2,2,2,2,2,2,2,2,2,2,2,2,2,2,
2,2,2,2,2,2,2,2,2,2,2,2,2,2,2,2,2,2,2,2,2,2,2,2,2,2,2,2,2,2,2,2,2,2,2,2,
2,2,2,2,2,2,2,2,2,2,2,2,2,2,2,2,2,2,4),(0.000629228676279194,0.0527834506842141,
0.0572122890737632,0.0609073219001442,0.0630791178976013,0.0649948664632921,
0.0673872018486889,0.0710961029451884,0.0893741307873062,0.100875358156077,
0.113855404834142,0.129422626240354,0.154644590672702,0.165757198924741,
0.168025986247171,0.169282505526748,0.170353540664101,0.171700384179906,
0.17431877797379,0.190313594831012,0.19570790421775,0.252779457535905,0.268947752408923,
0.272743940652662,0.274937889759981,0.276850920133946,0.279211074091741,
0.282816168391261,0.299508791647547,0.307019410709072,0.355519527389341,
0.3702513606368,0.378146063753463,0.380177794224394,0.381380972806579,0.382460726930709,
0.383867576065394,0.386233811473231,0.401654125028369,0.405923967024112,
0.448898512719925,0.476830175884744,0.483170369325384,0.485862824672043,
0.48782123787068,0.489616724533124,0.492499090160279,0.499491669635509,
0.551012040718334,0.57803351460542,0.589618494103655,0.591906363351962,
0.593165943163878,0.594236758012706,0.59557973577398,0.598180127255755,
0.613745321169219,0.620203171439649,0.66161261760335,0.688881510204923,
0.695141150523975,0.697819888360012,0.699775924492642,0.701574523450607,
0.704473563607079,0.711565843614122,0.761217898189458,0.799526595823581,
0.803130554894181,0.804644357639806,0.80573715469611,0.806761429207059,
0.808496950401207,0.813181324585151,0.854259244217092,0.900683905985834,
0.907075142276693,0.909776383056871,0.911736477921162,0.91353025530243,
0.916402766768146,0.923334954531907,0.975776204784388,1.00214730968667,
1.01357064115006,1.01584952895468,1.0171072144458,1.01817826251613,1.01952387516536,
1.0221362182242,1.03798592755138,1.04272917970373,1.05800575391191,1.09087775189184,
1.1074576345621,1.11777655337403,1.12102595057109,1.12309928639277,1.12503967987205,
1.12758004828269,1.131872757716,1.17426855659149,1.20332291167791,1.22293675891397,
1.22689151979009,1.22846302273638,1.22956648478356,1.23057684249836,1.23224028131276,
1.236464936696,1.25979359209778),.UNSPECIFIED.);
#2009=B_SPLINE_CURVE_WITH_KNOTS('',3,(#197858,#197859,#197860,#197861,#197862,
#197863,#197864,#197865,#197866,#197867,#197868,#197869,#197870,#197871,
#197872,#197873,#197874,#197875,#197876,#197877,#197878,#197879,#197880,
#197881,#197882,#197883,#197884,#197885,#197886,#197887,#197888,#197889,
#197890,#197891,#197892,#197893,#197894,#197895,#197896,#197897,#197898,
#197899,#197900,#197901,#197902,#197903,#197904,#197905,#197906,#197907,
#197908,#197909,#197910,#197911,#197912,#197913,#197914,#197915,#197916,
#197917,#197918,#197919,#197920,#197921,#197922,#197923,#197924,#197925,
#197926,#197927,#197928,#197929,#197930,#197931,#197932,#197933,#197934,
#197935,#197936,#197937,#197938,#197939,#197940,#197941,#197942,#197943,
#197944,#197945,#197946,#197947,#197948,#197949,#197950,#197951,#197952,
#197953,#197954,#197955,#197956,#197957,#197958,#197959,#197960,#197961,
#197962,#197963,#197964,#197965,#197966,#197967,#197968,#197969,#197970,
#197971,#197972,#197973,#197974,#197975,#197976,#197977,#197978,#197979,
#197980,#197981,#197982,#197983,#197984,#197985,#197986,#197987,#197988,
#197989,#197990,#197991,#197992,#197993,#197994,#197995,#197996,#197997,
#197998,#197999,#198000,#198001,#198002,#198003,#198004,#198005,#198006,
#198007,#198008,#198009,#198010,#198011,#198012,#198013,#198014,#198015,
#198016,#198017,#198018,#198019,#198020,#198021,#198022,#198023,#198024,
#198025,#198026,#198027,#198028,#198029,#198030,#198031,#198032,#198033,
#198034,#198035,#198036,#198037,#198038,#198039,#198040,#198041,#198042,
#198043,#198044,#198045,#198046,#198047,#198048,#198049,#198050,#198051,
#198052,#198053,#198054,#198055,#198056,#198057,#198058,#198059,#198060,
#198061,#198062,#198063,#198064,#198065,#198066,#198067,#198068,#198069,
#198070,#198071,#198072,#198073,#198074,#198075,#198076,#198077,#198078,
#198079,#198080,#198081,#198082,#198083),.UNSPECIFIED.,.F.,.F.,(4,2,2,2,
2,2,2,2,2,2,2,2,2,2,2,2,2,2,2,2,2,2,2,2,2,2,2,2,2,2,2,2,2,2,2,2,2,2,2,2,
2,2,2,2,2,2,2,2,2,2,2,2,2,2,2,2,2,2,2,2,2,2,2,2,2,2,2,2,2,2,2,2,2,2,2,2,
2,2,2,2,2,2,2,2,2,2,2,2,2,2,2,2,2,2,2,2,2,2,2,2,2,2,2,2,2,2,2,2,2,2,2,2,
4),(1.40880841792372,1.43101997011835,1.48144340271669,1.48850203098995,
1.49139648684803,1.49319500633745,1.49515315669075,1.49783876541391,1.5041327669713,
1.5316719318947,1.56007598033247,1.58240616418509,1.59511320409958,1.59735378325235,
1.59873883941128,1.59981366251036,1.60104466340688,1.60319981324344,1.61266153047195,
1.6618473339337,1.69705242112975,1.70134972363743,1.70389199475506,1.70583336105332,
1.70790726954843,1.71115658835216,1.7214669446394,1.73802746971779,1.77091963230637,
1.78465511414046,1.79152685943823,1.79173721671427,1.79510233306198,1.80720789297196,
1.80941609609006,1.81079133466597,1.81186513504218,1.81310241871079,1.81528637014086,
1.82516584462093,1.87399142184213,1.90908129797623,1.91337682220747,1.91591848588703,
1.91785964438777,1.91993357918921,1.92318345766908,1.9334999608329,1.95007451855918,
1.98297698893026,1.9978543197517,2.00287124273322,2.01889450782522,2.02151529739038,
2.02286301703774,2.02393456106175,2.02519146540749,2.02746545797424,2.03879304938004,
2.06477635953734,2.11776185631112,2.12465535076338,2.12752213243445,2.12931533802002,
2.13127722879156,2.13398537144229,2.14041383627185,2.16907359567702,2.22038027673558,
2.23140764499874,2.23355292398433,2.23490902409013,2.23598117748184,2.23723182647198,
2.23947699110722,2.25031485350018,2.27442776711455,2.33017537794966,2.33682517366497,
2.33936873441911,2.34119607934516,2.34313472547635,2.34570543075798,2.35135441365152,
2.37387692992762,2.40662272430839,2.44267392561182,2.44553218269773,2.44691002465133,
2.44794933915377,2.44914452258852,2.45041830743122,2.45235159391131,2.4559278827369,
2.46439798759593,2.52405085558296,2.54591226606874,2.54983010470779,2.55228662601291,
2.5542094882945,2.55634335583337,2.55986527124225,2.57283726665067,2.59578767651268,
2.64810982117262,2.65598082521307,2.65807664894648,2.65930652318843,2.6603632451898,
2.66140905420161,2.66275937318509,2.66521722158727,2.66831062682325),
 .UNSPECIFIED.);
#2010=B_SPLINE_CURVE_WITH_KNOTS('',3,(#198084,#198085,#198086,#198087,#198088,
#198089),.UNSPECIFIED.,.F.,.F.,(4,2,4),(0.000817343676032421,0.0612254265673932,
0.0752219485597137),.UNSPECIFIED.);
#2011=B_SPLINE_CURVE_WITH_KNOTS('',3,(#198095,#198096,#198097,#198098,#198099,
#198100,#198101,#198102,#198103,#198104,#198105,#198106,#198107),
 .UNSPECIFIED.,.F.,.F.,(4,3,3,3,4),(82.9907456874175,83.0928761471927,83.1948834239568,
83.2967928187986,83.3413404565306),.UNSPECIFIED.);
#2012=B_SPLINE_CURVE_WITH_KNOTS('',3,(#198108,#198109,#198110,#198111,#198112,
#198113,#198114,#198115,#198116,#198117),.UNSPECIFIED.,.F.,.F.,(4,1,1,1,
1,1,1,4),(77.0584304051426,77.9092430970262,78.9080795469881,79.9069159969499,
80.9057524469118,81.9045888968737,82.9034253468356,82.9907454093913),
 .UNSPECIFIED.);
#2013=B_SPLINE_CURVE_WITH_KNOTS('',3,(#198118,#198119,#198120,#198121,#198122,
#198123,#198124,#198125,#198126,#198127,#198128,#198129,#198130,#198131,
#198132,#198133,#198134,#198135,#198136,#198137,#198138,#198139,#198140,
#198141,#198142,#198143,#198144,#198145,#198146,#198147,#198148,#198149,
#198150,#198151,#198152,#198153,#198154,#198155,#198156,#198157,#198158,
#198159,#198160,#198161,#198162,#198163,#198164,#198165,#198166,#198167,
#198168,#198169,#198170,#198171,#198172,#198173,#198174,#198175,#198176,
#198177,#198178,#198179,#198180,#198181,#198182,#198183,#198184,#198185,
#198186,#198187,#198188,#198189,#198190,#198191,#198192,#198193,#198194,
#198195,#198196,#198197,#198198,#198199,#198200,#198201,#198202,#198203,
#198204,#198205,#198206,#198207,#198208,#198209,#198210,#198211,#198212,
#198213,#198214,#198215,#198216,#198217,#198218,#198219,#198220,#198221,
#198222,#198223,#198224,#198225,#198226,#198227,#198228,#198229,#198230,
#198231,#198232,#198233,#198234,#198235,#198236,#198237,#198238,#198239,
#198240,#198241,#198242,#198243,#198244,#198245,#198246,#198247,#198248,
#198249,#198250,#198251,#198252,#198253,#198254,#198255,#198256,#198257,
#198258,#198259,#198260,#198261,#198262,#198263,#198264,#198265,#198266,
#198267,#198268,#198269,#198270,#198271,#198272,#198273,#198274,#198275,
#198276,#198277,#198278,#198279,#198280,#198281,#198282,#198283,#198284,
#198285,#198286,#198287,#198288,#198289,#198290,#198291,#198292,#198293,
#198294,#198295,#198296,#198297,#198298,#198299,#198300,#198301,#198302,
#198303,#198304,#198305,#198306,#198307,#198308,#198309,#198310,#198311,
#198312,#198313,#198314,#198315,#198316,#198317,#198318,#198319,#198320,
#198321,#198322,#198323,#198324,#198325,#198326,#198327,#198328,#198329,
#198330,#198331,#198332,#198333,#198334,#198335,#198336,#198337,#198338,
#198339,#198340,#198341,#198342,#198343,#198344,#198345,#198346,#198347,
#198348,#198349,#198350,#198351,#198352,#198353,#198354,#198355,#198356,
#198357,#198358,#198359,#198360,#198361,#198362,#198363,#198364,#198365,
#198366,#198367,#198368,#198369,#198370,#198371,#198372,#198373,#198374,
#198375,#198376,#198377,#198378,#198379,#198380,#198381,#198382,#198383,
#198384,#198385,#198386,#198387),.UNSPECIFIED.,.F.,.F.,(4,2,2,2,2,2,2,2,
2,2,2,2,2,2,2,2,2,2,2,2,2,2,2,2,2,2,2,2,2,2,2,2,2,2,2,2,2,2,2,2,2,2,2,2,
2,2,2,2,2,2,2,2,2,2,2,2,2,2,2,2,2,2,2,2,2,2,2,2,2,2,2,2,2,2,2,2,2,2,2,2,
2,2,2,2,2,2,2,2,2,2,2,2,2,2,2,2,2,2,2,2,2,2,2,2,2,2,2,2,2,2,2,2,2,2,2,2,
2,2,2,2,2,2,2,2,2,2,2,2,2,2,2,2,2,2,4),(0.0752219485597137,0.0876737733029266,
0.0938318777926784,0.0964929851085831,0.0984458590727868,0.100248364936695,
0.103168891336402,0.110389684477826,0.154249330517679,0.195394745934447,
0.199213040908045,0.201237857018698,0.2025493772978,0.203773004267836,0.203776571015409,
0.203780150357518,0.203783742356241,0.203787580102183,0.203791479604201,
0.203795442215694,0.203799469200582,0.203803562193082,0.203807722511776,
0.203811951609945,0.203816250925197,0.203820621936599,0.203825066484,0.203829586160866,
0.203834182563694,0.203838857492989,0.203843612621636,0.203848449836046,
0.204892179818097,0.206274880308293,0.209159666278352,0.243328974195012,
0.27757081259187,0.294125489025972,0.30443276469162,0.307680647015343,0.309753533172861,
0.311693868908419,0.314234685553496,0.318529326413003,0.353664018923092,
0.402636125373647,0.412344052578725,0.414515702355721,0.41574996653691,
0.416823681212764,0.418202116159678,0.421064705760515,0.45673982715691,
0.489566236134306,0.506090988429658,0.516384984815751,0.51963153449997,
0.521704256101316,0.523644919890115,0.526186861985578,0.5304849656276,0.565866214730676,
0.615040069717612,0.624354377622764,0.626498422545301,0.627726677807272,
0.628801450447854,0.630189525985197,0.633101119278578,0.664540225858998,
0.715320677188441,0.72791257676452,0.731398750354841,0.733524475083077,
0.735448754805604,0.737919265477722,0.741884064547403,0.76485918052092,
0.823420483458493,0.836039021492217,0.838381978493775,0.839653663194521,
0.840724022450337,0.842052962543649,0.844110099785209,0.8538100709527,0.859594247613297,
0.860030125278103,0.866915603183283,0.880642879647557,0.913503964103421,
0.930065916623037,0.940377309841268,0.943626270016112,0.945699791319999,
0.94764068452207,0.95018217767509,0.954477842139657,0.989605027864029,1.03853647933468,
1.0483122506774,1.05048899500394,1.0517246010037,1.05279848804178,1.05417584379465,
1.05703171390351,1.07981293386321,1.09265757223245,1.12551358123912,1.14206696315663,
1.15237477849041,1.15562354724399,1.15769717133001,1.15963831877472,1.1621803728906,
1.16647749671,1.20168515380954,1.25086767596654,1.26035706105177,1.26251406211317,
1.26374540444121,1.26482006731463,1.26620430415427,1.26909488658854,1.29479851747829,
1.33424611894595,1.36197018183995,1.3661108826407,1.36860741670612,1.37054151261102,
1.37263503959985,1.37597366853975,1.38709012111101,1.4054761068303,1.40869849150873),
 .UNSPECIFIED.);
#2014=B_SPLINE_CURVE_WITH_KNOTS('',3,(#198393,#198394,#198395,#198396,#198397,
#198398,#198399,#198400,#198401,#198402,#198403,#198404,#198405,#198406,
#198407,#198408,#198409,#198410,#198411,#198412,#198413,#198414,#198415,
#198416,#198417,#198418),.UNSPECIFIED.,.F.,.F.,(4,2,2,2,2,2,2,2,2,2,2,2,
4),(2.59385173281912,2.61315066313481,2.62526726593595,2.62709460362196,
2.62809611461634,2.63678412524615,2.63993532549552,2.64178241720017,2.64363741504273,
2.64550551036064,2.6479070159309,2.65164701932836,2.66828059292683),
 .UNSPECIFIED.);
#2015=B_SPLINE_CURVE_WITH_KNOTS('',3,(#198419,#198420,#198421,#198422,#198423,
#198424,#198425,#198426,#198427,#198428,#198429,#198430,#198431,#198432,
#198433,#198434,#198435,#198436,#198437,#198438,#198439,#198440,#198441,
#198442,#198443,#198444,#198445,#198446,#198447,#198448,#198449,#198450,
#198451,#198452,#198453,#198454,#198455,#198456,#198457,#198458,#198459,
#198460,#198461,#198462,#198463,#198464,#198465,#198466,#198467,#198468,
#198469,#198470,#198471,#198472,#198473,#198474,#198475,#198476,#198477,
#198478,#198479,#198480,#198481,#198482,#198483,#198484,#198485,#198486,
#198487,#198488,#198489,#198490,#198491,#198492,#198493,#198494,#198495,
#198496,#198497,#198498,#198499,#198500,#198501,#198502,#198503,#198504,
#198505,#198506,#198507,#198508,#198509,#198510,#198511,#198512,#198513,
#198514,#198515,#198516,#198517,#198518,#198519,#198520,#198521,#198522,
#198523,#198524,#198525,#198526,#198527,#198528,#198529,#198530,#198531,
#198532,#198533,#198534,#198535,#198536,#198537,#198538,#198539,#198540,
#198541,#198542,#198543,#198544,#198545,#198546,#198547,#198548,#198549,
#198550,#198551,#198552,#198553,#198554,#198555,#198556,#198557,#198558,
#198559,#198560,#198561,#198562,#198563,#198564,#198565,#198566,#198567,
#198568,#198569,#198570,#198571,#198572,#198573,#198574,#198575,#198576,
#198577,#198578,#198579,#198580,#198581,#198582,#198583,#198584,#198585,
#198586,#198587,#198588,#198589,#198590,#198591,#198592,#198593,#198594,
#198595,#198596,#198597,#198598,#198599),.UNSPECIFIED.,.F.,.F.,(4,3,3,3,
3,3,3,3,3,3,3,3,3,3,3,3,3,3,3,3,3,3,3,3,3,3,3,3,3,3,3,3,3,3,3,3,3,3,3,3,
3,3,3,3,3,3,3,3,3,3,3,3,3,3,3,3,3,3,3,3,4),(83.3413404565306,83.4431911419029,
83.5450420266759,83.6469948978629,83.7490046894964,83.851187834397,83.9022617967974,
84.0056565338452,84.1088978159599,84.2120177813522,84.315072349561,84.4180955579187,
84.5211214005913,84.6242541673693,84.7274432587791,84.8308152521607,84.9010982467593,
85.0044929838072,85.1077342659224,85.2108542313147,85.3139087995236,85.4169320078813,
85.5199578505538,85.6230906173319,85.7262797087417,85.8296517021233,85.8999346967212,
86.0033294337692,86.1065707158841,86.2096906812764,86.3127452494853,86.415768457843,
86.5187943005157,86.6219270672937,86.7251161587035,86.8284881520851,86.8987711466831,
87.0021658837311,87.105407165846,87.2085271312382,87.3115816994471,87.4146049078047,
87.5176307504776,87.6207635172557,87.7239526086653,87.8273246020469,87.8976075966449,
88.0010023336929,88.1042436158077,88.2073635811999,88.3104181494089,88.4134413577665,
88.516467200439,88.6195999672169,88.7227890586267,88.8261610520084,88.8964440466068,
89.0132269961633,89.129558683076,89.245139987838,89.2739307161836),
 .UNSPECIFIED.);
#2016=B_SPLINE_CURVE_WITH_KNOTS('',3,(#198601,#198602,#198603,#198604,#198605,
#198606,#198607,#198608,#198609,#198610,#198611,#198612,#198613,#198614,
#198615,#198616,#198617,#198618,#198619,#198620,#198621,#198622,#198623,
#198624,#198625,#198626,#198627,#198628,#198629,#198630,#198631,#198632,
#198633,#198634,#198635,#198636,#198637,#198638,#198639,#198640,#198641,
#198642,#198643,#198644,#198645,#198646,#198647,#198648,#198649,#198650,
#198651,#198652,#198653,#198654,#198655,#198656,#198657,#198658,#198659,
#198660,#198661,#198662,#198663,#198664,#198665,#198666,#198667,#198668,
#198669,#198670,#198671,#198672,#198673,#198674,#198675,#198676,#198677,
#198678,#198679,#198680,#198681,#198682,#198683,#198684,#198685,#198686,
#198687,#198688,#198689,#198690,#198691,#198692,#198693,#198694,#198695,
#198696,#198697,#198698,#198699,#198700,#198701,#198702,#198703,#198704,
#198705,#198706,#198707,#198708,#198709,#198710,#198711,#198712,#198713,
#198714,#198715,#198716,#198717,#198718,#198719,#198720,#198721,#198722,
#198723,#198724,#198725,#198726,#198727,#198728,#198729,#198730,#198731,
#198732,#198733,#198734,#198735,#198736,#198737,#198738,#198739,#198740,
#198741,#198742,#198743,#198744,#198745,#198746,#198747,#198748,#198749,
#198750,#198751,#198752,#198753,#198754,#198755,#198756,#198757,#198758,
#198759,#198760,#198761,#198762,#198763,#198764,#198765,#198766,#198767,
#198768,#198769,#198770,#198771,#198772,#198773,#198774,#198775,#198776,
#198777,#198778,#198779,#198780,#198781,#198782,#198783,#198784,#198785,
#198786,#198787,#198788,#198789,#198790,#198791,#198792,#198793,#198794,
#198795,#198796,#198797,#198798,#198799,#198800,#198801,#198802,#198803,
#198804,#198805,#198806,#198807,#198808,#198809,#198810,#198811,#198812,
#198813,#198814,#198815,#198816,#198817,#198818,#198819,#198820,#198821,
#198822,#198823,#198824,#198825,#198826,#198827,#198828),.UNSPECIFIED.,
 .F.,.F.,(4,2,2,2,2,2,2,2,2,2,2,2,2,2,2,2,2,2,2,2,2,2,2,2,2,2,2,2,2,2,2,
2,2,2,2,2,2,2,2,2,2,2,2,2,2,2,2,2,2,2,2,2,2,2,2,2,2,2,2,2,2,2,2,2,2,2,2,
2,2,2,2,2,2,2,2,2,2,2,2,2,2,2,2,2,2,2,2,2,2,2,2,2,2,2,2,2,2,2,2,2,2,2,2,
2,2,2,2,2,2,2,2,2,2,4),(1.40869849150873,1.45282999451277,1.47139320436944,
1.47413964982754,1.4754954227699,1.47656762600383,1.47781868811996,1.48006548139551,
1.49092827283456,1.51513260841594,1.5557644112509,1.57472007913753,1.57847476178802,
1.58088182783535,1.58279981247997,1.58496394597157,1.58862108920682,1.60315630343547,
1.63041105310353,1.67885590606411,1.68487399554867,1.6867933446037,1.68797195217562,
1.68906063826672,1.69054748325081,1.69399238118545,1.69876842221026,1.71159051457192,
1.75729466100386,1.78601286148282,1.79018013714976,1.79268458549216,1.79462002923047,
1.79671026364585,1.80003340912451,1.81100424264699,1.82905329556861,1.87930839629007,
1.8853934510873,1.89613523163867,1.89826280713267,1.89961363106515,1.90068558746215,
1.90194059826735,1.90420514712472,1.91536385835007,1.9406865562147,1.99464856661658,
2.00146566612399,2.00432022060142,2.00611147851677,2.00807584100176,2.01079586987848,
2.01729299201516,2.04652667672953,2.08228004942426,2.09145789885947,2.10770424299693,
2.11033421361682,2.1116840227843,2.11275584801668,2.11401148510361,2.11627913667979,
2.12749284169255,2.15302910826818,2.20667365531364,2.21351662363869,2.21637534133464,
2.21816727041529,2.22013080194248,2.22284679400517,2.22932047284512,2.2836635842511,
2.28607016932554,2.30397872243829,2.31983135887965,2.32244507202444,2.323791374139,
2.32486296197884,2.32612127644059,2.32840128113389,2.33983030250532,2.36621192370692,
2.41864182465004,2.42557719298027,2.42845110295001,2.43024577948122,2.43216758461202,
2.43478026075135,2.43770639068747,2.44271806203508,2.45338552959112,2.48461083736921,
2.52889863931077,2.53356177346718,2.53529459443978,2.53631869273946,2.53741251089712,
2.53892970481681,2.54255092618303,2.54764383670332,2.56173527925422,2.61338515130572,
2.62550364419783,2.62733126705756,2.62833293305939,2.63702229924639,2.64017399109347,
2.64202137093178,2.64387665813868,2.64574504485191,2.64814692501092,2.65188751176353,
2.6685236796344),.UNSPECIFIED.);
#2017=B_SPLINE_CURVE_WITH_KNOTS('',3,(#198829,#198830,#198831,#198832,#198833,
#198834,#198835,#198836,#198837,#198838),.UNSPECIFIED.,.F.,.F.,(4,3,3,4),
(-85.8723819380379,-85.7556990039215,-85.6390735155331,-85.5224480271446),
 .UNSPECIFIED.);
#2018=B_SPLINE_CURVE_WITH_KNOTS('',3,(#198843,#198844,#198845,#198846,#198847,
#198848,#198849,#198850,#198851,#198852,#198853,#198854,#198855,#198856,
#198857,#198858,#198859,#198860,#198861,#198862,#198863,#198864,#198865,
#198866,#198867,#198868,#198869,#198870,#198871,#198872,#198873,#198874,
#198875,#198876,#198877,#198878,#198879,#198880,#198881,#198882,#198883,
#198884,#198885,#198886,#198887,#198888,#198889,#198890,#198891,#198892,
#198893,#198894,#198895,#198896,#198897,#198898,#198899,#198900,#198901,
#198902,#198903,#198904,#198905,#198906,#198907,#198908,#198909,#198910,
#198911,#198912,#198913,#198914,#198915,#198916,#198917,#198918,#198919,
#198920,#198921,#198922,#198923,#198924,#198925,#198926,#198927,#198928,
#198929,#198930,#198931,#198932,#198933,#198934,#198935,#198936,#198937,
#198938,#198939,#198940,#198941,#198942,#198943,#198944,#198945,#198946,
#198947,#198948,#198949,#198950,#198951,#198952,#198953,#198954,#198955,
#198956,#198957,#198958,#198959,#198960,#198961,#198962,#198963,#198964,
#198965,#198966,#198967,#198968,#198969,#198970,#198971,#198972,#198973,
#198974,#198975,#198976,#198977,#198978,#198979,#198980,#198981,#198982,
#198983,#198984,#198985,#198986,#198987,#198988,#198989,#198990,#198991,
#198992,#198993,#198994,#198995,#198996,#198997,#198998,#198999,#199000,
#199001,#199002,#199003,#199004,#199005,#199006,#199007,#199008,#199009,
#199010,#199011,#199012,#199013,#199014,#199015,#199016,#199017,#199018,
#199019,#199020,#199021,#199022,#199023,#199024,#199025,#199026,#199027,
#199028,#199029,#199030,#199031,#199032,#199033,#199034,#199035,#199036,
#199037,#199038,#199039,#199040,#199041,#199042,#199043,#199044,#199045,
#199046,#199047,#199048,#199049,#199050,#199051,#199052,#199053,#199054,
#199055,#199056,#199057,#199058,#199059,#199060,#199061,#199062,#199063,
#199064,#199065,#199066,#199067,#199068,#199069,#199070,#199071,#199072,
#199073,#199074,#199075,#199076),.UNSPECIFIED.,.F.,.F.,(4,2,2,2,2,2,2,2,
2,2,2,2,2,2,2,2,2,2,2,2,2,2,2,2,2,2,2,2,2,2,2,2,2,2,2,2,2,2,2,2,2,2,2,2,
2,2,2,2,2,2,2,2,2,2,2,2,2,2,2,2,2,2,2,2,2,2,2,2,2,2,2,2,2,2,2,2,2,2,2,2,
2,2,2,2,2,2,2,2,2,2,2,2,2,2,2,2,2,2,2,2,2,2,2,2,2,2,2,2,2,2,2,2,2,2,2,2,
4),(1.26008679584093,1.2603413105264,1.26249802864315,1.26372920944908,
1.26480373135215,1.26618778661088,1.2690779898589,1.29477824700187,1.3342206771408,
1.36194110379178,1.36608126145692,1.36857746804445,1.37051131024333,1.37260456260776,
1.37594275358238,1.38705774777023,1.40544132125641,1.45278900991273,1.47134977490511,
1.47409585979184,1.47545145482721,1.47652351740771,1.47777441545709,1.48002091420739,
1.4908822840175,1.51508345677271,1.55570992129749,1.57466309758851,1.57841728731957,
1.58082403749609,1.58274177053474,1.5849056202199,1.58856228407212,1.60309559589524,
1.63034678272025,1.67878538567897,1.68480258921642,1.68672167451692,1.68790012481218,
1.68898866915346,1.69047532557243,1.69391980857443,1.71499919649434,1.75523958959363,
1.78583819386779,1.79005036886686,1.79256780132352,1.79450508384327,1.79658922337749,
1.79988543356867,1.81061260261821,1.82810633394543,1.87781222265419,1.89544518422071,
1.89812709711412,1.89948798428238,1.9005605708405,1.9018078838582,1.90403752821918,
1.91462094565197,1.93780182652106,1.99499600940796,2.00149099514587,2.00400988944245,
2.00583081917494,2.00777314725302,2.01036673091977,2.01614041302495,2.03959180885092,
2.08393330297765,2.10728335130664,2.11014619447026,2.11152499875734,2.11259911362248,
2.11383397325131,2.11600698016759,2.12572639757834,2.17468533809976,2.20983460356922,
2.21412171957463,2.21666091332031,2.21860163017905,2.22067649562734,2.22393076493239,
2.23428600884851,2.25094648885346,2.2839198252524,2.30291616025821,2.30400226766826,
2.31965431988133,2.32226135506949,2.32360609237969,2.32467742555796,2.32593659224789,
2.32822108271443,2.33973407961209,2.36645438123486,2.41839183487559,2.42535909431864,
2.42823799163131,2.43003337632152,2.4319540526298,2.43456182748373,2.43748124032635,
2.44247667344687,2.4530966500259,2.48435517938215,2.52866826149156,2.53333737182369,
2.53507094185315,2.53609508012374,2.53718859750785,2.53870481229946,2.54232108570804,
2.54740525298321,2.56146200600718,2.59385173281912),.UNSPECIFIED.);
#2019=B_SPLINE_CURVE_WITH_KNOTS('',3,(#199078,#199079,#199080,#199081,#199082,
#199083,#199084,#199085,#199086,#199087,#199088,#199089,#199090,#199091,
#199092,#199093,#199094,#199095,#199096,#199097,#199098,#199099,#199100,
#199101,#199102,#199103,#199104,#199105,#199106,#199107,#199108,#199109,
#199110,#199111,#199112,#199113,#199114,#199115,#199116,#199117,#199118,
#199119,#199120,#199121,#199122,#199123,#199124,#199125,#199126,#199127,
#199128,#199129,#199130,#199131,#199132,#199133,#199134,#199135,#199136,
#199137,#199138,#199139,#199140,#199141,#199142,#199143,#199144,#199145,
#199146,#199147,#199148,#199149,#199150,#199151,#199152,#199153,#199154,
#199155,#199156,#199157,#199158,#199159,#199160,#199161,#199162,#199163,
#199164,#199165,#199166,#199167,#199168,#199169,#199170,#199171,#199172,
#199173,#199174,#199175,#199176,#199177,#199178,#199179,#199180,#199181,
#199182,#199183,#199184,#199185,#199186,#199187,#199188,#199189,#199190,
#199191,#199192,#199193,#199194,#199195,#199196,#199197,#199198,#199199,
#199200,#199201,#199202,#199203,#199204,#199205,#199206,#199207,#199208,
#199209,#199210,#199211,#199212,#199213,#199214,#199215,#199216,#199217,
#199218,#199219,#199220,#199221,#199222,#199223,#199224,#199225,#199226,
#199227,#199228,#199229,#199230,#199231,#199232,#199233,#199234,#199235,
#199236,#199237,#199238,#199239,#199240,#199241,#199242,#199243,#199244,
#199245,#199246,#199247,#199248,#199249,#199250,#199251,#199252,#199253,
#199254,#199255,#199256,#199257,#199258),.UNSPECIFIED.,.F.,.F.,(4,3,3,3,
3,3,3,3,3,3,3,3,3,3,3,3,3,3,3,3,3,3,3,3,3,3,3,3,3,3,3,3,3,3,3,3,3,3,3,3,
3,3,3,3,3,3,3,3,3,3,3,3,3,3,3,3,3,3,3,3,4),(-91.8056330559093,-91.7034783920339,
-91.6014794906741,-91.4995669524681,-91.3977052133587,-91.295858778697,
-91.1939207704756,-91.0919397623156,-90.9897717066845,-90.8941169465305,
-90.7907222094827,-90.6874809273677,-90.5843609619754,-90.4813063937665,
-90.3782831854088,-90.2752573427366,-90.1721245759585,-90.0689354845488,
-89.9655634911672,-89.8952804965687,-89.7918857595209,-89.6886444774058,
-89.5855245120135,-89.4824699438045,-89.3794467354468,-89.2764208927742,
-89.1732881259961,-89.0700990345864,-88.9667270412048,-88.8964440466068,
-88.7930493095588,-88.689808027444,-88.5866880620518,-88.4836334938429,
-88.3806102854851,-88.2775844428123,-88.1744516760342,-88.0712625846243,
-87.9678905912427,-87.8976075966449,-87.7942128595969,-87.690971577482,
-87.5878516120897,-87.4847970438807,-87.3817738355228,-87.2787479928502,
-87.1756152260721,-87.0724261346624,-86.9690541412807,-86.898771146683,
-86.795376409635,-86.6921351275196,-86.5890151621273,-86.4859605939185,
-86.3829373855607,-86.2799115428881,-86.17677877611,-86.0735896847,-85.9702176913185,
-85.8999346967211,-85.8723819380379),.UNSPECIFIED.);
#2020=B_SPLINE_CURVE_WITH_KNOTS('',3,(#199259,#199260,#199261,#199262,#199263),
 .UNSPECIFIED.,.F.,.F.,(4,1,4),(-92.1566392082287,-91.8929533964924,-91.8056333339369),
 .UNSPECIFIED.);
#2021=B_SPLINE_CURVE_WITH_KNOTS('',3,(#199269,#199270,#199271,#199272,#199273,
#199274,#199275,#199276,#199277,#199278,#199279,#199280,#199281,#199282,
#199283,#199284,#199285,#199286,#199287,#199288,#199289,#199290),
 .UNSPECIFIED.,.F.,.F.,(4,2,2,2,2,2,2,2,2,2,4),(2.59411274951175,2.59558337459403,
2.64820215244959,2.65607324743657,2.65816909558666,2.65939898408976,2.66045571833172,
2.66150153941828,2.66285187396475,2.66530975094863,2.66840319211896),
 .UNSPECIFIED.);
#2022=B_SPLINE_CURVE_WITH_KNOTS('',3,(#199291,#199292,#199293,#199294,#199295,
#199296,#199297,#199298,#199299,#199300,#199301,#199302,#199303,#199304,
#199305,#199306,#199307,#199308,#199309,#199310,#199311,#199312,#199313,
#199314,#199315,#199316,#199317,#199318,#199319,#199320,#199321,#199322,
#199323,#199324,#199325,#199326,#199327,#199328,#199329,#199330,#199331,
#199332,#199333,#199334,#199335,#199336,#199337,#199338,#199339,#199340,
#199341,#199342,#199343,#199344,#199345,#199346,#199347,#199348,#199349,
#199350,#199351,#199352,#199353,#199354,#199355,#199356,#199357,#199358,
#199359,#199360,#199361,#199362,#199363,#199364,#199365,#199366,#199367,
#199368,#199369,#199370,#199371,#199372,#199373,#199374,#199375,#199376,
#199377,#199378,#199379,#199380,#199381,#199382,#199383,#199384,#199385,
#199386,#199387,#199388,#199389,#199390,#199391,#199392,#199393,#199394,
#199395,#199396,#199397,#199398,#199399,#199400,#199401,#199402,#199403,
#199404,#199405,#199406,#199407,#199408,#199409,#199410,#199411,#199412,
#199413,#199414,#199415,#199416,#199417,#199418,#199419,#199420,#199421,
#199422,#199423,#199424,#199425,#199426,#199427,#199428,#199429,#199430,
#199431,#199432,#199433,#199434,#199435,#199436,#199437,#199438,#199439,
#199440,#199441,#199442,#199443,#199444,#199445,#199446,#199447,#199448,
#199449,#199450,#199451,#199452,#199453,#199454,#199455,#199456,#199457,
#199458,#199459,#199460,#199461,#199462,#199463,#199464,#199465,#199466,
#199467,#199468,#199469,#199470,#199471,#199472,#199473,#199474,#199475,
#199476,#199477,#199478,#199479,#199480,#199481,#199482,#199483,#199484,
#199485,#199486,#199487,#199488,#199489,#199490,#199491,#199492,#199493,
#199494,#199495,#199496,#199497,#199498,#199499,#199500,#199501,#199502,
#199503,#199504,#199505,#199506,#199507,#199508,#199509,#199510,#199511,
#199512,#199513,#199514,#199515,#199516,#199517,#199518,#199519,#199520,
#199521,#199522,#199523,#199524,#199525,#199526),.UNSPECIFIED.,.F.,.F.,
(4,2,2,2,2,2,2,2,2,2,2,2,2,2,2,2,2,2,2,2,2,2,2,2,2,2,2,2,2,2,2,2,2,2,2,
2,2,2,2,2,2,2,2,2,2,2,2,2,2,2,2,2,2,2,2,2,2,2,2,2,2,2,2,2,2,2,2,2,2,2,2,
2,2,2,2,2,2,2,2,2,2,2,2,2,2,2,2,2,2,2,2,2,2,2,2,2,2,2,2,2,2,2,2,2,2,2,2,
2,2,2,2,2,2,2,2,2,2,4),(0.000817343104692811,0.0612264047101083,0.0876739253814859,
0.0938319268654868,0.0964930162299291,0.098445887033816,0.100248397018484,
0.103168945834367,0.110389872091982,0.154219030417253,0.195392564819818,
0.199211984485171,0.201237223955867,0.202548919747056,0.203772670562241,
0.203776236263053,0.203779814524098,0.20378340541055,0.203787237992897,
0.203791132332205,0.203795089702009,0.203799111357241,0.203803198731046,
0.203807353328477,0.203811576507947,0.203815869861654,0.203820234884912,
0.203824673218311,0.20382918641534,0.20383377623661,0.204877042706698,0.206251542867918,
0.209094350699173,0.231552325634205,0.272263518415933,0.29947632210628,
0.305729177081129,0.308406798604377,0.310362684358796,0.312161608637725,
0.315062199518276,0.322163428537016,0.37162248936672,0.410140140515592,
0.413726291685597,0.415237092776774,0.41632939331663,0.41735453176652,0.419094348826339,
0.42380681086065,0.464614149582666,0.511274379443645,0.517666451742583,
0.520367885181392,0.522328061222922,0.524121872451105,0.526994349817061,
0.533925999287603,0.586379560045428,0.612743989316309,0.624165792435812,
0.626444644865933,0.627702346735141,0.628773430477803,0.630119115555004,
0.632731680126114,0.648588061810793,0.653230360564274,0.711106002460536,
0.727399678916953,0.731188904258926,0.733381484591536,0.735294899668541,
0.73765755804755,0.741270258057818,0.75806104322685,0.765486199005169,0.823507764376126,
0.836082559142699,0.838423097235704,0.839694161009163,0.840764403263711,
0.842093705700601,0.844152313225193,0.853875391593583,0.859629710644237,
0.860066731061031,0.866951568986201,0.880676935212725,0.913533708533091,
0.930093487515048,0.940403527685748,0.943652061627753,0.945725310926782,
0.947665949537185,0.950207109337411,0.95450221041078,0.989624794075012,
1.03854983994315,1.04832431369406,1.05050077144486,1.05173621513491,1.05280996133788,
1.05418713675854,1.05704263399532,1.07982093558274,1.09266381887799,1.12551551786689,
1.14206672793493,1.15237319094318,1.15562153351618,1.15769488558872,1.15963577840455,
1.16217749907585,1.16647405925301,1.20167709949866,1.2508531702071,1.26008679584093),
 .UNSPECIFIED.);
#2023=B_SPLINE_CURVE_WITH_KNOTS('',3,(#199528,#199529,#199530,#199531,#199532,
#199533,#199534,#199535,#199536,#199537),.UNSPECIFIED.,.F.,.F.,(4,1,1,1,
1,1,1,4),(-98.0888186411165,-97.8859720962637,-96.8871356463018,-95.8882991963399,
-94.889462746378,-93.8906262964161,-92.8917898464543,-92.1566392082287),
 .UNSPECIFIED.);
#2024=B_SPLINE_CURVE_WITH_KNOTS('',3,(#199538,#199539,#199540,#199541,#199542,
#199543,#199544,#199545,#199546,#199547,#199548,#199549,#199550,#199551,
#199552,#199553,#199554,#199555,#199556,#199557),.UNSPECIFIED.,.F.,.F.,
(4,2,2,2,2,2,2,2,2,4),(0.000629224934217057,0.0465168723163532,0.0540117796467721,
0.0579010153661128,0.0612291109511265,0.0633196903264559,0.0652535612880513,
0.0677533146320536,0.0719070152574981,0.0751024976388681),.UNSPECIFIED.);
#2025=B_SPLINE_CURVE_WITH_KNOTS('',3,(#199562,#199563,#199564,#199565,#199566,
#199567,#199568,#199569,#199570,#199571,#199572,#199573,#199574,#199575,
#199576,#199577,#199578,#199579,#199580,#199581,#199582,#199583,#199584,
#199585,#199586,#199587,#199588,#199589,#199590,#199591,#199592,#199593,
#199594,#199595,#199596,#199597,#199598,#199599,#199600,#199601,#199602,
#199603,#199604,#199605,#199606,#199607,#199608,#199609,#199610,#199611,
#199612,#199613,#199614,#199615,#199616,#199617,#199618,#199619,#199620,
#199621,#199622,#199623,#199624,#199625,#199626,#199627,#199628,#199629,
#199630,#199631,#199632,#199633,#199634,#199635,#199636,#199637,#199638,
#199639,#199640,#199641,#199642,#199643,#199644,#199645,#199646,#199647,
#199648,#199649,#199650,#199651,#199652,#199653,#199654,#199655,#199656,
#199657,#199658,#199659,#199660,#199661,#199662,#199663,#199664,#199665,
#199666,#199667,#199668,#199669,#199670,#199671,#199672,#199673,#199674,
#199675,#199676,#199677,#199678,#199679,#199680,#199681,#199682,#199683,
#199684,#199685,#199686,#199687,#199688,#199689,#199690,#199691,#199692,
#199693,#199694,#199695,#199696,#199697,#199698,#199699,#199700,#199701,
#199702,#199703,#199704,#199705,#199706,#199707,#199708,#199709,#199710,
#199711,#199712,#199713,#199714,#199715,#199716,#199717,#199718,#199719,
#199720,#199721,#199722,#199723,#199724,#199725,#199726,#199727,#199728,
#199729,#199730,#199731,#199732,#199733,#199734,#199735,#199736,#199737,
#199738,#199739,#199740,#199741,#199742,#199743,#199744,#199745,#199746,
#199747,#199748,#199749,#199750,#199751,#199752,#199753,#199754,#199755,
#199756,#199757,#199758,#199759,#199760,#199761,#199762,#199763,#199764,
#199765,#199766,#199767,#199768,#199769,#199770,#199771,#199772,#199773,
#199774,#199775,#199776,#199777,#199778,#199779,#199780,#199781,#199782,
#199783,#199784,#199785,#199786,#199787,#199788,#199789,#199790,#199791,
#199792,#199793,#199794,#199795,#199796,#199797,#199798,#199799),
 .UNSPECIFIED.,.F.,.F.,(4,2,2,2,2,2,2,2,2,2,2,2,2,2,2,2,2,2,2,2,2,2,2,2,
2,2,2,2,2,2,2,2,2,2,2,2,2,2,2,2,2,2,2,2,2,2,2,2,2,2,2,2,2,2,2,2,2,2,2,2,
2,2,2,2,2,2,2,2,2,2,2,2,2,2,2,2,2,2,2,2,2,2,2,2,2,2,2,2,2,2,2,2,2,2,2,2,
2,2,2,2,2,2,2,2,2,2,2,2,2,2,2,2,2,2,2,2,2,2,4),(1.26019912898447,1.26516552744649,
1.27565047414906,1.27891977403079,1.28099812674898,1.28293784845713,1.28546963111691,
1.28973065308912,1.33473149857969,1.37978354292382,1.38450885614848,1.38625119796463,
1.38727721581579,1.3883699387183,1.38988048343202,1.39346218127488,1.43110066479073,
1.48152458713467,1.48858328117212,1.49147776415741,1.49327630055056,1.49523446934483,
1.49792010342713,1.50421416472924,1.53175359299828,1.56015790678291,1.58248829887166,
1.59519545881556,1.59743605907672,1.59882112827533,1.59989596148789,1.60112697396055,
1.60328214404654,1.61274394989476,1.66193021659652,1.69713563666701,1.70143297964506,
1.703975274694,1.70591665926005,1.70799058726325,1.71123993661749,1.72155038971792,
1.73811107015389,1.77100354210081,1.78473908951812,1.7916110515609,1.79182202413196,
1.79520272497235,1.80729365920458,1.80950106961012,1.8108760751632,1.81194986281409,
1.81318732329243,1.81537204712466,1.8252627572925,1.87407949047141,1.90916655087235,
1.91346207371923,1.91600374925331,1.91794492410745,1.92001888345942,1.92326881519186,
1.93358561205764,1.95016076026618,1.98306390245923,1.99797142940292,2.00296893744556,
2.01898174083656,2.02160193856687,2.02294953815711,2.02402108365242,2.0252781020688,
2.02755258658585,2.03888848731206,2.06490428416925,2.11784401249317,2.12474108952783,
2.12760847672961,2.12940180431983,2.13136362222565,2.13407128599487,2.1404968231754,
2.16913178685335,2.22043122728788,2.23149183504546,2.23363918612668,2.23499592480715,
2.2360681352172,2.2373183358121,2.23956141075427,2.25036457564538,2.27434880313221,
2.33029315208289,2.33692315238296,2.33946362183626,2.34129016054295,2.34322925368523,
2.3458027683106,2.35146696216876,2.37410175434962,2.40691975477404,2.44275877922739,
2.44562069758294,2.44699926424349,2.44803877475975,2.44923356683259,2.45050679225612,
2.45243871827031,2.45601143638465,2.46446957027703,2.52388921598066,2.54598478691587,
2.54991219363759,2.55237162506368,2.55429484554131,2.55642714249414,2.55994191654172,
2.57283594732367,2.59411274951175),.UNSPECIFIED.);
#2026=B_SPLINE_CURVE_WITH_KNOTS('',3,(#199800,#199801,#199802,#199803,#199804,
#199805,#199806,#199807,#199808,#199809,#199810,#199811,#199812,#199813,
#199814,#199815,#199816,#199817,#199818,#199819,#199820,#199821,#199822,
#199823,#199824,#199825,#199826,#199827,#199828,#199829,#199830,#199831,
#199832,#199833,#199834,#199835,#199836,#199837,#199838,#199839,#199840,
#199841,#199842,#199843,#199844,#199845,#199846,#199847,#199848,#199849,
#199850,#199851,#199852,#199853,#199854,#199855,#199856,#199857,#199858,
#199859,#199860,#199861,#199862,#199863,#199864,#199865,#199866,#199867,
#199868,#199869,#199870,#199871,#199872,#199873,#199874,#199875,#199876,
#199877,#199878,#199879,#199880,#199881,#199882,#199883,#199884,#199885,
#199886,#199887,#199888,#199889,#199890,#199891,#199892,#199893,#199894,
#199895,#199896,#199897,#199898,#199899,#199900,#199901,#199902,#199903,
#199904,#199905,#199906,#199907,#199908,#199909,#199910,#199911,#199912,
#199913,#199914,#199915,#199916,#199917,#199918,#199919,#199920,#199921,
#199922,#199923,#199924,#199925,#199926,#199927,#199928,#199929,#199930,
#199931,#199932,#199933,#199934,#199935,#199936,#199937,#199938,#199939,
#199940,#199941,#199942,#199943,#199944,#199945,#199946,#199947,#199948,
#199949,#199950,#199951,#199952,#199953,#199954,#199955,#199956,#199957,
#199958,#199959,#199960,#199961,#199962,#199963,#199964,#199965,#199966,
#199967,#199968,#199969,#199970,#199971,#199972,#199973,#199974,#199975,
#199976,#199977,#199978,#199979,#199980,#199981,#199982,#199983,#199984,
#199985,#199986,#199987,#199988,#199989,#199990,#199991,#199992,#199993,
#199994,#199995,#199996,#199997,#199998,#199999,#200000,#200001,#200002,
#200003,#200004,#200005,#200006,#200007,#200008,#200009,#200010,#200011,
#200012,#200013,#200014,#200015,#200016,#200017,#200018,#200019,#200020,
#200021,#200022,#200023),.UNSPECIFIED.,.F.,.F.,(4,2,2,2,2,2,2,2,2,2,2,2,
2,2,2,2,2,2,2,2,2,2,2,2,2,2,2,2,2,2,2,2,2,2,2,2,2,2,2,2,2,2,2,2,2,2,2,2,
2,2,2,2,2,2,2,2,2,2,2,2,2,2,2,2,2,2,2,2,2,2,2,2,2,2,2,2,2,2,2,2,2,2,2,2,
2,2,2,2,2,2,2,2,2,2,2,2,2,2,2,2,2,2,2,2,2,2,2,2,2,2,2,4),(0.0751024976388681,
0.100173146895298,0.113801182309511,0.129357242395927,0.154621270231427,
0.16574502811648,0.168013829907005,0.169270713533231,0.170341757364332,
0.171688227814516,0.174304768538712,0.190264821349283,0.195792699913727,
0.252782593681776,0.268941064366794,0.27273664188936,0.274930502925903,
0.276843613715273,0.279204068839098,0.282809998823665,0.299513718575246,
0.30701523152462,0.355518416127759,0.370247953838068,0.378141906569891,
0.380173618302696,0.381376818270048,0.382456614250652,0.383863547667469,
0.38622998851002,0.401654001311554,0.405922021285589,0.448897014545642,
0.476829270098281,0.483169635994594,0.485862175594031,0.487820654124135,
0.489616203486893,0.49249867592284,0.499491545958294,0.551012816803328,
0.578035821914904,0.589621346486818,0.591909302009542,0.593168926512293,
0.594239777664312,0.59558279881323,0.598183268064083,0.613748740242112,
0.620207314566039,0.661617986531234,0.688887761373014,0.695147609107977,
0.697826437144618,0.699782539677545,0.701581200064785,0.704480340061765,
0.711572868475071,0.761226455833534,0.799536600739436,0.803140683842643,
0.804654538342414,0.805747372631676,0.806771681940235,0.808507261882338,
0.813191793391958,0.854271180339101,0.900697354279703,0.907088807858633,
0.90979014053422,0.911750302102162,0.913544140542142,0.91641674981925,0.923349173805305,
0.975792202674048,1.00216420832525,1.01358792934847,1.01586689475685,1.01712462306176,
1.01819570758363,1.01954136601911,1.02215379793928,1.0380040447313,1.04274741961133,
1.05802455246317,1.09089766918535,1.10747811641254,1.11779738653335,1.12104689433375,
1.12312030072295,1.12506076024193,1.12760121510776,1.13189407062283,1.17429131127521,
1.20334665408896,1.2229611694138,1.22691606494033,1.22848762138044,1.22959112098465,
1.23060151308425,1.23226500850481,1.23648980762861,1.28582954827231,1.32659526345396,
1.33166117468821,1.33412063709304,1.33604348664034,1.33817496755308,1.34168746194444,
1.35456256393462,1.37726334489159,1.40841236097604),.UNSPECIFIED.);
#2027=B_SPLINE_CURVE_WITH_KNOTS('',3,(#200029,#200030,#200031,#200032),
 .UNSPECIFIED.,.F.,.F.,(4,4),(114.406674973168,114.756144668717),
 .UNSPECIFIED.);
#2028=B_SPLINE_CURVE_WITH_KNOTS('',3,(#200033,#200034,#200035,#200036,#200037,
#200038,#200039,#200040,#200041,#200042,#200043,#200044,#200045,#200046,
#200047,#200048,#200049,#200050,#200051,#200052,#200053,#200054,#200055,
#200056,#200057,#200058,#200059,#200060,#200061,#200062,#200063,#200064,
#200065,#200066,#200067,#200068,#200069,#200070,#200071,#200072,#200073,
#200074,#200075,#200076,#200077,#200078,#200079,#200080,#200081,#200082,
#200083,#200084,#200085,#200086,#200087,#200088,#200089,#200090,#200091,
#200092,#200093,#200094,#200095,#200096,#200097,#200098,#200099,#200100,
#200101,#200102,#200103,#200104,#200105,#200106,#200107,#200108,#200109,
#200110,#200111,#200112,#200113,#200114,#200115,#200116,#200117,#200118,
#200119,#200120,#200121,#200122,#200123,#200124,#200125,#200126,#200127,
#200128,#200129,#200130,#200131,#200132,#200133,#200134,#200135,#200136,
#200137,#200138,#200139,#200140,#200141,#200142,#200143,#200144,#200145,
#200146,#200147,#200148,#200149,#200150,#200151,#200152,#200153,#200154,
#200155,#200156,#200157,#200158,#200159,#200160,#200161,#200162,#200163,
#200164,#200165,#200166,#200167,#200168,#200169,#200170,#200171,#200172,
#200173,#200174,#200175,#200176,#200177,#200178,#200179,#200180,#200181,
#200182,#200183,#200184,#200185,#200186,#200187,#200188,#200189,#200190,
#200191,#200192,#200193,#200194,#200195,#200196,#200197,#200198,#200199,
#200200,#200201,#200202,#200203,#200204,#200205,#200206,#200207,#200208,
#200209,#200210,#200211,#200212,#200213,#200214,#200215,#200216,#200217,
#200218,#200219,#200220,#200221,#200222,#200223,#200224,#200225,#200226,
#200227,#200228,#200229,#200230,#200231,#200232,#200233,#200234,#200235,
#200236,#200237,#200238,#200239,#200240,#200241,#200242,#200243,#200244,
#200245,#200246,#200247,#200248,#200249,#200250,#200251,#200252),
 .UNSPECIFIED.,.F.,.F.,(4,2,2,2,2,2,2,2,2,2,2,2,2,2,2,2,2,2,2,2,2,2,2,2,
2,2,2,2,2,2,2,2,2,2,2,2,2,2,2,2,2,2,2,2,2,2,2,2,2,2,2,2,2,2,2,2,2,2,2,2,
2,2,2,2,2,2,2,2,2,2,2,2,2,2,2,2,2,2,2,2,2,2,2,2,2,2,2,2,2,2,2,2,2,2,2,2,
2,2,2,2,2,2,2,2,2,2,2,2,2,4),(0.000658788894674154,0.00332970132034127,
0.00592165829033243,0.00778879648581875,0.00964368923404936,0.0114909184853086,
0.0146445377053462,0.0233614970618546,0.092229541711162,0.109144084551986,
0.112803141256342,0.114326472957728,0.115421149470292,0.116443232178583,
0.118166704238405,0.122770276101425,0.165872185719283,0.208362522370533,
0.213664594158701,0.216707561179275,0.218819371417798,0.220855490232865,
0.222735969728323,0.225227342514191,0.229351510339336,0.256647990146848,
0.299685109788396,0.315418438681117,0.323672694298771,0.32573518356848,
0.326945458119776,0.328023929938131,0.329419151128872,0.331744783434459,
0.346117811018334,0.35471782018955,0.367795135811537,0.400650498847912,
0.417205081784512,0.427513198543129,0.430761824601561,0.432835300478543,
0.434776269046985,0.437318030994917,0.441614531091708,0.476730751585137,
0.525632470784906,0.535444939306928,0.53762421666097,0.538860394860561,
0.539934225817554,0.541310786866089,0.544162526319072,0.580485084603969,
0.63432567418599,0.640783781255109,0.643496853714483,0.645459583395521,
0.647251682948482,0.650112617667215,0.65697091859575,0.710435266942078,
0.736113857521736,0.747362715689847,0.749632144645471,0.750888030278971,
0.751959623668511,0.753308568550604,0.755935169058406,0.772041733613367,
0.77251762365382,0.823030705846806,0.840706703734584,0.851514906899761,
0.854819828013481,0.856905747406168,0.858842114811428,0.861354716666702,
0.865550838001097,0.895444937635017,0.94730779998003,0.959334192030385,
0.961646875854829,0.962912173502525,0.963983109465477,0.965320260546943,
0.967403656729176,0.977474780762184,0.982987097800833,0.99237762543089,
1.00394871724414,1.03679626470523,1.05333776343544,1.06364040669498,1.06688873198901,
1.06896235837823,1.07090370849627,1.07344631743539,1.07774502806268,1.11305593701797,
1.16231140812583,1.1716492636795,1.17379556394198,1.17502460294623,1.17609973025966,
1.17748782717431,1.18039792620084,1.20852959895016,1.24821969646968,1.26019912898447),
 .UNSPECIFIED.);
#2029=B_SPLINE_CURVE_WITH_KNOTS('',3,(#200254,#200255,#200256,#200257,#200258,
#200259,#200260,#200261,#200262,#200263,#200264,#200265,#200266,#200267,
#200268,#200269,#200270,#200271,#200272,#200273,#200274,#200275,#200276,
#200277,#200278,#200279,#200280,#200281,#200282,#200283,#200284,#200285,
#200286,#200287,#200288,#200289,#200290,#200291,#200292,#200293,#200294,
#200295,#200296,#200297,#200298,#200299,#200300,#200301,#200302,#200303,
#200304,#200305,#200306,#200307,#200308,#200309,#200310,#200311,#200312,
#200313,#200314,#200315,#200316,#200317,#200318,#200319,#200320,#200321,
#200322,#200323,#200324,#200325,#200326,#200327,#200328,#200329,#200330,
#200331,#200332,#200333,#200334,#200335,#200336,#200337,#200338,#200339,
#200340,#200341,#200342,#200343,#200344,#200345,#200346,#200347,#200348,
#200349,#200350,#200351,#200352,#200353,#200354,#200355,#200356,#200357,
#200358,#200359,#200360,#200361,#200362,#200363,#200364,#200365,#200366,
#200367,#200368,#200369,#200370,#200371,#200372,#200373,#200374,#200375,
#200376,#200377,#200378,#200379,#200380,#200381,#200382,#200383,#200384,
#200385,#200386,#200387,#200388,#200389,#200390,#200391,#200392,#200393,
#200394,#200395,#200396,#200397,#200398,#200399,#200400,#200401,#200402,
#200403,#200404,#200405,#200406,#200407,#200408,#200409,#200410,#200411,
#200412,#200413,#200414,#200415,#200416,#200417,#200418,#200419,#200420,
#200421,#200422,#200423,#200424,#200425,#200426,#200427,#200428,#200429,
#200430,#200431,#200432,#200433,#200434,#200435,#200436,#200437,#200438,
#200439,#200440,#200441,#200442,#200443,#200444,#200445,#200446,#200447,
#200448,#200449,#200450,#200451,#200452,#200453,#200454,#200455,#200456,
#200457,#200458,#200459,#200460,#200461,#200462,#200463,#200464,#200465,
#200466,#200467,#200468,#200469,#200470,#200471),.UNSPECIFIED.,.F.,.F.,
(4,2,2,2,2,2,2,2,2,2,2,2,2,2,2,2,2,2,2,2,2,2,2,2,2,2,2,2,2,2,2,2,2,2,2,
2,2,2,2,2,2,2,2,2,2,2,2,2,2,2,2,2,2,2,2,2,2,2,2,2,2,2,2,2,2,2,2,2,2,2,2,
2,2,2,2,2,2,2,2,2,2,2,2,2,2,2,2,2,2,2,2,2,2,2,2,2,2,2,2,2,2,2,2,2,2,2,2,
2,4),(1.40841236097604,1.41585081406069,1.42084495972905,1.43685104509067,
1.43947024757663,1.44081735202331,1.44188851260067,1.44314508967006,1.445418801523,
1.45675138344984,1.48276078399497,1.53567732968201,1.54257225267126,1.54543866432514,
1.54723135854491,1.54919246489714,1.55189911235796,1.55832207571103,1.58694450706505,
1.63822367807732,1.64928437009302,1.65143120163553,1.65278753024501,1.65385936201447,
1.65510905838423,1.6573510722311,1.66814613729271,1.69210614285944,1.74805427396802,
1.75467945962303,1.7572186345253,1.759044417037,1.76098286815877,1.76355580451578,
1.76921984354574,1.79186040852704,1.82467554360162,1.82894784270214,1.8603909912648,
1.86330242500633,1.8646903486468,1.86576496494066,1.86699300744002,1.86913658671504,
1.87844771779498,1.92759189116734,1.96295389057885,1.96725105524298,1.96979258787608,
1.9717330120747,1.97380554763751,1.97705195047991,1.98734661357816,2.00387581172515,
2.03673162265381,2.04840005046803,2.0570704174793,2.07274531215951,2.07535037524001,
2.07669433642549,2.07776517879802,2.07902391684396,2.08130800879691,2.0928269691322,
2.11958001108092,2.17143120860544,2.17839959343032,2.18127790274253,2.18307261111663,
2.1850315782303,2.18772734339576,2.19408722180299,2.25006525654493,2.27220693590807,
2.28496370072602,2.28720592872981,2.28859105841952,2.28966533389733,2.29089502958668,
2.29304629673985,2.30246579198581,2.35165424156335,2.38684772922228,2.39114259589775,
2.39368338998927,2.39562360765204,2.39769626899719,2.40094359186727,2.41104270525211,
2.42722893507529,2.46891343386274,2.49623218564847,2.49913555813965,2.50052184689885,
2.50159621630899,2.50282511775341,2.50411851950549,2.50878390124864,2.53289345834914,
2.55378951587328,2.59882588228687,2.60308236521915,2.60561202494915,2.60755044214656,
2.6096277104179,2.61289596265875,2.61669868245321,2.62396228455341,2.66758385820486),
 .UNSPECIFIED.);
#2030=B_SPLINE_CURVE_WITH_KNOTS('',3,(#200472,#200473,#200474,#200475,#200476,
#200477,#200478,#200479,#200480,#200481,#200482,#200483,#200484,#200485,
#200486,#200487,#200488,#200489,#200490,#200491),.UNSPECIFIED.,.F.,.F.,
(4,2,2,2,2,2,2,2,2,4),(0.000649992924200273,0.037515273389423,0.0412926063506684,
0.0433020337866211,0.0446072154259599,0.0458444190226681,0.0469177316247823,
0.0482917908521054,0.0511320595409267,0.0747588858459464),.UNSPECIFIED.);
#2031=B_SPLINE_CURVE_WITH_KNOTS('',3,(#200497,#200498,#200499,#200500,#200501,
#200502,#200503,#200504,#200505,#200506),.UNSPECIFIED.,.F.,.F.,(4,3,3,4),
(120.689857252469,120.859210445387,120.962579625184,121.040543977909),
 .UNSPECIFIED.);
#2032=B_SPLINE_CURVE_WITH_KNOTS('',3,(#200507,#200508,#200509,#200510,#200511,
#200512,#200513,#200514,#200515,#200516),.UNSPECIFIED.,.F.,.F.,(4,1,1,1,
1,1,1,4),(114.756144668717,114.866191745616,115.865028195577,116.863864645539,
117.862701095501,118.861537545463,119.860373995425,120.689851223097),
 .UNSPECIFIED.);
#2033=B_SPLINE_CURVE_WITH_KNOTS('',3,(#200517,#200518,#200519,#200520,#200521,
#200522,#200523,#200524,#200525,#200526,#200527,#200528,#200529,#200530,
#200531,#200532,#200533,#200534,#200535,#200536,#200537,#200538,#200539,
#200540,#200541,#200542,#200543,#200544,#200545,#200546,#200547,#200548,
#200549,#200550,#200551,#200552,#200553,#200554,#200555,#200556,#200557,
#200558,#200559,#200560,#200561,#200562,#200563,#200564,#200565,#200566,
#200567,#200568,#200569,#200570,#200571,#200572,#200573,#200574,#200575,
#200576,#200577,#200578,#200579,#200580,#200581,#200582,#200583,#200584,
#200585,#200586,#200587,#200588,#200589,#200590,#200591,#200592,#200593,
#200594,#200595,#200596,#200597,#200598,#200599,#200600,#200601,#200602,
#200603,#200604,#200605,#200606,#200607,#200608,#200609,#200610,#200611,
#200612,#200613,#200614,#200615,#200616,#200617,#200618,#200619,#200620,
#200621,#200622,#200623,#200624,#200625,#200626,#200627,#200628,#200629,
#200630,#200631,#200632,#200633,#200634,#200635,#200636,#200637,#200638,
#200639,#200640,#200641,#200642,#200643,#200644,#200645,#200646,#200647,
#200648,#200649,#200650,#200651,#200652,#200653,#200654,#200655,#200656,
#200657,#200658,#200659,#200660,#200661,#200662,#200663,#200664,#200665,
#200666,#200667,#200668,#200669,#200670,#200671,#200672,#200673,#200674,
#200675,#200676,#200677,#200678,#200679,#200680,#200681,#200682,#200683,
#200684,#200685,#200686,#200687,#200688,#200689,#200690,#200691,#200692,
#200693,#200694,#200695,#200696,#200697,#200698,#200699,#200700,#200701,
#200702,#200703,#200704,#200705,#200706,#200707,#200708,#200709,#200710,
#200711,#200712,#200713,#200714,#200715,#200716,#200717,#200718,#200719,
#200720,#200721,#200722,#200723,#200724,#200725,#200726,#200727,#200728,
#200729,#200730,#200731,#200732,#200733,#200734),.UNSPECIFIED.,.F.,.F.,
(4,2,2,2,2,2,2,2,2,2,2,2,2,2,2,2,2,2,2,2,2,2,2,2,2,2,2,2,2,2,2,2,2,2,2,
2,2,2,2,2,2,2,2,2,2,2,2,2,2,2,2,2,2,2,2,2,2,2,2,2,2,2,2,2,2,2,2,2,2,2,2,
2,2,2,2,2,2,2,2,2,2,2,2,2,2,2,2,2,2,2,2,2,2,2,2,2,2,2,2,2,2,2,2,2,2,2,2,
2,4),(0.0747588858459464,0.0879797100071701,0.109399210605851,0.1361824288672,
0.146436093238305,0.149706957161066,0.151785046590808,0.1537236459466,0.156252708008424,
0.160506359700356,0.193188587404338,0.222560667390916,0.244175416228302,
0.254295391077272,0.256485297263878,0.25773343018092,0.258805433744377,
0.260163916946221,0.262836074139897,0.280219844032183,0.329263015910941,
0.34730554909262,0.3545735683608,0.360002510934368,0.362567737056095,0.364505076273853,
0.366333274476484,0.368881377847341,0.375563261598372,0.430967218228503,
0.45531854455265,0.466218383893618,0.468466837905448,0.469717974758843,
0.470789723056959,0.472144248604246,0.474885982334562,0.493328942238641,
0.537460382854009,0.565331826300443,0.57166532396708,0.574356959584286,
0.576315520801497,0.578111658932356,0.580996202893888,0.587999848161857,
0.639384588344836,0.666515502702058,0.678128415070438,0.680418167992362,
0.681678308392531,0.682749313041741,0.684092165345215,0.68669125548634,
0.702216899000038,0.708760971634423,0.72263387812871,0.755493941726029,
0.772056444543111,0.782367868914643,0.785616673179452,0.787690055163526,
0.789630789989735,0.792172035406727,0.796467190705044,0.831578304350796,
0.880465439404303,0.890288614785536,0.892468472230853,0.893704703836293,
0.894778405091688,0.896154569949096,0.899004699646103,0.93537456298567,
0.989163016853752,0.99561907129515,0.998331639332602,1.00029413354789,1.00208610698246,
1.00494703321247,1.01180631146846,1.06524491881451,1.09093516386653,1.10218656064975,
1.10445597823434,1.10571178682071,1.10678327142763,1.10813202452887,1.11075808991063,
1.12692228326169,1.17758027648585,1.20199424684519,1.20789426565626,1.21051032975775,
1.21245602804851,1.21427042462654,1.21676503388208,1.2231148806821,1.28150383668905,
1.3039545071262,1.31433172996214,1.31654813469475,1.31779242056303,1.31886514467892,
1.32022973899236,1.32240314909759,1.3338998499708,1.38263544072133,1.40832418655118),
 .UNSPECIFIED.);
#2034=B_SPLINE_CURVE_WITH_KNOTS('',3,(#200740,#200741,#200742,#200743,#200744,
#200745,#200746,#200747),.UNSPECIFIED.,.F.,.F.,(4,2,2,4),(2.5938719493606,
2.59862224991634,2.62666588587967,2.66835909139805),.UNSPECIFIED.);
#2035=B_SPLINE_CURVE_WITH_KNOTS('',3,(#200748,#200749,#200750,#200751,#200752,
#200753,#200754,#200755,#200756,#200757,#200758,#200759,#200760,#200761,
#200762,#200763,#200764,#200765,#200766,#200767,#200768,#200769,#200770,
#200771,#200772,#200773,#200774,#200775,#200776,#200777,#200778,#200779,
#200780,#200781,#200782,#200783,#200784,#200785,#200786,#200787,#200788,
#200789,#200790,#200791,#200792,#200793,#200794,#200795,#200796,#200797,
#200798,#200799,#200800,#200801,#200802,#200803,#200804,#200805,#200806,
#200807,#200808,#200809,#200810,#200811,#200812,#200813,#200814,#200815,
#200816,#200817,#200818,#200819,#200820,#200821,#200822,#200823,#200824,
#200825,#200826,#200827,#200828,#200829,#200830,#200831,#200832,#200833,
#200834,#200835,#200836,#200837,#200838,#200839,#200840,#200841,#200842,
#200843,#200844,#200845,#200846,#200847,#200848,#200849,#200850,#200851,
#200852,#200853,#200854,#200855,#200856,#200857,#200858,#200859,#200860,
#200861,#200862,#200863,#200864,#200865,#200866,#200867,#200868,#200869,
#200870,#200871,#200872,#200873,#200874,#200875,#200876,#200877,#200878,
#200879,#200880,#200881,#200882,#200883,#200884,#200885,#200886,#200887,
#200888,#200889,#200890,#200891,#200892,#200893,#200894,#200895,#200896,
#200897,#200898,#200899,#200900,#200901,#200902,#200903,#200904,#200905,
#200906,#200907,#200908,#200909,#200910,#200911,#200912,#200913,#200914,
#200915,#200916,#200917,#200918,#200919,#200920,#200921,#200922,#200923,
#200924,#200925),.UNSPECIFIED.,.F.,.F.,(4,3,3,3,3,3,3,3,3,3,3,3,3,3,3,3,
3,3,3,3,3,3,3,3,3,3,3,3,3,3,3,3,3,3,3,3,3,3,3,3,3,3,3,3,3,3,3,3,3,3,3,3,
3,3,3,3,3,3,3,4),(121.040543977909,121.143685186123,121.246752639545,121.34978039127,
121.452802442928,121.555926066816,121.659098529552,121.762462041336,121.858046895349,
121.961441632397,122.064682914512,122.167802879905,122.270857448114,122.373880656471,
122.476906499144,122.580039265922,122.683228357332,122.786600350714,122.856883345311,
122.960278082359,123.063519364473,123.166639329866,123.269693898074,123.372717106432,
123.475742949104,123.578875715882,123.682064807291,123.785436800673,123.855719795272,
123.95911453232,124.062355814435,124.165475779827,124.268530348036,124.371553556394,
124.474579399066,124.577712165844,124.680901257254,124.784273250636,124.854556245234,
124.957950982282,125.061192264397,125.16431222979,125.267366797999,125.370390006357,
125.473415849029,125.576548615808,125.679737707218,125.783109700599,125.853392695196,
125.956787432244,126.060028714359,126.163148679751,126.26620324796,126.369226456318,
126.472252298991,126.575385065769,126.678574157179,126.78194615056,126.852229145158,
126.973042559648),.UNSPECIFIED.);
#2036=B_SPLINE_CURVE_WITH_KNOTS('',3,(#200927,#200928,#200929,#200930,#200931,
#200932,#200933,#200934,#200935,#200936,#200937,#200938,#200939,#200940,
#200941,#200942,#200943,#200944,#200945,#200946,#200947,#200948,#200949,
#200950,#200951,#200952,#200953,#200954,#200955,#200956,#200957,#200958,
#200959,#200960,#200961,#200962,#200963,#200964,#200965,#200966,#200967,
#200968,#200969,#200970,#200971,#200972,#200973,#200974,#200975,#200976,
#200977,#200978,#200979,#200980,#200981,#200982,#200983,#200984,#200985,
#200986,#200987,#200988,#200989,#200990,#200991,#200992,#200993,#200994,
#200995,#200996,#200997,#200998,#200999,#201000,#201001,#201002,#201003,
#201004,#201005,#201006,#201007,#201008,#201009,#201010,#201011,#201012,
#201013,#201014,#201015,#201016,#201017,#201018,#201019,#201020,#201021,
#201022,#201023,#201024,#201025,#201026,#201027,#201028,#201029,#201030,
#201031,#201032,#201033,#201034,#201035,#201036,#201037,#201038,#201039,
#201040,#201041,#201042,#201043,#201044,#201045,#201046,#201047,#201048,
#201049,#201050,#201051,#201052,#201053,#201054,#201055,#201056,#201057,
#201058,#201059,#201060,#201061,#201062,#201063,#201064,#201065,#201066,
#201067,#201068,#201069,#201070,#201071,#201072,#201073,#201074,#201075,
#201076,#201077,#201078,#201079,#201080,#201081,#201082,#201083,#201084,
#201085,#201086,#201087,#201088,#201089,#201090,#201091,#201092,#201093,
#201094,#201095,#201096,#201097,#201098,#201099,#201100,#201101,#201102,
#201103,#201104,#201105,#201106,#201107,#201108,#201109,#201110,#201111,
#201112,#201113,#201114,#201115,#201116,#201117,#201118,#201119,#201120,
#201121,#201122,#201123,#201124,#201125,#201126,#201127,#201128,#201129,
#201130,#201131,#201132,#201133,#201134,#201135,#201136,#201137,#201138,
#201139,#201140,#201141,#201142,#201143,#201144,#201145,#201146,#201147,
#201148,#201149,#201150,#201151,#201152,#201153,#201154,#201155,#201156,
#201157,#201158,#201159,#201160,#201161,#201162,#201163,#201164,#201165,
#201166,#201167,#201168,#201169,#201170,#201171,#201172,#201173,#201174,
#201175,#201176,#201177,#201178,#201179,#201180,#201181,#201182,#201183,
#201184,#201185,#201186,#201187,#201188,#201189,#201190),.UNSPECIFIED.,
 .F.,.F.,(4,2,2,2,2,2,2,2,2,2,2,2,2,2,2,2,2,2,2,2,2,2,2,2,2,2,2,2,2,2,2,
2,2,2,2,2,2,2,2,2,2,2,2,2,2,2,2,2,2,2,2,2,2,2,2,2,2,2,2,2,2,2,2,2,2,2,2,
2,2,2,2,2,2,2,2,2,2,2,2,2,2,2,2,2,2,2,2,2,2,2,2,2,2,2,2,2,2,2,2,2,2,2,2,
2,2,2,2,2,2,2,2,2,2,2,2,2,2,2,2,2,2,2,2,2,2,2,2,2,2,2,2,4),(1.40832418655118,
1.41583872157815,1.42010257572939,1.4226348669936,1.42457428742719,1.42665164267686,
1.42991795340268,1.44038101522293,1.4572819688539,1.49511046458649,1.52518585406619,
1.52810044555585,1.5294892222838,1.53056419895257,1.53179231764653,1.53393524396405,
1.54323139990793,1.56207794175142,1.60247841650693,1.61474051057434,1.62934634609348,
1.63313462366128,1.63534961323343,1.63726187255969,1.63959690251243,1.64404682602657,
1.67495957322253,1.72180664623564,1.73760389838481,1.7402163798589,1.74156226399387,
1.74263363332685,1.74389182374998,1.74617194177872,1.75760855961769,1.78402411855815,
1.83638765294265,1.8433261011902,1.84620018155187,1.8479946416121,1.849955250322,
1.85265676724047,1.85904660892856,1.88738479009089,1.93728384336638,1.94991437905467,
1.9521506667732,1.95353430165758,1.95460881103608,1.95584033888736,1.95799850500166,
1.96750669461709,2.01664172526128,2.05182798614575,2.05612434747821,2.05866610990359,
2.06060711544705,2.06268066541234,2.06592947855171,2.0762387027851,2.09279785893303,
2.12568540440676,2.13955073775261,2.14611503786987,2.16166396020909,2.16426434365899,
2.16560757339552,2.16667872461248,2.16793886303792,2.17022815481917,2.18182958993675,
2.20890891976209,2.26033584398661,2.26733480309933,2.2702187914972,2.27201499178972,
2.27397395214511,2.2766667313089,2.28300567537386,2.31092263620224,2.35691900429129,
2.3582212446484,2.37368714132845,2.3760558649217,2.37746369558322,2.37854390485505,
2.37974727321361,2.38177861880869,2.38966330880926,2.40436315051192,2.44559174097471,
2.47594830264476,2.48016553672262,2.48268423140849,2.48462145646318,2.48469685162256,
2.48474248809897,2.48478674315558,2.48482687148383,2.48486331755192,2.48489646882688,
2.48492666434582,2.48495420342987,2.48497934912401,2.48500233407452,2.48502336466585,
2.48504262448749,2.48506027729796,2.48507646954186,2.48509922830073,2.4851215630853,
2.48514348550655,2.48516501052931,2.4851861509435,2.48520691907636,2.48522732673606,
2.48524738528785,2.48750364533091,2.49161544699482,2.4967486418115,2.50777948381343,
2.53230080123694,2.54783910363152,2.58533079090176,2.58816258109248,2.58953513216007,
2.59060849255101,2.59184714882272,2.59403805432889,2.60402580906601,2.65274977226297,
2.6674812874869),.UNSPECIFIED.);
#2037=B_SPLINE_CURVE_WITH_KNOTS('',3,(#201191,#201192,#201193,#201194,#201195,
#201196,#201197,#201198,#201199,#201200,#201201,#201202,#201203,#201204,
#201205,#201206,#201207,#201208,#201209,#201210,#201211,#201212),
 .UNSPECIFIED.,.F.,.F.,(4,2,2,2,2,2,2,2,2,2,4),(0.000768638562662975,0.0217328432260458,
0.0248352869314532,0.0269713212508239,0.0287705216612541,0.0306857495874429,
0.0330701219975814,0.0367527850347077,0.0546136258233204,0.0730984127855758,
0.0751664351648031),.UNSPECIFIED.);
#2038=B_SPLINE_CURVE_WITH_KNOTS('',3,(#201217,#201218,#201219,#201220,#201221,
#201222,#201223,#201224,#201225,#201226,#201227,#201228,#201229,#201230,
#201231,#201232,#201233,#201234,#201235,#201236,#201237,#201238,#201239,
#201240,#201241,#201242,#201243,#201244,#201245,#201246,#201247,#201248,
#201249,#201250,#201251,#201252,#201253,#201254,#201255,#201256,#201257,
#201258,#201259,#201260,#201261,#201262,#201263,#201264,#201265,#201266,
#201267,#201268,#201269,#201270,#201271,#201272,#201273,#201274,#201275,
#201276,#201277,#201278,#201279,#201280,#201281,#201282,#201283,#201284,
#201285,#201286,#201287,#201288,#201289,#201290,#201291,#201292,#201293,
#201294,#201295,#201296,#201297,#201298,#201299,#201300,#201301,#201302,
#201303,#201304,#201305,#201306,#201307,#201308,#201309,#201310,#201311,
#201312,#201313,#201314,#201315,#201316,#201317,#201318,#201319,#201320,
#201321,#201322,#201323,#201324,#201325,#201326,#201327,#201328,#201329,
#201330,#201331,#201332,#201333,#201334,#201335,#201336,#201337,#201338,
#201339,#201340,#201341,#201342,#201343,#201344,#201345,#201346,#201347,
#201348,#201349,#201350,#201351,#201352,#201353,#201354,#201355,#201356,
#201357,#201358,#201359,#201360,#201361,#201362,#201363,#201364,#201365,
#201366,#201367,#201368,#201369,#201370,#201371,#201372,#201373,#201374,
#201375,#201376,#201377,#201378,#201379,#201380,#201381,#201382,#201383,
#201384,#201385,#201386,#201387,#201388,#201389,#201390,#201391,#201392,
#201393,#201394,#201395,#201396,#201397,#201398,#201399,#201400,#201401,
#201402,#201403,#201404,#201405,#201406,#201407,#201408,#201409,#201410,
#201411,#201412,#201413,#201414,#201415,#201416,#201417,#201418,#201419,
#201420,#201421,#201422,#201423,#201424,#201425,#201426,#201427,#201428,
#201429,#201430,#201431,#201432,#201433,#201434,#201435,#201436,#201437,
#201438,#201439,#201440,#201441,#201442,#201443,#201444,#201445,#201446,
#201447,#201448,#201449,#201450,#201451,#201452),.UNSPECIFIED.,.F.,.F.,
(4,2,2,2,2,2,2,2,2,2,2,2,2,2,2,2,2,2,2,2,2,2,2,2,2,2,2,2,2,2,2,2,2,2,2,
2,2,2,2,2,2,2,2,2,2,2,2,2,2,2,2,2,2,2,2,2,2,2,2,2,2,2,2,2,2,2,2,2,2,2,2,
2,2,2,2,2,2,2,2,2,2,2,2,2,2,2,2,2,2,2,2,2,2,2,2,2,2,2,2,2,2,2,2,2,2,2,2,
2,2,2,2,2,2,2,2,2,2,4),(1.25996976443291,1.27817361085212,1.30767742298493,
1.31208784385346,1.31441477689738,1.3161418694476,1.31829830389366,1.32192113954004,
1.33437189970869,1.38533272483373,1.41654250559185,1.4194556905084,1.42084434731202,
1.4219194844673,1.42314806984404,1.42529247407934,1.43460529192529,1.48376433305904,
1.51915472469176,1.52345408005697,1.52599686704145,1.52793822513192,1.53001173511723,
1.53325961618488,1.54355856207559,1.56009425210006,1.59296459462998,1.60449112209311,
1.61424405337767,1.61613067747189,1.62921218400807,1.63147177164606,1.63286244468406,
1.63393772572315,1.63516489280432,1.63730312334334,1.64653235436676,1.66516775824721,
1.70928295141884,1.73178833335573,1.73573347955207,1.73819841855544,1.74012247611274,
1.74225215532024,1.74575445084859,1.75851110058937,1.78090243119528,1.82131909217728,
1.82560552285894,1.82817328265896,1.84121561111651,1.84347319952846,1.84486326513884,
1.84593847223012,1.84716599696492,1.84930588295451,1.85855805352352,1.87726537301691,
1.9214776507342,1.94380175410119,1.9477390887044,1.95020165156345,1.95212540689174,
1.95425633864387,1.95776434765773,1.97058270806592,1.99313317729192,2.0445576670405,
2.05370287779019,2.05591496086657,2.05717173628615,2.05824336245306,2.0595914236533,
2.06229969955907,2.08724550384447,2.13283196920506,2.15579518609972,2.15976036328525,
2.16223142123502,2.1641563080508,2.16628288744377,2.16977088182105,2.18237378370215,
2.23320115794848,2.26466186980415,2.26756932863816,2.26895689154742,2.2700319360336,
2.27126125988575,2.27340893395648,2.28276669661786,2.33204117454941,2.36727110126,
2.37156857205427,2.37411084201532,2.37605214943738,2.37812593881716,2.38137495363604,
2.39168335653041,2.40823980370276,2.47089936102958,2.47226100486589,2.47844116564448,
2.48038049069598,2.48156360485752,2.48259548735953,2.48400849450304,2.48702260108564,
2.49111903976041,2.50139060443183,2.52422264305586,2.57594785564152,2.58293221503037,
2.58581439829049,2.58761071994399,2.58957080718724,2.5922669462497,2.5938719493606),
 .UNSPECIFIED.);
#2039=B_SPLINE_CURVE_WITH_KNOTS('',3,(#201453,#201454,#201455,#201456,#201457,
#201458,#201459,#201460,#201461,#201462,#201463,#201464,#201465,#201466,
#201467,#201468,#201469,#201470,#201471,#201472,#201473,#201474,#201475,
#201476,#201477,#201478,#201479,#201480,#201481,#201482,#201483,#201484,
#201485,#201486,#201487,#201488,#201489,#201490,#201491,#201492,#201493,
#201494,#201495,#201496,#201497,#201498,#201499,#201500,#201501,#201502,
#201503,#201504,#201505,#201506,#201507,#201508,#201509,#201510,#201511,
#201512,#201513,#201514,#201515,#201516,#201517,#201518,#201519,#201520,
#201521,#201522,#201523,#201524,#201525,#201526,#201527,#201528,#201529,
#201530,#201531,#201532,#201533,#201534,#201535,#201536,#201537,#201538,
#201539,#201540,#201541,#201542,#201543,#201544,#201545,#201546,#201547,
#201548,#201549,#201550,#201551,#201552,#201553,#201554,#201555,#201556,
#201557,#201558,#201559,#201560,#201561,#201562,#201563,#201564,#201565,
#201566,#201567,#201568,#201569,#201570,#201571,#201572,#201573,#201574,
#201575,#201576,#201577,#201578,#201579,#201580,#201581,#201582,#201583,
#201584,#201585,#201586,#201587,#201588,#201589,#201590,#201591,#201592,
#201593,#201594,#201595,#201596,#201597,#201598,#201599,#201600,#201601,
#201602,#201603,#201604,#201605,#201606,#201607,#201608,#201609,#201610,
#201611,#201612,#201613,#201614,#201615,#201616,#201617,#201618,#201619,
#201620,#201621,#201622,#201623,#201624,#201625,#201626,#201627,#201628,
#201629,#201630,#201631,#201632,#201633,#201634,#201635,#201636,#201637,
#201638,#201639,#201640,#201641,#201642,#201643,#201644,#201645,#201646,
#201647,#201648,#201649,#201650,#201651,#201652,#201653,#201654,#201655,
#201656,#201657,#201658,#201659,#201660,#201661,#201662,#201663,#201664,
#201665,#201666,#201667,#201668,#201669,#201670,#201671,#201672,#201673,
#201674,#201675,#201676,#201677,#201678,#201679,#201680,#201681,#201682,
#201683,#201684,#201685,#201686,#201687,#201688,#201689,#201690),
 .UNSPECIFIED.,.F.,.F.,(4,2,2,2,2,2,2,2,2,2,2,2,2,2,2,2,2,2,2,2,2,2,2,2,
2,2,2,2,2,2,2,2,2,2,2,2,2,2,2,2,2,2,2,2,2,2,2,2,2,2,2,2,2,2,2,2,2,2,2,2,
2,2,2,2,2,2,2,2,2,2,2,2,2,2,2,2,2,2,2,2,2,2,2,2,2,2,2,2,2,2,2,2,2,2,2,2,
2,2,2,2,2,2,2,2,2,2,2,2,2,2,2,2,2,2,2,2,2,2,4),(0.0751664351648031,0.122346988242776,
0.131739194028345,0.133888806838276,0.135118276127824,0.1361928262999,0.137578921985736,
0.139823906855139,0.152628924282625,0.175045242086882,0.176210251072167,
0.208995272148526,0.225468169851392,0.232290879392018,0.237477834907157,
0.239949624495637,0.241788408939016,0.24361212485394,0.246142773384682,
0.252712751909429,0.30921693134264,0.33285432384443,0.34356160478676,0.345798534369181,
0.347047242671779,0.34811937263827,0.349477543323348,0.35163003158643,0.362779252651479,
0.413985155630467,0.442564674332054,0.44898357179459,0.451689848675295,
0.453651177127508,0.455444416017757,0.458312430817586,0.465214979187494,
0.518090453251227,0.544171167015094,0.555522174530228,0.557797297791336,
0.559054333708411,0.560125694169351,0.561472800404662,0.564091274875453,
0.580077896377513,0.585051565819623,0.629888712394502,0.648403829159917,
0.659576321811341,0.662920461139756,0.665014916094884,0.666948150920659,
0.669441169827075,0.673570863440185,0.700887508256962,0.743165790636969,
0.759418905946359,0.767854581617672,0.769931853395434,0.771145420820618,
0.772223167090481,0.773612710819158,0.775918979638267,0.789956654166822,
0.791301275937858,0.798311946222876,0.811988063787585,0.844849725796133,
0.861411599515774,0.871723051859038,0.874972088233509,0.877045672001599,
0.878986633389305,0.881528229847167,0.885824100341373,0.920957123164556,
0.969904495249132,0.979663687783069,0.981839348924972,0.98307474229114,
0.984148702056385,0.985526487748217,0.988384407862714,1.01124436943733,
1.02401053854181,1.05686693545025,1.0734200073315,1.08372777741852,1.08697661061679,
1.08905029475539,1.09099151170807,1.09353367602977,1.09783102914395,1.13304642848679,
1.1822527497537,1.19171696001675,1.19387222900763,1.19510321528332,1.19617797727302,
1.19756288077777,1.19980305841912,1.2125046529123,1.23488278711341,1.26848763937002,
1.29386537302104,1.29813616405493,1.30043374327061,1.30232685311879,1.30456764276984,
1.30846688370272,1.32437589687919,1.33459835185838,1.37388350711125,1.40246828626482,
1.40538090048541,1.40676947902978,1.40784464482559,1.4087765566926),
 .UNSPECIFIED.);
#2040=B_SPLINE_CURVE_WITH_KNOTS('',3,(#201696,#201697,#201698,#201699,#201700,
#201701,#201702,#201703,#201704,#201705,#201706,#201707,#201708,#201709,
#201710,#201711,#201712,#201713,#201714,#201715),.UNSPECIFIED.,.F.,.F.,
(4,2,2,2,2,2,2,2,2,4),(2.59331776226468,2.59687882416504,2.60151583696546,
2.60324440012632,2.60426747560143,2.60536147889293,2.60688102367856,2.61051762964333,
2.62723443668624,2.66742808210211),.UNSPECIFIED.);
#2041=B_SPLINE_CURVE_WITH_KNOTS('',3,(#201716,#201717,#201718,#201719,#201720,
#201721,#201722,#201723,#201724,#201725,#201726,#201727,#201728,#201729,
#201730,#201731,#201732,#201733,#201734,#201735,#201736,#201737,#201738,
#201739,#201740,#201741,#201742,#201743,#201744,#201745,#201746,#201747,
#201748,#201749,#201750,#201751,#201752,#201753,#201754,#201755,#201756,
#201757,#201758,#201759,#201760,#201761,#201762,#201763,#201764,#201765,
#201766,#201767,#201768,#201769,#201770,#201771,#201772,#201773,#201774,
#201775,#201776,#201777,#201778,#201779,#201780,#201781,#201782,#201783,
#201784,#201785,#201786,#201787,#201788,#201789,#201790,#201791,#201792,
#201793,#201794,#201795,#201796,#201797,#201798,#201799,#201800,#201801,
#201802,#201803,#201804,#201805,#201806,#201807,#201808,#201809,#201810,
#201811,#201812,#201813,#201814,#201815,#201816,#201817,#201818,#201819,
#201820,#201821,#201822,#201823,#201824,#201825,#201826,#201827,#201828,
#201829,#201830,#201831,#201832,#201833,#201834,#201835,#201836,#201837,
#201838,#201839,#201840,#201841,#201842,#201843,#201844,#201845,#201846,
#201847,#201848,#201849,#201850,#201851,#201852,#201853,#201854,#201855,
#201856,#201857,#201858,#201859,#201860,#201861,#201862,#201863,#201864,
#201865,#201866,#201867,#201868,#201869,#201870,#201871,#201872,#201873,
#201874,#201875,#201876,#201877,#201878,#201879,#201880,#201881,#201882,
#201883,#201884,#201885,#201886,#201887,#201888,#201889,#201890,#201891,
#201892,#201893,#201894,#201895,#201896,#201897,#201898,#201899,#201900,
#201901,#201902,#201903,#201904,#201905,#201906,#201907,#201908,#201909,
#201910,#201911,#201912,#201913,#201914,#201915,#201916,#201917,#201918,
#201919,#201920,#201921,#201922,#201923,#201924,#201925,#201926,#201927,
#201928,#201929,#201930,#201931,#201932,#201933,#201934,#201935,#201936,
#201937,#201938,#201939,#201940,#201941,#201942,#201943),.UNSPECIFIED.,
 .F.,.F.,(4,2,2,2,2,2,2,2,2,2,2,2,2,2,2,2,2,2,2,2,2,2,2,2,2,2,2,2,2,2,2,
2,2,2,2,2,2,2,2,2,2,2,2,2,2,2,2,2,2,2,2,2,2,2,2,2,2,2,2,2,2,2,2,2,2,2,2,
2,2,2,2,2,2,2,2,2,2,2,2,2,2,2,2,2,2,2,2,2,2,2,2,2,2,2,2,2,2,2,2,2,2,2,2,
2,2,2,2,2,2,2,2,2,2,4),(0.000704176387045162,0.0257174322174643,0.0359847029828326,
0.0390634760632502,0.0411897927333798,0.0432709570732162,0.0452083127274846,
0.0477298836914721,0.0519579433509182,0.0833451108736209,0.108642544508692,
0.136441798274749,0.145889395539929,0.148042836964259,0.149273089934266,
0.150347412956808,0.151732015589897,0.153972226003156,0.166687678355829,
0.188909395211854,0.215758615574672,0.237101823061518,0.24525349541233,
0.251225010735527,0.253845482176166,0.255800832283127,0.257600841493377,
0.260506681045256,0.267638306195958,0.316560289453651,0.355576580857015,
0.359166447748164,0.360677966617491,0.361770469902082,0.362795547041832,
0.364534723615624,0.369242329256875,0.409907236760057,0.456724709819592,
0.463117778256212,0.465819532313761,0.46777990438124,0.469573869737443,
0.472446538760659,0.47937836588777,0.531836911889365,0.558204274393352,
0.569627264630605,0.571906337375766,0.573164158634075,0.574235342718159,
0.575581152168262,0.578193953237735,0.594051450236483,0.598845344651008,
0.614069728480908,0.646945161062718,0.663526294999738,0.673846133326886,
0.677095894888077,0.679169481159531,0.681110121641195,0.683650831617003,
0.687944158977412,0.7303396011891,0.759387452405715,0.774118491642773,0.782013616435622,
0.784045763351531,0.785249245910931,0.786329312856606,0.78773662210919,
0.790103743863349,0.805534003367715,0.812264938970139,0.826056928548069,
0.858917448528633,0.875479587581388,0.885790959134291,0.889039839149378,
0.891113291674948,0.893054108121677,0.895595482909654,0.899890907285595,
0.935010850491094,0.983922413167823,0.993719231293955,0.995897355068234,
0.997133235743125,0.99820703638444,0.999583856581085,1.00243715643119,1.0251180204931,
1.03806278363758,1.07091848092184,1.08747235741845,1.09778029013521,1.10102899440095,
1.1031025529331,1.10504362187498,1.10758554845504,1.11188240124442,1.14708029997422,
1.19623277295707,1.20575435496611,1.2079135712673,1.20914537292454,1.21021991596308,
1.21160331437633,1.21383866255834,1.22645024787071,1.23297812007256,1.23811063457995,
1.25996976443291),.UNSPECIFIED.);
#2042=B_SPLINE_CURVE_WITH_KNOTS('',3,(#201945,#201946,#201947,#201948,#201949,
#201950,#201951,#201952,#201953,#201954,#201955,#201956,#201957,#201958,
#201959,#201960,#201961,#201962,#201963,#201964,#201965,#201966,#201967,
#201968,#201969,#201970,#201971,#201972,#201973,#201974,#201975,#201976,
#201977,#201978,#201979,#201980,#201981,#201982,#201983,#201984,#201985,
#201986,#201987,#201988,#201989,#201990,#201991,#201992,#201993,#201994,
#201995,#201996,#201997,#201998,#201999,#202000,#202001,#202002,#202003,
#202004,#202005,#202006,#202007,#202008,#202009,#202010,#202011,#202012,
#202013,#202014,#202015,#202016,#202017,#202018,#202019,#202020,#202021,
#202022,#202023,#202024,#202025,#202026,#202027,#202028,#202029,#202030,
#202031,#202032,#202033,#202034,#202035,#202036,#202037,#202038,#202039,
#202040,#202041,#202042,#202043,#202044,#202045,#202046,#202047,#202048,
#202049,#202050,#202051,#202052,#202053,#202054,#202055,#202056,#202057,
#202058,#202059,#202060,#202061,#202062,#202063,#202064,#202065,#202066,
#202067,#202068,#202069,#202070,#202071,#202072,#202073,#202074,#202075,
#202076,#202077,#202078,#202079,#202080,#202081,#202082,#202083,#202084,
#202085,#202086,#202087,#202088,#202089,#202090,#202091,#202092,#202093,
#202094,#202095,#202096,#202097,#202098,#202099,#202100,#202101,#202102,
#202103,#202104,#202105,#202106,#202107,#202108,#202109,#202110,#202111,
#202112,#202113,#202114,#202115,#202116,#202117,#202118,#202119,#202120,
#202121,#202122,#202123,#202124,#202125,#202126,#202127,#202128,#202129,
#202130,#202131,#202132,#202133,#202134,#202135,#202136,#202137,#202138,
#202139,#202140,#202141,#202142,#202143,#202144,#202145,#202146,#202147,
#202148,#202149,#202150,#202151,#202152,#202153,#202154,#202155,#202156,
#202157,#202158,#202159,#202160,#202161,#202162,#202163,#202164,#202165,
#202166,#202167,#202168,#202169,#202170,#202171,#202172,#202173,#202174,
#202175,#202176,#202177,#202178,#202179,#202180,#202181,#202182,#202183,
#202184,#202185,#202186,#202187,#202188,#202189,#202190,#202191,#202192,
#202193,#202194,#202195,#202196),.UNSPECIFIED.,.F.,.F.,(4,2,2,2,2,2,2,2,
2,2,2,2,2,2,2,2,2,2,2,2,2,2,2,2,2,2,2,2,2,2,2,2,2,2,2,2,2,2,2,2,2,2,2,2,
2,2,2,2,2,2,2,2,2,2,2,2,2,2,2,2,2,2,2,2,2,2,2,2,2,2,2,2,2,2,2,2,2,2,2,2,
2,2,2,2,2,2,2,2,2,2,2,2,2,2,2,2,2,2,2,2,2,2,2,2,2,2,2,2,2,2,2,2,2,2,2,2,
2,2,2,2,2,2,2,2,2,4),(1.4087765566926,1.40907336275232,1.4112182322391,
1.42053668861001,1.46971412927234,1.50508398887219,1.50938325226647,1.51192606388548,
1.51386748627527,1.51594110902301,1.51918925871308,1.5294898306286,1.54602886699855,
1.57357620420324,1.58971959996764,1.600802714468,1.6150361174334,1.61735264301978,
1.61874531396276,1.61982360776035,1.62103570079976,1.62310576441306,1.6314496999546,
1.64743527989167,1.68975214452658,1.71736328225565,1.72150090272662,1.72399648681361,
1.72593038437794,1.72802423287369,1.73136453467282,1.74249734349255,1.7609215473519,
1.80769170426024,1.81239636126156,1.82702418612506,1.82935850623005,1.83075641110029,
1.83183541342338,1.83304457384182,1.83510136760709,1.84328361300178,1.85880947313267,
1.90026437117459,1.90568732077929,1.91248088503755,1.93024129957683,1.93391848720998,
1.9363016658098,1.93821746452181,1.94039729841907,1.94412577070548,1.9595735030194,
2.01117048502747,2.03856342563001,2.04146895397035,2.04285615362426,2.04393117427766,
2.04516075937704,2.04730956747509,2.0566828324811,2.10594454896407,2.14117115456242,
2.14546864018391,2.14801093363032,2.14995226745882,2.15202609326085,2.15527518228868,
2.16558396509852,2.18214115986211,2.21503010009364,2.25067402459901,2.25353929057919,
2.25491859956229,2.25599279730645,2.25722740238569,2.25939912693306,2.26909913043769,
2.31807663577105,2.35321663378768,2.35751286566527,2.36005474967951,2.36199596220488,
2.36406984394431,2.36731940794986,2.37763296236546,2.39420092671154,2.42791430094642,
2.46269184112862,2.4655709325517,2.46695291782961,2.46799572897164,2.46800048615618,
2.46800515994633,2.46800975198409,2.46801426420427,2.46801869840922,2.46802305638761,
2.46802733966539,2.46803154982998,2.46803568862605,2.46803975739891,2.46804375757856,
2.46804769072524,2.46805155828045,2.46805515525448,2.46805873875214,2.46806230882394,
2.46806586566859,2.46806940949222,2.46929342575355,2.47060523319878,2.47263011108784,
2.47644761109667,2.48573747155612,2.52373742824155,2.53838555562746,2.56552945305741,
2.56965537121082,2.57214764549138,2.57408120384947,2.57617690892246,2.57952499461605,
2.59072883132307,2.60931753906047,2.6683654535451),.UNSPECIFIED.);
#2043=B_SPLINE_CURVE_WITH_KNOTS('',3,(#202197,#202198,#202199,#202200,#202201,
#202202,#202203,#202204,#202205,#202206,#202207,#202208,#202209,#202210,
#202211,#202212,#202213,#202214,#202215,#202216,#202217,#202218),
 .UNSPECIFIED.,.F.,.F.,(4,2,2,2,2,2,2,2,2,2,4),(0.000810723293800813,0.00554261288036417,
0.00881069567732799,0.0102445757462057,0.0113189845998339,0.0123418012301504,
0.0133650032428226,0.0148060197505862,0.0186526214094667,0.0263910128961989,
0.0750776857911647),.UNSPECIFIED.);
#2044=B_SPLINE_CURVE_WITH_KNOTS('',3,(#202223,#202224,#202225,#202226,#202227,
#202228,#202229,#202230,#202231,#202232,#202233,#202234,#202235,#202236,
#202237,#202238,#202239,#202240,#202241,#202242,#202243,#202244,#202245,
#202246,#202247,#202248,#202249,#202250,#202251,#202252,#202253,#202254,
#202255,#202256,#202257,#202258,#202259,#202260,#202261,#202262,#202263,
#202264,#202265,#202266,#202267,#202268,#202269,#202270,#202271,#202272,
#202273,#202274,#202275,#202276,#202277,#202278,#202279,#202280,#202281,
#202282,#202283,#202284,#202285,#202286,#202287,#202288,#202289,#202290,
#202291,#202292,#202293,#202294,#202295,#202296,#202297,#202298,#202299,
#202300,#202301,#202302,#202303,#202304,#202305,#202306,#202307,#202308,
#202309,#202310,#202311,#202312,#202313,#202314,#202315,#202316,#202317,
#202318,#202319,#202320,#202321,#202322,#202323,#202324,#202325,#202326,
#202327,#202328,#202329,#202330,#202331,#202332,#202333,#202334,#202335,
#202336,#202337,#202338,#202339,#202340,#202341,#202342,#202343,#202344,
#202345,#202346,#202347,#202348,#202349,#202350,#202351,#202352,#202353,
#202354,#202355,#202356,#202357,#202358,#202359,#202360,#202361,#202362,
#202363,#202364,#202365,#202366,#202367,#202368,#202369,#202370,#202371,
#202372,#202373,#202374,#202375,#202376,#202377,#202378,#202379,#202380,
#202381,#202382,#202383,#202384,#202385,#202386,#202387,#202388,#202389,
#202390,#202391,#202392,#202393,#202394,#202395,#202396,#202397,#202398,
#202399,#202400,#202401,#202402,#202403,#202404,#202405,#202406,#202407,
#202408,#202409,#202410,#202411,#202412,#202413,#202414,#202415,#202416,
#202417,#202418,#202419,#202420,#202421,#202422,#202423,#202424,#202425,
#202426,#202427,#202428,#202429,#202430,#202431,#202432,#202433,#202434,
#202435,#202436,#202437,#202438,#202439,#202440,#202441,#202442,#202443,
#202444,#202445,#202446,#202447,#202448,#202449,#202450,#202451,#202452,
#202453,#202454),.UNSPECIFIED.,.F.,.F.,(4,2,2,2,2,2,2,2,2,2,2,2,2,2,2,2,
2,2,2,2,2,2,2,2,2,2,2,2,2,2,2,2,2,2,2,2,2,2,2,2,2,2,2,2,2,2,2,2,2,2,2,2,
2,2,2,2,2,2,2,2,2,2,2,2,2,2,2,2,2,2,2,2,2,2,2,2,2,2,2,2,2,2,2,2,2,2,2,2,
2,2,2,2,2,2,2,2,2,2,2,2,2,2,2,2,2,2,2,2,2,2,2,2,2,2,2,4),(1.25972979047866,
1.26441544661838,1.3053610613189,1.32784160728741,1.33050512980155,1.33184401796151,
1.33281203044151,1.33403568918917,1.33615828902696,1.34517733233056,1.36316313661643,
1.4133807127183,1.43118515687013,1.43486474854704,1.43724846399644,1.43916402554714,
1.44134286563753,1.44506784009828,1.46047491616359,1.51181204801717,1.53949164612553,
1.5423987079172,1.54378607016068,1.54486095401903,1.54609008841637,1.54823741794453,
1.55759346836069,1.60686081724013,1.64208553053703,1.64638235700535,1.6489242455072,
1.65086526147395,1.65293873934485,1.65618726577919,1.66649411625969,1.6830480673437,
1.71593115656945,1.7293786806246,1.73696339845124,1.75196165556578,1.75431125715591,
1.75571350569481,1.75679293741798,1.75799933084553,1.7600442820177,1.76808819268639,
1.78322781985062,1.82293120494068,1.85417110674922,1.85839662823766,1.86091774065261,
1.86285534853089,1.86493737621978,1.86822502090342,1.8788782170039,1.89620582015083,
1.94441101571001,1.94870738494384,1.95125573763788,1.96413443037342,1.96638353439067,
1.96777099166722,1.96884584752657,1.97007483613716,1.97222164393327,1.98157126688385,
2.03084192735482,2.0660667153899,2.07036338620625,2.07290517686419,2.07484611479717,
2.07691950609162,2.08016789016946,2.09047423240022,2.10702731337179,2.13990890153686,
2.1533392808224,2.16096715021381,2.17594022523108,2.17828871779687,2.17969061312604,
2.18076996043251,2.18197646777555,2.184022068518,2.19207431895256,2.20723746151434,
2.24809402712651,2.27819036368754,2.2823904040134,2.28490402384112,2.28684038669099,
2.28892552206687,2.29222753760886,2.30301126794517,2.32063481327829,2.36540042647044,
2.37279931702476,2.3780325514617,2.38836987511231,2.39047057420638,2.39181291642993,
2.39288397540113,2.39414472195357,2.39643695913237,2.40809259323571,2.45644047193006,
2.49005757649922,2.49432866384189,2.49686296032778,2.49880259141716,2.50087888167573,
2.50396415646811,2.51344816507387,2.52832065029717,2.55076555222504,2.59331776226468),
 .UNSPECIFIED.);
#2045=B_SPLINE_CURVE_WITH_KNOTS('',3,(#202455,#202456,#202457,#202458,#202459,
#202460,#202461,#202462,#202463,#202464,#202465,#202466,#202467,#202468,
#202469,#202470,#202471,#202472,#202473,#202474,#202475,#202476,#202477,
#202478,#202479,#202480,#202481,#202482,#202483,#202484,#202485,#202486,
#202487,#202488,#202489,#202490,#202491,#202492,#202493,#202494,#202495,
#202496,#202497,#202498,#202499,#202500,#202501,#202502,#202503,#202504,
#202505,#202506,#202507,#202508,#202509,#202510,#202511,#202512,#202513,
#202514,#202515,#202516,#202517,#202518,#202519,#202520,#202521,#202522,
#202523,#202524,#202525,#202526,#202527,#202528,#202529,#202530,#202531,
#202532,#202533,#202534,#202535,#202536,#202537,#202538,#202539,#202540,
#202541,#202542,#202543,#202544,#202545,#202546,#202547,#202548,#202549,
#202550,#202551,#202552,#202553,#202554,#202555,#202556,#202557,#202558,
#202559,#202560,#202561,#202562,#202563,#202564,#202565,#202566,#202567,
#202568,#202569,#202570,#202571,#202572,#202573,#202574,#202575,#202576,
#202577,#202578,#202579,#202580,#202581,#202582,#202583,#202584,#202585,
#202586,#202587,#202588,#202589,#202590,#202591,#202592,#202593,#202594,
#202595,#202596,#202597,#202598,#202599,#202600,#202601,#202602,#202603,
#202604,#202605,#202606,#202607,#202608,#202609,#202610,#202611,#202612,
#202613,#202614,#202615,#202616,#202617,#202618,#202619,#202620,#202621,
#202622,#202623,#202624,#202625,#202626,#202627,#202628,#202629,#202630,
#202631,#202632,#202633,#202634,#202635,#202636,#202637,#202638,#202639,
#202640,#202641,#202642,#202643,#202644,#202645,#202646,#202647,#202648,
#202649,#202650,#202651,#202652,#202653,#202654,#202655,#202656,#202657,
#202658,#202659,#202660,#202661,#202662,#202663,#202664,#202665,#202666,
#202667,#202668,#202669,#202670,#202671,#202672,#202673,#202674,#202675,
#202676,#202677,#202678,#202679,#202680,#202681,#202682,#202683,#202684,
#202685,#202686,#202687,#202688,#202689,#202690,#202691,#202692),
 .UNSPECIFIED.,.F.,.F.,(4,2,2,2,2,2,2,2,2,2,2,2,2,2,2,2,2,2,2,2,2,2,2,2,
2,2,2,2,2,2,2,2,2,2,2,2,2,2,2,2,2,2,2,2,2,2,2,2,2,2,2,2,2,2,2,2,2,2,2,2,
2,2,2,2,2,2,2,2,2,2,2,2,2,2,2,2,2,2,2,2,2,2,2,2,2,2,2,2,2,2,2,2,2,2,2,2,
2,2,2,2,2,2,2,2,2,2,2,2,2,2,2,2,2,2,2,2,2,2,4),(0.0750776857911647,0.0854662128806517,
0.102113513010209,0.112462472456125,0.115715011359714,0.117788838543863,
0.119728630399909,0.122266681563765,0.126552051773031,0.169578646218511,
0.206314577630255,0.21544505052592,0.219215482639955,0.221222238265942,
0.222526258215038,0.223741864100537,0.224784482334952,0.226132418959838,
0.228755851296678,0.244846643278332,0.279928082166132,0.308528693246175,
0.323516269928108,0.32720807634895,0.329379151199865,0.331294981377584,
0.333688364679299,0.337400697434074,0.355733226600146,0.400166554420321,
0.422006851272112,0.432208086194616,0.434412653047945,0.435654098356039,
0.436726766395204,0.438094390116348,0.440902368864504,0.461852212431691,
0.508438144622218,0.532022390876901,0.537812874490773,0.540408818687665,
0.542350850112764,0.544170007538085,0.546684082903521,0.553153512053729,
0.610547729454446,0.63360267901706,0.644148564382533,0.646375206844844,
0.64762153109111,0.648693701157503,0.65005461102966,0.652216513321899,0.66352505516041,
0.667420965350106,0.675166234930583,0.688551738819603,0.721403415187081,
0.744143066111857,0.749821033615603,0.752396643121415,0.754335628674015,
0.756160833714146,0.75869747484129,0.765305818218002,0.821458408085833,
0.845317348858873,0.856084653013628,0.85832513359427,0.859574557371751,
0.860646518783183,0.862003470709962,0.86466817254514,0.881842551046938,
0.927336280123037,0.955192998759887,0.961524797529677,0.964216189288776,
0.966174748980582,0.967971007649691,0.970856013044009,0.977862144219322,
1.02919750989356,1.05636664255927,1.06798908640502,1.07027941596559,1.07153970300641,
1.07261072957908,1.07395347920677,1.0765519918091,1.09206281584894,1.09863713189724,
1.1400150245994,1.16727980036919,1.17353960115029,1.17621873185625,1.1781751753605,
1.17997423290247,1.18287419811612,1.18996967520648,1.23959823919283,1.27797520449599,
1.28156104996634,1.28307197542321,1.28416446040919,1.28518984720792,1.28693024629093,
1.29164521912667,1.3320546855614,1.33394409779729,1.3777690553888,1.38499098155144,
1.38791221156124,1.38971522305868,1.39166870674747,1.39433074808804,1.40049146476992,
1.40843319572732),.UNSPECIFIED.);
#2046=B_SPLINE_CURVE_WITH_KNOTS('',3,(#202698,#202699,#202700,#202701),
 .UNSPECIFIED.,.F.,.F.,(4,4),(152.105783788367,152.455231388399),
 .UNSPECIFIED.);
#2047=B_SPLINE_CURVE_WITH_KNOTS('',3,(#202702,#202703,#202704,#202705,#202706,
#202707,#202708,#202709,#202710,#202711,#202712,#202713,#202714,#202715,
#202716,#202717,#202718,#202719,#202720,#202721,#202722,#202723,#202724,
#202725,#202726,#202727,#202728,#202729,#202730,#202731,#202732,#202733,
#202734,#202735,#202736,#202737,#202738,#202739,#202740,#202741,#202742,
#202743,#202744,#202745,#202746,#202747,#202748,#202749,#202750,#202751,
#202752,#202753,#202754,#202755,#202756,#202757,#202758,#202759,#202760,
#202761,#202762,#202763,#202764,#202765,#202766,#202767,#202768,#202769,
#202770,#202771,#202772,#202773,#202774,#202775,#202776,#202777,#202778,
#202779,#202780,#202781,#202782,#202783,#202784,#202785,#202786,#202787,
#202788,#202789,#202790,#202791,#202792,#202793,#202794,#202795,#202796,
#202797,#202798,#202799,#202800,#202801,#202802,#202803,#202804,#202805,
#202806,#202807,#202808,#202809,#202810,#202811,#202812,#202813,#202814,
#202815,#202816,#202817,#202818,#202819,#202820,#202821,#202822,#202823,
#202824,#202825,#202826,#202827,#202828,#202829,#202830,#202831,#202832,
#202833,#202834,#202835,#202836,#202837,#202838,#202839,#202840,#202841,
#202842,#202843,#202844,#202845,#202846,#202847,#202848,#202849,#202850,
#202851,#202852,#202853,#202854,#202855,#202856,#202857,#202858,#202859,
#202860,#202861,#202862,#202863,#202864,#202865,#202866,#202867,#202868,
#202869,#202870,#202871,#202872,#202873,#202874,#202875,#202876,#202877,
#202878,#202879,#202880,#202881,#202882,#202883,#202884,#202885,#202886,
#202887,#202888,#202889,#202890,#202891,#202892,#202893,#202894,#202895,
#202896,#202897,#202898,#202899,#202900,#202901,#202902,#202903,#202904,
#202905,#202906,#202907,#202908,#202909,#202910,#202911),.UNSPECIFIED.,
 .F.,.F.,(4,2,2,2,2,2,2,2,2,2,2,2,2,2,2,2,2,2,2,2,2,2,2,2,2,2,2,2,2,2,2,
2,2,2,2,2,2,2,2,2,2,2,2,2,2,2,2,2,2,2,2,2,2,2,2,2,2,2,2,2,2,2,2,2,2,2,2,
2,2,2,2,2,2,2,2,2,2,2,2,2,2,2,2,2,2,2,2,2,2,2,2,2,2,2,2,2,2,2,2,2,2,2,2,
2,4),(0.000629313894772825,0.0163201057884129,0.0544201859933447,0.058003511077306,
0.0595138340669082,0.0606060551084784,0.0616313308680476,0.0633718331634841,
0.0680887831680241,0.112806259851638,0.13693201608523,0.151520373459769,
0.160861098942264,0.163933559753649,0.166006632046877,0.167947109366619,
0.170488064305094,0.174782833329962,0.209904581901936,0.258831998605639,
0.268597987373947,0.27077373873528,0.272008963729442,0.273082636513288,
0.274459870255308,0.277316013071211,0.300127821126255,0.345794510276056,
0.362353003017357,0.372662406694839,0.37591082752992,0.377984025652916,
0.379924631118862,0.382465768811906,0.386760880245431,0.421889856834204,
0.470835662474782,0.480584246911095,0.482758903857259,0.483993937037209,
0.485067718214192,0.486445450690249,0.489303866086973,0.525387805716559,
0.558081158061455,0.580569801177691,0.586214163995462,0.588783792192102,
0.590722045777741,0.592549333440548,0.595093317229995,0.601747175732378,
0.657468429688583,0.681617892032286,0.692464258824482,0.694709737579719,
0.695960345083562,0.697032333501087,0.698388051759229,0.700532391059881,
0.71154838607147,0.762828588164124,0.791475767664967,0.797902873859704,
0.800610610486495,0.802572270015877,0.80436531139643,0.807231921514496,
0.814125449677963,0.867130606206088,0.893123385419549,0.904452259754445,
0.906726188400712,0.907982999434976,0.909054432270387,0.910401965547792,
0.913022257816694,0.929039407105128,0.929690928185521,0.974004119802603,
1.00337474986631,1.00988765092338,1.01260988419403,1.01457426067376,1.0163644561045,
1.01921498407812,1.0260105189294,1.08022203964785,1.10538729233139,1.11650314549799,
1.11876478978648,1.12001896803965,1.12109069161044,1.12244182620981,1.12507868313549,
1.14151014293562,1.19210040090442,1.20981256340647,1.22063658528523,1.2239432024748,
1.22602946922786,1.22796566111022,1.23047733012731,1.23467034641304,1.25972979047866),
 .UNSPECIFIED.);
#2048=B_SPLINE_CURVE_WITH_KNOTS('',3,(#202913,#202914,#202915,#202916,#202917,
#202918,#202919,#202920,#202921,#202922,#202923,#202924,#202925,#202926,
#202927,#202928,#202929,#202930,#202931,#202932,#202933,#202934,#202935,
#202936,#202937,#202938,#202939,#202940,#202941,#202942,#202943,#202944,
#202945,#202946,#202947,#202948,#202949,#202950,#202951,#202952,#202953,
#202954,#202955,#202956,#202957,#202958,#202959,#202960,#202961,#202962,
#202963,#202964,#202965,#202966,#202967,#202968,#202969,#202970,#202971,
#202972,#202973,#202974,#202975,#202976,#202977,#202978,#202979,#202980,
#202981,#202982,#202983,#202984,#202985,#202986,#202987,#202988,#202989,
#202990,#202991,#202992,#202993,#202994,#202995,#202996,#202997,#202998,
#202999,#203000,#203001,#203002,#203003,#203004,#203005,#203006,#203007,
#203008,#203009,#203010,#203011,#203012,#203013,#203014,#203015,#203016,
#203017,#203018,#203019,#203020,#203021,#203022,#203023,#203024,#203025,
#203026,#203027,#203028,#203029,#203030,#203031,#203032,#203033,#203034,
#203035,#203036,#203037,#203038,#203039,#203040,#203041,#203042,#203043,
#203044,#203045,#203046,#203047,#203048,#203049,#203050,#203051,#203052,
#203053,#203054,#203055,#203056,#203057,#203058,#203059,#203060,#203061,
#203062,#203063,#203064,#203065,#203066,#203067,#203068,#203069,#203070,
#203071,#203072,#203073,#203074,#203075,#203076,#203077,#203078,#203079,
#203080,#203081,#203082,#203083,#203084,#203085,#203086,#203087,#203088,
#203089,#203090,#203091,#203092,#203093,#203094,#203095,#203096,#203097,
#203098,#203099,#203100,#203101,#203102,#203103,#203104,#203105,#203106,
#203107,#203108,#203109,#203110,#203111,#203112,#203113,#203114,#203115,
#203116,#203117,#203118,#203119,#203120,#203121,#203122,#203123,#203124,
#203125,#203126,#203127,#203128),.UNSPECIFIED.,.F.,.F.,(4,2,2,2,2,2,2,2,
2,2,2,2,2,2,2,2,2,2,2,2,2,2,2,2,2,2,2,2,2,2,2,2,2,2,2,2,2,2,2,2,2,2,2,2,
2,2,2,2,2,2,2,2,2,2,2,2,2,2,2,2,2,2,2,2,2,2,2,2,2,2,2,2,2,2,2,2,2,2,2,2,
2,2,2,2,2,2,2,2,2,2,2,2,2,2,2,2,2,2,2,2,2,2,2,2,2,2,2,4),(1.40843319572732,
1.42695731648832,1.46587333981965,1.47401635250847,1.49128931104146,1.49395781187334,
1.49531562368928,1.49638770882099,1.49763664550364,1.49987467007586,1.51060061965061,
1.53430394351945,1.56167608299342,1.59360626912867,1.59784576883013,1.60037091261219,
1.60230911167032,1.6043893183177,1.60766889029093,1.61825047610564,1.63541707716733,
1.68115614033856,1.68792200324815,1.70336678250791,1.70573464644326,1.70714221331575,
1.70822236916999,1.70942584279954,1.71145772380151,1.71934890486926,1.73406667207418,
1.76310493703932,1.80549050289223,1.8097835210629,1.81232423638252,1.8142649785188,
1.81633876714915,1.81958904046634,1.8299120618514,1.84650210602008,1.87941417023541,
1.89545412468211,1.89925794956622,1.91528181190017,1.91790235229976,1.91924988487568,
1.92032124917145,1.92157790678213,1.9238513616789,1.93517440363395,1.96114299568423,
2.01413424879559,2.02102544135396,2.02389154930304,2.02568441579992,2.0276460017689,
2.03035384504351,2.03678217404211,2.06544509919645,2.11674021308599,2.12775980409431,
2.12990435161104,2.13126010903991,2.13233207143994,2.13358258959672,2.13582774902764,
2.14666999949005,2.17080195418908,2.22650529605477,2.23315721559891,2.23570085203259,
2.23752802028449,2.23946626654463,2.24203608049835,2.24768163593029,2.27018211658393,
2.30291064292561,2.33898617511563,2.34184595819503,2.34322396051763,2.34429776587213,
2.34553262532202,2.34770648123255,2.35744366393611,2.40637342642948,2.44148699526411,
2.4461649031357,2.44859886023886,2.45046883506032,2.45255445190642,2.45473702611308,
2.45795216888837,2.49308193384322,2.54887914088592,2.55315894461639,2.55483153729244,
2.55584379223923,2.55694602488149,2.5585102056888,2.56241787407287,2.58158152562364,
2.64854564337416,2.65670852799325,2.65977977395676,2.66161107895188,2.66345503868571,
2.66574688078778,2.6678112172335),.UNSPECIFIED.);
#2049=B_SPLINE_CURVE_WITH_KNOTS('',3,(#203129,#203130,#203131,#203132,#203133,
#203134,#203135,#203136,#203137,#203138),.UNSPECIFIED.,.F.,.F.,(4,2,2,2,
4),(0.000823824276227816,0.00402823554000867,0.0105267000676126,0.0601103595096327,
0.0751122659302341),.UNSPECIFIED.);
#2050=B_SPLINE_CURVE_WITH_KNOTS('',3,(#203144,#203145,#203146,#203147,#203148,
#203149),.UNSPECIFIED.,.F.,.F.,(4,2,4),(2.59315592359719,2.60891630066588,
2.66742167112986),.UNSPECIFIED.);
#2051=B_SPLINE_CURVE_WITH_KNOTS('',3,(#203150,#203151,#203152,#203153,#203154,
#203155,#203156,#203157,#203158,#203159),.UNSPECIFIED.,.F.,.F.,(4,1,1,1,
1,1,1,4),(152.455231388399,152.821976844167,153.820813294129,154.81964974409,
155.818486194052,156.817322644014,157.816159093976,158.388969095546),
 .UNSPECIFIED.);
#2052=B_SPLINE_CURVE_WITH_KNOTS('',3,(#203160,#203161,#203162,#203163,#203164,
#203165,#203166,#203167,#203168,#203169,#203170,#203171,#203172,#203173,
#203174,#203175,#203176,#203177,#203178,#203179,#203180,#203181,#203182,
#203183,#203184,#203185,#203186,#203187,#203188,#203189,#203190,#203191,
#203192,#203193,#203194,#203195,#203196,#203197,#203198,#203199,#203200,
#203201,#203202,#203203,#203204,#203205,#203206,#203207,#203208,#203209,
#203210,#203211,#203212,#203213,#203214,#203215,#203216,#203217,#203218,
#203219,#203220,#203221,#203222,#203223,#203224,#203225,#203226,#203227,
#203228,#203229,#203230,#203231,#203232,#203233,#203234,#203235,#203236,
#203237,#203238,#203239,#203240,#203241,#203242,#203243,#203244,#203245,
#203246,#203247,#203248,#203249,#203250,#203251,#203252,#203253,#203254,
#203255,#203256,#203257,#203258,#203259,#203260,#203261,#203262,#203263,
#203264,#203265,#203266,#203267,#203268,#203269,#203270,#203271,#203272,
#203273,#203274,#203275,#203276,#203277,#203278,#203279,#203280,#203281,
#203282,#203283,#203284,#203285,#203286,#203287,#203288,#203289,#203290,
#203291,#203292,#203293,#203294,#203295,#203296,#203297,#203298,#203299,
#203300,#203301,#203302,#203303,#203304,#203305,#203306,#203307,#203308,
#203309,#203310,#203311,#203312,#203313,#203314,#203315,#203316,#203317,
#203318,#203319,#203320,#203321,#203322,#203323,#203324,#203325,#203326,
#203327,#203328,#203329,#203330,#203331,#203332,#203333,#203334,#203335,
#203336,#203337,#203338,#203339,#203340,#203341,#203342,#203343,#203344,
#203345,#203346,#203347,#203348,#203349,#203350,#203351,#203352,#203353,
#203354,#203355,#203356,#203357,#203358,#203359,#203360,#203361,#203362,
#203363,#203364,#203365,#203366,#203367,#203368,#203369,#203370,#203371,
#203372,#203373,#203374,#203375,#203376,#203377,#203378,#203379,#203380,
#203381,#203382,#203383,#203384,#203385,#203386,#203387,#203388,#203389,
#203390,#203391,#203392,#203393,#203394,#203395,#203396,#203397,#203398,
#203399,#203400,#203401,#203402,#203403,#203404,#203405,#203406,#203407,
#203408,#203409,#203410,#203411,#203412,#203413,#203414,#203415,#203416,
#203417,#203418,#203419,#203420,#203421,#203422,#203423,#203424,#203425,
#203426,#203427,#203428,#203429,#203430,#203431,#203432,#203433,#203434,
#203435),.UNSPECIFIED.,.F.,.F.,(4,2,2,2,2,2,2,2,2,2,2,2,2,2,2,2,2,2,2,2,
2,2,2,2,2,2,2,2,2,2,2,2,2,2,2,2,2,2,2,2,2,2,2,2,2,2,2,2,2,2,2,2,2,2,2,2,
2,2,2,2,2,2,2,2,2,2,2,2,2,2,2,2,2,2,2,2,2,2,2,2,2,2,2,2,2,2,2,2,2,2,2,2,
2,2,2,2,2,2,2,2,2,2,2,2,2,2,2,2,2,2,2,2,2,2,2,2,2,2,2,2,2,2,2,2,2,2,2,2,
2,2,2,2,2,2,2,2,2,4),(0.0751122659302341,0.085828878825592,0.0970868110481651,
0.0993563555451385,0.100612073461201,0.101683382847819,0.103031790709545,
0.10565681638989,0.121802814244195,0.172381098038625,0.190284662893531,
0.201191748518281,0.203647518624949,0.205928943311196,0.205943863292443,
0.205959399610425,0.205975593874828,0.205992491573063,0.206010142783773,
0.206028602703602,0.206047932242364,0.206068198973089,0.206089477926499,
0.206111852850056,0.206135417431713,0.206160276963575,0.206186550301097,
0.20621437210921,0.206243895752698,0.206275296862062,0.206308777602607,
0.206344572247025,0.20821731272881,0.210599717359116,0.215045795121062,
0.241166177948392,0.284929293597834,0.301025008859123,0.309405652452208,
0.311478260239731,0.31269067274794,0.313768460568666,0.315159440535809,
0.31747097912074,0.331619418740069,0.342238328607994,0.38562798519719,0.409018583727364,
0.414783744998917,0.417375305203036,0.419316841122738,0.421137558099361,
0.423656999570428,0.43015805816979,0.487280697079861,0.510517692195319,
0.521114646640081,0.523344682687182,0.524591849602223,0.525664087826453,
0.527024238510021,0.529703813501034,0.547289991057891,0.555090515258147,
0.565599528223832,0.598431611186449,0.614959756296749,0.625255709364678,
0.628502792552046,0.630575834651251,0.63251678438357,0.635059080611407,
0.63935773728141,0.674736803913771,0.723923619866213,0.733241115571108,
0.735385610659766,0.736614078190253,0.737689006812695,0.739077244557444,
0.741989039743823,0.773695991869402,0.777689021102544,0.810489725132012,
0.833142836239981,0.838809742899897,0.841383685350726,0.843322775963028,
0.845149077890299,0.847688842652357,0.854314735300919,0.910325837239713,
0.934291589604419,0.945088860945829,0.947331540212699,0.948581622742244,
0.949653799092122,0.951010573603945,0.953158118252572,0.964223221520589,
1.01536624081847,1.04409282272519,1.0505297317483,1.05323930695841,1.0552014672327,
1.05699439464595,1.0598595792886,1.06674323897249,1.11989293571659,1.14579229963293,
1.15709790249943,1.15937067895881,1.16062732651352,1.16169890755991,1.16304699331893,
1.16566943644532,1.18171826673186,1.18582956695817,1.20152232426753,1.23441215403954,
1.25720138141645,1.26288695609681,1.26546450453172,1.2674043374973,1.26922989156428,
1.27176629974413,1.27836983492409,1.33461082161945,1.35356472111645,1.36856797597223,
1.37091816755845,1.37232074623916,1.37340041866843,1.37460706603077,1.37665241518814,
1.38469748033816,1.39983872514726,1.40873148512311),.UNSPECIFIED.);
#2053=B_SPLINE_CURVE_WITH_KNOTS('',3,(#203440,#203441,#203442,#203443,#203444,
#203445,#203446,#203447,#203448,#203449,#203450,#203451,#203452,#203453,
#203454,#203455,#203456,#203457,#203458,#203459,#203460,#203461,#203462,
#203463,#203464,#203465,#203466,#203467,#203468,#203469,#203470,#203471,
#203472,#203473,#203474,#203475,#203476,#203477,#203478,#203479,#203480,
#203481,#203482,#203483,#203484,#203485,#203486,#203487,#203488,#203489,
#203490,#203491,#203492,#203493,#203494,#203495,#203496,#203497,#203498,
#203499,#203500,#203501,#203502,#203503,#203504,#203505,#203506,#203507,
#203508,#203509,#203510,#203511,#203512,#203513,#203514,#203515,#203516,
#203517,#203518,#203519,#203520,#203521,#203522,#203523,#203524,#203525,
#203526,#203527,#203528,#203529,#203530,#203531,#203532,#203533,#203534,
#203535,#203536,#203537,#203538,#203539,#203540,#203541,#203542,#203543,
#203544,#203545,#203546,#203547,#203548,#203549,#203550,#203551,#203552,
#203553,#203554,#203555,#203556,#203557,#203558,#203559,#203560,#203561,
#203562,#203563,#203564,#203565,#203566,#203567,#203568,#203569,#203570,
#203571,#203572,#203573,#203574,#203575,#203576,#203577,#203578,#203579,
#203580,#203581,#203582,#203583,#203584,#203585,#203586,#203587,#203588,
#203589,#203590,#203591,#203592,#203593,#203594,#203595,#203596,#203597,
#203598,#203599,#203600,#203601,#203602,#203603,#203604,#203605,#203606,
#203607,#203608,#203609,#203610,#203611,#203612,#203613,#203614,#203615,
#203616,#203617,#203618,#203619,#203620,#203621,#203622,#203623,#203624,
#203625,#203626,#203627,#203628,#203629,#203630,#203631,#203632,#203633,
#203634,#203635,#203636,#203637,#203638,#203639,#203640,#203641,#203642,
#203643,#203644,#203645,#203646,#203647,#203648,#203649,#203650,#203651,
#203652,#203653,#203654,#203655,#203656,#203657,#203658,#203659,#203660,
#203661,#203662,#203663,#203664,#203665,#203666,#203667,#203668,#203669,
#203670,#203671,#203672,#203673),.UNSPECIFIED.,.F.,.F.,(4,2,2,2,2,2,2,2,
2,2,2,2,2,2,2,2,2,2,2,2,2,2,2,2,2,2,2,2,2,2,2,2,2,2,2,2,2,2,2,2,2,2,2,2,
2,2,2,2,2,2,2,2,2,2,2,2,2,2,2,2,2,2,2,2,2,2,2,2,2,2,2,2,2,2,2,2,2,2,2,2,
2,2,2,2,2,2,2,2,2,2,2,2,2,2,2,2,2,2,2,2,2,2,2,2,2,2,2,2,2,2,2,2,2,2,2,2,
4),(1.25960927945369,1.26784056068535,1.29070305517887,1.30119586223981,
1.30341928562604,1.30466495514073,1.30573723667345,1.30709916579662,1.30978755174501,
1.32763514716263,1.33373204795653,1.37574263997476,1.40292854467451,1.40705404771045,
1.40954560847968,1.41147833629177,1.41357286270537,1.41691845713225,1.42810816167539,
1.44666703455994,1.49069774575448,1.49656843927689,1.51244824705574,1.51506158886226,
1.51640745051267,1.51747862366803,1.51873640767557,1.52101504423773,1.53242877663141,
1.5587556144553,1.61123418639183,1.61816335064033,1.62103577214087,1.62282983684166,
1.62479052775042,1.62749309914301,1.63388987746754,1.68178582156254,1.7213746982433,
1.72610769207243,1.72785089277105,1.72887687622625,1.72996904238941,1.73147806418142,
1.73505278632489,1.77424216861532,1.82298145965566,1.83011236861365,1.83301825935914,
1.83481840225398,1.8367739839029,1.83944824471868,1.84567976943025,1.87271784907334,
1.91343456524463,1.93614252156641,1.93899624933968,1.94037305645156,1.94144673945619,
1.94268236965753,1.94485976391051,1.95464886093963,2.00353430065314,2.03864073873109,
2.04293543194623,2.04547649278712,2.04741712656729,2.04949043819454,2.05273920904223,
2.06305108153262,2.07961711155464,2.11250738363383,2.1270680362877,2.13238492367237,
2.14842385062004,2.1510451305138,2.15239273736957,2.15346400855855,2.15472038501481,
2.15699285603943,2.16830127058305,2.19421412126112,2.24727753742218,2.25416201565285,
2.25702687422792,2.25881940752266,2.26078098958741,2.26348948923292,2.26992251464575,
2.29862707764436,2.3498476032982,2.3608812297336,2.36302652803489,2.36438245774963,
2.36545435010505,2.36670454699238,2.36894855284607,2.37977416098886,2.40384585326639,
2.45963485770822,2.46627520364442,2.46881688665781,2.47064342899255,2.4725194430492,
2.47500336289316,2.47774110006639,2.48229185387961,2.49161991296542,2.54225956213082,
2.57203621327389,2.57495058484101,2.57633919796764,2.57741402116202,2.57864193453782,
2.58078443077413,2.59007761168861,2.59315592359719),.UNSPECIFIED.);
#2054=B_SPLINE_CURVE_WITH_KNOTS('',3,(#203675,#203676,#203677,#203678,#203679,
#203680,#203681,#203682,#203683,#203684,#203685,#203686,#203687,#203688,
#203689,#203690,#203691,#203692,#203693,#203694,#203695,#203696,#203697,
#203698,#203699,#203700,#203701,#203702,#203703,#203704,#203705,#203706,
#203707,#203708,#203709,#203710,#203711,#203712,#203713,#203714,#203715,
#203716,#203717,#203718,#203719,#203720,#203721,#203722,#203723,#203724,
#203725,#203726,#203727,#203728,#203729,#203730,#203731,#203732,#203733,
#203734,#203735,#203736,#203737,#203738,#203739,#203740,#203741,#203742,
#203743,#203744,#203745,#203746,#203747,#203748,#203749,#203750,#203751,
#203752,#203753,#203754,#203755,#203756,#203757,#203758,#203759,#203760,
#203761,#203762,#203763,#203764,#203765,#203766,#203767,#203768,#203769,
#203770,#203771,#203772,#203773,#203774,#203775,#203776,#203777,#203778,
#203779,#203780,#203781,#203782,#203783,#203784,#203785,#203786,#203787,
#203788,#203789,#203790,#203791,#203792,#203793,#203794,#203795,#203796,
#203797,#203798,#203799,#203800,#203801,#203802,#203803,#203804,#203805,
#203806,#203807,#203808,#203809,#203810,#203811,#203812,#203813,#203814,
#203815,#203816,#203817,#203818,#203819,#203820,#203821,#203822,#203823,
#203824,#203825,#203826,#203827,#203828,#203829,#203830,#203831,#203832,
#203833,#203834,#203835,#203836,#203837,#203838,#203839,#203840,#203841,
#203842,#203843,#203844,#203845,#203846,#203847,#203848,#203849,#203850,
#203851,#203852,#203853,#203854,#203855,#203856,#203857,#203858,#203859,
#203860,#203861,#203862,#203863,#203864,#203865,#203866,#203867,#203868,
#203869,#203870,#203871,#203872,#203873,#203874,#203875,#203876,#203877,
#203878,#203879,#203880,#203881,#203882,#203883,#203884,#203885,#203886,
#203887,#203888,#203889,#203890,#203891,#203892,#203893,#203894,#203895,
#203896,#203897,#203898),.UNSPECIFIED.,.F.,.F.,(4,2,2,2,2,2,2,2,2,2,2,2,
2,2,2,2,2,2,2,2,2,2,2,2,2,2,2,2,2,2,2,2,2,2,2,2,2,2,2,2,2,2,2,2,2,2,2,2,
2,2,2,2,2,2,2,2,2,2,2,2,2,2,2,2,2,2,2,2,2,2,2,2,2,2,2,2,2,2,2,2,2,2,2,2,
2,2,2,2,2,2,2,2,2,2,2,2,2,2,2,2,2,2,2,2,2,2,2,2,2,2,2,4),(1.40873148512311,
1.43954141038742,1.47079962802823,1.47502632051913,1.47754805802225,1.47948610340675,
1.4815685590938,1.48485679029968,1.49551110179774,1.51283974492747,1.55312800056793,
1.58012246481206,1.58302494697855,1.58441154160231,1.58548648574311,1.58671642281291,
1.58886687965066,1.5982634941122,1.64750384981752,1.6827241502224,1.68702149907781,
1.68956373353539,1.69150503492834,1.69357883830035,1.69682791768685,1.70713688465068,
1.72369458008402,1.75658366016653,1.77013897321832,1.77745269684894,1.78179090962933,
1.79297526494844,1.79513021280011,1.7964892638977,1.79756164775093,1.79881015301174,
1.80104546560828,1.81172187639829,1.8352408649652,1.89190053299344,1.89845482549405,
1.90098324363558,1.90280660268653,1.90474739266829,1.90733183552432,1.9130557756659,
1.93613505434352,1.96966870742379,1.99211409908916,2.00484619071758,2.0070877605922,
2.00847297320677,2.00954762509103,2.01077810063698,2.0129315592425,2.02237367369485,
2.07156495933937,2.10676763193365,2.11106412780525,2.1136059029602,2.11554687968838,
2.11762036148754,2.12086898972392,2.13117696796551,2.14773349155529,2.18061848600975,
2.21625346366134,2.21911651538686,2.22049524404451,2.22156921712478,2.22280381975302,
2.22497615127895,2.23468888175323,2.28364516430624,2.31877576290163,2.32307119649038,
2.32561261931894,2.32755348597996,2.32962700433937,2.33287601171029,2.34318790662308,
2.35975331282198,2.3912034672034,2.42829559713972,2.43113341468106,2.43250716066688,
2.433580642496,2.43479364705273,2.43689635354939,2.43949336807867,2.44490278294649,
2.46031812615432,2.50136047554929,2.53093500282094,2.53512497338509,2.53763570477168,
2.53957168392176,2.54165822449844,2.54496634977607,2.55580486074104,2.57355287739486,
2.61947634618228,2.6278080198572,2.64081332124416,2.64306886678551,2.64445824632581,
2.64553327890896,2.64654209452073,2.64775526287028,2.64954167370693,2.65527690517876,
2.6679454068061),.UNSPECIFIED.);
#2055=B_SPLINE_CURVE_WITH_KNOTS('',3,(#203899,#203900,#203901,#203902,#203903,
#203904,#203905,#203906,#203907,#203908,#203909,#203910,#203911),
 .UNSPECIFIED.,.F.,.F.,(4,3,3,3,4),(-161.271232394665,-161.16946618359,
-161.067655474371,-160.965693995851,-160.920671713183),.UNSPECIFIED.);
#2056=B_SPLINE_CURVE_WITH_KNOTS('',3,(#203917,#203918,#203919,#203920,#203921,
#203922,#203923,#203924,#203925,#203926,#203927,#203928,#203929),
 .UNSPECIFIED.,.F.,.F.,(4,3,3,3,4),(170.955339710339,171.057208845626,171.158971098887,
171.260660137299,171.305836600057),.UNSPECIFIED.);
#2057=B_SPLINE_CURVE_WITH_KNOTS('',3,(#203930,#203931,#203932,#203933,#203934,
#203935,#203936,#203937,#203938,#203939,#203940,#203941,#203942,#203943,
#203944,#203945,#203946,#203947,#203948,#203949,#203950,#203951,#203952,
#203953,#203954,#203955,#203956,#203957,#203958,#203959,#203960,#203961,
#203962,#203963,#203964,#203965,#203966,#203967,#203968,#203969,#203970,
#203971,#203972,#203973,#203974,#203975,#203976,#203977,#203978,#203979,
#203980,#203981,#203982,#203983,#203984,#203985,#203986,#203987,#203988,
#203989,#203990,#203991,#203992,#203993,#203994,#203995,#203996,#203997,
#203998,#203999,#204000,#204001,#204002,#204003,#204004,#204005,#204006,
#204007,#204008,#204009,#204010,#204011,#204012,#204013,#204014,#204015,
#204016,#204017,#204018,#204019,#204020,#204021,#204022,#204023,#204024,
#204025,#204026,#204027,#204028,#204029,#204030,#204031,#204032,#204033,
#204034,#204035,#204036,#204037,#204038,#204039,#204040,#204041,#204042,
#204043,#204044,#204045,#204046,#204047,#204048,#204049,#204050,#204051,
#204052,#204053,#204054,#204055,#204056,#204057,#204058,#204059,#204060,
#204061,#204062,#204063,#204064,#204065,#204066,#204067,#204068,#204069,
#204070,#204071,#204072,#204073,#204074,#204075,#204076,#204077,#204078,
#204079,#204080,#204081,#204082,#204083,#204084,#204085,#204086,#204087,
#204088,#204089,#204090,#204091,#204092,#204093,#204094,#204095,#204096,
#204097,#204098,#204099,#204100,#204101,#204102,#204103,#204104,#204105,
#204106,#204107,#204108,#204109,#204110,#204111,#204112,#204113,#204114,
#204115,#204116,#204117,#204118,#204119,#204120,#204121,#204122,#204123,
#204124,#204125,#204126,#204127,#204128,#204129,#204130,#204131,#204132,
#204133,#204134,#204135,#204136,#204137,#204138,#204139,#204140,#204141,
#204142,#204143,#204144,#204145,#204146,#204147,#204148,#204149,#204150,
#204151),.UNSPECIFIED.,.F.,.F.,(4,2,2,2,2,2,2,2,2,2,2,2,2,2,2,2,2,2,2,2,
2,2,2,2,2,2,2,2,2,2,2,2,2,2,2,2,2,2,2,2,2,2,2,2,2,2,2,2,2,2,2,2,2,2,2,2,
2,2,2,2,2,2,2,2,2,2,2,2,2,2,2,2,2,2,2,2,2,2,2,2,2,2,2,2,2,2,2,2,2,2,2,2,
2,2,2,2,2,2,2,2,2,2,2,2,2,2,2,2,2,2,4),(0.000655555487746406,0.0215326867220369,
0.0285521057207997,0.0303960777145486,0.0316335698167745,0.0326484404410412,
0.0337175254276835,0.0350634362659286,0.0377855770018737,0.0559574692004484,
0.061638161908966,0.0739378941501972,0.0845184776971982,0.106384522445289,
0.122977092814764,0.133286052670248,0.136520215528419,0.138580655542259,
0.140506662082009,0.143024731538882,0.147271552045667,0.192337636321466,
0.220917652812677,0.234451027551801,0.241869026835945,0.243841420654799,
0.244851141182566,0.245918180059928,0.247244796379088,0.249294128909632,
0.258883142395294,0.318505419951983,0.335297078770584,0.345718786023299,
0.348984818510775,0.351065107730897,0.353009480963641,0.355551477179388,
0.359839182118602,0.39423280182301,0.443435079782813,0.453287138480796,
0.455474742211183,0.456715723135277,0.457791987620055,0.459170643306667,
0.462028507550171,0.48480471709289,0.527329230071651,0.545904435004286,
0.557102170076887,0.560449685950735,0.562545350531582,0.564479092283313,
0.566971916582978,0.571099442096233,0.598278238353839,0.640348116479544,
0.65690820639345,0.665449594930443,0.667534919720363,0.668750047887287,
0.669826498733916,0.671211235833482,0.673503643660504,0.687287896422153,
0.698621228031735,0.737949806914923,0.764492324349816,0.770660377970032,
0.773322016361416,0.775273840198162,0.777074356311094,0.779989358629309,
0.787184867462303,0.833862611011882,0.856213838851044,0.870037675624283,
0.875062793485331,0.878645311342973,0.880154605271385,0.881246040641265,
0.882271325117263,0.884011299816394,0.888723661899274,0.929075125968494,
0.977359006375441,0.982966744880172,0.985530002193917,0.98746767807645,
0.989297544767694,0.991850158636646,0.998557347295345,1.05366058603572,
1.0781766973765,1.08912118873027,1.09137328663972,1.09262570343644,1.09369780423249,
1.095051993725,1.09779133469493,1.11614973897311,1.16514968613826,1.18898302761693,
1.19480674987626,1.19740895638714,1.19935224745615,1.20117010545591,1.20367846665727,
1.2101117363724,1.25960927945369),.UNSPECIFIED.);
#2058=B_SPLINE_CURVE_WITH_KNOTS('',3,(#204153,#204154,#204155,#204156,#204157,
#204158,#204159,#204160,#204161,#204162,#204163,#204164,#204165,#204166,
#204167,#204168,#204169,#204170,#204171,#204172,#204173,#204174,#204175,
#204176,#204177,#204178,#204179,#204180,#204181,#204182,#204183,#204184,
#204185,#204186,#204187,#204188,#204189,#204190,#204191,#204192,#204193,
#204194,#204195,#204196,#204197,#204198,#204199,#204200,#204201,#204202,
#204203,#204204,#204205,#204206,#204207,#204208,#204209,#204210,#204211,
#204212,#204213,#204214,#204215,#204216,#204217,#204218,#204219,#204220,
#204221,#204222,#204223,#204224,#204225,#204226,#204227,#204228,#204229,
#204230,#204231,#204232,#204233,#204234,#204235,#204236,#204237,#204238,
#204239,#204240,#204241,#204242,#204243,#204244,#204245,#204246,#204247,
#204248,#204249,#204250,#204251,#204252,#204253,#204254,#204255,#204256,
#204257,#204258,#204259,#204260,#204261,#204262,#204263,#204264,#204265,
#204266,#204267,#204268,#204269,#204270,#204271,#204272,#204273,#204274,
#204275,#204276,#204277,#204278,#204279,#204280,#204281,#204282,#204283,
#204284,#204285,#204286,#204287,#204288,#204289,#204290,#204291,#204292,
#204293,#204294,#204295,#204296,#204297,#204298,#204299,#204300,#204301,
#204302,#204303,#204304,#204305,#204306,#204307,#204308,#204309,#204310,
#204311,#204312,#204313,#204314,#204315,#204316,#204317,#204318,#204319,
#204320,#204321,#204322,#204323,#204324,#204325,#204326,#204327,#204328,
#204329,#204330,#204331,#204332,#204333),.UNSPECIFIED.,.F.,.F.,(4,3,3,3,
3,3,3,3,3,3,3,3,3,3,3,3,3,3,3,3,3,3,3,3,3,3,3,3,3,3,3,3,3,3,3,3,3,3,3,3,
3,3,3,3,3,3,3,3,3,3,3,3,3,3,3,3,3,3,3,3,4),(-167.203857019737,-167.089811010942,
-166.97534442206,-166.860315018448,-166.805687143633,-166.70228742583,-166.59904112641,
-166.495916113768,-166.392856482536,-166.289828202843,-166.186797287972,
-166.083659483083,-165.980465364832,-165.877088418964,-165.806850693671,
-165.703453682928,-165.600210070056,-165.497087699756,-165.394030682219,
-165.291004983628,-165.187976613287,-165.084841278379,-164.981649592209,
-164.878274989697,-164.808014243709,-164.704622124948,-164.601383502989,
-164.498266247439,-164.395214418258,-164.292193974136,-164.189170916953,
-164.086040949216,-163.982854668774,-163.879485474421,-163.809177793747,
-163.705782197978,-163.602540048974,-163.499419208732,-163.396363761232,
-163.293339670433,-163.190312943454,-163.08717929565,-162.983989323685,
-162.880616460327,-162.810341343785,-162.706946384013,-162.603704872483,
-162.500584668762,-162.397529856858,-162.294506399785,-162.19148030372,
-162.088347278056,-161.985157924285,-161.881785665815,-161.811504893824,
-161.709471728966,-161.607582178419,-161.505807285033,-161.404097846253,
-161.302405175455,-161.271232394665),.UNSPECIFIED.);
#2059=B_SPLINE_CURVE_WITH_KNOTS('',3,(#204334,#204335,#204336,#204337,#204338,
#204339,#204340,#204341,#204342,#204343,#204344,#204345,#204346),
 .UNSPECIFIED.,.F.,.F.,(4,3,3,3,4),(-167.55333770454,-167.448855755634,
-167.344457480827,-167.240110523684,-167.203857020092),.UNSPECIFIED.);
#2060=B_SPLINE_CURVE_WITH_KNOTS('',3,(#204349,#204350,#204351,#204352,#204353,
#204354,#204355,#204356,#204357,#204358,#204359,#204360,#204361,#204362,
#204363,#204364,#204365,#204366,#204367,#204368,#204369,#204370,#204371,
#204372,#204373,#204374,#204375,#204376,#204377,#204378,#204379,#204380,
#204381,#204382,#204383,#204384,#204385,#204386,#204387,#204388,#204389,
#204390,#204391,#204392,#204393,#204394,#204395,#204396,#204397,#204398,
#204399,#204400,#204401,#204402,#204403,#204404,#204405,#204406,#204407,
#204408,#204409,#204410,#204411,#204412,#204413,#204414,#204415,#204416,
#204417,#204418,#204419,#204420,#204421,#204422,#204423,#204424,#204425,
#204426,#204427,#204428,#204429,#204430,#204431,#204432,#204433,#204434,
#204435,#204436,#204437,#204438,#204439,#204440,#204441,#204442,#204443,
#204444,#204445,#204446,#204447,#204448,#204449,#204450,#204451,#204452,
#204453,#204454,#204455,#204456,#204457,#204458,#204459,#204460,#204461,
#204462,#204463,#204464,#204465,#204466,#204467,#204468,#204469,#204470,
#204471,#204472,#204473,#204474,#204475,#204476,#204477,#204478,#204479,
#204480,#204481,#204482,#204483,#204484,#204485,#204486,#204487,#204488,
#204489,#204490,#204491,#204492,#204493,#204494,#204495,#204496,#204497,
#204498,#204499,#204500,#204501,#204502,#204503,#204504,#204505,#204506,
#204507,#204508),.UNSPECIFIED.,.F.,.F.,(4,3,3,3,3,3,3,3,3,3,3,3,3,3,3,3,
3,3,3,3,3,3,3,3,3,3,3,3,3,3,3,3,3,3,3,3,3,3,3,3,3,3,3,3,3,3,3,3,3,3,3,3,
3,4),(-172.787594225567,-172.684274861804,-172.581108909343,-172.478064373147,
-172.375085039686,-172.272136763294,-172.169185441327,-172.066129317591,
-171.963016197798,-171.859726812786,-171.799869393442,-171.696296438965,
-171.592873179124,-171.489566512639,-171.386322438044,-171.283107200028,
-171.179887083779,-171.076557935617,-170.973170984353,-170.869600941516,
-170.80103294348,-170.697770604844,-170.594663628611,-170.491680177536,
-170.388763416087,-170.285879110466,-170.182993071298,-170.080000538274,
-169.976952142771,-169.873720029761,-169.802196493519,-169.698775165844,
-169.595507193078,-169.492360519935,-169.389279247763,-169.286229378952,
-169.183176959081,-169.080017930163,-168.97680271242,-168.873405104616,
-168.803360043557,-168.69994450726,-168.59668195947,-168.493540133569,-168.390463349949,
-168.287417603378,-168.184368931446,-168.081213043256,-167.978000631122,
-167.874605253038,-167.804523593595,-167.699655949217,-167.594982598059,
-167.55333770454),.UNSPECIFIED.);
#2061=B_SPLINE_CURVE_WITH_KNOTS('',3,(#204511,#204512,#204513,#204514,#204515,
#204516,#204517,#204518,#204519,#204520,#204521,#204522,#204523,#204524,
#204525,#204526,#204527,#204528,#204529,#204530,#204531,#204532,#204533,
#204534,#204535,#204536,#204537,#204538,#204539,#204540,#204541,#204542,
#204543,#204544,#204545,#204546,#204547,#204548,#204549,#204550,#204551,
#204552,#204553,#204554,#204555,#204556,#204557,#204558,#204559,#204560,
#204561,#204562,#204563,#204564,#204565,#204566,#204567,#204568,#204569,
#204570,#204571,#204572,#204573,#204574,#204575,#204576,#204577,#204578,
#204579,#204580,#204581,#204582,#204583,#204584,#204585,#204586,#204587,
#204588,#204589,#204590,#204591,#204592,#204593,#204594,#204595,#204596,
#204597,#204598,#204599,#204600,#204601,#204602,#204603,#204604,#204605,
#204606,#204607,#204608,#204609,#204610,#204611,#204612,#204613,#204614,
#204615,#204616),.UNSPECIFIED.,.F.,.F.,(4,3,3,3,3,3,3,3,3,3,3,3,3,3,3,3,
3,3,3,3,3,3,3,3,3,3,3,3,3,3,3,3,3,3,3,4),(171.305836600057,171.407491404046,
171.509232486424,171.611015128153,171.712976057781,171.799869393442,171.903390392073,
172.006760388742,172.110012049377,172.213200068173,172.316358267267,172.419520427281,
172.522790560255,172.626117812871,172.729627673424,172.798705843404,172.901009665115,
173.003159435031,173.105191801349,173.207161461353,173.309103780221,173.411054082656,
173.513126731748,173.615262377252,173.717603714352,173.797542293366,173.903815640338,
174.015386028212,174.121306049069,174.227126474861,174.332875046754,174.43857941621,
174.544296925171,174.650019520939,174.75581508523,174.796378743328),
 .UNSPECIFIED.);
#2062=B_SPLINE_CURVE_WITH_KNOTS('',3,(#204619,#204620,#204621,#204622,#204623,
#204624,#204625,#204626,#204627,#204628,#204629,#204630,#204631,#204632,
#204633,#204634,#204635,#204636,#204637,#204638,#204639,#204640,#204641,
#204642,#204643,#204644,#204645,#204646,#204647,#204648,#204649,#204650,
#204651,#204652,#204653,#204654,#204655,#204656,#204657,#204658,#204659,
#204660,#204661,#204662,#204663,#204664,#204665,#204666,#204667,#204668,
#204669,#204670,#204671,#204672,#204673,#204674,#204675,#204676,#204677,
#204678,#204679,#204680,#204681,#204682,#204683,#204684,#204685,#204686,
#204687,#204688,#204689,#204690,#204691,#204692,#204693,#204694,#204695,
#204696,#204697,#204698,#204699,#204700,#204701,#204702,#204703,#204704,
#204705,#204706,#204707,#204708,#204709,#204710,#204711,#204712,#204713,
#204714,#204715,#204716,#204717,#204718,#204719,#204720,#204721,#204722,
#204723,#204724,#204725,#204726,#204727,#204728,#204729,#204730,#204731,
#204732,#204733,#204734,#204735,#204736,#204737,#204738,#204739,#204740,
#204741,#204742,#204743,#204744,#204745,#204746,#204747,#204748,#204749,
#204750,#204751,#204752,#204753,#204754,#204755,#204756,#204757,#204758,
#204759,#204760,#204761,#204762,#204763,#204764,#204765,#204766,#204767,
#204768,#204769,#204770,#204771,#204772,#204773,#204774,#204775,#204776,
#204777,#204778),.UNSPECIFIED.,.F.,.F.,(4,3,3,3,3,3,3,3,3,3,3,3,3,3,3,3,
3,3,3,3,3,3,3,3,3,3,3,3,3,3,3,3,3,3,3,3,3,3,3,3,3,3,3,3,3,3,3,3,3,3,3,3,
3,4),(-172.787594226707,-172.684274547493,-172.581108276202,-172.478063417649,
-172.375083759813,-172.272135157488,-172.169183508487,-172.066127058214,
-171.963013611671,-171.859723903019,-171.799869393442,-171.696296383671,
-171.592873066918,-171.489566341367,-171.386322206412,-171.283106906827,
-171.179886727883,-171.076557515714,-170.973170499612,-170.8696003913,-170.80103294348,
-170.697770746273,-170.594663913509,-170.491680608289,-170.388763994098,
-170.285879836938,-170.182993947235,-170.08000156422,-169.976953319269,
-169.873721356035,-169.802196493519,-169.698775105051,-169.595507070885,
-169.492360335737,-169.38927900122,-169.286229069815,-169.183176587192,
-169.080017495714,-168.976802215422,-168.873404545781,-168.803360043557,
-168.699944492337,-168.59668192921,-168.493540087422,-168.390463287585,
-168.287417524489,-168.184368835746,-168.081212930417,-167.978000500935,
-167.874605105352,-167.804523593595,-167.699655977959,-167.594982656148,
-167.553337646663),.UNSPECIFIED.);
#2063=B_SPLINE_CURVE_WITH_KNOTS('',3,(#204781,#204782,#204783,#204784,#204785,
#204786,#204787,#204788,#204789,#204790,#204791,#204792,#204793,#204794,
#204795,#204796,#204797,#204798,#204799,#204800,#204801,#204802,#204803,
#204804,#204805,#204806,#204807,#204808,#204809,#204810,#204811,#204812,
#204813,#204814,#204815,#204816,#204817,#204818,#204819,#204820,#204821,
#204822,#204823,#204824,#204825,#204826,#204827,#204828,#204829,#204830,
#204831,#204832,#204833,#204834,#204835,#204836,#204837,#204838,#204839,
#204840,#204841,#204842,#204843,#204844,#204845,#204846,#204847,#204848,
#204849,#204850,#204851,#204852,#204853,#204854,#204855,#204856,#204857,
#204858,#204859,#204860,#204861,#204862,#204863,#204864,#204865,#204866,
#204867,#204868,#204869,#204870,#204871,#204872,#204873,#204874,#204875,
#204876,#204877,#204878,#204879,#204880,#204881,#204882,#204883,#204884,
#204885,#204886),.UNSPECIFIED.,.F.,.F.,(4,3,3,3,3,3,3,3,3,3,3,3,3,3,3,3,
3,3,3,3,3,3,3,3,3,3,3,3,3,3,3,3,3,3,3,4),(171.305836553012,171.407491357116,
171.509232440247,171.611015083074,171.712976014387,171.799869393442,171.903390296067,
172.006760196182,172.110011759924,172.213199681674,172.316357783713,172.419519846812,
172.522789883762,172.626117040711,172.729626807232,172.798705843404,172.901009858667,
173.003159822786,173.105192383572,173.207162238204,173.309104751679,173.411055248523,
173.513128090537,173.615263928529,173.717605455249,173.797542293366,173.90381549814,
174.015385903789,174.121305781442,174.227126064404,174.332874494259,174.438578722884,
174.544296093967,174.650018553652,174.755813985758,174.796378743328),
 .UNSPECIFIED.);
#2064=B_SPLINE_CURVE_WITH_KNOTS('',3,(#204889,#204890,#204891,#204892,#204893,
#204894,#204895,#204896,#204897,#204898,#204899,#204900,#204901,#204902,
#204903,#204904,#204905,#204906,#204907,#204908,#204909,#204910,#204911,
#204912,#204913,#204914,#204915,#204916,#204917,#204918,#204919,#204920,
#204921,#204922,#204923,#204924,#204925,#204926,#204927,#204928,#204929,
#204930,#204931,#204932,#204933,#204934,#204935,#204936,#204937,#204938,
#204939,#204940,#204941,#204942,#204943,#204944,#204945,#204946,#204947,
#204948,#204949,#204950,#204951,#204952,#204953,#204954,#204955,#204956,
#204957,#204958,#204959,#204960,#204961,#204962,#204963,#204964,#204965,
#204966,#204967,#204968,#204969,#204970,#204971,#204972,#204973,#204974,
#204975,#204976,#204977,#204978,#204979,#204980,#204981,#204982,#204983,
#204984,#204985,#204986,#204987,#204988,#204989,#204990,#204991,#204992,
#204993,#204994,#204995,#204996,#204997,#204998,#204999,#205000,#205001,
#205002,#205003,#205004,#205005,#205006,#205007,#205008,#205009,#205010,
#205011,#205012,#205013,#205014,#205015,#205016,#205017,#205018,#205019,
#205020,#205021,#205022,#205023,#205024,#205025,#205026,#205027,#205028,
#205029,#205030,#205031,#205032,#205033,#205034,#205035,#205036,#205037,
#205038,#205039,#205040,#205041,#205042,#205043,#205044,#205045,#205046,
#205047,#205048),.UNSPECIFIED.,.F.,.F.,(4,3,3,3,3,3,3,3,3,3,3,3,3,3,3,3,
3,3,3,3,3,3,3,3,3,3,3,3,3,3,3,3,3,3,3,3,3,3,3,3,3,3,3,3,3,3,3,3,3,3,3,3,
3,4),(-172.787594226732,-172.684274540723,-172.581108262565,-172.478063397069,
-172.375083732247,-172.272135122901,-172.169183466856,-172.06612700955,
-171.963013555969,-171.859723840347,-171.799869393442,-171.69629638248,
-171.592873064501,-171.489566337677,-171.386322201422,-171.28310690051,
-171.179886720216,-171.076557506667,-170.973170489168,-170.869600379445,
-170.801032943481,-170.697770749322,-170.594663919649,-170.491680617572,
-170.388764006554,-170.285879852593,-170.18299396611,-170.080001586328,
-169.976953344622,-169.873721384615,-169.802196493519,-169.69877510374,
-169.595507068251,-169.492360331767,-169.389278995906,-169.286229063151,
-169.183176579175,-169.080017486348,-168.976802204708,-168.873404533735,
-168.803360043557,-168.699944492016,-168.596681928558,-168.493540086429,
-168.390463286242,-168.28741752279,-168.184368833685,-168.081212927987,
-167.978000498131,-167.874605102172,-167.804523593595,-167.699655978575,
-167.594982657392,-167.553337655846),.UNSPECIFIED.);
#2065=B_SPLINE_CURVE_WITH_KNOTS('',3,(#205051,#205052,#205053,#205054,#205055,
#205056,#205057,#205058,#205059,#205060,#205061,#205062,#205063,#205064,
#205065,#205066,#205067,#205068,#205069,#205070,#205071,#205072,#205073,
#205074,#205075,#205076,#205077,#205078,#205079,#205080,#205081,#205082,
#205083,#205084,#205085,#205086,#205087,#205088,#205089,#205090,#205091,
#205092,#205093,#205094,#205095,#205096,#205097,#205098,#205099,#205100,
#205101,#205102,#205103,#205104,#205105,#205106,#205107,#205108,#205109,
#205110,#205111,#205112,#205113,#205114,#205115,#205116,#205117,#205118,
#205119,#205120,#205121,#205122,#205123,#205124,#205125,#205126,#205127,
#205128,#205129,#205130,#205131,#205132,#205133,#205134,#205135,#205136,
#205137,#205138,#205139,#205140,#205141,#205142,#205143,#205144,#205145,
#205146,#205147,#205148,#205149,#205150,#205151,#205152,#205153,#205154,
#205155,#205156),.UNSPECIFIED.,.F.,.F.,(4,3,3,3,3,3,3,3,3,3,3,3,3,3,3,3,
3,3,3,3,3,3,3,3,3,3,3,3,3,3,3,3,3,3,3,4),(171.305836564222,171.407491368278,
171.509232451096,171.611015093464,171.71297602408,171.799869393442,171.903390335715,
172.006760275705,172.110011879462,172.21319984129,172.31635798341,172.419520086533,
172.522790163139,172.626117359596,172.72962716495,172.798705843404,172.901009778732,
173.003159662647,173.105192143119,173.207161917372,173.309104350476,173.411054767032,
173.513127529371,173.615263287867,173.717604736276,173.797542293366,173.903815556868,
174.015385955175,174.121305891971,174.227126233922,174.332874722438,174.438579009226,
174.544296437251,174.650018953138,174.755814439837,174.796378743328),
 .UNSPECIFIED.);
#2066=B_SPLINE_CURVE_WITH_KNOTS('',3,(#205159,#205160,#205161,#205162,#205163,
#205164,#205165,#205166,#205167,#205168,#205169,#205170,#205171,#205172,
#205173,#205174,#205175,#205176,#205177,#205178,#205179,#205180,#205181,
#205182,#205183,#205184,#205185,#205186,#205187,#205188,#205189,#205190,
#205191,#205192,#205193,#205194,#205195,#205196,#205197,#205198,#205199,
#205200,#205201,#205202,#205203,#205204,#205205,#205206,#205207,#205208,
#205209,#205210,#205211,#205212,#205213,#205214,#205215,#205216,#205217,
#205218,#205219,#205220,#205221,#205222,#205223,#205224,#205225,#205226,
#205227,#205228,#205229,#205230,#205231,#205232,#205233,#205234,#205235,
#205236,#205237,#205238,#205239,#205240,#205241,#205242,#205243,#205244,
#205245,#205246,#205247,#205248,#205249,#205250,#205251,#205252,#205253,
#205254,#205255,#205256,#205257,#205258,#205259,#205260,#205261,#205262,
#205263,#205264,#205265,#205266,#205267,#205268,#205269,#205270,#205271,
#205272,#205273,#205274,#205275,#205276,#205277,#205278,#205279,#205280,
#205281,#205282,#205283,#205284,#205285,#205286,#205287,#205288,#205289,
#205290,#205291,#205292,#205293,#205294,#205295,#205296,#205297,#205298,
#205299,#205300,#205301,#205302,#205303,#205304,#205305,#205306,#205307,
#205308,#205309,#205310,#205311,#205312,#205313,#205314,#205315,#205316,
#205317,#205318),.UNSPECIFIED.,.F.,.F.,(4,3,3,3,3,3,3,3,3,3,3,3,3,3,3,3,
3,3,3,3,3,3,3,3,3,3,3,3,3,3,3,3,3,3,3,3,3,3,3,3,3,3,3,3,3,3,3,3,3,3,3,3,
3,4),(-172.787594226351,-172.684274645609,-172.581108473843,-172.478063715916,
-172.375084159336,-172.272135658752,-172.169184111836,-172.066127763492,
-171.963014418944,-171.859724811317,-171.799869393442,-171.696296400939,
-171.592873101958,-171.489566394852,-171.386322278747,-171.283106998388,
-171.179886839023,-171.076557646842,-170.973170650988,-170.869600563122,
-170.801032943481,-170.69777070211,-170.594663824546,-170.491680473781,
-170.388763813606,-170.285879610087,-170.182993673711,-170.080001243854,
-169.976952951891,-169.873720941887,-169.802196493519,-169.698775124036,
-169.595507109046,-169.492360393262,-169.389279078215,-169.286229166357,
-169.183176703332,-169.080017631391,-168.976802370632,-168.873404720303,
-168.803360043557,-168.699944496997,-168.59668193866,-168.493540101833,
-168.39046330706,-168.287417549124,-168.184368865631,-168.081212965654,
-167.978000541589,-167.874605151471,-167.804523593595,-167.699655968957,
-167.594982637949,-167.55333773927),.UNSPECIFIED.);
#2067=B_SPLINE_CURVE_WITH_KNOTS('',3,(#205321,#205322,#205323,#205324,#205325,
#205326,#205327,#205328,#205329,#205330,#205331,#205332,#205333,#205334,
#205335,#205336,#205337,#205338,#205339,#205340,#205341,#205342,#205343,
#205344,#205345,#205346,#205347,#205348,#205349,#205350,#205351,#205352,
#205353,#205354,#205355,#205356,#205357,#205358,#205359,#205360,#205361,
#205362,#205363,#205364,#205365,#205366,#205367,#205368,#205369,#205370,
#205371,#205372,#205373,#205374,#205375,#205376,#205377,#205378,#205379,
#205380,#205381,#205382,#205383,#205384,#205385,#205386,#205387,#205388,
#205389,#205390,#205391,#205392,#205393,#205394,#205395,#205396,#205397,
#205398,#205399,#205400,#205401,#205402,#205403,#205404,#205405,#205406,
#205407,#205408,#205409,#205410,#205411,#205412,#205413,#205414,#205415,
#205416,#205417,#205418,#205419,#205420,#205421,#205422,#205423,#205424,
#205425,#205426),.UNSPECIFIED.,.F.,.F.,(4,3,3,3,3,3,3,3,3,3,3,3,3,3,3,3,
3,3,3,3,3,3,3,3,3,3,3,3,3,3,3,3,3,3,3,4),(171.305836655045,171.407491458764,
171.509232539317,171.611015178365,171.712976103912,171.799869393442,171.903390623982,
172.006760853885,172.110012748576,172.2132010018,172.316359435341,172.419521829469,
172.522792194405,172.626119678124,172.729629765827,172.798705843404,172.90100919765,
173.00315849853,173.10519039517,173.207159585109,173.309101433958,173.411051266852,
173.513123449993,173.615258630591,173.71759950971,173.797542293366,173.903815983742,
174.01538632869,174.121306695383,174.227127466107,174.332876381024,174.438581090584,
174.544298932523,174.650021856933,174.755817740451,174.796378743328),
 .UNSPECIFIED.);
#2068=B_SPLINE_CURVE_WITH_KNOTS('',3,(#205429,#205430,#205431,#205432,#205433,
#205434,#205435,#205436,#205437,#205438,#205439,#205440,#205441,#205442,
#205443,#205444),.UNSPECIFIED.,.F.,.F.,(4,2,2,2,2,2,2,4),(-3.36796842350093,
-3.29693348725048,-3.2276059680982,-3.10443413185248,-3.02217223145102,
-2.85176927650461,-2.77989380916357,-2.68789745416103),.UNSPECIFIED.);
#2069=B_SPLINE_CURVE_WITH_KNOTS('',3,(#205448,#205449,#205450,#205451,#205452,
#205453,#205454,#205455,#205456,#205457,#205458,#205459,#205460,#205461,
#205462),.UNSPECIFIED.,.F.,.F.,(4,1,1,1,1,1,1,1,1,1,1,1,4),(2.02178176728025,
2.43673748880502,2.92408498656602,3.41143248432702,3.89877998208802,4.38612747984902,
4.87347497761003,5.36082247537103,5.84816997313203,6.33551747089303,6.82286496865404,
7.31021246641504,7.59153924858055),.UNSPECIFIED.);
#2070=B_SPLINE_CURVE_WITH_KNOTS('',3,(#205465,#205466,#205467,#205468,#205469,
#205470,#205471,#205472,#205473,#205474,#205475,#205476,#205477,#205478,
#205479,#205480,#205481,#205482,#205483,#205484,#205485,#205486,#205487,
#205488,#205489,#205490,#205491,#205492,#205493,#205494,#205495,#205496,
#205497,#205498),.UNSPECIFIED.,.F.,.F.,(4,2,2,2,2,2,2,2,2,2,2,2,2,2,2,2,
4),(2.08269173712794E-5,0.0904906817544001,0.176689485912824,0.297418593220784,
0.379377464742978,0.549734405369124,0.620055052536581,0.741861277008205,
0.810969949261042,0.891261322378703,1.03196791749396,1.11156489827869,1.23025736979253,
1.31034234680985,1.4491620241015,1.58466358484633,1.64869401953039),
 .UNSPECIFIED.);
#2071=B_SPLINE_CURVE_WITH_KNOTS('',3,(#205501,#205502,#205503,#205504,#205505,
#205506,#205507),.UNSPECIFIED.,.F.,.F.,(4,1,1,1,4),(183.127688252684,183.201986895449,
184.200823345411,185.199659795373,185.353966561798),.UNSPECIFIED.);
#2072=B_SPLINE_CURVE_WITH_KNOTS('',3,(#205509,#205510,#205511,#205512,#205513,
#205514,#205515,#205516,#205517,#205518,#205519,#205520,#205521,#205522,
#205523,#205524,#205525,#205526,#205527,#205528,#205529,#205530,#205531,
#205532,#205533,#205534,#205535,#205536,#205537,#205538,#205539,#205540,
#205541,#205542,#205543,#205544,#205545,#205546,#205547,#205548,#205549,
#205550,#205551,#205552,#205553,#205554,#205555,#205556,#205557,#205558,
#205559,#205560,#205561,#205562,#205563,#205564,#205565,#205566),
 .UNSPECIFIED.,.F.,.F.,(4,3,3,3,3,3,3,3,3,3,3,3,3,3,3,3,3,3,3,4),(185.353966561798,
185.451129862355,185.548173545581,185.645152144533,185.742096651447,185.839038013602,
185.93606867674,186.033145889087,186.130383557083,186.198496245335,186.297012011071,
186.39538977669,186.494243904503,186.592449804335,186.690624726039,186.788798244729,
186.888154383345,186.9864710254,187.086346912297,187.186222799194),
 .UNSPECIFIED.);
#2073=B_SPLINE_CURVE_WITH_KNOTS('',3,(#205570,#205571,#205572,#205573,#205574),
 .UNSPECIFIED.,.F.,.F.,(4,1,4),(185.353966561798,185.664466527893,186.663302977854),
 .UNSPECIFIED.);
#2074=B_SPLINE_CURVE_WITH_KNOTS('',3,(#205575,#205576,#205577,#205578,#205579,
#205580),.UNSPECIFIED.,.F.,.F.,(4,1,1,4),(183.128402505335,183.666793627969,
184.665630077931,185.353966561798),.UNSPECIFIED.);
#2075=B_SPLINE_CURVE_WITH_KNOTS('',3,(#205583,#205584,#205585,#205586,#205587,
#205588,#205589),.UNSPECIFIED.,.F.,.F.,(4,1,1,1,4),(183.127688302604,183.201986895449,
184.200823345411,185.199659795373,185.353966561798),.UNSPECIFIED.);
#2076=B_SPLINE_CURVE_WITH_KNOTS('',3,(#205591,#205592,#205593,#205594,#205595,
#205596,#205597,#205598,#205599,#205600,#205601,#205602,#205603,#205604,
#205605,#205606,#205607,#205608,#205609,#205610,#205611,#205612,#205613,
#205614,#205615,#205616,#205617,#205618,#205619,#205620,#205621,#205622,
#205623,#205624,#205625,#205626,#205627,#205628,#205629,#205630,#205631,
#205632,#205633,#205634,#205635,#205636,#205637,#205638,#205639,#205640,
#205641,#205642,#205643,#205644,#205645,#205646,#205647,#205648),
 .UNSPECIFIED.,.F.,.F.,(4,3,3,3,3,3,3,3,3,3,3,3,3,3,3,3,3,3,3,4),(185.353966561798,
185.451129857721,185.548173538225,185.645152135629,185.742096642157,185.839038005082,
185.936068670734,186.033145886574,186.130383559583,186.198496245335,186.297011743078,
186.39538923924,186.494243434233,186.592449062934,186.690623713446,186.78879696123,
186.88815342072,186.986469795236,187.086346297213,187.186222799189),
 .UNSPECIFIED.);
#2077=B_SPLINE_CURVE_WITH_KNOTS('',3,(#205652,#205653,#205654,#205655,#205656),
 .UNSPECIFIED.,.F.,.F.,(4,1,4),(185.353966561798,185.664466527893,186.663302977854),
 .UNSPECIFIED.);
#2078=B_SPLINE_CURVE_WITH_KNOTS('',3,(#205657,#205658,#205659,#205660,#205661,
#205662),.UNSPECIFIED.,.F.,.F.,(4,1,1,4),(183.128402568106,183.666793627969,
184.665630077931,185.353966561798),.UNSPECIFIED.);
#2079=B_SPLINE_CURVE_WITH_KNOTS('',3,(#205665,#205666,#205667,#205668,#205669,
#205670,#205671),.UNSPECIFIED.,.F.,.F.,(4,1,1,1,4),(183.127688309466,183.201986895449,
184.200823345411,185.199659795373,185.353966561798),.UNSPECIFIED.);
#2080=B_SPLINE_CURVE_WITH_KNOTS('',3,(#205673,#205674,#205675,#205676,#205677,
#205678,#205679,#205680,#205681,#205682,#205683,#205684,#205685,#205686,
#205687,#205688,#205689,#205690,#205691,#205692,#205693,#205694,#205695,
#205696,#205697,#205698,#205699,#205700,#205701,#205702,#205703,#205704,
#205705,#205706,#205707,#205708,#205709,#205710,#205711,#205712,#205713,
#205714,#205715,#205716,#205717,#205718,#205719,#205720,#205721,#205722,
#205723,#205724,#205725,#205726,#205727,#205728,#205729,#205730),
 .UNSPECIFIED.,.F.,.F.,(4,3,3,3,3,3,3,3,3,3,3,3,3,3,3,3,3,3,3,4),(185.353966561798,
185.451129857085,185.548173537216,185.645152134409,185.742096640885,185.839038003917,
185.936068669915,186.033145886238,186.130383559937,186.198496245335,186.297011706217,
186.395389165318,186.494243369552,186.592448960961,186.690623574174,186.788796784698,
186.888153288321,186.986469626041,187.086346212615,187.186222799188),
 .UNSPECIFIED.);
#2081=B_SPLINE_CURVE_WITH_KNOTS('',3,(#205734,#205735,#205736,#205737,#205738),
 .UNSPECIFIED.,.F.,.F.,(4,1,4),(185.353966561798,185.664466527893,186.663302977854),
 .UNSPECIFIED.);
#2082=B_SPLINE_CURVE_WITH_KNOTS('',3,(#205739,#205740,#205741,#205742,#205743,
#205744),.UNSPECIFIED.,.F.,.F.,(4,1,1,4),(183.128402575235,183.666793627969,
184.665630077931,185.353966561798),.UNSPECIFIED.);
#2083=B_SPLINE_CURVE_WITH_KNOTS('',3,(#205747,#205748,#205749,#205750,#205751,
#205752,#205753),.UNSPECIFIED.,.F.,.F.,(4,1,1,1,4),(183.12768829285,183.201986895449,
184.200823345411,185.199659795373,185.353966561798),.UNSPECIFIED.);
#2084=B_SPLINE_CURVE_WITH_KNOTS('',3,(#205755,#205756,#205757,#205758,#205759,
#205760,#205761,#205762,#205763,#205764,#205765,#205766,#205767,#205768,
#205769,#205770,#205771,#205772,#205773,#205774,#205775,#205776,#205777,
#205778,#205779,#205780,#205781,#205782,#205783,#205784,#205785,#205786,
#205787,#205788,#205789,#205790,#205791,#205792,#205793,#205794,#205795,
#205796,#205797,#205798,#205799,#205800,#205801,#205802,#205803,#205804,
#205805,#205806,#205807,#205808,#205809,#205810,#205811,#205812),
 .UNSPECIFIED.,.F.,.F.,(4,3,3,3,3,3,3,3,3,3,3,3,3,3,3,3,3,3,3,4),(185.353966561798,
185.451129858625,185.54817353966,185.645152137366,185.742096643968,185.839038006741,
185.9360686719,186.033145887057,186.130383559085,186.198496245335,186.297011795472,
186.395389344314,186.494243526173,186.592449207881,186.690623911412,186.788797212158,
186.888153608916,186.986470035736,187.086346417463,187.18622279919),
 .UNSPECIFIED.);
#2085=B_SPLINE_CURVE_WITH_KNOTS('',3,(#205816,#205817,#205818,#205819,#205820),
 .UNSPECIFIED.,.F.,.F.,(4,1,4),(185.353966561798,185.664466527893,186.663302977854),
 .UNSPECIFIED.);
#2086=B_SPLINE_CURVE_WITH_KNOTS('',3,(#205821,#205822,#205823,#205824,#205825,
#205826),.UNSPECIFIED.,.F.,.F.,(4,1,1,4),(183.128402534571,183.666793627969,
184.665630077931,185.353966561798),.UNSPECIFIED.);
#2087=B_SPLINE_CURVE_WITH_KNOTS('',3,(#205829,#205830,#205831,#205832,#205833,
#205834),.UNSPECIFIED.,.F.,.F.,(4,1,1,4),(33.4844854751707,33.8935092369881,
34.3808567347491,34.5575191593334),.UNSPECIFIED.);
#2088=B_SPLINE_CURVE_WITH_KNOTS('',3,(#205836,#205837,#205838,#205839,#205840,
#205841,#205842,#205843,#205844,#205845,#205846,#205847,#205848,#205849,
#205850,#205851,#205852,#205853,#205854,#205855,#205856,#205857,#205858,
#205859,#205860,#205861,#205862,#205863,#205864,#205865,#205866,#205867,
#205868,#205869,#205870,#205871,#205872,#205873,#205874,#205875,#205876,
#205877,#205878,#205879,#205880,#205881,#205882,#205883,#205884,#205885,
#205886,#205887,#205888,#205889,#205890,#205891,#205892,#205893,#205894,
#205895,#205896,#205897,#205898,#205899,#205900,#205901,#205902,#205903,
#205904,#205905,#205906,#205907,#205908,#205909,#205910,#205911,#205912,
#205913,#205914,#205915,#205916,#205917,#205918,#205919,#205920,#205921,
#205922,#205923,#205924,#205925,#205926,#205927,#205928,#205929,#205930,
#205931,#205932,#205933,#205934,#205935,#205936,#205937,#205938,#205939,
#205940,#205941,#205942,#205943,#205944,#205945,#205946,#205947,#205948,
#205949,#205950,#205951,#205952,#205953,#205954,#205955,#205956,#205957,
#205958,#205959,#205960,#205961,#205962,#205963,#205964,#205965,#205966,
#205967,#205968,#205969,#205970,#205971,#205972,#205973,#205974,#205975,
#205976,#205977,#205978,#205979,#205980,#205981,#205982,#205983,#205984,
#205985,#205986,#205987,#205988,#205989),.UNSPECIFIED.,.F.,.F.,(4,3,3,3,
3,3,3,3,3,3,3,3,3,3,3,3,3,3,3,3,3,3,3,3,3,3,3,3,3,3,3,3,3,3,3,3,3,3,3,3,
3,3,3,3,3,3,3,3,3,3,3,4),(34.5575191894877,34.6447569868975,34.7319919193617,
34.8192474749927,34.8682042325101,34.9553345482705,35.0424483237626,35.1295651730742,
35.2166773096183,35.3038088155763,35.3555517302711,35.4426813818879,35.5297944898996,
35.6169106732714,35.7040221463605,35.7911529985374,35.8428992280321,35.9300290900273,
36.0171424031941,36.1042587818684,36.1913704442032,36.2785014746032,36.3302467257931,
36.4173754321069,36.5044875913759,36.5916028300414,36.6787133629673,36.7658432901786,
36.8175942235541,36.9047259024205,36.9918410382111,37.0789592304618,37.1660726969111,
37.2532055011073,37.3049417213151,37.3920685401476,37.4791788111556,37.5662921786384,
37.6534008545103,37.7405289626034,37.7922892190761,37.8794201719593,37.966534565058,
38.0536519969681,38.1407646949544,38.2278967250119,38.2796367168371,38.3664398085489,
38.4532349861649,38.5400191597449,38.6268188966943,38.6945925143091),
 .UNSPECIFIED.);
#2089=B_SPLINE_CURVE_WITH_KNOTS('',3,(#205993,#205994,#205995,#205996,#205997,
#205998,#205999,#206000,#206001,#206002,#206003),.UNSPECIFIED.,.F.,.F.,
(4,1,1,1,1,1,1,1,4),(34.5575192147677,34.7582752591941,35.2456227569552,
35.7329702547162,36.2203177524772,36.7076652502382,37.1950127479992,37.6823602457602,
38.1697077435212),.UNSPECIFIED.);
#2090=B_SPLINE_CURVE_WITH_KNOTS('',3,(#206004,#206005,#206006,#206007,#206008,
#206009,#206010,#206011,#206012,#206013,#206014,#206015,#206016,#206017,
#206018,#206019,#206020,#206021,#206022,#206023,#206024,#206025,#206026,
#206027,#206028,#206029,#206030,#206031,#206032,#206033,#206034,#206035,
#206036,#206037,#206038,#206039,#206040,#206041,#206042,#206043,#206044,
#206045,#206046),.UNSPECIFIED.,.F.,.F.,(4,3,3,3,3,3,3,3,3,3,3,3,3,3,4),
(33.4844725988534,33.5715877001674,33.6586993242475,33.7458293437006,33.7835802636721,
33.8707089685104,33.9578211263055,34.0449363635138,34.1320468949955,34.2191768207952,
34.2709277614331,34.3584567371214,34.4459664694995,34.5334668195807,34.5575191894877),
 .UNSPECIFIED.);
#2091=B_SPLINE_CURVE_WITH_KNOTS('',3,(#206049,#206050,#206051,#206052,#206053,
#206054),.UNSPECIFIED.,.F.,.F.,(4,1,1,4),(33.4844854782753,33.8935092369881,
34.3808567347491,34.5575191593289),.UNSPECIFIED.);
#2092=B_SPLINE_CURVE_WITH_KNOTS('',3,(#206056,#206057,#206058,#206059,#206060,
#206061,#206062,#206063,#206064,#206065,#206066,#206067,#206068,#206069,
#206070,#206071,#206072,#206073,#206074,#206075,#206076,#206077,#206078,
#206079,#206080,#206081,#206082,#206083,#206084,#206085,#206086,#206087,
#206088,#206089,#206090,#206091,#206092,#206093,#206094,#206095,#206096,
#206097,#206098,#206099,#206100,#206101,#206102,#206103,#206104,#206105,
#206106,#206107,#206108,#206109,#206110,#206111,#206112,#206113,#206114,
#206115,#206116,#206117,#206118,#206119,#206120,#206121,#206122,#206123,
#206124,#206125,#206126,#206127,#206128,#206129,#206130,#206131,#206132,
#206133,#206134,#206135,#206136,#206137,#206138,#206139,#206140,#206141,
#206142,#206143,#206144,#206145,#206146,#206147,#206148,#206149,#206150,
#206151,#206152,#206153,#206154,#206155,#206156,#206157,#206158,#206159,
#206160,#206161,#206162,#206163,#206164,#206165,#206166,#206167,#206168,
#206169,#206170,#206171,#206172,#206173,#206174,#206175,#206176,#206177,
#206178,#206179,#206180,#206181,#206182,#206183,#206184,#206185,#206186,
#206187,#206188,#206189,#206190,#206191,#206192,#206193,#206194,#206195,
#206196,#206197,#206198,#206199,#206200,#206201,#206202,#206203,#206204,
#206205,#206206,#206207,#206208,#206209),.UNSPECIFIED.,.F.,.F.,(4,3,3,3,
3,3,3,3,3,3,3,3,3,3,3,3,3,3,3,3,3,3,3,3,3,3,3,3,3,3,3,3,3,3,3,3,3,3,3,3,
3,3,3,3,3,3,3,3,3,3,3,4),(34.5575191894877,34.6447569757657,34.7319918970944,
34.8192474416769,34.8682042325101,34.9553345524685,35.0424483321962,35.1295651857588,
35.2166773265522,35.3038088367198,35.3555517302711,35.4426813814716,35.5297944890805,
35.6169106720737,35.7040221447989,35.7911529966377,35.8428992280321,35.9300290910938,
36.0171424053112,36.1042587850018,36.191370448331,36.278501479683,36.3302467257931,
36.4173754284676,36.5044875841013,36.5916028191727,36.6787133485363,36.7658432722657,
36.8175942235541,36.9047259080441,36.9918410494598,37.0789592472834,37.1660727192629,
37.2532055288754,37.3049417213151,37.3920685377782,37.4791788064371,37.5662921716237,
37.6534008452347,37.7405289511405,37.7922892190762,37.8794201571563,37.966534535352,
38.0536519523545,38.1407646354665,38.2278966508317,38.2796367168372,38.3664398614179,
38.4532350920939,38.5400193187296,38.6268191082651,38.6945925143091),
 .UNSPECIFIED.);
#2093=B_SPLINE_CURVE_WITH_KNOTS('',3,(#206213,#206214,#206215,#206216,#206217,
#206218,#206219,#206220,#206221,#206222,#206223),.UNSPECIFIED.,.F.,.F.,
(4,1,1,1,1,1,1,1,4),(34.5575192147699,34.7582752591942,35.2456227569552,
35.7329702547162,36.2203177524772,36.7076652502382,37.1950127479992,37.6823602457602,
38.1697077435212),.UNSPECIFIED.);
#2094=B_SPLINE_CURVE_WITH_KNOTS('',3,(#206224,#206225,#206226,#206227,#206228,
#206229,#206230,#206231,#206232,#206233,#206234,#206235,#206236,#206237,
#206238,#206239,#206240,#206241,#206242,#206243,#206244,#206245,#206246,
#206247,#206248,#206249,#206250,#206251,#206252,#206253,#206254,#206255,
#206256,#206257,#206258,#206259,#206260,#206261,#206262,#206263,#206264,
#206265,#206266),.UNSPECIFIED.,.F.,.F.,(4,3,3,3,3,3,3,3,3,3,3,3,3,3,4),
(33.4844725969432,33.5715876990605,33.6586993239259,33.7458293441317,33.7835802636722,
33.8707089656242,33.9578211205362,34.0449363548941,34.1320468835505,34.2191768065887,
34.2709277614332,34.3584567439305,34.4459664831206,34.5334668399684,34.5575191894877),
 .UNSPECIFIED.);
#2095=B_SPLINE_CURVE_WITH_KNOTS('',3,(#206401,#206402,#206403,#206404,#206405,
#206406,#206407,#206408,#206409,#206410,#206411,#206412,#206413,#206414,
#206415,#206416,#206417,#206418,#206419,#206420,#206421,#206422,#206423,
#206424,#206425,#206426,#206427,#206428,#206429,#206430,#206431,#206432,
#206433,#206434,#206435,#206436,#206437,#206438,#206439,#206440,#206441,
#206442,#206443,#206444,#206445,#206446,#206447,#206448,#206449,#206450,
#206451,#206452,#206453,#206454,#206455,#206456,#206457,#206458,#206459,
#206460,#206461,#206462,#206463,#206464,#206465,#206466,#206467,#206468,
#206469,#206470,#206471,#206472,#206473,#206474,#206475,#206476,#206477,
#206478,#206479,#206480,#206481,#206482,#206483,#206484,#206485,#206486,
#206487,#206488),.UNSPECIFIED.,.F.,.F.,(4,3,3,3,3,3,3,3,3,3,3,3,3,3,3,3,
3,3,3,3,3,3,3,3,3,3,3,3,3,4),(0.,0.0223800438562092,0.0455571551208265,
0.0675550647019532,0.0773342777042101,0.0821512753707187,0.0865889152558688,
0.110577888018852,0.135008177242286,0.157206748761003,0.165672870216831,
0.170323072593406,0.173915834948667,0.198993095015584,0.224022472738064,
0.248522734273475,0.258554636060882,0.264135020452961,0.288903377496841,
0.314991214965925,0.34107905243501,0.351267090483404,0.355315312120404,
0.381664714548268,0.403487578295303,0.410694478291004,0.416463279199868,
0.443066534667853,0.469275862304387,0.472065636590528),.UNSPECIFIED.);
#2096=B_SPLINE_CURVE_WITH_KNOTS('',3,(#206489,#206490,#206491,#206492,#206493,
#206494,#206495,#206496,#206497,#206498,#206499,#206500,#206501,#206502,
#206503,#206504,#206505,#206506,#206507,#206508,#206509,#206510,#206511,
#206512,#206513,#206514,#206515,#206516,#206517,#206518,#206519,#206520,
#206521,#206522,#206523,#206524,#206525,#206526,#206527,#206528,#206529,
#206530,#206531,#206532,#206533,#206534,#206535,#206536,#206537,#206538,
#206539,#206540,#206541,#206542,#206543,#206544,#206545,#206546,#206547,
#206548,#206549,#206550,#206551,#206552,#206553,#206554,#206555,#206556,
#206557,#206558,#206559,#206560,#206561,#206562,#206563,#206564,#206565,
#206566,#206567,#206568,#206569,#206570,#206571,#206572,#206573,#206574,
#206575,#206576),.UNSPECIFIED.,.F.,.F.,(4,3,3,3,3,3,3,3,3,3,3,3,3,3,3,3,
3,3,3,3,3,3,3,3,3,3,3,3,3,4),(0.,0.0260517790363247,0.0527225331749561,
0.0776790837678674,0.0889727987852075,0.0959464344588869,0.100845925000849,
0.126855201330774,0.152534130317405,0.176212520341607,0.186122361847472,
0.192547946339425,0.196620306261614,0.221672219573634,0.246724132885653,
0.272050620367204,0.282513655994357,0.286631738476199,0.311154772354938,
0.335765994613648,0.360166888444423,0.370324933502905,0.375577979330509,
0.39932663886447,0.417608625696714,0.42311115157445,0.427811305959952,0.450556505121144,
0.47164802816755,0.474022601254833),.UNSPECIFIED.);
#2097=B_SPLINE_CURVE_WITH_KNOTS('',3,(#206577,#206578,#206579,#206580,#206581,
#206582,#206583,#206584,#206585,#206586,#206587,#206588,#206589,#206590,
#206591,#206592,#206593,#206594,#206595,#206596,#206597,#206598,#206599,
#206600,#206601,#206602,#206603,#206604,#206605,#206606,#206607,#206608,
#206609,#206610,#206611,#206612,#206613,#206614,#206615,#206616,#206617,
#206618,#206619,#206620,#206621,#206622,#206623,#206624,#206625,#206626,
#206627,#206628,#206629,#206630,#206631,#206632,#206633,#206634,#206635,
#206636,#206637,#206638,#206639,#206640,#206641,#206642,#206643,#206644,
#206645,#206646,#206647,#206648,#206649,#206650,#206651,#206652,#206653,
#206654,#206655,#206656,#206657,#206658,#206659,#206660,#206661,#206662,
#206663,#206664),.UNSPECIFIED.,.F.,.F.,(4,3,3,3,3,3,3,3,3,3,3,3,3,3,3,3,
3,3,3,3,3,3,3,3,3,3,3,3,3,4),(0.,0.0223800372151332,0.0455571433122737,
0.0675550536686484,0.0773342673604862,0.0821512524289193,0.0865889078224679,
0.110577875996286,0.135008164711438,0.157206738276085,0.165672856963219,
0.170323012283074,0.173915733667268,0.198992994974291,0.224022472738052,
0.248477225379953,0.258554635842646,0.264135020504929,0.288903381765905,
0.314991218209838,0.341079054653772,0.351267092682162,0.355315313446979,
0.381664716363141,0.403487580067799,0.410694485847216,0.41646327764549,
0.443066533245083,0.469275862304372,0.472065636984178),.UNSPECIFIED.);
#2098=B_SPLINE_CURVE_WITH_KNOTS('',3,(#206665,#206666,#206667,#206668,#206669,
#206670,#206671,#206672,#206673,#206674,#206675,#206676,#206677,#206678,
#206679,#206680,#206681,#206682,#206683,#206684,#206685,#206686,#206687,
#206688,#206689,#206690,#206691,#206692,#206693,#206694,#206695,#206696,
#206697,#206698,#206699,#206700,#206701,#206702,#206703,#206704,#206705,
#206706,#206707,#206708,#206709,#206710,#206711,#206712,#206713,#206714,
#206715,#206716,#206717,#206718,#206719,#206720,#206721,#206722,#206723,
#206724,#206725,#206726,#206727,#206728,#206729,#206730,#206731,#206732,
#206733,#206734,#206735,#206736,#206737,#206738,#206739,#206740,#206741,
#206742,#206743,#206744,#206745,#206746,#206747,#206748,#206749,#206750,
#206751,#206752),.UNSPECIFIED.,.F.,.F.,(4,3,3,3,3,3,3,3,3,3,3,3,3,3,3,3,
3,3,3,3,3,3,3,3,3,3,3,3,3,4),(0.,0.0260517968486712,0.0527225544316126,
0.0776790985121134,0.088972803707389,0.0959464341599202,0.100845925569268,
0.126855201703201,0.152534124099972,0.176212516457141,0.186122361672799,
0.192547951517572,0.196620308043645,0.221672220464654,0.246724132885662,
0.272050621021719,0.282513655344617,0.286631737801889,0.311154771378497,
0.335765992439757,0.360166881962943,0.370324927588301,0.375577975882316,
0.399326629362452,0.417608623757103,0.423111147264353,0.427811294162416,
0.450556481123398,0.471648028167544,0.474022601254839),.UNSPECIFIED.);
#2099=B_SPLINE_CURVE_WITH_KNOTS('',3,(#206753,#206754,#206755,#206756,#206757,
#206758,#206759,#206760,#206761,#206762,#206763,#206764,#206765,#206766,
#206767,#206768,#206769,#206770,#206771,#206772,#206773,#206774,#206775,
#206776,#206777,#206778,#206779,#206780,#206781,#206782,#206783,#206784,
#206785,#206786,#206787,#206788,#206789,#206790,#206791,#206792,#206793,
#206794,#206795,#206796,#206797,#206798,#206799,#206800,#206801,#206802,
#206803,#206804,#206805,#206806,#206807,#206808,#206809,#206810,#206811,
#206812,#206813,#206814,#206815,#206816,#206817,#206818,#206819,#206820,
#206821,#206822,#206823,#206824,#206825,#206826,#206827,#206828,#206829,
#206830,#206831,#206832,#206833,#206834,#206835,#206836,#206837,#206838,
#206839,#206840),.UNSPECIFIED.,.F.,.F.,(4,3,3,3,3,3,3,3,3,3,3,3,3,3,3,3,
3,3,3,3,3,3,3,3,3,3,3,3,3,4),(0.,0.0226012852117639,0.0452025704235279,
0.067555058212843,0.0773342716206684,0.0821512618789957,0.0865889109720383,
0.110761871811172,0.134934832650306,0.157206742672241,0.165672862519276,
0.17032303759631,0.173915776335193,0.198993037124029,0.224022472738049,
0.24847722404691,0.258554635931002,0.264135020402494,0.289777625640233,
0.315428339653183,0.341079053666132,0.351267091758101,0.355315312641973,
0.381664715351708,0.403487579124147,0.410694481959163,0.416463278906866,
0.443066534477174,0.469275862304408,0.472065636821688),.UNSPECIFIED.);
#2100=B_SPLINE_CURVE_WITH_KNOTS('',3,(#206841,#206842,#206843,#206844,#206845,
#206846,#206847,#206848,#206849,#206850,#206851,#206852,#206853,#206854,
#206855,#206856,#206857,#206858,#206859,#206860,#206861,#206862,#206863,
#206864,#206865,#206866,#206867,#206868,#206869,#206870,#206871,#206872,
#206873,#206874,#206875,#206876,#206877,#206878,#206879,#206880,#206881,
#206882,#206883,#206884,#206885,#206886,#206887,#206888,#206889,#206890,
#206891,#206892,#206893,#206894,#206895,#206896,#206897,#206898,#206899,
#206900,#206901,#206902,#206903,#206904,#206905,#206906,#206907,#206908,
#206909,#206910,#206911,#206912,#206913,#206914,#206915,#206916,#206917,
#206918,#206919,#206920,#206921,#206922,#206923,#206924,#206925,#206926,
#206927,#206928),.UNSPECIFIED.,.F.,.F.,(4,3,3,3,3,3,3,3,3,3,3,3,3,3,3,3,
3,3,3,3,3,3,3,3,3,3,3,3,3,4),(0.,0.0259306190073998,0.0526009583628542,
0.0776790988226147,0.0889728038113335,0.0959464341623167,0.100845925575729,
0.126856858203815,0.152713971416374,0.177949842661688,0.186122361669415,
0.192547951595364,0.196620308076219,0.221672220480934,0.24672413288565,
0.272050621046898,0.282513655340624,0.286631737980665,0.311197491830502,
0.335883934863211,0.360158613898702,0.3703249274938,0.375577975829039,0.399326629202051,
0.41760862372711,0.423111147116857,0.427811294064984,0.450556480771396,
0.471648028167486,0.47402260125479),.UNSPECIFIED.);
#2101=B_SPLINE_CURVE_WITH_KNOTS('',3,(#206929,#206930,#206931,#206932,#206933,
#206934,#206935,#206936,#206937,#206938,#206939,#206940,#206941,#206942,
#206943,#206944,#206945,#206946,#206947,#206948,#206949,#206950,#206951,
#206952,#206953,#206954,#206955,#206956,#206957,#206958,#206959,#206960,
#206961,#206962,#206963,#206964,#206965,#206966,#206967,#206968,#206969,
#206970,#206971,#206972,#206973,#206974,#206975,#206976,#206977,#206978,
#206979,#206980,#206981,#206982,#206983,#206984,#206985,#206986,#206987,
#206988,#206989,#206990,#206991,#206992,#206993,#206994,#206995,#206996,
#206997,#206998,#206999,#207000,#207001,#207002,#207003,#207004,#207005,
#207006,#207007,#207008,#207009,#207010,#207011,#207012,#207013,#207014,
#207015,#207016),.UNSPECIFIED.,.F.,.F.,(4,3,3,3,3,3,3,3,3,3,3,3,3,3,3,3,
3,3,3,3,3,3,3,3,3,3,3,3,3,4),(0.,0.0223800600970233,0.045557183874987,0.0675550913477831,
0.0773343026846742,0.0821513307715598,0.086588933128813,0.110761903794659,
0.134934874460505,0.159278641767771,0.165672902158484,0.170323218744956,
0.173916080012127,0.198993337115258,0.224022472738042,0.24852272682622,
0.25855463659488,0.264135020001501,0.288903366541005,0.314991206662608,
0.341079046784212,0.351267085078404,0.355315309150301,0.381664710560744,
0.403487574104964,0.411770819428486,0.416463283580499,0.443066538814214,
0.469275862304419,0.472065635637224),.UNSPECIFIED.);
#2102=B_SPLINE_CURVE_WITH_KNOTS('',3,(#207017,#207018,#207019,#207020,#207021,
#207022,#207023,#207024,#207025,#207026,#207027,#207028,#207029,#207030,
#207031,#207032,#207033,#207034,#207035,#207036,#207037,#207038,#207039,
#207040,#207041,#207042,#207043,#207044,#207045,#207046,#207047,#207048,
#207049,#207050,#207051,#207052,#207053,#207054,#207055,#207056,#207057,
#207058,#207059,#207060,#207061,#207062,#207063,#207064,#207065,#207066,
#207067,#207068,#207069,#207070,#207071,#207072,#207073,#207074,#207075,
#207076,#207077,#207078,#207079,#207080,#207081,#207082,#207083,#207084,
#207085,#207086,#207087,#207088,#207089,#207090,#207091,#207092,#207093,
#207094,#207095,#207096,#207097,#207098,#207099,#207100,#207101),
 .UNSPECIFIED.,.F.,.F.,(4,3,3,3,3,3,3,3,3,3,3,3,3,3,3,3,3,3,3,3,3,3,3,3,
3,3,3,3,4),(0.,0.0260517912929934,0.0527225478485455,0.0776790939050551,
0.0889728021702812,0.0959464342551659,0.100845925350706,0.126855201462976,
0.152534125917849,0.176212517636641,0.192547949849574,0.196620307478408,
0.221672220182029,0.24672413288565,0.272050620811562,0.282513655553444,
0.286631738154676,0.311154771782915,0.335765993229603,0.360166884129707,
0.370324929459797,0.375577976970675,0.399326632351765,0.417608624369275,
0.423111148621278,0.427811298126592,0.450556488913046,0.471648028167475,
0.474022601254778),.UNSPECIFIED.);
#2103=B_SPLINE_CURVE_WITH_KNOTS('',3,(#207318,#207319,#207320,#207321,#207322,
#207323,#207324,#207325,#207326,#207327,#207328,#207329,#207330,#207331,
#207332,#207333,#207334,#207335,#207336,#207337,#207338,#207339,#207340,
#207341,#207342,#207343,#207344,#207345,#207346,#207347,#207348,#207349,
#207350,#207351,#207352,#207353,#207354,#207355,#207356,#207357,#207358,
#207359,#207360,#207361,#207362,#207363,#207364,#207365,#207366,#207367,
#207368,#207369,#207370,#207371,#207372,#207373,#207374,#207375,#207376,
#207377,#207378,#207379,#207380,#207381,#207382,#207383,#207384,#207385,
#207386,#207387,#207388,#207389,#207390,#207391,#207392,#207393,#207394,
#207395,#207396,#207397,#207398,#207399,#207400,#207401,#207402,#207403,
#207404,#207405,#207406,#207407,#207408,#207409,#207410,#207411,#207412,
#207413,#207414,#207415,#207416,#207417,#207418,#207419,#207420),
 .UNSPECIFIED.,.F.,.F.,(4,3,3,3,3,3,3,3,3,3,3,3,3,3,3,3,3,3,3,3,3,3,3,3,
3,3,3,3,3,3,3,3,3,3,4),(-0.950777871811442,-0.906336425390168,-0.861875033114161,
-0.842434685731619,-0.832698894406312,-0.823679279165542,-0.779911530164976,
-0.736812975118332,-0.713111655774817,-0.707528734983928,-0.706840830508988,
-0.663970529007278,-0.62096019743997,-0.578452544080758,-0.53653757030824,
-0.528618153061017,-0.5197784899906,-0.479103795974014,-0.472085166836762,
-0.430141730544578,-0.388512020610736,-0.35295009564229,-0.345831806228506,
-0.34009678874744,-0.299353453374947,-0.258818746671375,-0.246812444972861,
-0.206136253916913,-0.172639040264036,-0.165053203014642,-0.125295016427036,
-0.0858747403733512,-0.046745972523297,-0.0311581910594031,0.),
 .UNSPECIFIED.);
#2104=B_SPLINE_CURVE_WITH_KNOTS('',3,(#207421,#207422,#207423,#207424,#207425,
#207426,#207427,#207428,#207429,#207430,#207431,#207432,#207433,#207434,
#207435,#207436,#207437,#207438,#207439,#207440,#207441,#207442,#207443,
#207444,#207445,#207446,#207447,#207448,#207449,#207450,#207451,#207452,
#207453,#207454,#207455,#207456,#207457,#207458,#207459,#207460,#207461,
#207462,#207463,#207464,#207465,#207466,#207467,#207468,#207469,#207470,
#207471,#207472,#207473,#207474,#207475,#207476,#207477,#207478,#207479,
#207480,#207481,#207482,#207483,#207484,#207485,#207486,#207487,#207488,
#207489,#207490,#207491,#207492,#207493,#207494,#207495,#207496,#207497,
#207498,#207499,#207500,#207501,#207502,#207503,#207504,#207505,#207506,
#207507,#207508,#207509,#207510,#207511,#207512,#207513,#207514,#207515,
#207516,#207517,#207518,#207519,#207520,#207521,#207522,#207523),
 .UNSPECIFIED.,.F.,.F.,(4,3,3,3,3,3,3,3,3,3,3,3,3,3,3,3,3,3,3,3,3,3,3,3,
3,3,3,3,3,3,3,3,3,3,4),(0.,0.0392937243200445,0.078648792419632,0.118430422481667,
0.157174897280178,0.16530965460934,0.172511921016207,0.214141585432509,
0.254364238175765,0.295024495344819,0.335842707328534,0.340554091141284,
0.347540360366197,0.389002662438937,0.430931272514703,0.437981494075935,
0.479749916301002,0.518812960683757,0.524399035743027,0.530138494511844,
0.57262664708442,0.615529815026447,0.658476413952203,0.671400602336179,
0.691337520740504,0.703515645442784,0.711692863532045,0.721145455934051,
0.764504689623414,0.808363873685668,0.829117588621419,0.836453781446258,
0.880985314545998,0.913941349417081,0.950775682567348),.UNSPECIFIED.);
#2105=B_SPLINE_CURVE_WITH_KNOTS('',3,(#207740,#207741,#207742,#207743,#207744,
#207745,#207746,#207747,#207748,#207749,#207750,#207751,#207752,#207753,
#207754,#207755,#207756,#207757,#207758,#207759,#207760,#207761,#207762,
#207763,#207764,#207765,#207766,#207767,#207768,#207769,#207770,#207771,
#207772,#207773,#207774,#207775,#207776,#207777,#207778,#207779,#207780,
#207781,#207782,#207783,#207784,#207785,#207786,#207787,#207788,#207789,
#207790,#207791,#207792,#207793,#207794,#207795,#207796,#207797,#207798,
#207799,#207800,#207801,#207802,#207803,#207804,#207805,#207806,#207807,
#207808,#207809,#207810,#207811,#207812,#207813,#207814,#207815,#207816,
#207817,#207818,#207819,#207820,#207821,#207822,#207823,#207824,#207825,
#207826,#207827,#207828,#207829,#207830,#207831,#207832,#207833,#207834,
#207835,#207836,#207837,#207838,#207839),.UNSPECIFIED.,.F.,.F.,(4,3,3,3,
3,3,3,3,3,3,3,3,3,3,3,3,3,3,3,3,3,3,3,3,3,3,3,3,3,3,3,3,3,4),(-0.954382097139067,
-0.915540356901139,-0.875987953878927,-0.858553371309591,-0.851652578164575,
-0.844316096216611,-0.803953485084637,-0.771951682750547,-0.755904221756574,
-0.746876223962411,-0.741004834362442,-0.7398567607626,-0.698120295630557,
-0.657232380143924,-0.615071640189176,-0.572910900234428,-0.567449445615807,
-0.525372539405531,-0.515246554457167,-0.473498151147513,-0.430271385468235,
-0.387044619788958,-0.380028835408339,-0.337077765616228,-0.293664876806399,
-0.280914982302858,-0.237661647632792,-0.200416680658377,-0.194604991995093,
-0.1507164440315,-0.10637737364008,-0.0619596473409019,-0.0369876293288037,
-2.19658856801564E-6),.UNSPECIFIED.);
#2106=B_SPLINE_CURVE_WITH_KNOTS('',3,(#207840,#207841,#207842,#207843,#207844,
#207845,#207846,#207847,#207848,#207849,#207850,#207851,#207852,#207853,
#207854,#207855,#207856,#207857,#207858,#207859,#207860,#207861,#207862,
#207863,#207864,#207865,#207866,#207867,#207868,#207869,#207870,#207871,
#207872,#207873,#207874,#207875,#207876,#207877,#207878,#207879,#207880,
#207881,#207882,#207883,#207884,#207885,#207886,#207887,#207888,#207889,
#207890,#207891,#207892,#207893,#207894,#207895,#207896,#207897,#207898,
#207899,#207900,#207901,#207902,#207903,#207904,#207905,#207906,#207907,
#207908,#207909,#207910,#207911,#207912,#207913,#207914,#207915,#207916,
#207917,#207918,#207919,#207920,#207921,#207922,#207923,#207924,#207925,
#207926,#207927,#207928,#207929,#207930,#207931,#207932,#207933,#207934,
#207935,#207936,#207937,#207938,#207939,#207940,#207941,#207942),
 .UNSPECIFIED.,.F.,.F.,(4,3,3,3,3,3,3,3,3,3,3,3,3,3,3,3,3,3,3,3,3,3,3,3,
3,3,3,3,3,3,3,3,3,3,4),(3.92004242434274E-15,0.0440097382289323,0.0884882554286592,
0.132783546573759,0.176334546416905,0.187993870420512,0.19423572748739,
0.19979115047153,0.245254179237364,0.288657155098451,0.331818541228064,
0.369239411527086,0.3808541168619,0.388821225436964,0.431108255685854,0.473065176320765,
0.481013297040258,0.52321857616724,0.558979311157592,0.56811322256641,0.573516263988367,
0.614763363362682,0.655642090775697,0.696286761208482,0.70713567464641,
0.734136415169824,0.744264975553648,0.750002339682418,0.790439331413119,
0.830523899192685,0.849662847172381,0.855799185905343,0.895145184350553,
0.923141598833727,0.954382097139069),.UNSPECIFIED.);
#2107=B_SPLINE_CURVE_WITH_KNOTS('',3,(#208159,#208160,#208161,#208162,#208163,
#208164,#208165,#208166,#208167,#208168,#208169,#208170,#208171,#208172,
#208173,#208174,#208175,#208176,#208177,#208178,#208179,#208180,#208181,
#208182,#208183,#208184,#208185,#208186,#208187,#208188,#208189,#208190,
#208191,#208192,#208193,#208194,#208195,#208196,#208197,#208198,#208199,
#208200,#208201,#208202,#208203,#208204,#208205,#208206,#208207,#208208,
#208209,#208210,#208211,#208212,#208213,#208214,#208215,#208216,#208217,
#208218,#208219,#208220,#208221,#208222,#208223,#208224,#208225,#208226,
#208227,#208228,#208229,#208230,#208231,#208232,#208233,#208234,#208235,
#208236,#208237,#208238,#208239,#208240,#208241,#208242,#208243,#208244,
#208245,#208246,#208247,#208248,#208249,#208250,#208251,#208252,#208253,
#208254,#208255,#208256,#208257,#208258,#208259,#208260,#208261,#208262,
#208263,#208264),.UNSPECIFIED.,.F.,.F.,(4,3,3,3,3,3,3,3,3,3,3,3,3,3,3,3,
3,3,3,3,3,3,3,3,3,3,3,3,3,3,3,3,3,3,3,4),(-0.950777871811489,-0.90633643654385,
-0.861875036957276,-0.842434689817133,-0.831093639563838,-0.825301574638444,
-0.781525133147754,-0.738411526679356,-0.713111654821142,-0.707528734408151,
-0.70684083050903,-0.664137304886556,-0.621129293398492,-0.578512193972095,
-0.5364863625863,-0.527113744824773,-0.519453631915209,-0.479103798452372,
-0.472085166836776,-0.430141731436706,-0.38851202234129,-0.352950096664573,
-0.345831809185344,-0.340096789032849,-0.299287338987686,-0.258818748565295,
-0.246812444972867,-0.206034245191185,-0.184174738424713,-0.172639040068934,
-0.164351647577379,-0.124589561132121,-0.0849805995846697,-0.0460567214433639,
-0.0311581910594067,0.),.UNSPECIFIED.);
#2108=B_SPLINE_CURVE_WITH_KNOTS('',3,(#208265,#208266,#208267,#208268,#208269,
#208270,#208271,#208272,#208273,#208274,#208275,#208276,#208277,#208278,
#208279,#208280,#208281,#208282,#208283,#208284,#208285,#208286,#208287,
#208288,#208289,#208290,#208291,#208292,#208293,#208294,#208295,#208296,
#208297,#208298,#208299,#208300,#208301,#208302,#208303,#208304,#208305,
#208306,#208307,#208308,#208309,#208310,#208311,#208312,#208313,#208314,
#208315,#208316,#208317,#208318,#208319,#208320,#208321,#208322,#208323,
#208324,#208325,#208326,#208327,#208328,#208329,#208330,#208331,#208332,
#208333,#208334,#208335,#208336,#208337,#208338,#208339,#208340,#208341,
#208342,#208343,#208344,#208345,#208346,#208347,#208348,#208349,#208350,
#208351,#208352,#208353,#208354,#208355,#208356,#208357,#208358,#208359,
#208360,#208361,#208362,#208363,#208364,#208365,#208366,#208367),
 .UNSPECIFIED.,.F.,.F.,(4,3,3,3,3,3,3,3,3,3,3,3,3,3,3,3,3,3,3,3,3,3,3,3,
3,3,3,3,3,3,3,3,3,3,4),(2.82530270380345E-15,0.0383561142044138,0.0777322538410477,
0.117448352720408,0.157136327541592,0.16530959676955,0.172511917896846,
0.214141585432506,0.254319391003502,0.295111323821341,0.330724243378432,
0.341693770779204,0.348846513511567,0.39059233282008,0.430931232999916,
0.437981494075929,0.479749911159561,0.518812944385605,0.524709771531363,
0.530138484534004,0.572570423222229,0.615574325975759,0.658476390767529,
0.671400602336174,0.701718195721287,0.711077059751642,0.717874112270349,
0.761139330498572,0.804963166413058,0.816774798744654,0.829117599322156,
0.836453798394249,0.880985331409096,0.913941349417075,0.950775682377203),
 .UNSPECIFIED.);
#2109=B_SPLINE_CURVE_WITH_KNOTS('',3,(#208584,#208585,#208586,#208587,#208588,
#208589,#208590,#208591,#208592,#208593,#208594,#208595,#208596,#208597,
#208598,#208599,#208600,#208601,#208602,#208603,#208604,#208605,#208606,
#208607,#208608,#208609,#208610,#208611,#208612,#208613,#208614,#208615,
#208616,#208617,#208618,#208619,#208620,#208621,#208622,#208623,#208624,
#208625,#208626,#208627,#208628,#208629,#208630,#208631,#208632,#208633,
#208634,#208635,#208636,#208637,#208638,#208639,#208640,#208641,#208642,
#208643,#208644,#208645,#208646,#208647,#208648,#208649,#208650,#208651,
#208652,#208653,#208654,#208655,#208656,#208657,#208658,#208659,#208660,
#208661,#208662,#208663,#208664,#208665,#208666,#208667,#208668,#208669,
#208670,#208671,#208672,#208673,#208674,#208675,#208676,#208677,#208678,
#208679,#208680,#208681,#208682,#208683,#208684,#208685,#208686,#208687,
#208688,#208689),.UNSPECIFIED.,.F.,.F.,(4,3,3,3,3,3,3,3,3,3,3,3,3,3,3,3,
3,3,3,3,3,3,3,3,3,3,3,3,3,3,3,3,3,3,3,4),(-0.954382097139027,-0.915540393312965,
-0.875988011049171,-0.858553452015747,-0.851651720979109,-0.84431594622701,
-0.803953347308934,-0.771951616163724,-0.755904188463154,-0.746876173424658,
-0.741004793318458,-0.739856760762583,-0.698120275698938,-0.657232336987918,
-0.615071578747959,-0.572910820508001,-0.567449396059044,-0.525372472030206,
-0.515246554457162,-0.473526932909523,-0.431236741001746,-0.393744912161324,
-0.387044679913831,-0.381221890286597,-0.338027165363515,-0.294874550582207,
-0.28091498230286,-0.237709647788549,-0.212648675820495,-0.200416680015836,
-0.194604990965853,-0.150716441724806,-0.106377371171992,-0.0619596447480801,
-0.0369876293288071,-2.1968306284113E-6),.UNSPECIFIED.);
#2110=B_SPLINE_CURVE_WITH_KNOTS('',3,(#208690,#208691,#208692,#208693,#208694,
#208695,#208696,#208697,#208698,#208699,#208700,#208701,#208702,#208703,
#208704,#208705,#208706,#208707,#208708,#208709,#208710,#208711,#208712,
#208713,#208714,#208715,#208716,#208717,#208718,#208719,#208720,#208721,
#208722,#208723,#208724,#208725,#208726,#208727,#208728,#208729,#208730,
#208731,#208732,#208733,#208734,#208735,#208736,#208737,#208738,#208739,
#208740,#208741,#208742,#208743,#208744,#208745,#208746,#208747,#208748,
#208749,#208750,#208751,#208752,#208753,#208754,#208755,#208756,#208757,
#208758,#208759,#208760,#208761,#208762,#208763,#208764,#208765,#208766,
#208767,#208768,#208769,#208770,#208771,#208772,#208773,#208774,#208775,
#208776,#208777,#208778,#208779,#208780,#208781,#208782,#208783,#208784,
#208785,#208786,#208787,#208788,#208789,#208790,#208791,#208792,#208793,
#208794,#208795),.UNSPECIFIED.,.F.,.F.,(4,3,3,3,3,3,3,3,3,3,3,3,3,3,3,3,
3,3,3,3,3,3,3,3,3,3,3,3,3,3,3,3,3,3,3,4),(0.,0.0440097102619271,0.0884882277684458,
0.132783533024059,0.176334557243343,0.187993903233133,0.194235848510683,
0.199791297605252,0.245254179237363,0.288657161367001,0.331818543103485,
0.369239414789171,0.380854128970053,0.388821223648941,0.431034523258865,
0.473065169701532,0.481013297040253,0.523218575748239,0.558979309133477,
0.568113222474232,0.57351626392526,0.614765000689446,0.655861440299277,
0.696286756072865,0.707135674646407,0.734136415169823,0.74426497460981,
0.752455611749943,0.792892563063861,0.833036427815749,0.838982768060298,
0.849662831772539,0.855799161052988,0.89514516223825,0.923141598833728,
0.954382097139071),.UNSPECIFIED.);
#2111=B_SPLINE_CURVE_WITH_KNOTS('',3,(#209508,#209509,#209510,#209511,#209512,
#209513,#209514,#209515,#209516,#209517,#209518,#209519,#209520,#209521,
#209522,#209523,#209524,#209525,#209526,#209527,#209528,#209529,#209530,
#209531,#209532,#209533,#209534,#209535,#209536,#209537,#209538,#209539,
#209540,#209541,#209542,#209543,#209544,#209545,#209546,#209547,#209548,
#209549,#209550,#209551,#209552,#209553,#209554,#209555,#209556,#209557,
#209558,#209559,#209560,#209561,#209562,#209563,#209564,#209565,#209566,
#209567,#209568,#209569,#209570,#209571,#209572,#209573,#209574,#209575,
#209576,#209577,#209578,#209579,#209580,#209581,#209582,#209583,#209584,
#209585,#209586,#209587,#209588,#209589,#209590,#209591,#209592,#209593,
#209594,#209595),.UNSPECIFIED.,.F.,.F.,(4,3,3,3,3,3,3,3,3,3,3,3,3,3,3,3,
3,3,3,3,3,3,3,3,3,3,3,3,3,4),(0.,0.0223800415826111,0.0455571510723243,
0.0675550609170155,0.0773342741558292,0.0821512675008773,0.0865889126878389,
0.11057788386222,0.135008172941507,0.157206745152612,0.16567286565653,0.170323051943897,
0.173915800266865,0.198993060769186,0.224022472738035,0.248477223249604,
0.258554635986008,0.264135020444879,0.28890337893006,0.314991216050641,
0.341079053171223,0.351267091230857,0.355315312478378,0.381664715071331,
0.403487578818942,0.410694480570935,0.416463278950785,0.443066534470941,
0.469275862304353,0.472065636725432),.UNSPECIFIED.);
#2112=B_SPLINE_CURVE_WITH_KNOTS('',3,(#210308,#210309,#210310,#210311,#210312,
#210313,#210314,#210315,#210316,#210317,#210318,#210319,#210320,#210321,
#210322,#210323,#210324,#210325,#210326,#210327,#210328,#210329,#210330,
#210331,#210332,#210333,#210334,#210335,#210336,#210337,#210338,#210339,
#210340,#210341,#210342,#210343,#210344,#210345,#210346,#210347,#210348,
#210349,#210350,#210351,#210352,#210353,#210354,#210355,#210356,#210357,
#210358,#210359,#210360,#210361,#210362,#210363,#210364,#210365,#210366,
#210367,#210368,#210369,#210370,#210371,#210372,#210373,#210374,#210375,
#210376,#210377,#210378,#210379,#210380,#210381,#210382,#210383,#210384,
#210385,#210386,#210387,#210388,#210389,#210390,#210391,#210392,#210393,
#210394,#210395,#210396,#210397,#210398),.UNSPECIFIED.,.F.,.F.,(4,3,3,3,
3,3,3,3,3,3,3,3,3,3,3,3,3,3,3,3,3,3,3,3,3,3,3,3,3,3,4),(7.90123170449159E-15,
0.0260517808136012,0.0527225352991877,0.0776790852361114,0.0889727992741923,
0.0959464344241781,0.100845925040092,0.126855201361835,0.152534129667343,
0.17621251994363,0.186122361828502,0.19254794682658,0.196620306433238,0.221672219659448,
0.246724132885659,0.272058447969215,0.280886246322291,0.285802388610614,
0.299566540114185,0.311229550951507,0.33591592242145,0.360190200940758,
0.370324932919906,0.375577978970566,0.399326637919175,0.417608625494232,
0.423111151172439,0.427811304835429,0.450556502779002,0.471648028167516,
0.474022601254811),.UNSPECIFIED.);
#2113=B_SPLINE_CURVE_WITH_KNOTS('',3,(#211111,#211112,#211113,#211114,#211115,
#211116,#211117,#211118,#211119,#211120,#211121,#211122,#211123,#211124,
#211125,#211126,#211127,#211128,#211129,#211130,#211131,#211132,#211133,
#211134,#211135,#211136,#211137,#211138,#211139,#211140,#211141,#211142,
#211143,#211144,#211145,#211146,#211147,#211148,#211149,#211150,#211151,
#211152,#211153,#211154,#211155,#211156,#211157,#211158,#211159,#211160,
#211161,#211162,#211163,#211164,#211165,#211166,#211167,#211168,#211169,
#211170,#211171,#211172,#211173,#211174,#211175,#211176,#211177,#211178,
#211179,#211180,#211181,#211182,#211183,#211184,#211185,#211186,#211187,
#211188,#211189,#211190,#211191,#211192,#211193,#211194,#211195,#211196,
#211197,#211198),.UNSPECIFIED.,.F.,.F.,(4,3,3,3,3,3,3,3,3,3,3,3,3,3,3,3,
3,3,3,3,3,3,3,3,3,3,3,3,3,4),(0.,0.022380064656475,0.0455571919885892,0.0675550989125488,
0.077334309776642,0.0821513465008637,0.0865889382889745,0.110577925353253,
0.135008216273016,0.157206781258753,0.165672911295151,0.170323260534971,
0.173916149941423,0.198993406189961,0.22402247273804,0.248477212094458,
0.258554636746328,0.26413501995488,0.288903363466092,0.314991204360096,
0.341079045254099,0.351267083567837,0.355315308310309,0.381664709440852,
0.403487572943969,0.410694455370546,0.416463284762423,0.443066539898884,
0.469275862304369,0.472065635365967),.UNSPECIFIED.);
#2114=B_SPLINE_CURVE_WITH_KNOTS('',3,(#211911,#211912,#211913,#211914,#211915,
#211916,#211917,#211918,#211919,#211920,#211921,#211922,#211923,#211924,
#211925,#211926,#211927,#211928,#211929,#211930,#211931,#211932,#211933,
#211934,#211935,#211936,#211937,#211938,#211939,#211940,#211941,#211942,
#211943,#211944,#211945,#211946,#211947,#211948,#211949,#211950,#211951,
#211952,#211953,#211954,#211955,#211956,#211957,#211958,#211959,#211960,
#211961,#211962,#211963,#211964,#211965,#211966,#211967,#211968,#211969,
#211970,#211971,#211972,#211973,#211974,#211975,#211976,#211977,#211978,
#211979,#211980,#211981,#211982,#211983,#211984,#211985,#211986,#211987,
#211988,#211989,#211990,#211991,#211992,#211993,#211994,#211995,#211996,
#211997,#211998),.UNSPECIFIED.,.F.,.F.,(4,3,3,3,3,3,3,3,3,3,3,3,3,3,3,3,
3,3,3,3,3,3,3,3,3,3,3,3,3,4),(0.,0.026051775604345,0.0527225290853877,0.0776790809548157,
0.0889727978441528,0.0959464345074647,0.10084592486155,0.126855201263961,
0.152534131465872,0.176212521061365,0.186122361876941,0.192547945329784,
0.196620305916515,0.221672219401092,0.246724132885669,0.27206158277579,
0.282513656118586,0.286631738568381,0.311197492372781,0.335883935062334,
0.360158620947264,0.370324934628168,0.375577979963716,0.399595492014671,
0.417608626052888,0.423111152459427,0.427811308268704,0.45055650974011,
0.471648028167537,0.474022601254832),.UNSPECIFIED.);
#2115=B_SPLINE_CURVE_WITH_KNOTS('',3,(#212711,#212712,#212713,#212714,#212715,
#212716,#212717,#212718,#212719,#212720,#212721,#212722,#212723,#212724,
#212725,#212726,#212727,#212728,#212729,#212730,#212731,#212732,#212733,
#212734,#212735,#212736,#212737,#212738,#212739,#212740,#212741,#212742,
#212743,#212744,#212745,#212746,#212747,#212748,#212749,#212750,#212751,
#212752,#212753,#212754,#212755,#212756,#212757,#212758,#212759,#212760,
#212761,#212762,#212763,#212764,#212765,#212766,#212767,#212768,#212769,
#212770,#212771,#212772,#212773,#212774,#212775,#212776,#212777,#212778,
#212779,#212780,#212781,#212782,#212783,#212784,#212785,#212786,#212787,
#212788,#212789,#212790,#212791,#212792,#212793,#212794,#212795,#212796,
#212797,#212798),.UNSPECIFIED.,.F.,.F.,(4,3,3,3,3,3,3,3,3,3,3,3,3,3,3,3,
3,3,3,3,3,3,3,3,3,3,3,3,3,4),(0.,0.0223800651370331,0.0455571928568673,
0.0675550997304994,0.0773343105434705,0.0833848318194916,0.0865889388358174,
0.110577926266239,0.135008217226555,0.157206782032257,0.165672912272975,
0.170323265017005,0.173916157466764,0.198993413622444,0.224022472738036,
0.248477211854248,0.258554636762497,0.264135019948427,0.28898134258909,
0.314338830544068,0.340111642432823,0.351267083403808,0.355315308234309,
0.381664709331105,0.403487572828058,0.410694454865743,0.416463284884501,
0.443066539997533,0.469275862304369,0.472065635336616),.UNSPECIFIED.);
#2116=B_SPLINE_CURVE_WITH_KNOTS('',3,(#213511,#213512,#213513,#213514,#213515,
#213516,#213517,#213518,#213519,#213520,#213521,#213522,#213523,#213524,
#213525,#213526,#213527,#213528,#213529,#213530,#213531,#213532,#213533,
#213534,#213535,#213536,#213537,#213538,#213539,#213540,#213541,#213542,
#213543,#213544,#213545,#213546,#213547,#213548,#213549,#213550,#213551,
#213552,#213553,#213554,#213555,#213556,#213557,#213558,#213559,#213560,
#213561,#213562,#213563,#213564,#213565,#213566,#213567,#213568,#213569,
#213570,#213571,#213572,#213573,#213574,#213575,#213576,#213577,#213578,
#213579,#213580,#213581,#213582,#213583,#213584,#213585,#213586,#213587,
#213588,#213589,#213590,#213591,#213592,#213593,#213594,#213595,#213596,
#213597,#213598),.UNSPECIFIED.,.F.,.F.,(4,3,3,3,3,3,3,3,3,3,3,3,3,3,3,3,
3,3,3,3,3,3,3,3,3,3,3,3,3,4),(0.,0.0261324658014236,0.0526962913261088,
0.0793415357281651,0.0889727984346616,0.095835043250178,0.10084592493607,
0.126856858695135,0.152713978120786,0.17794985603476,0.186122361857045,
0.192547945950156,0.196620306130287,0.221672219507975,0.246724132885664,
0.272050620322494,0.282513656041832,0.286631738502527,0.311258832154326,
0.335885925806125,0.360166888882926,0.37032493392055,0.375577979558784,
0.399326639542124,0.417608625825101,0.423111151926387,0.42781130682219,
0.45055650683662,0.47164802816751,0.474022601254803),.UNSPECIFIED.);
#2117=B_SPLINE_CURVE_WITH_KNOTS('',3,(#214311,#214312,#214313,#214314,#214315,
#214316,#214317,#214318,#214319,#214320,#214321,#214322,#214323,#214324,
#214325,#214326,#214327,#214328,#214329,#214330,#214331,#214332,#214333,
#214334,#214335,#214336,#214337,#214338,#214339,#214340,#214341,#214342,
#214343,#214344,#214345,#214346,#214347,#214348,#214349,#214350,#214351,
#214352,#214353,#214354,#214355,#214356,#214357,#214358,#214359,#214360,
#214361,#214362,#214363,#214364,#214365,#214366,#214367,#214368,#214369,
#214370,#214371,#214372,#214373,#214374,#214375,#214376,#214377,#214378,
#214379,#214380,#214381,#214382,#214383,#214384,#214385,#214386,#214387,
#214388,#214389,#214390,#214391,#214392,#214393,#214394,#214395),
 .UNSPECIFIED.,.F.,.F.,(4,3,3,3,3,3,3,3,3,3,3,3,3,3,3,3,3,3,3,3,3,3,3,3,
3,3,3,3,4),(0.,0.0222914007901619,0.0454674359825707,0.0675550870544155,
0.0821513218453204,0.0865889302954898,0.110629677084235,0.134994651844209,
0.159338030720047,0.165672897048461,0.170323195429502,0.173916040779313,
0.19899329834446,0.224022472738044,0.248477215576034,0.258554636508914,
0.264135020109551,0.288903368301885,0.314991208014035,0.341079047726185,
0.351267085960766,0.355315309607254,0.381664711215564,0.4034875747766,0.410694463232085,
0.416463282945419,0.443066538202943,0.469275862304378,0.472065635791059),
 .UNSPECIFIED.);
#2118=B_SPLINE_CURVE_WITH_KNOTS('',3,(#215108,#215109,#215110,#215111,#215112,
#215113,#215114,#215115,#215116,#215117,#215118,#215119,#215120,#215121,
#215122,#215123,#215124,#215125,#215126,#215127,#215128,#215129,#215130,
#215131,#215132,#215133,#215134,#215135,#215136,#215137,#215138,#215139,
#215140,#215141,#215142,#215143,#215144,#215145,#215146,#215147,#215148,
#215149,#215150,#215151,#215152,#215153,#215154,#215155,#215156,#215157,
#215158,#215159,#215160,#215161,#215162,#215163,#215164,#215165,#215166,
#215167,#215168,#215169,#215170,#215171,#215172,#215173,#215174,#215175,
#215176,#215177,#215178,#215179,#215180,#215181,#215182,#215183,#215184,
#215185,#215186,#215187,#215188,#215189,#215190,#215191,#215192,#215193,
#215194,#215195),.UNSPECIFIED.,.F.,.F.,(4,3,3,3,3,3,3,3,3,3,3,3,3,3,3,3,
3,3,3,3,3,3,3,3,3,3,3,3,3,4),(7.97682625883415E-15,0.0260517932991795,0.0527225502147213,
0.077679095575174,0.0889728027275484,0.0959464342222353,0.10084592545247,
0.126855201609306,0.152534125302762,0.176212517229938,0.186122361708183,
0.19254795046146,0.196620307684512,0.221672220285089,0.246724132885667,
0.272050620894862,0.282513655479386,0.286631738114849,0.31115477174714,
0.335765993047061,0.360166883426141,0.370324928797177,0.375577976589965,
0.399326631291424,0.417608624155145,0.423111148097321,0.427811296634432,
0.450556486039326,0.47164802816752,0.474022601254815),.UNSPECIFIED.);
#2119=SHAPE_REPRESENTATION_RELATIONSHIP('SRR','None',#215644,#2128);
#2120=SHAPE_REPRESENTATION_RELATIONSHIP('SRR','None',#215645,#2129);
#2121=SHAPE_REPRESENTATION_RELATIONSHIP('SRR','None',#215646,#2130);
#2122=SHAPE_REPRESENTATION_RELATIONSHIP('SRR','None',#215648,#2131);
#2123=SHAPE_REPRESENTATION_RELATIONSHIP('SRR','None',#215649,#2132);
#2124=SHAPE_REPRESENTATION_RELATIONSHIP('SRR','None',#215647,#2133);
#2125=SHAPE_REPRESENTATION_RELATIONSHIP('SRR','None',#215650,#2134);
#2126=SHAPE_REPRESENTATION_RELATIONSHIP('SRR','None',#215651,#2135);
#2127=SHAPE_REPRESENTATION_RELATIONSHIP('SRR','None',#215652,#2136);
#2128=ADVANCED_BREP_SHAPE_REPRESENTATION('',(#2146),#215600);
#2129=ADVANCED_BREP_SHAPE_REPRESENTATION('',(#2147),#215601);
#2130=ADVANCED_BREP_SHAPE_REPRESENTATION('',(#2148),#215602);
#2131=ADVANCED_BREP_SHAPE_REPRESENTATION('',(#2149),#215604);
#2132=ADVANCED_BREP_SHAPE_REPRESENTATION('',(#2150),#215605);
#2133=ADVANCED_BREP_SHAPE_REPRESENTATION('',(#2151),#215603);
#2134=ADVANCED_BREP_SHAPE_REPRESENTATION('',(#2152),#215606);
#2135=ADVANCED_BREP_SHAPE_REPRESENTATION('',(#2153),#215607);
#2136=ADVANCED_BREP_SHAPE_REPRESENTATION('',(#2154),#215608);
#2137=STYLED_ITEM('',(#215698),#2146);
#2138=STYLED_ITEM('',(#215698),#2147);
#2139=STYLED_ITEM('',(#215698),#2148);
#2140=STYLED_ITEM('',(#215698),#2149);
#2141=STYLED_ITEM('',(#215698),#2150);
#2142=STYLED_ITEM('',(#215698),#2151);
#2143=STYLED_ITEM('',(#215698),#2152);
#2144=STYLED_ITEM('',(#215698),#2153);
#2145=STYLED_ITEM('',(#215698),#2154);
#2146=MANIFOLD_SOLID_BREP('Body1',#28080);
#2147=MANIFOLD_SOLID_BREP('Body1',#28081);
#2148=MANIFOLD_SOLID_BREP('Body1',#28082);
#2149=MANIFOLD_SOLID_BREP('Body1',#28083);
#2150=MANIFOLD_SOLID_BREP('Body1',#28084);
#2151=MANIFOLD_SOLID_BREP('Body1',#28085);
#2152=MANIFOLD_SOLID_BREP('Body1',#28086);
#2153=MANIFOLD_SOLID_BREP('Body1',#28087);
#2154=MANIFOLD_SOLID_BREP('Body1',#28088);
#2155=CYLINDRICAL_SURFACE('',#28193,0.127);
#2156=CYLINDRICAL_SURFACE('',#28196,0.202999999999999);
#2157=CYLINDRICAL_SURFACE('',#28199,0.127000000000001);
#2158=CYLINDRICAL_SURFACE('',#28202,0.159000000000001);
#2159=CYLINDRICAL_SURFACE('',#28205,0.203000000000001);
#2160=CYLINDRICAL_SURFACE('',#28209,0.203);
#2161=CYLINDRICAL_SURFACE('',#28212,0.159000000000001);
#2162=CYLINDRICAL_SURFACE('',#28215,0.127000000000001);
#2163=CYLINDRICAL_SURFACE('',#28218,0.203);
#2164=CYLINDRICAL_SURFACE('',#28221,0.126999999999999);
#2165=CYLINDRICAL_SURFACE('',#28237,0.203000000000002);
#2166=CYLINDRICAL_SURFACE('',#28240,0.203000000000002);
#2167=CYLINDRICAL_SURFACE('',#28243,0.159);
#2168=CYLINDRICAL_SURFACE('',#28251,0.381);
#2169=CYLINDRICAL_SURFACE('',#28254,2.54);
#2170=CYLINDRICAL_SURFACE('',#28257,2.54);
#2171=CYLINDRICAL_SURFACE('',#28260,0.381);
#2172=CYLINDRICAL_SURFACE('',#28268,0.159);
#2173=CYLINDRICAL_SURFACE('',#28273,5.099);
#2174=CYLINDRICAL_SURFACE('',#28275,5.099);
#2175=CYLINDRICAL_SURFACE('',#28276,5.099);
#2176=CYLINDRICAL_SURFACE('',#28277,5.099);
#2177=CYLINDRICAL_SURFACE('',#28279,5.099);
#2178=CYLINDRICAL_SURFACE('',#28281,5.099);
#2179=CYLINDRICAL_SURFACE('',#28282,5.099);
#2180=CYLINDRICAL_SURFACE('',#28283,5.099);
#2181=CYLINDRICAL_SURFACE('',#28285,2.55999999999999);
#2182=CYLINDRICAL_SURFACE('',#28287,2.55999999999999);
#2183=CYLINDRICAL_SURFACE('',#28288,2.55999999999999);
#2184=CYLINDRICAL_SURFACE('',#28289,2.55999999999999);
#2185=CYLINDRICAL_SURFACE('',#28290,2.55999999999999);
#2186=CYLINDRICAL_SURFACE('',#28291,2.55999999999999);
#2187=CYLINDRICAL_SURFACE('',#28292,2.55999999999999);
#2188=CYLINDRICAL_SURFACE('',#28293,2.55999999999999);
#2189=CYLINDRICAL_SURFACE('',#28294,2.55999999999999);
#2190=CYLINDRICAL_SURFACE('',#28295,2.55999999999999);
#2191=CYLINDRICAL_SURFACE('',#28296,2.55999999999999);
#2192=CYLINDRICAL_SURFACE('',#28297,2.55999999999999);
#2193=CYLINDRICAL_SURFACE('',#28298,2.55999999999999);
#2194=CYLINDRICAL_SURFACE('',#28299,2.55999999999999);
#2195=CYLINDRICAL_SURFACE('',#28300,2.55999999999999);
#2196=CYLINDRICAL_SURFACE('',#28301,2.55999999999999);
#2197=CYLINDRICAL_SURFACE('',#28302,2.55999999999999);
#2198=CYLINDRICAL_SURFACE('',#28303,2.55999999999999);
#2199=CYLINDRICAL_SURFACE('',#28304,2.55999999999999);
#2200=CYLINDRICAL_SURFACE('',#28305,2.55999999999999);
#2201=CYLINDRICAL_SURFACE('',#28306,2.55999999999999);
#2202=CYLINDRICAL_SURFACE('',#28307,2.55999999999999);
#2203=CYLINDRICAL_SURFACE('',#28308,2.55999999999999);
#2204=CYLINDRICAL_SURFACE('',#28309,2.55999999999999);
#2205=CYLINDRICAL_SURFACE('',#28310,2.55999999999999);
#2206=CYLINDRICAL_SURFACE('',#28311,2.55999999999999);
#2207=CYLINDRICAL_SURFACE('',#28312,2.55999999999999);
#2208=CYLINDRICAL_SURFACE('',#28314,2.56);
#2209=CYLINDRICAL_SURFACE('',#28316,2.56);
#2210=CYLINDRICAL_SURFACE('',#28317,2.56);
#2211=CYLINDRICAL_SURFACE('',#28318,2.56);
#2212=CYLINDRICAL_SURFACE('',#28319,2.56);
#2213=CYLINDRICAL_SURFACE('',#28320,2.56);
#2214=CYLINDRICAL_SURFACE('',#28321,2.56);
#2215=CYLINDRICAL_SURFACE('',#28322,2.56);
#2216=CYLINDRICAL_SURFACE('',#28323,2.56);
#2217=CYLINDRICAL_SURFACE('',#28324,2.56);
#2218=CYLINDRICAL_SURFACE('',#28325,2.56);
#2219=CYLINDRICAL_SURFACE('',#28326,2.56);
#2220=CYLINDRICAL_SURFACE('',#28327,2.56);
#2221=CYLINDRICAL_SURFACE('',#28328,2.56);
#2222=CYLINDRICAL_SURFACE('',#28329,2.56);
#2223=CYLINDRICAL_SURFACE('',#28330,2.56);
#2224=CYLINDRICAL_SURFACE('',#28331,2.56);
#2225=CYLINDRICAL_SURFACE('',#28332,2.56);
#2226=CYLINDRICAL_SURFACE('',#28333,2.56);
#2227=CYLINDRICAL_SURFACE('',#28334,2.56);
#2228=CYLINDRICAL_SURFACE('',#28335,2.56);
#2229=CYLINDRICAL_SURFACE('',#28336,2.56);
#2230=CYLINDRICAL_SURFACE('',#28337,2.56);
#2231=CYLINDRICAL_SURFACE('',#28338,2.56);
#2232=CYLINDRICAL_SURFACE('',#28339,2.56);
#2233=CYLINDRICAL_SURFACE('',#28340,2.56);
#2234=CYLINDRICAL_SURFACE('',#28341,2.56);
#2235=CYLINDRICAL_SURFACE('',#28343,2.56);
#2236=CYLINDRICAL_SURFACE('',#28345,2.56);
#2237=CYLINDRICAL_SURFACE('',#28346,2.56);
#2238=CYLINDRICAL_SURFACE('',#28347,2.56);
#2239=CYLINDRICAL_SURFACE('',#28348,2.56);
#2240=CYLINDRICAL_SURFACE('',#28349,2.56);
#2241=CYLINDRICAL_SURFACE('',#28350,2.56);
#2242=CYLINDRICAL_SURFACE('',#28351,2.56);
#2243=CYLINDRICAL_SURFACE('',#28352,2.56);
#2244=CYLINDRICAL_SURFACE('',#28353,2.56);
#2245=CYLINDRICAL_SURFACE('',#28354,2.56);
#2246=CYLINDRICAL_SURFACE('',#28355,2.56);
#2247=CYLINDRICAL_SURFACE('',#28356,2.56);
#2248=CYLINDRICAL_SURFACE('',#28357,2.56);
#2249=CYLINDRICAL_SURFACE('',#28358,2.56);
#2250=CYLINDRICAL_SURFACE('',#28359,2.56);
#2251=CYLINDRICAL_SURFACE('',#28360,2.56);
#2252=CYLINDRICAL_SURFACE('',#28361,2.56);
#2253=CYLINDRICAL_SURFACE('',#28362,2.56);
#2254=CYLINDRICAL_SURFACE('',#28363,2.56);
#2255=CYLINDRICAL_SURFACE('',#28364,2.56);
#2256=CYLINDRICAL_SURFACE('',#28365,2.56);
#2257=CYLINDRICAL_SURFACE('',#28366,2.56);
#2258=CYLINDRICAL_SURFACE('',#28367,2.56);
#2259=CYLINDRICAL_SURFACE('',#28368,2.56);
#2260=CYLINDRICAL_SURFACE('',#28369,2.56);
#2261=CYLINDRICAL_SURFACE('',#28370,2.56);
#2262=CYLINDRICAL_SURFACE('',#28372,2.56);
#2263=CYLINDRICAL_SURFACE('',#28374,2.56);
#2264=CYLINDRICAL_SURFACE('',#28375,2.56);
#2265=CYLINDRICAL_SURFACE('',#28376,2.56);
#2266=CYLINDRICAL_SURFACE('',#28377,2.56);
#2267=CYLINDRICAL_SURFACE('',#28378,2.56);
#2268=CYLINDRICAL_SURFACE('',#28379,2.56);
#2269=CYLINDRICAL_SURFACE('',#28380,2.56);
#2270=CYLINDRICAL_SURFACE('',#28381,2.56);
#2271=CYLINDRICAL_SURFACE('',#28382,2.56);
#2272=CYLINDRICAL_SURFACE('',#28383,2.56);
#2273=CYLINDRICAL_SURFACE('',#28384,2.56);
#2274=CYLINDRICAL_SURFACE('',#28385,2.56);
#2275=CYLINDRICAL_SURFACE('',#28386,2.56);
#2276=CYLINDRICAL_SURFACE('',#28387,2.56);
#2277=CYLINDRICAL_SURFACE('',#28388,2.56);
#2278=CYLINDRICAL_SURFACE('',#28389,2.56);
#2279=CYLINDRICAL_SURFACE('',#28390,2.56);
#2280=CYLINDRICAL_SURFACE('',#28391,2.56);
#2281=CYLINDRICAL_SURFACE('',#28392,2.56);
#2282=CYLINDRICAL_SURFACE('',#28393,2.56);
#2283=CYLINDRICAL_SURFACE('',#28394,2.56);
#2284=CYLINDRICAL_SURFACE('',#28395,2.56);
#2285=CYLINDRICAL_SURFACE('',#28396,2.56);
#2286=CYLINDRICAL_SURFACE('',#28397,2.56);
#2287=CYLINDRICAL_SURFACE('',#28398,2.56);
#2288=CYLINDRICAL_SURFACE('',#28399,2.56);
#2289=CYLINDRICAL_SURFACE('',#28401,4.263);
#2290=CYLINDRICAL_SURFACE('',#28403,4.263);
#2291=CYLINDRICAL_SURFACE('',#28404,4.263);
#2292=CYLINDRICAL_SURFACE('',#28405,4.263);
#2293=CYLINDRICAL_SURFACE('',#28407,4.263);
#2294=CYLINDRICAL_SURFACE('',#28409,4.263);
#2295=CYLINDRICAL_SURFACE('',#28411,4.263);
#2296=CYLINDRICAL_SURFACE('',#28412,4.263);
#2297=CYLINDRICAL_SURFACE('',#28414,2.117);
#2298=CYLINDRICAL_SURFACE('',#28416,2.117);
#2299=CYLINDRICAL_SURFACE('',#28417,2.117);
#2300=CYLINDRICAL_SURFACE('',#28418,2.117);
#2301=CYLINDRICAL_SURFACE('',#28419,2.117);
#2302=CYLINDRICAL_SURFACE('',#28420,2.117);
#2303=CYLINDRICAL_SURFACE('',#28421,2.117);
#2304=CYLINDRICAL_SURFACE('',#28422,2.117);
#2305=CYLINDRICAL_SURFACE('',#28423,2.117);
#2306=CYLINDRICAL_SURFACE('',#28424,2.117);
#2307=CYLINDRICAL_SURFACE('',#28425,2.117);
#2308=CYLINDRICAL_SURFACE('',#28426,2.117);
#2309=CYLINDRICAL_SURFACE('',#28427,2.117);
#2310=CYLINDRICAL_SURFACE('',#28428,2.117);
#2311=CYLINDRICAL_SURFACE('',#28429,2.117);
#2312=CYLINDRICAL_SURFACE('',#28430,2.117);
#2313=CYLINDRICAL_SURFACE('',#28431,2.117);
#2314=CYLINDRICAL_SURFACE('',#28432,2.117);
#2315=CYLINDRICAL_SURFACE('',#28433,2.117);
#2316=CYLINDRICAL_SURFACE('',#28434,2.117);
#2317=CYLINDRICAL_SURFACE('',#28435,2.117);
#2318=CYLINDRICAL_SURFACE('',#28436,2.117);
#2319=CYLINDRICAL_SURFACE('',#28437,2.117);
#2320=CYLINDRICAL_SURFACE('',#28438,2.117);
#2321=CYLINDRICAL_SURFACE('',#28439,2.117);
#2322=CYLINDRICAL_SURFACE('',#28440,2.117);
#2323=CYLINDRICAL_SURFACE('',#28441,2.117);
#2324=CYLINDRICAL_SURFACE('',#28443,2.117);
#2325=CYLINDRICAL_SURFACE('',#28445,2.117);
#2326=CYLINDRICAL_SURFACE('',#28446,2.117);
#2327=CYLINDRICAL_SURFACE('',#28447,2.117);
#2328=CYLINDRICAL_SURFACE('',#28448,2.117);
#2329=CYLINDRICAL_SURFACE('',#28449,2.117);
#2330=CYLINDRICAL_SURFACE('',#28450,2.117);
#2331=CYLINDRICAL_SURFACE('',#28451,2.117);
#2332=CYLINDRICAL_SURFACE('',#28452,2.117);
#2333=CYLINDRICAL_SURFACE('',#28453,2.117);
#2334=CYLINDRICAL_SURFACE('',#28454,2.117);
#2335=CYLINDRICAL_SURFACE('',#28455,2.117);
#2336=CYLINDRICAL_SURFACE('',#28456,2.117);
#2337=CYLINDRICAL_SURFACE('',#28457,2.117);
#2338=CYLINDRICAL_SURFACE('',#28458,2.117);
#2339=CYLINDRICAL_SURFACE('',#28459,2.117);
#2340=CYLINDRICAL_SURFACE('',#28460,2.117);
#2341=CYLINDRICAL_SURFACE('',#28461,2.117);
#2342=CYLINDRICAL_SURFACE('',#28462,2.117);
#2343=CYLINDRICAL_SURFACE('',#28463,2.117);
#2344=CYLINDRICAL_SURFACE('',#28464,2.117);
#2345=CYLINDRICAL_SURFACE('',#28465,2.117);
#2346=CYLINDRICAL_SURFACE('',#28466,2.117);
#2347=CYLINDRICAL_SURFACE('',#28467,2.117);
#2348=CYLINDRICAL_SURFACE('',#28468,2.117);
#2349=CYLINDRICAL_SURFACE('',#28469,2.117);
#2350=CYLINDRICAL_SURFACE('',#28470,2.117);
#2351=CYLINDRICAL_SURFACE('',#28472,2.117);
#2352=CYLINDRICAL_SURFACE('',#28474,2.117);
#2353=CYLINDRICAL_SURFACE('',#28475,2.117);
#2354=CYLINDRICAL_SURFACE('',#28476,2.117);
#2355=CYLINDRICAL_SURFACE('',#28477,2.117);
#2356=CYLINDRICAL_SURFACE('',#28478,2.117);
#2357=CYLINDRICAL_SURFACE('',#28479,2.117);
#2358=CYLINDRICAL_SURFACE('',#28480,2.117);
#2359=CYLINDRICAL_SURFACE('',#28481,2.117);
#2360=CYLINDRICAL_SURFACE('',#28482,2.117);
#2361=CYLINDRICAL_SURFACE('',#28483,2.117);
#2362=CYLINDRICAL_SURFACE('',#28484,2.117);
#2363=CYLINDRICAL_SURFACE('',#28485,2.117);
#2364=CYLINDRICAL_SURFACE('',#28486,2.117);
#2365=CYLINDRICAL_SURFACE('',#28487,2.117);
#2366=CYLINDRICAL_SURFACE('',#28488,2.117);
#2367=CYLINDRICAL_SURFACE('',#28489,2.117);
#2368=CYLINDRICAL_SURFACE('',#28490,2.117);
#2369=CYLINDRICAL_SURFACE('',#28491,2.117);
#2370=CYLINDRICAL_SURFACE('',#28492,2.117);
#2371=CYLINDRICAL_SURFACE('',#28493,2.117);
#2372=CYLINDRICAL_SURFACE('',#28494,2.117);
#2373=CYLINDRICAL_SURFACE('',#28495,2.117);
#2374=CYLINDRICAL_SURFACE('',#28496,2.117);
#2375=CYLINDRICAL_SURFACE('',#28497,2.117);
#2376=CYLINDRICAL_SURFACE('',#28498,2.117);
#2377=CYLINDRICAL_SURFACE('',#28499,2.117);
#2378=CYLINDRICAL_SURFACE('',#28501,2.117);
#2379=CYLINDRICAL_SURFACE('',#28503,2.117);
#2380=CYLINDRICAL_SURFACE('',#28504,2.117);
#2381=CYLINDRICAL_SURFACE('',#28505,2.117);
#2382=CYLINDRICAL_SURFACE('',#28506,2.117);
#2383=CYLINDRICAL_SURFACE('',#28507,2.117);
#2384=CYLINDRICAL_SURFACE('',#28508,2.117);
#2385=CYLINDRICAL_SURFACE('',#28509,2.117);
#2386=CYLINDRICAL_SURFACE('',#28510,2.117);
#2387=CYLINDRICAL_SURFACE('',#28511,2.117);
#2388=CYLINDRICAL_SURFACE('',#28512,2.117);
#2389=CYLINDRICAL_SURFACE('',#28513,2.117);
#2390=CYLINDRICAL_SURFACE('',#28514,2.117);
#2391=CYLINDRICAL_SURFACE('',#28515,2.117);
#2392=CYLINDRICAL_SURFACE('',#28516,2.117);
#2393=CYLINDRICAL_SURFACE('',#28517,2.117);
#2394=CYLINDRICAL_SURFACE('',#28518,2.117);
#2395=CYLINDRICAL_SURFACE('',#28519,2.117);
#2396=CYLINDRICAL_SURFACE('',#28520,2.117);
#2397=CYLINDRICAL_SURFACE('',#28521,2.117);
#2398=CYLINDRICAL_SURFACE('',#28522,2.117);
#2399=CYLINDRICAL_SURFACE('',#28523,2.117);
#2400=CYLINDRICAL_SURFACE('',#28524,2.117);
#2401=CYLINDRICAL_SURFACE('',#28525,2.117);
#2402=CYLINDRICAL_SURFACE('',#28526,2.117);
#2403=CYLINDRICAL_SURFACE('',#28527,2.117);
#2404=CYLINDRICAL_SURFACE('',#28528,2.117);
#2405=CYLINDRICAL_SURFACE('',#28530,2.117);
#2406=CYLINDRICAL_SURFACE('',#28531,2.117);
#2407=CYLINDRICAL_SURFACE('',#28532,2.117);
#2408=CYLINDRICAL_SURFACE('',#28533,2.117);
#2409=CYLINDRICAL_SURFACE('',#28534,4.263);
#2410=CYLINDRICAL_SURFACE('',#28535,4.263);
#2411=CYLINDRICAL_SURFACE('',#28537,2.56);
#2412=CYLINDRICAL_SURFACE('',#28538,2.56);
#2413=CYLINDRICAL_SURFACE('',#28539,2.56);
#2414=CYLINDRICAL_SURFACE('',#28540,2.55999999999999);
#2415=CYLINDRICAL_SURFACE('',#28541,5.099);
#2416=CYLINDRICAL_SURFACE('',#28542,5.099);
#2417=CYLINDRICAL_SURFACE('',#28543,4.);
#2418=CYLINDRICAL_SURFACE('',#28547,4.5);
#2419=CYLINDRICAL_SURFACE('',#28552,4.);
#2420=CYLINDRICAL_SURFACE('',#28556,4.5);
#2421=CYLINDRICAL_SURFACE('',#28561,5.);
#2422=CYLINDRICAL_SURFACE('',#28588,3.);
#2423=CYLINDRICAL_SURFACE('',#28592,6.);
#2424=CYLINDRICAL_SURFACE('',#28596,6.);
#2425=CYLINDRICAL_SURFACE('',#28611,3.);
#2426=CYLINDRICAL_SURFACE('',#28617,4.);
#2427=CYLINDRICAL_SURFACE('',#28621,5.);
#2428=CYLINDRICAL_SURFACE('',#28624,6.);
#2429=CYLINDRICAL_SURFACE('',#28628,6.);
#2430=CYLINDRICAL_SURFACE('',#28643,3.);
#2431=CYLINDRICAL_SURFACE('',#28654,3.);
#2432=CYLINDRICAL_SURFACE('',#28662,5.);
#2433=CYLINDRICAL_SURFACE('',#28665,4.);
#2434=CYLINDRICAL_SURFACE('',#28668,2.5);
#2435=CYLINDRICAL_SURFACE('',#28671,2.5);
#2436=CYLINDRICAL_SURFACE('',#28675,3.99143708455989);
#2437=CYLINDRICAL_SURFACE('',#28677,0.190999999999999);
#2438=CYLINDRICAL_SURFACE('',#28680,0.190999999999999);
#2439=CYLINDRICAL_SURFACE('',#28683,0.254);
#2440=CYLINDRICAL_SURFACE('',#28686,5.);
#2441=CYLINDRICAL_SURFACE('',#28688,5.);
#2442=CYLINDRICAL_SURFACE('',#28691,5.);
#2443=CYLINDRICAL_SURFACE('',#28694,5.);
#2444=CYLINDRICAL_SURFACE('',#28697,0.253999999999999);
#2445=CYLINDRICAL_SURFACE('',#28700,0.190999999999999);
#2446=CYLINDRICAL_SURFACE('',#28703,0.191);
#2447=CYLINDRICAL_SURFACE('',#28706,3.9914370845599);
#2448=CYLINDRICAL_SURFACE('',#28711,3.);
#2449=CYLINDRICAL_SURFACE('',#28715,3.);
#2450=CYLINDRICAL_SURFACE('',#28719,0.5);
#2451=CYLINDRICAL_SURFACE('',#28722,0.5);
#2452=CYLINDRICAL_SURFACE('',#28724,0.5);
#2453=CYLINDRICAL_SURFACE('',#28731,0.5);
#2454=CYLINDRICAL_SURFACE('',#28737,0.5);
#2455=CYLINDRICAL_SURFACE('',#28743,0.5);
#2456=CYLINDRICAL_SURFACE('',#28748,0.5);
#2457=CYLINDRICAL_SURFACE('',#28750,0.5);
#2458=CYLINDRICAL_SURFACE('',#28752,0.5);
#2459=CYLINDRICAL_SURFACE('',#28758,0.5);
#2460=CYLINDRICAL_SURFACE('',#28760,0.5);
#2461=CYLINDRICAL_SURFACE('',#28761,0.5);
#2462=CYLINDRICAL_SURFACE('',#28767,0.5);
#2463=CYLINDRICAL_SURFACE('',#28769,0.5);
#2464=CYLINDRICAL_SURFACE('',#28771,0.5);
#2465=CYLINDRICAL_SURFACE('',#28776,0.5);
#2466=CYLINDRICAL_SURFACE('',#28782,0.5);
#2467=CYLINDRICAL_SURFACE('',#28788,0.5);
#2468=CYLINDRICAL_SURFACE('',#28794,0.5);
#2469=CYLINDRICAL_SURFACE('',#28796,0.5);
#2470=CYLINDRICAL_SURFACE('',#28799,0.5);
#2471=CYLINDRICAL_SURFACE('',#28801,0.5);
#2472=CYLINDRICAL_SURFACE('',#28808,1.);
#2473=CYLINDRICAL_SURFACE('',#28813,1.);
#2474=CYLINDRICAL_SURFACE('',#28816,5.);
#2475=CYLINDRICAL_SURFACE('',#28819,3.);
#2476=CYLINDRICAL_SURFACE('',#28823,0.508000000000002);
#2477=CYLINDRICAL_SURFACE('',#28826,0.5);
#2478=CYLINDRICAL_SURFACE('',#28832,0.5);
#2479=CYLINDRICAL_SURFACE('',#28837,0.5);
#2480=CYLINDRICAL_SURFACE('',#28840,0.5);
#2481=CYLINDRICAL_SURFACE('',#28842,0.5);
#2482=CYLINDRICAL_SURFACE('',#28848,0.5);
#2483=CYLINDRICAL_SURFACE('',#28852,0.5);
#2484=CYLINDRICAL_SURFACE('',#28862,0.5);
#2485=CYLINDRICAL_SURFACE('',#28867,0.5);
#2486=CYLINDRICAL_SURFACE('',#28871,0.5);
#2487=CYLINDRICAL_SURFACE('',#28875,0.5);
#2488=CYLINDRICAL_SURFACE('',#28877,0.5);
#2489=CYLINDRICAL_SURFACE('',#28882,0.5);
#2490=CYLINDRICAL_SURFACE('',#28883,0.5);
#2491=CYLINDRICAL_SURFACE('',#28886,0.5);
#2492=CYLINDRICAL_SURFACE('',#28888,0.5);
#2493=CYLINDRICAL_SURFACE('',#28889,0.5);
#2494=CYLINDRICAL_SURFACE('',#28895,0.5);
#2495=CYLINDRICAL_SURFACE('',#28896,0.5);
#2496=CYLINDRICAL_SURFACE('',#28901,0.5);
#2497=CYLINDRICAL_SURFACE('',#28905,0.5);
#2498=CYLINDRICAL_SURFACE('',#28910,0.999999999999992);
#2499=CYLINDRICAL_SURFACE('',#28914,1.);
#2500=CYLINDRICAL_SURFACE('',#28916,5.);
#2501=CYLINDRICAL_SURFACE('',#28918,3.);
#2502=CYLINDRICAL_SURFACE('',#28920,3.);
#2503=CYLINDRICAL_SURFACE('',#28922,3.);
#2504=CYLINDRICAL_SURFACE('',#28928,0.508000000000002);
#2505=CYLINDRICAL_SURFACE('',#28930,0.499999999999998);
#2506=CYLINDRICAL_SURFACE('',#28932,3.);
#2507=CYLINDRICAL_SURFACE('',#28936,3.);
#2508=CYLINDRICAL_SURFACE('',#28940,0.5);
#2509=CYLINDRICAL_SURFACE('',#28943,0.5);
#2510=CYLINDRICAL_SURFACE('',#28945,0.5);
#2511=CYLINDRICAL_SURFACE('',#28952,0.5);
#2512=CYLINDRICAL_SURFACE('',#28958,0.5);
#2513=CYLINDRICAL_SURFACE('',#28964,0.5);
#2514=CYLINDRICAL_SURFACE('',#28969,0.5);
#2515=CYLINDRICAL_SURFACE('',#28971,0.5);
#2516=CYLINDRICAL_SURFACE('',#28973,0.5);
#2517=CYLINDRICAL_SURFACE('',#28979,0.5);
#2518=CYLINDRICAL_SURFACE('',#28981,0.5);
#2519=CYLINDRICAL_SURFACE('',#28982,0.5);
#2520=CYLINDRICAL_SURFACE('',#28988,0.5);
#2521=CYLINDRICAL_SURFACE('',#28990,0.5);
#2522=CYLINDRICAL_SURFACE('',#28992,0.5);
#2523=CYLINDRICAL_SURFACE('',#28997,0.5);
#2524=CYLINDRICAL_SURFACE('',#29003,0.5);
#2525=CYLINDRICAL_SURFACE('',#29009,0.5);
#2526=CYLINDRICAL_SURFACE('',#29015,0.5);
#2527=CYLINDRICAL_SURFACE('',#29017,0.5);
#2528=CYLINDRICAL_SURFACE('',#29020,0.5);
#2529=CYLINDRICAL_SURFACE('',#29022,0.5);
#2530=CYLINDRICAL_SURFACE('',#29029,1.);
#2531=CYLINDRICAL_SURFACE('',#29034,1.);
#2532=CYLINDRICAL_SURFACE('',#29037,5.);
#2533=CYLINDRICAL_SURFACE('',#29040,3.);
#2534=CYLINDRICAL_SURFACE('',#29044,0.508000000000002);
#2535=CYLINDRICAL_SURFACE('',#29047,0.5);
#2536=CYLINDRICAL_SURFACE('',#29053,0.5);
#2537=CYLINDRICAL_SURFACE('',#29058,0.5);
#2538=CYLINDRICAL_SURFACE('',#29061,0.5);
#2539=CYLINDRICAL_SURFACE('',#29063,0.5);
#2540=CYLINDRICAL_SURFACE('',#29069,0.5);
#2541=CYLINDRICAL_SURFACE('',#29073,0.5);
#2542=CYLINDRICAL_SURFACE('',#29083,0.5);
#2543=CYLINDRICAL_SURFACE('',#29088,0.5);
#2544=CYLINDRICAL_SURFACE('',#29092,0.5);
#2545=CYLINDRICAL_SURFACE('',#29096,0.5);
#2546=CYLINDRICAL_SURFACE('',#29098,0.5);
#2547=CYLINDRICAL_SURFACE('',#29103,0.5);
#2548=CYLINDRICAL_SURFACE('',#29104,0.5);
#2549=CYLINDRICAL_SURFACE('',#29107,0.5);
#2550=CYLINDRICAL_SURFACE('',#29109,0.5);
#2551=CYLINDRICAL_SURFACE('',#29110,0.5);
#2552=CYLINDRICAL_SURFACE('',#29116,0.5);
#2553=CYLINDRICAL_SURFACE('',#29117,0.5);
#2554=CYLINDRICAL_SURFACE('',#29122,0.5);
#2555=CYLINDRICAL_SURFACE('',#29126,0.5);
#2556=CYLINDRICAL_SURFACE('',#29131,0.999999999999992);
#2557=CYLINDRICAL_SURFACE('',#29135,1.);
#2558=CYLINDRICAL_SURFACE('',#29137,5.);
#2559=CYLINDRICAL_SURFACE('',#29139,3.);
#2560=CYLINDRICAL_SURFACE('',#29141,3.);
#2561=CYLINDRICAL_SURFACE('',#29143,3.);
#2562=CYLINDRICAL_SURFACE('',#29149,0.508000000000002);
#2563=CYLINDRICAL_SURFACE('',#29151,0.499999999999998);
#2564=CYLINDRICAL_SURFACE('',#29152,3.);
#2565=CYLINDRICAL_SURFACE('',#29157,3.00000000000001);
#2566=CYLINDRICAL_SURFACE('',#29165,3.);
#2567=CYLINDRICAL_SURFACE('',#29185,3.);
#2568=CYLINDRICAL_SURFACE('',#29205,3.00000000000001);
#2569=CYLINDRICAL_SURFACE('',#29223,0.3);
#2570=CYLINDRICAL_SURFACE('',#29229,0.499999999999998);
#2571=CYLINDRICAL_SURFACE('',#29231,0.499999999999998);
#2572=CYLINDRICAL_SURFACE('',#29233,0.499999999999998);
#2573=CYLINDRICAL_SURFACE('',#29237,1.);
#2574=CYLINDRICAL_SURFACE('',#29239,1.);
#2575=CYLINDRICAL_SURFACE('',#29241,1.);
#2576=CYLINDRICAL_SURFACE('',#29245,2.);
#2577=CYLINDRICAL_SURFACE('',#29247,2.);
#2578=CYLINDRICAL_SURFACE('',#29249,2.);
#2579=CYLINDRICAL_SURFACE('',#29253,5.);
#2580=CYLINDRICAL_SURFACE('',#29255,5.);
#2581=CYLINDRICAL_SURFACE('',#29257,5.);
#2582=CYLINDRICAL_SURFACE('',#29261,0.800000000000001);
#2583=CYLINDRICAL_SURFACE('',#29263,0.800000000000001);
#2584=CYLINDRICAL_SURFACE('',#29265,0.800000000000001);
#2585=CYLINDRICAL_SURFACE('',#29269,0.3);
#2586=CYLINDRICAL_SURFACE('',#29275,0.499999999999998);
#2587=CYLINDRICAL_SURFACE('',#29277,0.499999999999998);
#2588=CYLINDRICAL_SURFACE('',#29278,0.499999999999998);
#2589=CYLINDRICAL_SURFACE('',#29282,1.);
#2590=CYLINDRICAL_SURFACE('',#29284,1.);
#2591=CYLINDRICAL_SURFACE('',#29285,1.);
#2592=CYLINDRICAL_SURFACE('',#29289,2.);
#2593=CYLINDRICAL_SURFACE('',#29291,2.);
#2594=CYLINDRICAL_SURFACE('',#29292,2.);
#2595=CYLINDRICAL_SURFACE('',#29296,5.);
#2596=CYLINDRICAL_SURFACE('',#29298,5.);
#2597=CYLINDRICAL_SURFACE('',#29299,5.);
#2598=CYLINDRICAL_SURFACE('',#29303,0.800000000000001);
#2599=CYLINDRICAL_SURFACE('',#29305,0.800000000000001);
#2600=CYLINDRICAL_SURFACE('',#29306,0.800000000000001);
#2601=CYLINDRICAL_SURFACE('',#29310,2.5);
#2602=CYLINDRICAL_SURFACE('',#29313,2.5);
#2603=CYLINDRICAL_SURFACE('',#29316,2.5);
#2604=CYLINDRICAL_SURFACE('',#29321,0.3);
#2605=CYLINDRICAL_SURFACE('',#29325,0.300000000000002);
#2606=CYLINDRICAL_SURFACE('',#29329,0.800000000000001);
#2607=CYLINDRICAL_SURFACE('',#29331,5.);
#2608=CYLINDRICAL_SURFACE('',#29333,2.);
#2609=CYLINDRICAL_SURFACE('',#29335,1.);
#2610=CYLINDRICAL_SURFACE('',#29337,0.499999999999998);
#2611=CYLINDRICAL_SURFACE('',#29340,0.300000000000002);
#2612=CYLINDRICAL_SURFACE('',#29344,0.500000000000001);
#2613=CYLINDRICAL_SURFACE('',#29348,0.508000000000002);
#2614=CYLINDRICAL_SURFACE('',#29352,3.);
#2615=CYLINDRICAL_SURFACE('',#29356,5.);
#2616=CYLINDRICAL_SURFACE('',#29360,1.);
#2617=CYLINDRICAL_SURFACE('',#29366,1.);
#2618=CYLINDRICAL_SURFACE('',#29373,0.3);
#2619=CYLINDRICAL_SURFACE('',#29377,0.300000000000002);
#2620=CYLINDRICAL_SURFACE('',#29381,0.800000000000001);
#2621=CYLINDRICAL_SURFACE('',#29384,5.);
#2622=CYLINDRICAL_SURFACE('',#29387,2.);
#2623=CYLINDRICAL_SURFACE('',#29390,1.);
#2624=CYLINDRICAL_SURFACE('',#29393,0.499999999999998);
#2625=CYLINDRICAL_SURFACE('',#29397,0.300000000000002);
#2626=CYLINDRICAL_SURFACE('',#29401,0.5);
#2627=CYLINDRICAL_SURFACE('',#29405,0.508000000000002);
#2628=CYLINDRICAL_SURFACE('',#29409,3.);
#2629=CYLINDRICAL_SURFACE('',#29413,5.);
#2630=CYLINDRICAL_SURFACE('',#29417,1.);
#2631=CYLINDRICAL_SURFACE('',#29423,1.);
#2632=CYLINDRICAL_SURFACE('',#29448,0.190999999999998);
#2633=CYLINDRICAL_SURFACE('',#29461,0.191);
#2634=CYLINDRICAL_SURFACE('',#29467,3.9858295958384);
#2635=CYLINDRICAL_SURFACE('',#29468,3.9858295958384);
#2636=CYLINDRICAL_SURFACE('',#29480,0.190999999999999);
#2637=CYLINDRICAL_SURFACE('',#29482,0.191);
#2638=CYLINDRICAL_SURFACE('',#29483,0.590999999999999);
#2639=CYLINDRICAL_SURFACE('',#29484,0.590999999999999);
#2640=CYLINDRICAL_SURFACE('',#29485,0.191000000000001);
#2641=CYLINDRICAL_SURFACE('',#29487,0.190999999999999);
#2642=CYLINDRICAL_SURFACE('',#29504,0.190999999999998);
#2643=CYLINDRICAL_SURFACE('',#29518,0.191);
#2644=CYLINDRICAL_SURFACE('',#29524,3.9858295958384);
#2645=CYLINDRICAL_SURFACE('',#29525,3.9858295958384);
#2646=CYLINDRICAL_SURFACE('',#29542,0.190999999999999);
#2647=CYLINDRICAL_SURFACE('',#29544,0.191);
#2648=CYLINDRICAL_SURFACE('',#29545,0.590999999999999);
#2649=CYLINDRICAL_SURFACE('',#29546,0.590999999999999);
#2650=CYLINDRICAL_SURFACE('',#29547,0.191000000000001);
#2651=CYLINDRICAL_SURFACE('',#29549,0.190999999999999);
#2652=CYLINDRICAL_SURFACE('',#29551,12.5);
#2653=CYLINDRICAL_SURFACE('',#29554,0.999999999999998);
#2654=CYLINDRICAL_SURFACE('',#29562,1.);
#2655=CYLINDRICAL_SURFACE('',#29567,0.299999999999999);
#2656=CYLINDRICAL_SURFACE('',#29570,0.75);
#2657=CYLINDRICAL_SURFACE('',#29573,0.300000000000001);
#2658=CYLINDRICAL_SURFACE('',#29579,1.);
#2659=CYLINDRICAL_SURFACE('',#29583,0.499999999999999);
#2660=CYLINDRICAL_SURFACE('',#29587,0.299999999999998);
#2661=CYLINDRICAL_SURFACE('',#29593,0.999999999999998);
#2662=CYLINDRICAL_SURFACE('',#29597,5.);
#2663=CYLINDRICAL_SURFACE('',#29601,5.);
#2664=CYLINDRICAL_SURFACE('',#29605,0.999999999999996);
#2665=CYLINDRICAL_SURFACE('',#29611,0.299999999999998);
#2666=CYLINDRICAL_SURFACE('',#29615,0.5);
#2667=CYLINDRICAL_SURFACE('',#29619,1.);
#2668=CYLINDRICAL_SURFACE('',#29625,0.300000000000002);
#2669=CYLINDRICAL_SURFACE('',#29628,0.75000062202425);
#2670=CYLINDRICAL_SURFACE('',#29631,0.300000000000001);
#2671=CYLINDRICAL_SURFACE('',#29636,1.);
#2672=CYLINDRICAL_SURFACE('',#29644,1.);
#2673=CYLINDRICAL_SURFACE('',#29649,0.300000000000002);
#2674=CYLINDRICAL_SURFACE('',#29652,0.75);
#2675=CYLINDRICAL_SURFACE('',#29655,0.300000000000001);
#2676=CYLINDRICAL_SURFACE('',#29661,1.);
#2677=CYLINDRICAL_SURFACE('',#29665,0.500000000000003);
#2678=CYLINDRICAL_SURFACE('',#29669,0.299999999999998);
#2679=CYLINDRICAL_SURFACE('',#29675,1.);
#2680=CYLINDRICAL_SURFACE('',#29679,4.99999999999999);
#2681=CYLINDRICAL_SURFACE('',#29683,4.99999999999999);
#2682=CYLINDRICAL_SURFACE('',#29687,1.);
#2683=CYLINDRICAL_SURFACE('',#29693,0.300000000000003);
#2684=CYLINDRICAL_SURFACE('',#29697,0.5);
#2685=CYLINDRICAL_SURFACE('',#29701,1.);
#2686=CYLINDRICAL_SURFACE('',#29707,0.300000000000001);
#2687=CYLINDRICAL_SURFACE('',#29710,0.750000622024213);
#2688=CYLINDRICAL_SURFACE('',#29713,0.300000000000001);
#2689=CYLINDRICAL_SURFACE('',#29721,5.099);
#2690=CYLINDRICAL_SURFACE('',#29723,5.099);
#2691=CYLINDRICAL_SURFACE('',#29724,5.099);
#2692=CYLINDRICAL_SURFACE('',#29725,5.099);
#2693=CYLINDRICAL_SURFACE('',#29726,5.099);
#2694=CYLINDRICAL_SURFACE('',#29728,5.099);
#2695=CYLINDRICAL_SURFACE('',#29729,5.099);
#2696=CYLINDRICAL_SURFACE('',#29730,5.099);
#2697=CYLINDRICAL_SURFACE('',#29731,2.55999999999999);
#2698=CYLINDRICAL_SURFACE('',#29733,2.55999999999999);
#2699=CYLINDRICAL_SURFACE('',#29734,2.55999999999999);
#2700=CYLINDRICAL_SURFACE('',#29735,2.55999999999999);
#2701=CYLINDRICAL_SURFACE('',#29736,2.55999999999999);
#2702=CYLINDRICAL_SURFACE('',#29737,2.55999999999999);
#2703=CYLINDRICAL_SURFACE('',#29738,2.55999999999999);
#2704=CYLINDRICAL_SURFACE('',#29739,2.55999999999999);
#2705=CYLINDRICAL_SURFACE('',#29740,2.55999999999999);
#2706=CYLINDRICAL_SURFACE('',#29741,2.55999999999999);
#2707=CYLINDRICAL_SURFACE('',#29742,2.55999999999999);
#2708=CYLINDRICAL_SURFACE('',#29743,2.55999999999999);
#2709=CYLINDRICAL_SURFACE('',#29744,2.55999999999999);
#2710=CYLINDRICAL_SURFACE('',#29745,2.55999999999999);
#2711=CYLINDRICAL_SURFACE('',#29746,2.55999999999999);
#2712=CYLINDRICAL_SURFACE('',#29747,2.55999999999999);
#2713=CYLINDRICAL_SURFACE('',#29748,2.55999999999999);
#2714=CYLINDRICAL_SURFACE('',#29749,2.55999999999999);
#2715=CYLINDRICAL_SURFACE('',#29750,2.55999999999999);
#2716=CYLINDRICAL_SURFACE('',#29751,2.55999999999999);
#2717=CYLINDRICAL_SURFACE('',#29752,2.55999999999999);
#2718=CYLINDRICAL_SURFACE('',#29753,2.55999999999999);
#2719=CYLINDRICAL_SURFACE('',#29754,2.55999999999999);
#2720=CYLINDRICAL_SURFACE('',#29755,2.55999999999999);
#2721=CYLINDRICAL_SURFACE('',#29756,2.55999999999999);
#2722=CYLINDRICAL_SURFACE('',#29757,2.55999999999999);
#2723=CYLINDRICAL_SURFACE('',#29758,2.55999999999999);
#2724=CYLINDRICAL_SURFACE('',#29759,2.56);
#2725=CYLINDRICAL_SURFACE('',#29761,2.56);
#2726=CYLINDRICAL_SURFACE('',#29762,2.56);
#2727=CYLINDRICAL_SURFACE('',#29763,2.56);
#2728=CYLINDRICAL_SURFACE('',#29764,2.56);
#2729=CYLINDRICAL_SURFACE('',#29765,2.56);
#2730=CYLINDRICAL_SURFACE('',#29766,2.56);
#2731=CYLINDRICAL_SURFACE('',#29767,2.56);
#2732=CYLINDRICAL_SURFACE('',#29768,2.56);
#2733=CYLINDRICAL_SURFACE('',#29769,2.56);
#2734=CYLINDRICAL_SURFACE('',#29770,2.56);
#2735=CYLINDRICAL_SURFACE('',#29771,2.56);
#2736=CYLINDRICAL_SURFACE('',#29772,2.56);
#2737=CYLINDRICAL_SURFACE('',#29773,2.56);
#2738=CYLINDRICAL_SURFACE('',#29774,2.56);
#2739=CYLINDRICAL_SURFACE('',#29775,2.56);
#2740=CYLINDRICAL_SURFACE('',#29776,2.56);
#2741=CYLINDRICAL_SURFACE('',#29777,2.56);
#2742=CYLINDRICAL_SURFACE('',#29778,2.56);
#2743=CYLINDRICAL_SURFACE('',#29779,2.56);
#2744=CYLINDRICAL_SURFACE('',#29780,2.56);
#2745=CYLINDRICAL_SURFACE('',#29781,2.56);
#2746=CYLINDRICAL_SURFACE('',#29782,2.56);
#2747=CYLINDRICAL_SURFACE('',#29783,2.56);
#2748=CYLINDRICAL_SURFACE('',#29784,2.56);
#2749=CYLINDRICAL_SURFACE('',#29785,2.56);
#2750=CYLINDRICAL_SURFACE('',#29786,2.56);
#2751=CYLINDRICAL_SURFACE('',#29787,2.56);
#2752=CYLINDRICAL_SURFACE('',#29789,2.56);
#2753=CYLINDRICAL_SURFACE('',#29790,2.56);
#2754=CYLINDRICAL_SURFACE('',#29791,2.56);
#2755=CYLINDRICAL_SURFACE('',#29792,2.56);
#2756=CYLINDRICAL_SURFACE('',#29793,2.56);
#2757=CYLINDRICAL_SURFACE('',#29794,2.56);
#2758=CYLINDRICAL_SURFACE('',#29795,2.56);
#2759=CYLINDRICAL_SURFACE('',#29796,2.56);
#2760=CYLINDRICAL_SURFACE('',#29797,2.56);
#2761=CYLINDRICAL_SURFACE('',#29798,2.56);
#2762=CYLINDRICAL_SURFACE('',#29799,2.56);
#2763=CYLINDRICAL_SURFACE('',#29800,2.56);
#2764=CYLINDRICAL_SURFACE('',#29801,2.56);
#2765=CYLINDRICAL_SURFACE('',#29802,2.56);
#2766=CYLINDRICAL_SURFACE('',#29803,2.56);
#2767=CYLINDRICAL_SURFACE('',#29804,2.56);
#2768=CYLINDRICAL_SURFACE('',#29805,2.56);
#2769=CYLINDRICAL_SURFACE('',#29806,2.56);
#2770=CYLINDRICAL_SURFACE('',#29807,2.56);
#2771=CYLINDRICAL_SURFACE('',#29808,2.56);
#2772=CYLINDRICAL_SURFACE('',#29809,2.56);
#2773=CYLINDRICAL_SURFACE('',#29810,2.56);
#2774=CYLINDRICAL_SURFACE('',#29811,2.56);
#2775=CYLINDRICAL_SURFACE('',#29812,2.56);
#2776=CYLINDRICAL_SURFACE('',#29813,2.56);
#2777=CYLINDRICAL_SURFACE('',#29814,2.56);
#2778=CYLINDRICAL_SURFACE('',#29815,2.56);
#2779=CYLINDRICAL_SURFACE('',#29817,2.56);
#2780=CYLINDRICAL_SURFACE('',#29818,2.56);
#2781=CYLINDRICAL_SURFACE('',#29819,2.56);
#2782=CYLINDRICAL_SURFACE('',#29820,2.56);
#2783=CYLINDRICAL_SURFACE('',#29821,2.56);
#2784=CYLINDRICAL_SURFACE('',#29822,2.56);
#2785=CYLINDRICAL_SURFACE('',#29823,2.56);
#2786=CYLINDRICAL_SURFACE('',#29824,2.56);
#2787=CYLINDRICAL_SURFACE('',#29825,2.56);
#2788=CYLINDRICAL_SURFACE('',#29826,2.56);
#2789=CYLINDRICAL_SURFACE('',#29827,2.56);
#2790=CYLINDRICAL_SURFACE('',#29828,2.56);
#2791=CYLINDRICAL_SURFACE('',#29829,2.56);
#2792=CYLINDRICAL_SURFACE('',#29830,2.56);
#2793=CYLINDRICAL_SURFACE('',#29831,2.56);
#2794=CYLINDRICAL_SURFACE('',#29832,2.56);
#2795=CYLINDRICAL_SURFACE('',#29833,2.56);
#2796=CYLINDRICAL_SURFACE('',#29834,2.56);
#2797=CYLINDRICAL_SURFACE('',#29835,2.56);
#2798=CYLINDRICAL_SURFACE('',#29836,2.56);
#2799=CYLINDRICAL_SURFACE('',#29837,2.56);
#2800=CYLINDRICAL_SURFACE('',#29838,2.56);
#2801=CYLINDRICAL_SURFACE('',#29839,2.56);
#2802=CYLINDRICAL_SURFACE('',#29840,2.56);
#2803=CYLINDRICAL_SURFACE('',#29841,2.56);
#2804=CYLINDRICAL_SURFACE('',#29842,2.56);
#2805=CYLINDRICAL_SURFACE('',#29843,4.263);
#2806=CYLINDRICAL_SURFACE('',#29845,4.263);
#2807=CYLINDRICAL_SURFACE('',#29847,4.263);
#2808=CYLINDRICAL_SURFACE('',#29848,4.263);
#2809=CYLINDRICAL_SURFACE('',#29849,4.263);
#2810=CYLINDRICAL_SURFACE('',#29851,4.263);
#2811=CYLINDRICAL_SURFACE('',#29852,4.263);
#2812=CYLINDRICAL_SURFACE('',#29853,4.263);
#2813=CYLINDRICAL_SURFACE('',#29855,2.117);
#2814=CYLINDRICAL_SURFACE('',#29857,2.117);
#2815=CYLINDRICAL_SURFACE('',#29858,2.117);
#2816=CYLINDRICAL_SURFACE('',#29859,2.117);
#2817=CYLINDRICAL_SURFACE('',#29860,2.117);
#2818=CYLINDRICAL_SURFACE('',#29861,2.117);
#2819=CYLINDRICAL_SURFACE('',#29862,2.117);
#2820=CYLINDRICAL_SURFACE('',#29863,2.117);
#2821=CYLINDRICAL_SURFACE('',#29864,2.117);
#2822=CYLINDRICAL_SURFACE('',#29865,2.117);
#2823=CYLINDRICAL_SURFACE('',#29866,2.117);
#2824=CYLINDRICAL_SURFACE('',#29867,2.117);
#2825=CYLINDRICAL_SURFACE('',#29868,2.117);
#2826=CYLINDRICAL_SURFACE('',#29869,2.117);
#2827=CYLINDRICAL_SURFACE('',#29870,2.117);
#2828=CYLINDRICAL_SURFACE('',#29871,2.117);
#2829=CYLINDRICAL_SURFACE('',#29872,2.117);
#2830=CYLINDRICAL_SURFACE('',#29873,2.117);
#2831=CYLINDRICAL_SURFACE('',#29874,2.117);
#2832=CYLINDRICAL_SURFACE('',#29875,2.117);
#2833=CYLINDRICAL_SURFACE('',#29876,2.117);
#2834=CYLINDRICAL_SURFACE('',#29877,2.117);
#2835=CYLINDRICAL_SURFACE('',#29878,2.117);
#2836=CYLINDRICAL_SURFACE('',#29879,2.117);
#2837=CYLINDRICAL_SURFACE('',#29880,2.117);
#2838=CYLINDRICAL_SURFACE('',#29881,2.117);
#2839=CYLINDRICAL_SURFACE('',#29882,2.117);
#2840=CYLINDRICAL_SURFACE('',#29883,2.117);
#2841=CYLINDRICAL_SURFACE('',#29885,2.117);
#2842=CYLINDRICAL_SURFACE('',#29886,2.117);
#2843=CYLINDRICAL_SURFACE('',#29887,2.117);
#2844=CYLINDRICAL_SURFACE('',#29888,2.117);
#2845=CYLINDRICAL_SURFACE('',#29889,2.117);
#2846=CYLINDRICAL_SURFACE('',#29890,2.117);
#2847=CYLINDRICAL_SURFACE('',#29891,2.117);
#2848=CYLINDRICAL_SURFACE('',#29892,2.117);
#2849=CYLINDRICAL_SURFACE('',#29893,2.117);
#2850=CYLINDRICAL_SURFACE('',#29894,2.117);
#2851=CYLINDRICAL_SURFACE('',#29895,2.117);
#2852=CYLINDRICAL_SURFACE('',#29896,2.117);
#2853=CYLINDRICAL_SURFACE('',#29897,2.117);
#2854=CYLINDRICAL_SURFACE('',#29898,2.117);
#2855=CYLINDRICAL_SURFACE('',#29899,2.117);
#2856=CYLINDRICAL_SURFACE('',#29900,2.117);
#2857=CYLINDRICAL_SURFACE('',#29901,2.117);
#2858=CYLINDRICAL_SURFACE('',#29902,2.117);
#2859=CYLINDRICAL_SURFACE('',#29903,2.117);
#2860=CYLINDRICAL_SURFACE('',#29904,2.117);
#2861=CYLINDRICAL_SURFACE('',#29905,2.117);
#2862=CYLINDRICAL_SURFACE('',#29906,2.117);
#2863=CYLINDRICAL_SURFACE('',#29907,2.117);
#2864=CYLINDRICAL_SURFACE('',#29908,2.117);
#2865=CYLINDRICAL_SURFACE('',#29909,2.117);
#2866=CYLINDRICAL_SURFACE('',#29910,2.117);
#2867=CYLINDRICAL_SURFACE('',#29911,2.117);
#2868=CYLINDRICAL_SURFACE('',#29913,2.117);
#2869=CYLINDRICAL_SURFACE('',#29914,2.117);
#2870=CYLINDRICAL_SURFACE('',#29915,2.117);
#2871=CYLINDRICAL_SURFACE('',#29916,2.117);
#2872=CYLINDRICAL_SURFACE('',#29917,2.117);
#2873=CYLINDRICAL_SURFACE('',#29918,2.117);
#2874=CYLINDRICAL_SURFACE('',#29919,2.117);
#2875=CYLINDRICAL_SURFACE('',#29920,2.117);
#2876=CYLINDRICAL_SURFACE('',#29921,2.117);
#2877=CYLINDRICAL_SURFACE('',#29922,2.117);
#2878=CYLINDRICAL_SURFACE('',#29923,2.117);
#2879=CYLINDRICAL_SURFACE('',#29924,2.117);
#2880=CYLINDRICAL_SURFACE('',#29925,2.117);
#2881=CYLINDRICAL_SURFACE('',#29926,2.117);
#2882=CYLINDRICAL_SURFACE('',#29927,2.117);
#2883=CYLINDRICAL_SURFACE('',#29928,2.117);
#2884=CYLINDRICAL_SURFACE('',#29929,2.117);
#2885=CYLINDRICAL_SURFACE('',#29930,2.117);
#2886=CYLINDRICAL_SURFACE('',#29931,2.117);
#2887=CYLINDRICAL_SURFACE('',#29932,2.117);
#2888=CYLINDRICAL_SURFACE('',#29933,2.117);
#2889=CYLINDRICAL_SURFACE('',#29934,2.117);
#2890=CYLINDRICAL_SURFACE('',#29935,2.117);
#2891=CYLINDRICAL_SURFACE('',#29936,2.117);
#2892=CYLINDRICAL_SURFACE('',#29937,2.117);
#2893=CYLINDRICAL_SURFACE('',#29938,2.117);
#2894=CYLINDRICAL_SURFACE('',#29939,2.117);
#2895=CYLINDRICAL_SURFACE('',#29941,2.117);
#2896=CYLINDRICAL_SURFACE('',#29942,2.117);
#2897=CYLINDRICAL_SURFACE('',#29943,2.117);
#2898=CYLINDRICAL_SURFACE('',#29944,2.117);
#2899=CYLINDRICAL_SURFACE('',#29945,2.117);
#2900=CYLINDRICAL_SURFACE('',#29946,2.117);
#2901=CYLINDRICAL_SURFACE('',#29947,2.117);
#2902=CYLINDRICAL_SURFACE('',#29948,2.117);
#2903=CYLINDRICAL_SURFACE('',#29949,2.117);
#2904=CYLINDRICAL_SURFACE('',#29950,2.117);
#2905=CYLINDRICAL_SURFACE('',#29951,2.117);
#2906=CYLINDRICAL_SURFACE('',#29952,2.117);
#2907=CYLINDRICAL_SURFACE('',#29953,2.117);
#2908=CYLINDRICAL_SURFACE('',#29954,2.117);
#2909=CYLINDRICAL_SURFACE('',#29955,2.117);
#2910=CYLINDRICAL_SURFACE('',#29956,2.117);
#2911=CYLINDRICAL_SURFACE('',#29957,2.117);
#2912=CYLINDRICAL_SURFACE('',#29958,2.117);
#2913=CYLINDRICAL_SURFACE('',#29959,2.117);
#2914=CYLINDRICAL_SURFACE('',#29960,2.117);
#2915=CYLINDRICAL_SURFACE('',#29961,2.117);
#2916=CYLINDRICAL_SURFACE('',#29962,2.117);
#2917=CYLINDRICAL_SURFACE('',#29963,2.117);
#2918=CYLINDRICAL_SURFACE('',#29964,2.117);
#2919=CYLINDRICAL_SURFACE('',#29965,2.117);
#2920=CYLINDRICAL_SURFACE('',#29966,2.117);
#2921=CYLINDRICAL_SURFACE('',#29967,2.117);
#2922=CYLINDRICAL_SURFACE('',#29969,2.117);
#2923=CYLINDRICAL_SURFACE('',#29971,2.117);
#2924=CYLINDRICAL_SURFACE('',#29973,2.117);
#2925=CYLINDRICAL_SURFACE('',#29975,4.263);
#2926=CYLINDRICAL_SURFACE('',#29977,4.263);
#2927=CYLINDRICAL_SURFACE('',#29979,2.56);
#2928=CYLINDRICAL_SURFACE('',#29981,2.56);
#2929=CYLINDRICAL_SURFACE('',#29983,2.56);
#2930=CYLINDRICAL_SURFACE('',#29985,2.55999999999999);
#2931=CYLINDRICAL_SURFACE('',#29987,5.099);
#2932=CYLINDRICAL_SURFACE('',#29989,5.099);
#2933=CYLINDRICAL_SURFACE('',#29991,4.);
#2934=CYLINDRICAL_SURFACE('',#29995,4.5);
#2935=CYLINDRICAL_SURFACE('',#30000,4.);
#2936=CYLINDRICAL_SURFACE('',#30004,4.5);
#2937=CYLINDRICAL_SURFACE('',#30009,5.);
#2938=CYLINDRICAL_SURFACE('',#30036,3.);
#2939=CYLINDRICAL_SURFACE('',#30040,6.);
#2940=CYLINDRICAL_SURFACE('',#30044,6.);
#2941=CYLINDRICAL_SURFACE('',#30059,3.);
#2942=CYLINDRICAL_SURFACE('',#30065,4.);
#2943=CYLINDRICAL_SURFACE('',#30069,5.);
#2944=CYLINDRICAL_SURFACE('',#30072,6.);
#2945=CYLINDRICAL_SURFACE('',#30076,6.);
#2946=CYLINDRICAL_SURFACE('',#30091,3.);
#2947=CYLINDRICAL_SURFACE('',#30102,3.);
#2948=CYLINDRICAL_SURFACE('',#30110,5.);
#2949=CYLINDRICAL_SURFACE('',#30113,4.);
#2950=CYLINDRICAL_SURFACE('',#30116,2.5);
#2951=CYLINDRICAL_SURFACE('',#30119,2.5);
#2952=CYLINDRICAL_SURFACE('',#30123,3.99143708455989);
#2953=CYLINDRICAL_SURFACE('',#30125,0.190999999999999);
#2954=CYLINDRICAL_SURFACE('',#30128,0.190999999999999);
#2955=CYLINDRICAL_SURFACE('',#30131,0.254);
#2956=CYLINDRICAL_SURFACE('',#30134,5.);
#2957=CYLINDRICAL_SURFACE('',#30136,5.);
#2958=CYLINDRICAL_SURFACE('',#30139,5.);
#2959=CYLINDRICAL_SURFACE('',#30142,5.);
#2960=CYLINDRICAL_SURFACE('',#30145,0.253999999999999);
#2961=CYLINDRICAL_SURFACE('',#30148,0.190999999999999);
#2962=CYLINDRICAL_SURFACE('',#30151,0.191);
#2963=CYLINDRICAL_SURFACE('',#30154,3.9914370845599);
#2964=FACE_OUTER_BOUND('',#4277,.T.);
#2965=FACE_OUTER_BOUND('',#4278,.T.);
#2966=FACE_OUTER_BOUND('',#4279,.T.);
#2967=FACE_OUTER_BOUND('',#4280,.T.);
#2968=FACE_OUTER_BOUND('',#4281,.T.);
#2969=FACE_OUTER_BOUND('',#4282,.T.);
#2970=FACE_OUTER_BOUND('',#4283,.T.);
#2971=FACE_OUTER_BOUND('',#4284,.T.);
#2972=FACE_OUTER_BOUND('',#4285,.T.);
#2973=FACE_OUTER_BOUND('',#4286,.T.);
#2974=FACE_OUTER_BOUND('',#4287,.T.);
#2975=FACE_OUTER_BOUND('',#4288,.T.);
#2976=FACE_OUTER_BOUND('',#4289,.T.);
#2977=FACE_OUTER_BOUND('',#4290,.T.);
#2978=FACE_OUTER_BOUND('',#4291,.T.);
#2979=FACE_OUTER_BOUND('',#4292,.T.);
#2980=FACE_OUTER_BOUND('',#4293,.T.);
#2981=FACE_OUTER_BOUND('',#4294,.T.);
#2982=FACE_OUTER_BOUND('',#4295,.T.);
#2983=FACE_OUTER_BOUND('',#4296,.T.);
#2984=FACE_OUTER_BOUND('',#4297,.T.);
#2985=FACE_OUTER_BOUND('',#4298,.T.);
#2986=FACE_OUTER_BOUND('',#4299,.T.);
#2987=FACE_OUTER_BOUND('',#4300,.T.);
#2988=FACE_OUTER_BOUND('',#4301,.T.);
#2989=FACE_OUTER_BOUND('',#4302,.T.);
#2990=FACE_OUTER_BOUND('',#4303,.T.);
#2991=FACE_OUTER_BOUND('',#4304,.T.);
#2992=FACE_OUTER_BOUND('',#4305,.T.);
#2993=FACE_OUTER_BOUND('',#4306,.T.);
#2994=FACE_OUTER_BOUND('',#4307,.T.);
#2995=FACE_OUTER_BOUND('',#4308,.T.);
#2996=FACE_OUTER_BOUND('',#4309,.T.);
#2997=FACE_OUTER_BOUND('',#4310,.T.);
#2998=FACE_OUTER_BOUND('',#4311,.T.);
#2999=FACE_OUTER_BOUND('',#4312,.T.);
#3000=FACE_OUTER_BOUND('',#4313,.T.);
#3001=FACE_OUTER_BOUND('',#4314,.T.);
#3002=FACE_OUTER_BOUND('',#4315,.T.);
#3003=FACE_OUTER_BOUND('',#4316,.T.);
#3004=FACE_OUTER_BOUND('',#4317,.T.);
#3005=FACE_OUTER_BOUND('',#4318,.T.);
#3006=FACE_OUTER_BOUND('',#4319,.T.);
#3007=FACE_OUTER_BOUND('',#4320,.T.);
#3008=FACE_OUTER_BOUND('',#4321,.T.);
#3009=FACE_OUTER_BOUND('',#4322,.T.);
#3010=FACE_OUTER_BOUND('',#4323,.T.);
#3011=FACE_OUTER_BOUND('',#4324,.T.);
#3012=FACE_OUTER_BOUND('',#4325,.T.);
#3013=FACE_OUTER_BOUND('',#4326,.T.);
#3014=FACE_OUTER_BOUND('',#4327,.T.);
#3015=FACE_OUTER_BOUND('',#4328,.T.);
#3016=FACE_OUTER_BOUND('',#4329,.T.);
#3017=FACE_OUTER_BOUND('',#4330,.T.);
#3018=FACE_OUTER_BOUND('',#4331,.T.);
#3019=FACE_OUTER_BOUND('',#4332,.T.);
#3020=FACE_OUTER_BOUND('',#4333,.T.);
#3021=FACE_OUTER_BOUND('',#4334,.T.);
#3022=FACE_OUTER_BOUND('',#4335,.T.);
#3023=FACE_OUTER_BOUND('',#4336,.T.);
#3024=FACE_OUTER_BOUND('',#4337,.T.);
#3025=FACE_OUTER_BOUND('',#4338,.T.);
#3026=FACE_OUTER_BOUND('',#4339,.T.);
#3027=FACE_OUTER_BOUND('',#4340,.T.);
#3028=FACE_OUTER_BOUND('',#4341,.T.);
#3029=FACE_OUTER_BOUND('',#4342,.T.);
#3030=FACE_OUTER_BOUND('',#4343,.T.);
#3031=FACE_OUTER_BOUND('',#4344,.T.);
#3032=FACE_OUTER_BOUND('',#4345,.T.);
#3033=FACE_OUTER_BOUND('',#4346,.T.);
#3034=FACE_OUTER_BOUND('',#4347,.T.);
#3035=FACE_OUTER_BOUND('',#4348,.T.);
#3036=FACE_OUTER_BOUND('',#4349,.T.);
#3037=FACE_OUTER_BOUND('',#4350,.T.);
#3038=FACE_OUTER_BOUND('',#4351,.T.);
#3039=FACE_OUTER_BOUND('',#4352,.T.);
#3040=FACE_OUTER_BOUND('',#4353,.T.);
#3041=FACE_OUTER_BOUND('',#4354,.T.);
#3042=FACE_OUTER_BOUND('',#4355,.T.);
#3043=FACE_OUTER_BOUND('',#4356,.T.);
#3044=FACE_OUTER_BOUND('',#4357,.T.);
#3045=FACE_OUTER_BOUND('',#4358,.T.);
#3046=FACE_OUTER_BOUND('',#4359,.T.);
#3047=FACE_OUTER_BOUND('',#4360,.T.);
#3048=FACE_OUTER_BOUND('',#4361,.T.);
#3049=FACE_OUTER_BOUND('',#4362,.T.);
#3050=FACE_OUTER_BOUND('',#4363,.T.);
#3051=FACE_OUTER_BOUND('',#4364,.T.);
#3052=FACE_OUTER_BOUND('',#4365,.T.);
#3053=FACE_OUTER_BOUND('',#4366,.T.);
#3054=FACE_OUTER_BOUND('',#4367,.T.);
#3055=FACE_OUTER_BOUND('',#4368,.T.);
#3056=FACE_OUTER_BOUND('',#4369,.T.);
#3057=FACE_OUTER_BOUND('',#4370,.T.);
#3058=FACE_OUTER_BOUND('',#4371,.T.);
#3059=FACE_OUTER_BOUND('',#4372,.T.);
#3060=FACE_OUTER_BOUND('',#4373,.T.);
#3061=FACE_OUTER_BOUND('',#4374,.T.);
#3062=FACE_OUTER_BOUND('',#4375,.T.);
#3063=FACE_OUTER_BOUND('',#4376,.T.);
#3064=FACE_OUTER_BOUND('',#4377,.T.);
#3065=FACE_OUTER_BOUND('',#4378,.T.);
#3066=FACE_OUTER_BOUND('',#4379,.T.);
#3067=FACE_OUTER_BOUND('',#4380,.T.);
#3068=FACE_OUTER_BOUND('',#4381,.T.);
#3069=FACE_OUTER_BOUND('',#4382,.T.);
#3070=FACE_OUTER_BOUND('',#4383,.T.);
#3071=FACE_OUTER_BOUND('',#4384,.T.);
#3072=FACE_OUTER_BOUND('',#4385,.T.);
#3073=FACE_OUTER_BOUND('',#4386,.T.);
#3074=FACE_OUTER_BOUND('',#4387,.T.);
#3075=FACE_OUTER_BOUND('',#4388,.T.);
#3076=FACE_OUTER_BOUND('',#4389,.T.);
#3077=FACE_OUTER_BOUND('',#4390,.T.);
#3078=FACE_OUTER_BOUND('',#4391,.T.);
#3079=FACE_OUTER_BOUND('',#4392,.T.);
#3080=FACE_OUTER_BOUND('',#4393,.T.);
#3081=FACE_OUTER_BOUND('',#4394,.T.);
#3082=FACE_OUTER_BOUND('',#4395,.T.);
#3083=FACE_OUTER_BOUND('',#4396,.T.);
#3084=FACE_OUTER_BOUND('',#4397,.T.);
#3085=FACE_OUTER_BOUND('',#4398,.T.);
#3086=FACE_OUTER_BOUND('',#4399,.T.);
#3087=FACE_OUTER_BOUND('',#4400,.T.);
#3088=FACE_OUTER_BOUND('',#4401,.T.);
#3089=FACE_OUTER_BOUND('',#4402,.T.);
#3090=FACE_OUTER_BOUND('',#4403,.T.);
#3091=FACE_OUTER_BOUND('',#4404,.T.);
#3092=FACE_OUTER_BOUND('',#4405,.T.);
#3093=FACE_OUTER_BOUND('',#4406,.T.);
#3094=FACE_OUTER_BOUND('',#4407,.T.);
#3095=FACE_OUTER_BOUND('',#4408,.T.);
#3096=FACE_OUTER_BOUND('',#4409,.T.);
#3097=FACE_OUTER_BOUND('',#4410,.T.);
#3098=FACE_OUTER_BOUND('',#4411,.T.);
#3099=FACE_OUTER_BOUND('',#4412,.T.);
#3100=FACE_OUTER_BOUND('',#4413,.T.);
#3101=FACE_OUTER_BOUND('',#4414,.T.);
#3102=FACE_OUTER_BOUND('',#4415,.T.);
#3103=FACE_OUTER_BOUND('',#4416,.T.);
#3104=FACE_OUTER_BOUND('',#4417,.T.);
#3105=FACE_OUTER_BOUND('',#4418,.T.);
#3106=FACE_OUTER_BOUND('',#4419,.T.);
#3107=FACE_OUTER_BOUND('',#4420,.T.);
#3108=FACE_OUTER_BOUND('',#4421,.T.);
#3109=FACE_OUTER_BOUND('',#4422,.T.);
#3110=FACE_OUTER_BOUND('',#4423,.T.);
#3111=FACE_OUTER_BOUND('',#4424,.T.);
#3112=FACE_OUTER_BOUND('',#4425,.T.);
#3113=FACE_OUTER_BOUND('',#4426,.T.);
#3114=FACE_OUTER_BOUND('',#4427,.T.);
#3115=FACE_OUTER_BOUND('',#4428,.T.);
#3116=FACE_OUTER_BOUND('',#4429,.T.);
#3117=FACE_OUTER_BOUND('',#4430,.T.);
#3118=FACE_OUTER_BOUND('',#4431,.T.);
#3119=FACE_OUTER_BOUND('',#4432,.T.);
#3120=FACE_OUTER_BOUND('',#4433,.T.);
#3121=FACE_OUTER_BOUND('',#4434,.T.);
#3122=FACE_OUTER_BOUND('',#4435,.T.);
#3123=FACE_OUTER_BOUND('',#4436,.T.);
#3124=FACE_OUTER_BOUND('',#4437,.T.);
#3125=FACE_OUTER_BOUND('',#4438,.T.);
#3126=FACE_OUTER_BOUND('',#4439,.T.);
#3127=FACE_OUTER_BOUND('',#4440,.T.);
#3128=FACE_OUTER_BOUND('',#4441,.T.);
#3129=FACE_OUTER_BOUND('',#4442,.T.);
#3130=FACE_OUTER_BOUND('',#4443,.T.);
#3131=FACE_OUTER_BOUND('',#4444,.T.);
#3132=FACE_OUTER_BOUND('',#4445,.T.);
#3133=FACE_OUTER_BOUND('',#4446,.T.);
#3134=FACE_OUTER_BOUND('',#4447,.T.);
#3135=FACE_OUTER_BOUND('',#4448,.T.);
#3136=FACE_OUTER_BOUND('',#4449,.T.);
#3137=FACE_OUTER_BOUND('',#4450,.T.);
#3138=FACE_OUTER_BOUND('',#4451,.T.);
#3139=FACE_OUTER_BOUND('',#4452,.T.);
#3140=FACE_OUTER_BOUND('',#4453,.T.);
#3141=FACE_OUTER_BOUND('',#4454,.T.);
#3142=FACE_OUTER_BOUND('',#4455,.T.);
#3143=FACE_OUTER_BOUND('',#4456,.T.);
#3144=FACE_OUTER_BOUND('',#4457,.T.);
#3145=FACE_OUTER_BOUND('',#4458,.T.);
#3146=FACE_OUTER_BOUND('',#4459,.T.);
#3147=FACE_OUTER_BOUND('',#4460,.T.);
#3148=FACE_OUTER_BOUND('',#4461,.T.);
#3149=FACE_OUTER_BOUND('',#4462,.T.);
#3150=FACE_OUTER_BOUND('',#4463,.T.);
#3151=FACE_OUTER_BOUND('',#4464,.T.);
#3152=FACE_OUTER_BOUND('',#4465,.T.);
#3153=FACE_OUTER_BOUND('',#4466,.T.);
#3154=FACE_OUTER_BOUND('',#4467,.T.);
#3155=FACE_OUTER_BOUND('',#4468,.T.);
#3156=FACE_OUTER_BOUND('',#4469,.T.);
#3157=FACE_OUTER_BOUND('',#4470,.T.);
#3158=FACE_OUTER_BOUND('',#4471,.T.);
#3159=FACE_OUTER_BOUND('',#4472,.T.);
#3160=FACE_OUTER_BOUND('',#4473,.T.);
#3161=FACE_OUTER_BOUND('',#4474,.T.);
#3162=FACE_OUTER_BOUND('',#4475,.T.);
#3163=FACE_OUTER_BOUND('',#4476,.T.);
#3164=FACE_OUTER_BOUND('',#4477,.T.);
#3165=FACE_OUTER_BOUND('',#4478,.T.);
#3166=FACE_OUTER_BOUND('',#4479,.T.);
#3167=FACE_OUTER_BOUND('',#4480,.T.);
#3168=FACE_OUTER_BOUND('',#4481,.T.);
#3169=FACE_OUTER_BOUND('',#4482,.T.);
#3170=FACE_OUTER_BOUND('',#4483,.T.);
#3171=FACE_OUTER_BOUND('',#4484,.T.);
#3172=FACE_OUTER_BOUND('',#4485,.T.);
#3173=FACE_OUTER_BOUND('',#4486,.T.);
#3174=FACE_OUTER_BOUND('',#4487,.T.);
#3175=FACE_OUTER_BOUND('',#4488,.T.);
#3176=FACE_OUTER_BOUND('',#4489,.T.);
#3177=FACE_OUTER_BOUND('',#4490,.T.);
#3178=FACE_OUTER_BOUND('',#4491,.T.);
#3179=FACE_OUTER_BOUND('',#4492,.T.);
#3180=FACE_OUTER_BOUND('',#4493,.T.);
#3181=FACE_OUTER_BOUND('',#4494,.T.);
#3182=FACE_OUTER_BOUND('',#4495,.T.);
#3183=FACE_OUTER_BOUND('',#4496,.T.);
#3184=FACE_OUTER_BOUND('',#4497,.T.);
#3185=FACE_OUTER_BOUND('',#4498,.T.);
#3186=FACE_OUTER_BOUND('',#4499,.T.);
#3187=FACE_OUTER_BOUND('',#4500,.T.);
#3188=FACE_OUTER_BOUND('',#4501,.T.);
#3189=FACE_OUTER_BOUND('',#4502,.T.);
#3190=FACE_OUTER_BOUND('',#4503,.T.);
#3191=FACE_OUTER_BOUND('',#4504,.T.);
#3192=FACE_OUTER_BOUND('',#4505,.T.);
#3193=FACE_OUTER_BOUND('',#4506,.T.);
#3194=FACE_OUTER_BOUND('',#4507,.T.);
#3195=FACE_OUTER_BOUND('',#4508,.T.);
#3196=FACE_OUTER_BOUND('',#4509,.T.);
#3197=FACE_OUTER_BOUND('',#4510,.T.);
#3198=FACE_OUTER_BOUND('',#4511,.T.);
#3199=FACE_OUTER_BOUND('',#4512,.T.);
#3200=FACE_OUTER_BOUND('',#4513,.T.);
#3201=FACE_OUTER_BOUND('',#4514,.T.);
#3202=FACE_OUTER_BOUND('',#4515,.T.);
#3203=FACE_OUTER_BOUND('',#4516,.T.);
#3204=FACE_OUTER_BOUND('',#4517,.T.);
#3205=FACE_OUTER_BOUND('',#4518,.T.);
#3206=FACE_OUTER_BOUND('',#4519,.T.);
#3207=FACE_OUTER_BOUND('',#4520,.T.);
#3208=FACE_OUTER_BOUND('',#4521,.T.);
#3209=FACE_OUTER_BOUND('',#4522,.T.);
#3210=FACE_OUTER_BOUND('',#4523,.T.);
#3211=FACE_OUTER_BOUND('',#4524,.T.);
#3212=FACE_OUTER_BOUND('',#4525,.T.);
#3213=FACE_OUTER_BOUND('',#4526,.T.);
#3214=FACE_OUTER_BOUND('',#4527,.T.);
#3215=FACE_OUTER_BOUND('',#4528,.T.);
#3216=FACE_OUTER_BOUND('',#4529,.T.);
#3217=FACE_OUTER_BOUND('',#4530,.T.);
#3218=FACE_OUTER_BOUND('',#4531,.T.);
#3219=FACE_OUTER_BOUND('',#4532,.T.);
#3220=FACE_OUTER_BOUND('',#4533,.T.);
#3221=FACE_OUTER_BOUND('',#4534,.T.);
#3222=FACE_OUTER_BOUND('',#4535,.T.);
#3223=FACE_OUTER_BOUND('',#4536,.T.);
#3224=FACE_OUTER_BOUND('',#4537,.T.);
#3225=FACE_OUTER_BOUND('',#4538,.T.);
#3226=FACE_OUTER_BOUND('',#4539,.T.);
#3227=FACE_OUTER_BOUND('',#4540,.T.);
#3228=FACE_OUTER_BOUND('',#4541,.T.);
#3229=FACE_OUTER_BOUND('',#4542,.T.);
#3230=FACE_OUTER_BOUND('',#4543,.T.);
#3231=FACE_OUTER_BOUND('',#4544,.T.);
#3232=FACE_OUTER_BOUND('',#4545,.T.);
#3233=FACE_OUTER_BOUND('',#4546,.T.);
#3234=FACE_OUTER_BOUND('',#4547,.T.);
#3235=FACE_OUTER_BOUND('',#4548,.T.);
#3236=FACE_OUTER_BOUND('',#4549,.T.);
#3237=FACE_OUTER_BOUND('',#4550,.T.);
#3238=FACE_OUTER_BOUND('',#4551,.T.);
#3239=FACE_OUTER_BOUND('',#4552,.T.);
#3240=FACE_OUTER_BOUND('',#4553,.T.);
#3241=FACE_OUTER_BOUND('',#4554,.T.);
#3242=FACE_OUTER_BOUND('',#4555,.T.);
#3243=FACE_OUTER_BOUND('',#4556,.T.);
#3244=FACE_OUTER_BOUND('',#4557,.T.);
#3245=FACE_OUTER_BOUND('',#4558,.T.);
#3246=FACE_OUTER_BOUND('',#4559,.T.);
#3247=FACE_OUTER_BOUND('',#4560,.T.);
#3248=FACE_OUTER_BOUND('',#4561,.T.);
#3249=FACE_OUTER_BOUND('',#4562,.T.);
#3250=FACE_OUTER_BOUND('',#4563,.T.);
#3251=FACE_OUTER_BOUND('',#4564,.T.);
#3252=FACE_OUTER_BOUND('',#4565,.T.);
#3253=FACE_OUTER_BOUND('',#4566,.T.);
#3254=FACE_OUTER_BOUND('',#4567,.T.);
#3255=FACE_OUTER_BOUND('',#4568,.T.);
#3256=FACE_OUTER_BOUND('',#4569,.T.);
#3257=FACE_OUTER_BOUND('',#4570,.T.);
#3258=FACE_OUTER_BOUND('',#4571,.T.);
#3259=FACE_OUTER_BOUND('',#4572,.T.);
#3260=FACE_OUTER_BOUND('',#4573,.T.);
#3261=FACE_OUTER_BOUND('',#4574,.T.);
#3262=FACE_OUTER_BOUND('',#4575,.T.);
#3263=FACE_OUTER_BOUND('',#4576,.T.);
#3264=FACE_OUTER_BOUND('',#4577,.T.);
#3265=FACE_OUTER_BOUND('',#4578,.T.);
#3266=FACE_OUTER_BOUND('',#4579,.T.);
#3267=FACE_OUTER_BOUND('',#4580,.T.);
#3268=FACE_OUTER_BOUND('',#4581,.T.);
#3269=FACE_OUTER_BOUND('',#4582,.T.);
#3270=FACE_OUTER_BOUND('',#4583,.T.);
#3271=FACE_OUTER_BOUND('',#4584,.T.);
#3272=FACE_OUTER_BOUND('',#4585,.T.);
#3273=FACE_OUTER_BOUND('',#4586,.T.);
#3274=FACE_OUTER_BOUND('',#4587,.T.);
#3275=FACE_OUTER_BOUND('',#4588,.T.);
#3276=FACE_OUTER_BOUND('',#4589,.T.);
#3277=FACE_OUTER_BOUND('',#4599,.T.);
#3278=FACE_OUTER_BOUND('',#4600,.T.);
#3279=FACE_OUTER_BOUND('',#4601,.T.);
#3280=FACE_OUTER_BOUND('',#4602,.T.);
#3281=FACE_OUTER_BOUND('',#4603,.T.);
#3282=FACE_OUTER_BOUND('',#4604,.T.);
#3283=FACE_OUTER_BOUND('',#4605,.T.);
#3284=FACE_OUTER_BOUND('',#4606,.T.);
#3285=FACE_OUTER_BOUND('',#4607,.T.);
#3286=FACE_OUTER_BOUND('',#4608,.T.);
#3287=FACE_OUTER_BOUND('',#4609,.T.);
#3288=FACE_OUTER_BOUND('',#4610,.T.);
#3289=FACE_OUTER_BOUND('',#4611,.T.);
#3290=FACE_OUTER_BOUND('',#4612,.T.);
#3291=FACE_OUTER_BOUND('',#4613,.T.);
#3292=FACE_OUTER_BOUND('',#4614,.T.);
#3293=FACE_OUTER_BOUND('',#4615,.T.);
#3294=FACE_OUTER_BOUND('',#4616,.T.);
#3295=FACE_OUTER_BOUND('',#4617,.T.);
#3296=FACE_OUTER_BOUND('',#4618,.T.);
#3297=FACE_OUTER_BOUND('',#4619,.T.);
#3298=FACE_OUTER_BOUND('',#4621,.T.);
#3299=FACE_OUTER_BOUND('',#4622,.T.);
#3300=FACE_OUTER_BOUND('',#4623,.T.);
#3301=FACE_OUTER_BOUND('',#4624,.T.);
#3302=FACE_OUTER_BOUND('',#4625,.T.);
#3303=FACE_OUTER_BOUND('',#4626,.T.);
#3304=FACE_OUTER_BOUND('',#4630,.T.);
#3305=FACE_OUTER_BOUND('',#4631,.T.);
#3306=FACE_OUTER_BOUND('',#4632,.T.);
#3307=FACE_OUTER_BOUND('',#4633,.T.);
#3308=FACE_OUTER_BOUND('',#4634,.T.);
#3309=FACE_OUTER_BOUND('',#4635,.T.);
#3310=FACE_OUTER_BOUND('',#4636,.T.);
#3311=FACE_OUTER_BOUND('',#4637,.T.);
#3312=FACE_OUTER_BOUND('',#4638,.T.);
#3313=FACE_OUTER_BOUND('',#4640,.T.);
#3314=FACE_OUTER_BOUND('',#4641,.T.);
#3315=FACE_OUTER_BOUND('',#4642,.T.);
#3316=FACE_OUTER_BOUND('',#4643,.T.);
#3317=FACE_OUTER_BOUND('',#4644,.T.);
#3318=FACE_OUTER_BOUND('',#4645,.T.);
#3319=FACE_OUTER_BOUND('',#4646,.T.);
#3320=FACE_OUTER_BOUND('',#4647,.T.);
#3321=FACE_OUTER_BOUND('',#4648,.T.);
#3322=FACE_OUTER_BOUND('',#4649,.T.);
#3323=FACE_OUTER_BOUND('',#4650,.T.);
#3324=FACE_OUTER_BOUND('',#4651,.T.);
#3325=FACE_OUTER_BOUND('',#4652,.T.);
#3326=FACE_OUTER_BOUND('',#4656,.T.);
#3327=FACE_OUTER_BOUND('',#4657,.T.);
#3328=FACE_OUTER_BOUND('',#4658,.T.);
#3329=FACE_OUTER_BOUND('',#4659,.T.);
#3330=FACE_OUTER_BOUND('',#4660,.T.);
#3331=FACE_OUTER_BOUND('',#4661,.T.);
#3332=FACE_OUTER_BOUND('',#4662,.T.);
#3333=FACE_OUTER_BOUND('',#4663,.T.);
#3334=FACE_OUTER_BOUND('',#4664,.T.);
#3335=FACE_OUTER_BOUND('',#4666,.T.);
#3336=FACE_OUTER_BOUND('',#4667,.T.);
#3337=FACE_OUTER_BOUND('',#4668,.T.);
#3338=FACE_OUTER_BOUND('',#4669,.T.);
#3339=FACE_OUTER_BOUND('',#4670,.T.);
#3340=FACE_OUTER_BOUND('',#4671,.T.);
#3341=FACE_OUTER_BOUND('',#4672,.T.);
#3342=FACE_OUTER_BOUND('',#4673,.T.);
#3343=FACE_OUTER_BOUND('',#4674,.T.);
#3344=FACE_OUTER_BOUND('',#4676,.T.);
#3345=FACE_OUTER_BOUND('',#4677,.T.);
#3346=FACE_OUTER_BOUND('',#4678,.T.);
#3347=FACE_OUTER_BOUND('',#4681,.T.);
#3348=FACE_OUTER_BOUND('',#4682,.T.);
#3349=FACE_OUTER_BOUND('',#4683,.T.);
#3350=FACE_OUTER_BOUND('',#4684,.T.);
#3351=FACE_OUTER_BOUND('',#4685,.T.);
#3352=FACE_OUTER_BOUND('',#4686,.T.);
#3353=FACE_OUTER_BOUND('',#4687,.T.);
#3354=FACE_OUTER_BOUND('',#4688,.T.);
#3355=FACE_OUTER_BOUND('',#4689,.T.);
#3356=FACE_OUTER_BOUND('',#4690,.T.);
#3357=FACE_OUTER_BOUND('',#4691,.T.);
#3358=FACE_OUTER_BOUND('',#4692,.T.);
#3359=FACE_OUTER_BOUND('',#4693,.T.);
#3360=FACE_OUTER_BOUND('',#4694,.T.);
#3361=FACE_OUTER_BOUND('',#4695,.T.);
#3362=FACE_OUTER_BOUND('',#4696,.T.);
#3363=FACE_OUTER_BOUND('',#4697,.T.);
#3364=FACE_OUTER_BOUND('',#4698,.T.);
#3365=FACE_OUTER_BOUND('',#4699,.T.);
#3366=FACE_OUTER_BOUND('',#4700,.T.);
#3367=FACE_OUTER_BOUND('',#4701,.T.);
#3368=FACE_OUTER_BOUND('',#4702,.T.);
#3369=FACE_OUTER_BOUND('',#4705,.T.);
#3370=FACE_OUTER_BOUND('',#4706,.T.);
#3371=FACE_OUTER_BOUND('',#4707,.T.);
#3372=FACE_OUTER_BOUND('',#4708,.T.);
#3373=FACE_OUTER_BOUND('',#4709,.T.);
#3374=FACE_OUTER_BOUND('',#4710,.T.);
#3375=FACE_OUTER_BOUND('',#4711,.T.);
#3376=FACE_OUTER_BOUND('',#4712,.T.);
#3377=FACE_OUTER_BOUND('',#4713,.T.);
#3378=FACE_OUTER_BOUND('',#4714,.T.);
#3379=FACE_OUTER_BOUND('',#4719,.T.);
#3380=FACE_OUTER_BOUND('',#4720,.T.);
#3381=FACE_OUTER_BOUND('',#4721,.T.);
#3382=FACE_OUTER_BOUND('',#4722,.T.);
#3383=FACE_OUTER_BOUND('',#4723,.T.);
#3384=FACE_OUTER_BOUND('',#4724,.T.);
#3385=FACE_OUTER_BOUND('',#4725,.T.);
#3386=FACE_OUTER_BOUND('',#4726,.T.);
#3387=FACE_OUTER_BOUND('',#4727,.T.);
#3388=FACE_OUTER_BOUND('',#4728,.T.);
#3389=FACE_OUTER_BOUND('',#4729,.T.);
#3390=FACE_OUTER_BOUND('',#4730,.T.);
#3391=FACE_OUTER_BOUND('',#4731,.T.);
#3392=FACE_OUTER_BOUND('',#4732,.T.);
#3393=FACE_OUTER_BOUND('',#4733,.T.);
#3394=FACE_OUTER_BOUND('',#4734,.T.);
#3395=FACE_OUTER_BOUND('',#4735,.T.);
#3396=FACE_OUTER_BOUND('',#4736,.T.);
#3397=FACE_OUTER_BOUND('',#4737,.T.);
#3398=FACE_OUTER_BOUND('',#4738,.T.);
#3399=FACE_OUTER_BOUND('',#4739,.T.);
#3400=FACE_OUTER_BOUND('',#4740,.T.);
#3401=FACE_OUTER_BOUND('',#4741,.T.);
#3402=FACE_OUTER_BOUND('',#4742,.T.);
#3403=FACE_OUTER_BOUND('',#4743,.T.);
#3404=FACE_OUTER_BOUND('',#4744,.T.);
#3405=FACE_OUTER_BOUND('',#4745,.T.);
#3406=FACE_OUTER_BOUND('',#4746,.T.);
#3407=FACE_OUTER_BOUND('',#4747,.T.);
#3408=FACE_OUTER_BOUND('',#4748,.T.);
#3409=FACE_OUTER_BOUND('',#4749,.T.);
#3410=FACE_OUTER_BOUND('',#4750,.T.);
#3411=FACE_OUTER_BOUND('',#4751,.T.);
#3412=FACE_OUTER_BOUND('',#4752,.T.);
#3413=FACE_OUTER_BOUND('',#4753,.T.);
#3414=FACE_OUTER_BOUND('',#4754,.T.);
#3415=FACE_OUTER_BOUND('',#4755,.T.);
#3416=FACE_OUTER_BOUND('',#4756,.T.);
#3417=FACE_OUTER_BOUND('',#4757,.T.);
#3418=FACE_OUTER_BOUND('',#4758,.T.);
#3419=FACE_OUTER_BOUND('',#4759,.T.);
#3420=FACE_OUTER_BOUND('',#4760,.T.);
#3421=FACE_OUTER_BOUND('',#4761,.T.);
#3422=FACE_OUTER_BOUND('',#4762,.T.);
#3423=FACE_OUTER_BOUND('',#4763,.T.);
#3424=FACE_OUTER_BOUND('',#4765,.T.);
#3425=FACE_OUTER_BOUND('',#4766,.T.);
#3426=FACE_OUTER_BOUND('',#4767,.T.);
#3427=FACE_OUTER_BOUND('',#4768,.T.);
#3428=FACE_OUTER_BOUND('',#4769,.T.);
#3429=FACE_OUTER_BOUND('',#4770,.T.);
#3430=FACE_OUTER_BOUND('',#4771,.T.);
#3431=FACE_OUTER_BOUND('',#4772,.T.);
#3432=FACE_OUTER_BOUND('',#4773,.T.);
#3433=FACE_OUTER_BOUND('',#4774,.T.);
#3434=FACE_OUTER_BOUND('',#4775,.T.);
#3435=FACE_OUTER_BOUND('',#4776,.T.);
#3436=FACE_OUTER_BOUND('',#4777,.T.);
#3437=FACE_OUTER_BOUND('',#4778,.T.);
#3438=FACE_OUTER_BOUND('',#4779,.T.);
#3439=FACE_OUTER_BOUND('',#4780,.T.);
#3440=FACE_OUTER_BOUND('',#4781,.T.);
#3441=FACE_OUTER_BOUND('',#4782,.T.);
#3442=FACE_OUTER_BOUND('',#4783,.T.);
#3443=FACE_OUTER_BOUND('',#4784,.T.);
#3444=FACE_OUTER_BOUND('',#4785,.T.);
#3445=FACE_OUTER_BOUND('',#4786,.T.);
#3446=FACE_OUTER_BOUND('',#4787,.T.);
#3447=FACE_OUTER_BOUND('',#4788,.T.);
#3448=FACE_OUTER_BOUND('',#4789,.T.);
#3449=FACE_OUTER_BOUND('',#4790,.T.);
#3450=FACE_OUTER_BOUND('',#4791,.T.);
#3451=FACE_OUTER_BOUND('',#4792,.T.);
#3452=FACE_OUTER_BOUND('',#4793,.T.);
#3453=FACE_OUTER_BOUND('',#4794,.T.);
#3454=FACE_OUTER_BOUND('',#4795,.T.);
#3455=FACE_OUTER_BOUND('',#4796,.T.);
#3456=FACE_OUTER_BOUND('',#4797,.T.);
#3457=FACE_OUTER_BOUND('',#4798,.T.);
#3458=FACE_OUTER_BOUND('',#4799,.T.);
#3459=FACE_OUTER_BOUND('',#4800,.T.);
#3460=FACE_OUTER_BOUND('',#4801,.T.);
#3461=FACE_OUTER_BOUND('',#4802,.T.);
#3462=FACE_OUTER_BOUND('',#4803,.T.);
#3463=FACE_OUTER_BOUND('',#4804,.T.);
#3464=FACE_OUTER_BOUND('',#4805,.T.);
#3465=FACE_OUTER_BOUND('',#4806,.T.);
#3466=FACE_OUTER_BOUND('',#4807,.T.);
#3467=FACE_OUTER_BOUND('',#4808,.T.);
#3468=FACE_OUTER_BOUND('',#4809,.T.);
#3469=FACE_OUTER_BOUND('',#4810,.T.);
#3470=FACE_OUTER_BOUND('',#4811,.T.);
#3471=FACE_OUTER_BOUND('',#4812,.T.);
#3472=FACE_OUTER_BOUND('',#4813,.T.);
#3473=FACE_OUTER_BOUND('',#4814,.T.);
#3474=FACE_OUTER_BOUND('',#4815,.T.);
#3475=FACE_OUTER_BOUND('',#4816,.T.);
#3476=FACE_OUTER_BOUND('',#4817,.T.);
#3477=FACE_OUTER_BOUND('',#4818,.T.);
#3478=FACE_OUTER_BOUND('',#4820,.T.);
#3479=FACE_OUTER_BOUND('',#4821,.T.);
#3480=FACE_OUTER_BOUND('',#4822,.T.);
#3481=FACE_OUTER_BOUND('',#4823,.T.);
#3482=FACE_OUTER_BOUND('',#4824,.T.);
#3483=FACE_OUTER_BOUND('',#4825,.T.);
#3484=FACE_OUTER_BOUND('',#4826,.T.);
#3485=FACE_OUTER_BOUND('',#4827,.T.);
#3486=FACE_OUTER_BOUND('',#4828,.T.);
#3487=FACE_OUTER_BOUND('',#4829,.T.);
#3488=FACE_OUTER_BOUND('',#4830,.T.);
#3489=FACE_OUTER_BOUND('',#4831,.T.);
#3490=FACE_OUTER_BOUND('',#4832,.T.);
#3491=FACE_OUTER_BOUND('',#4833,.T.);
#3492=FACE_OUTER_BOUND('',#4834,.T.);
#3493=FACE_OUTER_BOUND('',#4835,.T.);
#3494=FACE_OUTER_BOUND('',#4836,.T.);
#3495=FACE_OUTER_BOUND('',#4837,.T.);
#3496=FACE_OUTER_BOUND('',#4838,.T.);
#3497=FACE_OUTER_BOUND('',#4839,.T.);
#3498=FACE_OUTER_BOUND('',#4840,.T.);
#3499=FACE_OUTER_BOUND('',#4841,.T.);
#3500=FACE_OUTER_BOUND('',#4842,.T.);
#3501=FACE_OUTER_BOUND('',#4843,.T.);
#3502=FACE_OUTER_BOUND('',#4844,.T.);
#3503=FACE_OUTER_BOUND('',#4845,.T.);
#3504=FACE_OUTER_BOUND('',#4846,.T.);
#3505=FACE_OUTER_BOUND('',#4847,.T.);
#3506=FACE_OUTER_BOUND('',#4848,.T.);
#3507=FACE_OUTER_BOUND('',#4849,.T.);
#3508=FACE_OUTER_BOUND('',#4850,.T.);
#3509=FACE_OUTER_BOUND('',#4851,.T.);
#3510=FACE_OUTER_BOUND('',#4852,.T.);
#3511=FACE_OUTER_BOUND('',#4853,.T.);
#3512=FACE_OUTER_BOUND('',#4854,.T.);
#3513=FACE_OUTER_BOUND('',#4855,.T.);
#3514=FACE_OUTER_BOUND('',#4856,.T.);
#3515=FACE_OUTER_BOUND('',#4857,.T.);
#3516=FACE_OUTER_BOUND('',#4858,.T.);
#3517=FACE_OUTER_BOUND('',#4859,.T.);
#3518=FACE_OUTER_BOUND('',#4860,.T.);
#3519=FACE_OUTER_BOUND('',#4861,.T.);
#3520=FACE_OUTER_BOUND('',#4862,.T.);
#3521=FACE_OUTER_BOUND('',#4863,.T.);
#3522=FACE_OUTER_BOUND('',#4864,.T.);
#3523=FACE_OUTER_BOUND('',#4865,.T.);
#3524=FACE_OUTER_BOUND('',#4866,.T.);
#3525=FACE_OUTER_BOUND('',#4867,.T.);
#3526=FACE_OUTER_BOUND('',#4868,.T.);
#3527=FACE_OUTER_BOUND('',#4869,.T.);
#3528=FACE_OUTER_BOUND('',#4870,.T.);
#3529=FACE_OUTER_BOUND('',#4871,.T.);
#3530=FACE_OUTER_BOUND('',#4872,.T.);
#3531=FACE_OUTER_BOUND('',#4873,.T.);
#3532=FACE_OUTER_BOUND('',#4874,.T.);
#3533=FACE_OUTER_BOUND('',#4875,.T.);
#3534=FACE_OUTER_BOUND('',#4877,.T.);
#3535=FACE_OUTER_BOUND('',#4878,.T.);
#3536=FACE_OUTER_BOUND('',#4879,.T.);
#3537=FACE_OUTER_BOUND('',#4880,.T.);
#3538=FACE_OUTER_BOUND('',#4881,.T.);
#3539=FACE_OUTER_BOUND('',#4882,.T.);
#3540=FACE_OUTER_BOUND('',#4883,.T.);
#3541=FACE_OUTER_BOUND('',#4884,.T.);
#3542=FACE_OUTER_BOUND('',#4885,.T.);
#3543=FACE_OUTER_BOUND('',#4886,.T.);
#3544=FACE_OUTER_BOUND('',#4887,.T.);
#3545=FACE_OUTER_BOUND('',#4888,.T.);
#3546=FACE_OUTER_BOUND('',#4889,.T.);
#3547=FACE_OUTER_BOUND('',#4890,.T.);
#3548=FACE_OUTER_BOUND('',#4891,.T.);
#3549=FACE_OUTER_BOUND('',#4892,.T.);
#3550=FACE_OUTER_BOUND('',#4893,.T.);
#3551=FACE_OUTER_BOUND('',#4894,.T.);
#3552=FACE_OUTER_BOUND('',#4895,.T.);
#3553=FACE_OUTER_BOUND('',#4896,.T.);
#3554=FACE_OUTER_BOUND('',#4897,.T.);
#3555=FACE_OUTER_BOUND('',#4898,.T.);
#3556=FACE_OUTER_BOUND('',#4899,.T.);
#3557=FACE_OUTER_BOUND('',#4900,.T.);
#3558=FACE_OUTER_BOUND('',#4901,.T.);
#3559=FACE_OUTER_BOUND('',#4902,.T.);
#3560=FACE_OUTER_BOUND('',#4903,.T.);
#3561=FACE_OUTER_BOUND('',#4904,.T.);
#3562=FACE_OUTER_BOUND('',#4905,.T.);
#3563=FACE_OUTER_BOUND('',#4906,.T.);
#3564=FACE_OUTER_BOUND('',#4907,.T.);
#3565=FACE_OUTER_BOUND('',#4908,.T.);
#3566=FACE_OUTER_BOUND('',#4909,.T.);
#3567=FACE_OUTER_BOUND('',#4910,.T.);
#3568=FACE_OUTER_BOUND('',#4911,.T.);
#3569=FACE_OUTER_BOUND('',#4912,.T.);
#3570=FACE_OUTER_BOUND('',#4913,.T.);
#3571=FACE_OUTER_BOUND('',#4914,.T.);
#3572=FACE_OUTER_BOUND('',#4915,.T.);
#3573=FACE_OUTER_BOUND('',#4916,.T.);
#3574=FACE_OUTER_BOUND('',#4917,.T.);
#3575=FACE_OUTER_BOUND('',#4918,.T.);
#3576=FACE_OUTER_BOUND('',#4919,.T.);
#3577=FACE_OUTER_BOUND('',#4920,.T.);
#3578=FACE_OUTER_BOUND('',#4921,.T.);
#3579=FACE_OUTER_BOUND('',#4922,.T.);
#3580=FACE_OUTER_BOUND('',#4923,.T.);
#3581=FACE_OUTER_BOUND('',#4924,.T.);
#3582=FACE_OUTER_BOUND('',#4925,.T.);
#3583=FACE_OUTER_BOUND('',#4926,.T.);
#3584=FACE_OUTER_BOUND('',#4927,.T.);
#3585=FACE_OUTER_BOUND('',#4928,.T.);
#3586=FACE_OUTER_BOUND('',#4929,.T.);
#3587=FACE_OUTER_BOUND('',#4930,.T.);
#3588=FACE_OUTER_BOUND('',#4932,.T.);
#3589=FACE_OUTER_BOUND('',#4933,.T.);
#3590=FACE_OUTER_BOUND('',#4934,.T.);
#3591=FACE_OUTER_BOUND('',#4935,.T.);
#3592=FACE_OUTER_BOUND('',#4936,.T.);
#3593=FACE_OUTER_BOUND('',#4937,.T.);
#3594=FACE_OUTER_BOUND('',#4938,.T.);
#3595=FACE_OUTER_BOUND('',#4939,.T.);
#3596=FACE_OUTER_BOUND('',#4940,.T.);
#3597=FACE_OUTER_BOUND('',#4941,.T.);
#3598=FACE_OUTER_BOUND('',#4942,.T.);
#3599=FACE_OUTER_BOUND('',#4943,.T.);
#3600=FACE_OUTER_BOUND('',#4944,.T.);
#3601=FACE_OUTER_BOUND('',#4945,.T.);
#3602=FACE_OUTER_BOUND('',#4946,.T.);
#3603=FACE_OUTER_BOUND('',#4947,.T.);
#3604=FACE_OUTER_BOUND('',#4948,.T.);
#3605=FACE_OUTER_BOUND('',#4949,.T.);
#3606=FACE_OUTER_BOUND('',#4950,.T.);
#3607=FACE_OUTER_BOUND('',#4951,.T.);
#3608=FACE_OUTER_BOUND('',#4952,.T.);
#3609=FACE_OUTER_BOUND('',#4953,.T.);
#3610=FACE_OUTER_BOUND('',#4954,.T.);
#3611=FACE_OUTER_BOUND('',#4955,.T.);
#3612=FACE_OUTER_BOUND('',#4956,.T.);
#3613=FACE_OUTER_BOUND('',#4957,.T.);
#3614=FACE_OUTER_BOUND('',#4958,.T.);
#3615=FACE_OUTER_BOUND('',#4959,.T.);
#3616=FACE_OUTER_BOUND('',#4960,.T.);
#3617=FACE_OUTER_BOUND('',#4961,.T.);
#3618=FACE_OUTER_BOUND('',#4962,.T.);
#3619=FACE_OUTER_BOUND('',#4963,.T.);
#3620=FACE_OUTER_BOUND('',#4964,.T.);
#3621=FACE_OUTER_BOUND('',#4965,.T.);
#3622=FACE_OUTER_BOUND('',#4966,.T.);
#3623=FACE_OUTER_BOUND('',#4967,.T.);
#3624=FACE_OUTER_BOUND('',#4968,.T.);
#3625=FACE_OUTER_BOUND('',#4969,.T.);
#3626=FACE_OUTER_BOUND('',#4970,.T.);
#3627=FACE_OUTER_BOUND('',#4971,.T.);
#3628=FACE_OUTER_BOUND('',#4972,.T.);
#3629=FACE_OUTER_BOUND('',#4973,.T.);
#3630=FACE_OUTER_BOUND('',#4974,.T.);
#3631=FACE_OUTER_BOUND('',#4975,.T.);
#3632=FACE_OUTER_BOUND('',#4976,.T.);
#3633=FACE_OUTER_BOUND('',#4977,.T.);
#3634=FACE_OUTER_BOUND('',#4978,.T.);
#3635=FACE_OUTER_BOUND('',#4979,.T.);
#3636=FACE_OUTER_BOUND('',#4980,.T.);
#3637=FACE_OUTER_BOUND('',#4981,.T.);
#3638=FACE_OUTER_BOUND('',#4982,.T.);
#3639=FACE_OUTER_BOUND('',#4983,.T.);
#3640=FACE_OUTER_BOUND('',#4984,.T.);
#3641=FACE_OUTER_BOUND('',#4985,.T.);
#3642=FACE_OUTER_BOUND('',#4986,.T.);
#3643=FACE_OUTER_BOUND('',#4987,.T.);
#3644=FACE_OUTER_BOUND('',#4988,.T.);
#3645=FACE_OUTER_BOUND('',#4989,.T.);
#3646=FACE_OUTER_BOUND('',#4990,.T.);
#3647=FACE_OUTER_BOUND('',#4991,.T.);
#3648=FACE_OUTER_BOUND('',#4992,.T.);
#3649=FACE_OUTER_BOUND('',#4993,.T.);
#3650=FACE_OUTER_BOUND('',#4994,.T.);
#3651=FACE_OUTER_BOUND('',#4995,.T.);
#3652=FACE_OUTER_BOUND('',#4996,.T.);
#3653=FACE_OUTER_BOUND('',#4997,.T.);
#3654=FACE_OUTER_BOUND('',#4998,.T.);
#3655=FACE_OUTER_BOUND('',#4999,.T.);
#3656=FACE_OUTER_BOUND('',#5000,.T.);
#3657=FACE_OUTER_BOUND('',#5001,.T.);
#3658=FACE_OUTER_BOUND('',#5002,.T.);
#3659=FACE_OUTER_BOUND('',#5003,.T.);
#3660=FACE_OUTER_BOUND('',#5004,.T.);
#3661=FACE_OUTER_BOUND('',#5005,.T.);
#3662=FACE_OUTER_BOUND('',#5006,.T.);
#3663=FACE_OUTER_BOUND('',#5007,.T.);
#3664=FACE_OUTER_BOUND('',#5008,.T.);
#3665=FACE_OUTER_BOUND('',#5009,.T.);
#3666=FACE_OUTER_BOUND('',#5010,.T.);
#3667=FACE_OUTER_BOUND('',#5011,.T.);
#3668=FACE_OUTER_BOUND('',#5012,.T.);
#3669=FACE_OUTER_BOUND('',#5013,.T.);
#3670=FACE_OUTER_BOUND('',#5014,.T.);
#3671=FACE_OUTER_BOUND('',#5015,.T.);
#3672=FACE_OUTER_BOUND('',#5016,.T.);
#3673=FACE_OUTER_BOUND('',#5017,.T.);
#3674=FACE_OUTER_BOUND('',#5018,.T.);
#3675=FACE_OUTER_BOUND('',#5019,.T.);
#3676=FACE_OUTER_BOUND('',#5020,.T.);
#3677=FACE_OUTER_BOUND('',#5021,.T.);
#3678=FACE_OUTER_BOUND('',#5022,.T.);
#3679=FACE_OUTER_BOUND('',#5023,.T.);
#3680=FACE_OUTER_BOUND('',#5024,.T.);
#3681=FACE_OUTER_BOUND('',#5025,.T.);
#3682=FACE_OUTER_BOUND('',#5026,.T.);
#3683=FACE_OUTER_BOUND('',#5027,.T.);
#3684=FACE_OUTER_BOUND('',#5028,.T.);
#3685=FACE_OUTER_BOUND('',#5029,.T.);
#3686=FACE_OUTER_BOUND('',#5030,.T.);
#3687=FACE_OUTER_BOUND('',#5031,.T.);
#3688=FACE_OUTER_BOUND('',#5032,.T.);
#3689=FACE_OUTER_BOUND('',#5033,.T.);
#3690=FACE_OUTER_BOUND('',#5034,.T.);
#3691=FACE_OUTER_BOUND('',#5035,.T.);
#3692=FACE_OUTER_BOUND('',#5036,.T.);
#3693=FACE_OUTER_BOUND('',#5037,.T.);
#3694=FACE_OUTER_BOUND('',#5038,.T.);
#3695=FACE_OUTER_BOUND('',#5039,.T.);
#3696=FACE_OUTER_BOUND('',#5040,.T.);
#3697=FACE_OUTER_BOUND('',#5041,.T.);
#3698=FACE_OUTER_BOUND('',#5042,.T.);
#3699=FACE_OUTER_BOUND('',#5043,.T.);
#3700=FACE_OUTER_BOUND('',#5044,.T.);
#3701=FACE_OUTER_BOUND('',#5045,.T.);
#3702=FACE_OUTER_BOUND('',#5049,.T.);
#3703=FACE_OUTER_BOUND('',#5050,.T.);
#3704=FACE_OUTER_BOUND('',#5051,.T.);
#3705=FACE_OUTER_BOUND('',#5052,.T.);
#3706=FACE_OUTER_BOUND('',#5053,.T.);
#3707=FACE_OUTER_BOUND('',#5054,.T.);
#3708=FACE_OUTER_BOUND('',#5058,.T.);
#3709=FACE_OUTER_BOUND('',#5059,.T.);
#3710=FACE_OUTER_BOUND('',#5060,.T.);
#3711=FACE_OUTER_BOUND('',#5061,.T.);
#3712=FACE_OUTER_BOUND('',#5065,.T.);
#3713=FACE_OUTER_BOUND('',#5066,.T.);
#3714=FACE_OUTER_BOUND('',#5067,.T.);
#3715=FACE_OUTER_BOUND('',#5068,.T.);
#3716=FACE_OUTER_BOUND('',#5069,.T.);
#3717=FACE_OUTER_BOUND('',#5070,.T.);
#3718=FACE_OUTER_BOUND('',#5071,.T.);
#3719=FACE_OUTER_BOUND('',#5072,.T.);
#3720=FACE_OUTER_BOUND('',#5073,.T.);
#3721=FACE_OUTER_BOUND('',#5074,.T.);
#3722=FACE_OUTER_BOUND('',#5075,.T.);
#3723=FACE_OUTER_BOUND('',#5076,.T.);
#3724=FACE_OUTER_BOUND('',#5077,.T.);
#3725=FACE_OUTER_BOUND('',#5078,.T.);
#3726=FACE_OUTER_BOUND('',#5079,.T.);
#3727=FACE_OUTER_BOUND('',#5080,.T.);
#3728=FACE_OUTER_BOUND('',#5081,.T.);
#3729=FACE_OUTER_BOUND('',#5082,.T.);
#3730=FACE_OUTER_BOUND('',#5083,.T.);
#3731=FACE_OUTER_BOUND('',#5084,.T.);
#3732=FACE_OUTER_BOUND('',#5085,.T.);
#3733=FACE_OUTER_BOUND('',#5086,.T.);
#3734=FACE_OUTER_BOUND('',#5087,.T.);
#3735=FACE_OUTER_BOUND('',#5088,.T.);
#3736=FACE_OUTER_BOUND('',#5092,.T.);
#3737=FACE_OUTER_BOUND('',#5093,.T.);
#3738=FACE_OUTER_BOUND('',#5094,.T.);
#3739=FACE_OUTER_BOUND('',#5095,.T.);
#3740=FACE_OUTER_BOUND('',#5096,.T.);
#3741=FACE_OUTER_BOUND('',#5097,.T.);
#3742=FACE_OUTER_BOUND('',#5098,.T.);
#3743=FACE_OUTER_BOUND('',#5099,.T.);
#3744=FACE_OUTER_BOUND('',#5100,.T.);
#3745=FACE_OUTER_BOUND('',#5101,.T.);
#3746=FACE_OUTER_BOUND('',#5102,.T.);
#3747=FACE_OUTER_BOUND('',#5103,.T.);
#3748=FACE_OUTER_BOUND('',#5104,.T.);
#3749=FACE_OUTER_BOUND('',#5105,.T.);
#3750=FACE_OUTER_BOUND('',#5106,.T.);
#3751=FACE_OUTER_BOUND('',#5107,.T.);
#3752=FACE_OUTER_BOUND('',#5108,.T.);
#3753=FACE_OUTER_BOUND('',#5109,.T.);
#3754=FACE_OUTER_BOUND('',#5110,.T.);
#3755=FACE_OUTER_BOUND('',#5111,.T.);
#3756=FACE_OUTER_BOUND('',#5112,.T.);
#3757=FACE_OUTER_BOUND('',#5113,.T.);
#3758=FACE_OUTER_BOUND('',#5114,.T.);
#3759=FACE_OUTER_BOUND('',#5115,.T.);
#3760=FACE_OUTER_BOUND('',#5116,.T.);
#3761=FACE_OUTER_BOUND('',#5117,.T.);
#3762=FACE_OUTER_BOUND('',#5118,.T.);
#3763=FACE_OUTER_BOUND('',#5120,.T.);
#3764=FACE_OUTER_BOUND('',#5121,.T.);
#3765=FACE_OUTER_BOUND('',#5122,.T.);
#3766=FACE_OUTER_BOUND('',#5123,.T.);
#3767=FACE_OUTER_BOUND('',#5124,.T.);
#3768=FACE_OUTER_BOUND('',#5125,.T.);
#3769=FACE_OUTER_BOUND('',#5126,.T.);
#3770=FACE_OUTER_BOUND('',#5127,.T.);
#3771=FACE_OUTER_BOUND('',#5128,.T.);
#3772=FACE_OUTER_BOUND('',#5129,.T.);
#3773=FACE_OUTER_BOUND('',#5130,.T.);
#3774=FACE_OUTER_BOUND('',#5131,.T.);
#3775=FACE_OUTER_BOUND('',#5132,.T.);
#3776=FACE_OUTER_BOUND('',#5133,.T.);
#3777=FACE_OUTER_BOUND('',#5134,.T.);
#3778=FACE_OUTER_BOUND('',#5135,.T.);
#3779=FACE_OUTER_BOUND('',#5136,.T.);
#3780=FACE_OUTER_BOUND('',#5137,.T.);
#3781=FACE_OUTER_BOUND('',#5138,.T.);
#3782=FACE_OUTER_BOUND('',#5139,.T.);
#3783=FACE_OUTER_BOUND('',#5140,.T.);
#3784=FACE_OUTER_BOUND('',#5141,.T.);
#3785=FACE_OUTER_BOUND('',#5142,.T.);
#3786=FACE_OUTER_BOUND('',#5143,.T.);
#3787=FACE_OUTER_BOUND('',#5144,.T.);
#3788=FACE_OUTER_BOUND('',#5145,.T.);
#3789=FACE_OUTER_BOUND('',#5146,.T.);
#3790=FACE_OUTER_BOUND('',#5147,.T.);
#3791=FACE_OUTER_BOUND('',#5148,.T.);
#3792=FACE_OUTER_BOUND('',#5149,.T.);
#3793=FACE_OUTER_BOUND('',#5150,.T.);
#3794=FACE_OUTER_BOUND('',#5151,.T.);
#3795=FACE_OUTER_BOUND('',#5152,.T.);
#3796=FACE_OUTER_BOUND('',#5153,.T.);
#3797=FACE_OUTER_BOUND('',#5155,.T.);
#3798=FACE_OUTER_BOUND('',#5156,.T.);
#3799=FACE_OUTER_BOUND('',#5157,.T.);
#3800=FACE_OUTER_BOUND('',#5158,.T.);
#3801=FACE_OUTER_BOUND('',#5159,.T.);
#3802=FACE_OUTER_BOUND('',#5160,.T.);
#3803=FACE_OUTER_BOUND('',#5161,.T.);
#3804=FACE_OUTER_BOUND('',#5162,.T.);
#3805=FACE_OUTER_BOUND('',#5163,.T.);
#3806=FACE_OUTER_BOUND('',#5164,.T.);
#3807=FACE_OUTER_BOUND('',#5165,.T.);
#3808=FACE_OUTER_BOUND('',#5166,.T.);
#3809=FACE_OUTER_BOUND('',#5167,.T.);
#3810=FACE_OUTER_BOUND('',#5168,.T.);
#3811=FACE_OUTER_BOUND('',#5169,.T.);
#3812=FACE_OUTER_BOUND('',#5170,.T.);
#3813=FACE_OUTER_BOUND('',#5171,.T.);
#3814=FACE_OUTER_BOUND('',#5172,.T.);
#3815=FACE_OUTER_BOUND('',#5173,.T.);
#3816=FACE_OUTER_BOUND('',#5174,.T.);
#3817=FACE_OUTER_BOUND('',#5175,.T.);
#3818=FACE_OUTER_BOUND('',#5176,.T.);
#3819=FACE_OUTER_BOUND('',#5177,.T.);
#3820=FACE_OUTER_BOUND('',#5178,.T.);
#3821=FACE_OUTER_BOUND('',#5179,.T.);
#3822=FACE_OUTER_BOUND('',#5180,.T.);
#3823=FACE_OUTER_BOUND('',#5181,.T.);
#3824=FACE_OUTER_BOUND('',#5182,.T.);
#3825=FACE_OUTER_BOUND('',#5183,.T.);
#3826=FACE_OUTER_BOUND('',#5184,.T.);
#3827=FACE_OUTER_BOUND('',#5185,.T.);
#3828=FACE_OUTER_BOUND('',#5186,.T.);
#3829=FACE_OUTER_BOUND('',#5187,.T.);
#3830=FACE_OUTER_BOUND('',#5188,.T.);
#3831=FACE_OUTER_BOUND('',#5189,.T.);
#3832=FACE_OUTER_BOUND('',#5190,.T.);
#3833=FACE_OUTER_BOUND('',#5191,.T.);
#3834=FACE_OUTER_BOUND('',#5192,.T.);
#3835=FACE_OUTER_BOUND('',#5193,.T.);
#3836=FACE_OUTER_BOUND('',#5194,.T.);
#3837=FACE_OUTER_BOUND('',#5195,.T.);
#3838=FACE_OUTER_BOUND('',#5196,.T.);
#3839=FACE_OUTER_BOUND('',#5197,.T.);
#3840=FACE_OUTER_BOUND('',#5198,.T.);
#3841=FACE_OUTER_BOUND('',#5199,.T.);
#3842=FACE_OUTER_BOUND('',#5200,.T.);
#3843=FACE_OUTER_BOUND('',#5201,.T.);
#3844=FACE_OUTER_BOUND('',#5202,.T.);
#3845=FACE_OUTER_BOUND('',#5203,.T.);
#3846=FACE_OUTER_BOUND('',#5204,.T.);
#3847=FACE_OUTER_BOUND('',#5205,.T.);
#3848=FACE_OUTER_BOUND('',#5206,.T.);
#3849=FACE_OUTER_BOUND('',#5207,.T.);
#3850=FACE_OUTER_BOUND('',#5208,.T.);
#3851=FACE_OUTER_BOUND('',#5209,.T.);
#3852=FACE_OUTER_BOUND('',#5210,.T.);
#3853=FACE_OUTER_BOUND('',#5211,.T.);
#3854=FACE_OUTER_BOUND('',#5212,.T.);
#3855=FACE_OUTER_BOUND('',#5213,.T.);
#3856=FACE_OUTER_BOUND('',#5214,.T.);
#3857=FACE_OUTER_BOUND('',#5215,.T.);
#3858=FACE_OUTER_BOUND('',#5216,.T.);
#3859=FACE_OUTER_BOUND('',#5217,.T.);
#3860=FACE_OUTER_BOUND('',#5218,.T.);
#3861=FACE_OUTER_BOUND('',#5219,.T.);
#3862=FACE_OUTER_BOUND('',#5220,.T.);
#3863=FACE_OUTER_BOUND('',#5221,.T.);
#3864=FACE_OUTER_BOUND('',#5222,.T.);
#3865=FACE_OUTER_BOUND('',#5223,.T.);
#3866=FACE_OUTER_BOUND('',#5224,.T.);
#3867=FACE_OUTER_BOUND('',#5225,.T.);
#3868=FACE_OUTER_BOUND('',#5226,.T.);
#3869=FACE_OUTER_BOUND('',#5227,.T.);
#3870=FACE_OUTER_BOUND('',#5228,.T.);
#3871=FACE_OUTER_BOUND('',#5229,.T.);
#3872=FACE_OUTER_BOUND('',#5230,.T.);
#3873=FACE_OUTER_BOUND('',#5231,.T.);
#3874=FACE_OUTER_BOUND('',#5232,.T.);
#3875=FACE_OUTER_BOUND('',#5233,.T.);
#3876=FACE_OUTER_BOUND('',#5234,.T.);
#3877=FACE_OUTER_BOUND('',#5235,.T.);
#3878=FACE_OUTER_BOUND('',#5236,.T.);
#3879=FACE_OUTER_BOUND('',#5237,.T.);
#3880=FACE_OUTER_BOUND('',#5238,.T.);
#3881=FACE_OUTER_BOUND('',#5239,.T.);
#3882=FACE_OUTER_BOUND('',#5240,.T.);
#3883=FACE_OUTER_BOUND('',#5241,.T.);
#3884=FACE_OUTER_BOUND('',#5242,.T.);
#3885=FACE_OUTER_BOUND('',#5243,.T.);
#3886=FACE_OUTER_BOUND('',#5244,.T.);
#3887=FACE_OUTER_BOUND('',#5245,.T.);
#3888=FACE_OUTER_BOUND('',#5246,.T.);
#3889=FACE_OUTER_BOUND('',#5247,.T.);
#3890=FACE_OUTER_BOUND('',#5248,.T.);
#3891=FACE_OUTER_BOUND('',#5249,.T.);
#3892=FACE_OUTER_BOUND('',#5250,.T.);
#3893=FACE_OUTER_BOUND('',#5251,.T.);
#3894=FACE_OUTER_BOUND('',#5252,.T.);
#3895=FACE_OUTER_BOUND('',#5253,.T.);
#3896=FACE_OUTER_BOUND('',#5254,.T.);
#3897=FACE_OUTER_BOUND('',#5255,.T.);
#3898=FACE_OUTER_BOUND('',#5256,.T.);
#3899=FACE_OUTER_BOUND('',#5257,.T.);
#3900=FACE_OUTER_BOUND('',#5258,.T.);
#3901=FACE_OUTER_BOUND('',#5259,.T.);
#3902=FACE_OUTER_BOUND('',#5260,.T.);
#3903=FACE_OUTER_BOUND('',#5261,.T.);
#3904=FACE_OUTER_BOUND('',#5262,.T.);
#3905=FACE_OUTER_BOUND('',#5263,.T.);
#3906=FACE_OUTER_BOUND('',#5264,.T.);
#3907=FACE_OUTER_BOUND('',#5265,.T.);
#3908=FACE_OUTER_BOUND('',#5266,.T.);
#3909=FACE_OUTER_BOUND('',#5267,.T.);
#3910=FACE_OUTER_BOUND('',#5268,.T.);
#3911=FACE_OUTER_BOUND('',#5269,.T.);
#3912=FACE_OUTER_BOUND('',#5270,.T.);
#3913=FACE_OUTER_BOUND('',#5271,.T.);
#3914=FACE_OUTER_BOUND('',#5272,.T.);
#3915=FACE_OUTER_BOUND('',#5273,.T.);
#3916=FACE_OUTER_BOUND('',#5275,.T.);
#3917=FACE_OUTER_BOUND('',#5277,.T.);
#3918=FACE_OUTER_BOUND('',#5278,.T.);
#3919=FACE_OUTER_BOUND('',#5279,.T.);
#3920=FACE_OUTER_BOUND('',#5280,.T.);
#3921=FACE_OUTER_BOUND('',#5281,.T.);
#3922=FACE_OUTER_BOUND('',#5282,.T.);
#3923=FACE_OUTER_BOUND('',#5283,.T.);
#3924=FACE_OUTER_BOUND('',#5284,.T.);
#3925=FACE_OUTER_BOUND('',#5285,.T.);
#3926=FACE_OUTER_BOUND('',#5286,.T.);
#3927=FACE_OUTER_BOUND('',#5287,.T.);
#3928=FACE_OUTER_BOUND('',#5288,.T.);
#3929=FACE_OUTER_BOUND('',#5289,.T.);
#3930=FACE_OUTER_BOUND('',#5290,.T.);
#3931=FACE_OUTER_BOUND('',#5291,.T.);
#3932=FACE_OUTER_BOUND('',#5292,.T.);
#3933=FACE_OUTER_BOUND('',#5293,.T.);
#3934=FACE_OUTER_BOUND('',#5294,.T.);
#3935=FACE_OUTER_BOUND('',#5295,.T.);
#3936=FACE_OUTER_BOUND('',#5296,.T.);
#3937=FACE_OUTER_BOUND('',#5297,.T.);
#3938=FACE_OUTER_BOUND('',#5298,.T.);
#3939=FACE_OUTER_BOUND('',#5299,.T.);
#3940=FACE_OUTER_BOUND('',#5300,.T.);
#3941=FACE_OUTER_BOUND('',#5301,.T.);
#3942=FACE_OUTER_BOUND('',#5302,.T.);
#3943=FACE_OUTER_BOUND('',#5303,.T.);
#3944=FACE_OUTER_BOUND('',#5304,.T.);
#3945=FACE_OUTER_BOUND('',#5305,.T.);
#3946=FACE_OUTER_BOUND('',#5306,.T.);
#3947=FACE_OUTER_BOUND('',#5307,.T.);
#3948=FACE_OUTER_BOUND('',#5308,.T.);
#3949=FACE_OUTER_BOUND('',#5309,.T.);
#3950=FACE_OUTER_BOUND('',#5310,.T.);
#3951=FACE_OUTER_BOUND('',#5311,.T.);
#3952=FACE_OUTER_BOUND('',#5312,.T.);
#3953=FACE_OUTER_BOUND('',#5313,.T.);
#3954=FACE_OUTER_BOUND('',#5314,.T.);
#3955=FACE_OUTER_BOUND('',#5315,.T.);
#3956=FACE_OUTER_BOUND('',#5316,.T.);
#3957=FACE_OUTER_BOUND('',#5317,.T.);
#3958=FACE_OUTER_BOUND('',#5318,.T.);
#3959=FACE_OUTER_BOUND('',#5319,.T.);
#3960=FACE_OUTER_BOUND('',#5320,.T.);
#3961=FACE_OUTER_BOUND('',#5321,.T.);
#3962=FACE_OUTER_BOUND('',#5322,.T.);
#3963=FACE_OUTER_BOUND('',#5323,.T.);
#3964=FACE_OUTER_BOUND('',#5324,.T.);
#3965=FACE_OUTER_BOUND('',#5325,.T.);
#3966=FACE_OUTER_BOUND('',#5326,.T.);
#3967=FACE_OUTER_BOUND('',#5327,.T.);
#3968=FACE_OUTER_BOUND('',#5328,.T.);
#3969=FACE_OUTER_BOUND('',#5329,.T.);
#3970=FACE_OUTER_BOUND('',#5330,.T.);
#3971=FACE_OUTER_BOUND('',#5331,.T.);
#3972=FACE_OUTER_BOUND('',#5332,.T.);
#3973=FACE_OUTER_BOUND('',#5333,.T.);
#3974=FACE_OUTER_BOUND('',#5334,.T.);
#3975=FACE_OUTER_BOUND('',#5335,.T.);
#3976=FACE_OUTER_BOUND('',#5336,.T.);
#3977=FACE_OUTER_BOUND('',#5337,.T.);
#3978=FACE_OUTER_BOUND('',#5338,.T.);
#3979=FACE_OUTER_BOUND('',#5339,.T.);
#3980=FACE_OUTER_BOUND('',#5340,.T.);
#3981=FACE_OUTER_BOUND('',#5341,.T.);
#3982=FACE_OUTER_BOUND('',#5342,.T.);
#3983=FACE_OUTER_BOUND('',#5343,.T.);
#3984=FACE_OUTER_BOUND('',#5344,.T.);
#3985=FACE_OUTER_BOUND('',#5345,.T.);
#3986=FACE_OUTER_BOUND('',#5346,.T.);
#3987=FACE_OUTER_BOUND('',#5347,.T.);
#3988=FACE_OUTER_BOUND('',#5348,.T.);
#3989=FACE_OUTER_BOUND('',#5349,.T.);
#3990=FACE_OUTER_BOUND('',#5350,.T.);
#3991=FACE_OUTER_BOUND('',#5351,.T.);
#3992=FACE_OUTER_BOUND('',#5352,.T.);
#3993=FACE_OUTER_BOUND('',#5353,.T.);
#3994=FACE_OUTER_BOUND('',#5354,.T.);
#3995=FACE_OUTER_BOUND('',#5355,.T.);
#3996=FACE_OUTER_BOUND('',#5356,.T.);
#3997=FACE_OUTER_BOUND('',#5357,.T.);
#3998=FACE_OUTER_BOUND('',#5358,.T.);
#3999=FACE_OUTER_BOUND('',#5359,.T.);
#4000=FACE_OUTER_BOUND('',#5360,.T.);
#4001=FACE_OUTER_BOUND('',#5361,.T.);
#4002=FACE_OUTER_BOUND('',#5362,.T.);
#4003=FACE_OUTER_BOUND('',#5363,.T.);
#4004=FACE_OUTER_BOUND('',#5364,.T.);
#4005=FACE_OUTER_BOUND('',#5365,.T.);
#4006=FACE_OUTER_BOUND('',#5366,.T.);
#4007=FACE_OUTER_BOUND('',#5367,.T.);
#4008=FACE_OUTER_BOUND('',#5368,.T.);
#4009=FACE_OUTER_BOUND('',#5369,.T.);
#4010=FACE_OUTER_BOUND('',#5370,.T.);
#4011=FACE_OUTER_BOUND('',#5371,.T.);
#4012=FACE_OUTER_BOUND('',#5372,.T.);
#4013=FACE_OUTER_BOUND('',#5373,.T.);
#4014=FACE_OUTER_BOUND('',#5374,.T.);
#4015=FACE_OUTER_BOUND('',#5375,.T.);
#4016=FACE_OUTER_BOUND('',#5376,.T.);
#4017=FACE_OUTER_BOUND('',#5377,.T.);
#4018=FACE_OUTER_BOUND('',#5378,.T.);
#4019=FACE_OUTER_BOUND('',#5379,.T.);
#4020=FACE_OUTER_BOUND('',#5380,.T.);
#4021=FACE_OUTER_BOUND('',#5381,.T.);
#4022=FACE_OUTER_BOUND('',#5382,.T.);
#4023=FACE_OUTER_BOUND('',#5383,.T.);
#4024=FACE_OUTER_BOUND('',#5384,.T.);
#4025=FACE_OUTER_BOUND('',#5385,.T.);
#4026=FACE_OUTER_BOUND('',#5386,.T.);
#4027=FACE_OUTER_BOUND('',#5387,.T.);
#4028=FACE_OUTER_BOUND('',#5388,.T.);
#4029=FACE_OUTER_BOUND('',#5389,.T.);
#4030=FACE_OUTER_BOUND('',#5390,.T.);
#4031=FACE_OUTER_BOUND('',#5391,.T.);
#4032=FACE_OUTER_BOUND('',#5392,.T.);
#4033=FACE_OUTER_BOUND('',#5393,.T.);
#4034=FACE_OUTER_BOUND('',#5394,.T.);
#4035=FACE_OUTER_BOUND('',#5395,.T.);
#4036=FACE_OUTER_BOUND('',#5396,.T.);
#4037=FACE_OUTER_BOUND('',#5397,.T.);
#4038=FACE_OUTER_BOUND('',#5398,.T.);
#4039=FACE_OUTER_BOUND('',#5399,.T.);
#4040=FACE_OUTER_BOUND('',#5400,.T.);
#4041=FACE_OUTER_BOUND('',#5401,.T.);
#4042=FACE_OUTER_BOUND('',#5402,.T.);
#4043=FACE_OUTER_BOUND('',#5403,.T.);
#4044=FACE_OUTER_BOUND('',#5404,.T.);
#4045=FACE_OUTER_BOUND('',#5405,.T.);
#4046=FACE_OUTER_BOUND('',#5406,.T.);
#4047=FACE_OUTER_BOUND('',#5407,.T.);
#4048=FACE_OUTER_BOUND('',#5408,.T.);
#4049=FACE_OUTER_BOUND('',#5409,.T.);
#4050=FACE_OUTER_BOUND('',#5410,.T.);
#4051=FACE_OUTER_BOUND('',#5411,.T.);
#4052=FACE_OUTER_BOUND('',#5412,.T.);
#4053=FACE_OUTER_BOUND('',#5413,.T.);
#4054=FACE_OUTER_BOUND('',#5414,.T.);
#4055=FACE_OUTER_BOUND('',#5415,.T.);
#4056=FACE_OUTER_BOUND('',#5416,.T.);
#4057=FACE_OUTER_BOUND('',#5417,.T.);
#4058=FACE_OUTER_BOUND('',#5418,.T.);
#4059=FACE_OUTER_BOUND('',#5419,.T.);
#4060=FACE_OUTER_BOUND('',#5420,.T.);
#4061=FACE_OUTER_BOUND('',#5421,.T.);
#4062=FACE_OUTER_BOUND('',#5422,.T.);
#4063=FACE_OUTER_BOUND('',#5423,.T.);
#4064=FACE_OUTER_BOUND('',#5424,.T.);
#4065=FACE_OUTER_BOUND('',#5425,.T.);
#4066=FACE_OUTER_BOUND('',#5426,.T.);
#4067=FACE_OUTER_BOUND('',#5427,.T.);
#4068=FACE_OUTER_BOUND('',#5428,.T.);
#4069=FACE_OUTER_BOUND('',#5429,.T.);
#4070=FACE_OUTER_BOUND('',#5430,.T.);
#4071=FACE_OUTER_BOUND('',#5431,.T.);
#4072=FACE_OUTER_BOUND('',#5432,.T.);
#4073=FACE_OUTER_BOUND('',#5433,.T.);
#4074=FACE_OUTER_BOUND('',#5434,.T.);
#4075=FACE_OUTER_BOUND('',#5435,.T.);
#4076=FACE_OUTER_BOUND('',#5436,.T.);
#4077=FACE_OUTER_BOUND('',#5437,.T.);
#4078=FACE_OUTER_BOUND('',#5438,.T.);
#4079=FACE_OUTER_BOUND('',#5439,.T.);
#4080=FACE_OUTER_BOUND('',#5440,.T.);
#4081=FACE_OUTER_BOUND('',#5441,.T.);
#4082=FACE_OUTER_BOUND('',#5442,.T.);
#4083=FACE_OUTER_BOUND('',#5443,.T.);
#4084=FACE_OUTER_BOUND('',#5444,.T.);
#4085=FACE_OUTER_BOUND('',#5445,.T.);
#4086=FACE_OUTER_BOUND('',#5446,.T.);
#4087=FACE_OUTER_BOUND('',#5447,.T.);
#4088=FACE_OUTER_BOUND('',#5448,.T.);
#4089=FACE_OUTER_BOUND('',#5449,.T.);
#4090=FACE_OUTER_BOUND('',#5450,.T.);
#4091=FACE_OUTER_BOUND('',#5451,.T.);
#4092=FACE_OUTER_BOUND('',#5452,.T.);
#4093=FACE_OUTER_BOUND('',#5453,.T.);
#4094=FACE_OUTER_BOUND('',#5454,.T.);
#4095=FACE_OUTER_BOUND('',#5455,.T.);
#4096=FACE_OUTER_BOUND('',#5456,.T.);
#4097=FACE_OUTER_BOUND('',#5457,.T.);
#4098=FACE_OUTER_BOUND('',#5458,.T.);
#4099=FACE_OUTER_BOUND('',#5459,.T.);
#4100=FACE_OUTER_BOUND('',#5460,.T.);
#4101=FACE_OUTER_BOUND('',#5461,.T.);
#4102=FACE_OUTER_BOUND('',#5462,.T.);
#4103=FACE_OUTER_BOUND('',#5463,.T.);
#4104=FACE_OUTER_BOUND('',#5464,.T.);
#4105=FACE_OUTER_BOUND('',#5465,.T.);
#4106=FACE_OUTER_BOUND('',#5466,.T.);
#4107=FACE_OUTER_BOUND('',#5467,.T.);
#4108=FACE_OUTER_BOUND('',#5468,.T.);
#4109=FACE_OUTER_BOUND('',#5469,.T.);
#4110=FACE_OUTER_BOUND('',#5470,.T.);
#4111=FACE_OUTER_BOUND('',#5471,.T.);
#4112=FACE_OUTER_BOUND('',#5472,.T.);
#4113=FACE_OUTER_BOUND('',#5473,.T.);
#4114=FACE_OUTER_BOUND('',#5474,.T.);
#4115=FACE_OUTER_BOUND('',#5475,.T.);
#4116=FACE_OUTER_BOUND('',#5476,.T.);
#4117=FACE_OUTER_BOUND('',#5477,.T.);
#4118=FACE_OUTER_BOUND('',#5478,.T.);
#4119=FACE_OUTER_BOUND('',#5479,.T.);
#4120=FACE_OUTER_BOUND('',#5480,.T.);
#4121=FACE_OUTER_BOUND('',#5481,.T.);
#4122=FACE_OUTER_BOUND('',#5482,.T.);
#4123=FACE_OUTER_BOUND('',#5483,.T.);
#4124=FACE_OUTER_BOUND('',#5484,.T.);
#4125=FACE_OUTER_BOUND('',#5485,.T.);
#4126=FACE_OUTER_BOUND('',#5486,.T.);
#4127=FACE_OUTER_BOUND('',#5487,.T.);
#4128=FACE_OUTER_BOUND('',#5488,.T.);
#4129=FACE_OUTER_BOUND('',#5489,.T.);
#4130=FACE_OUTER_BOUND('',#5490,.T.);
#4131=FACE_OUTER_BOUND('',#5491,.T.);
#4132=FACE_OUTER_BOUND('',#5492,.T.);
#4133=FACE_OUTER_BOUND('',#5493,.T.);
#4134=FACE_OUTER_BOUND('',#5494,.T.);
#4135=FACE_OUTER_BOUND('',#5495,.T.);
#4136=FACE_OUTER_BOUND('',#5496,.T.);
#4137=FACE_OUTER_BOUND('',#5497,.T.);
#4138=FACE_OUTER_BOUND('',#5498,.T.);
#4139=FACE_OUTER_BOUND('',#5499,.T.);
#4140=FACE_OUTER_BOUND('',#5500,.T.);
#4141=FACE_OUTER_BOUND('',#5501,.T.);
#4142=FACE_OUTER_BOUND('',#5502,.T.);
#4143=FACE_OUTER_BOUND('',#5503,.T.);
#4144=FACE_OUTER_BOUND('',#5504,.T.);
#4145=FACE_OUTER_BOUND('',#5505,.T.);
#4146=FACE_OUTER_BOUND('',#5506,.T.);
#4147=FACE_OUTER_BOUND('',#5507,.T.);
#4148=FACE_OUTER_BOUND('',#5508,.T.);
#4149=FACE_OUTER_BOUND('',#5509,.T.);
#4150=FACE_OUTER_BOUND('',#5510,.T.);
#4151=FACE_OUTER_BOUND('',#5511,.T.);
#4152=FACE_OUTER_BOUND('',#5512,.T.);
#4153=FACE_OUTER_BOUND('',#5513,.T.);
#4154=FACE_OUTER_BOUND('',#5514,.T.);
#4155=FACE_OUTER_BOUND('',#5515,.T.);
#4156=FACE_OUTER_BOUND('',#5516,.T.);
#4157=FACE_OUTER_BOUND('',#5517,.T.);
#4158=FACE_OUTER_BOUND('',#5518,.T.);
#4159=FACE_OUTER_BOUND('',#5519,.T.);
#4160=FACE_OUTER_BOUND('',#5520,.T.);
#4161=FACE_OUTER_BOUND('',#5521,.T.);
#4162=FACE_OUTER_BOUND('',#5522,.T.);
#4163=FACE_OUTER_BOUND('',#5523,.T.);
#4164=FACE_OUTER_BOUND('',#5524,.T.);
#4165=FACE_OUTER_BOUND('',#5525,.T.);
#4166=FACE_OUTER_BOUND('',#5526,.T.);
#4167=FACE_OUTER_BOUND('',#5527,.T.);
#4168=FACE_OUTER_BOUND('',#5528,.T.);
#4169=FACE_OUTER_BOUND('',#5529,.T.);
#4170=FACE_OUTER_BOUND('',#5530,.T.);
#4171=FACE_OUTER_BOUND('',#5531,.T.);
#4172=FACE_OUTER_BOUND('',#5532,.T.);
#4173=FACE_OUTER_BOUND('',#5533,.T.);
#4174=FACE_OUTER_BOUND('',#5534,.T.);
#4175=FACE_OUTER_BOUND('',#5544,.T.);
#4176=FACE_OUTER_BOUND('',#5545,.T.);
#4177=FACE_OUTER_BOUND('',#5546,.T.);
#4178=FACE_OUTER_BOUND('',#5547,.T.);
#4179=FACE_OUTER_BOUND('',#5548,.T.);
#4180=FACE_OUTER_BOUND('',#5549,.T.);
#4181=FACE_OUTER_BOUND('',#5550,.T.);
#4182=FACE_OUTER_BOUND('',#5551,.T.);
#4183=FACE_OUTER_BOUND('',#5552,.T.);
#4184=FACE_OUTER_BOUND('',#5553,.T.);
#4185=FACE_OUTER_BOUND('',#5554,.T.);
#4186=FACE_OUTER_BOUND('',#5555,.T.);
#4187=FACE_OUTER_BOUND('',#5556,.T.);
#4188=FACE_OUTER_BOUND('',#5557,.T.);
#4189=FACE_OUTER_BOUND('',#5558,.T.);
#4190=FACE_OUTER_BOUND('',#5559,.T.);
#4191=FACE_OUTER_BOUND('',#5560,.T.);
#4192=FACE_OUTER_BOUND('',#5561,.T.);
#4193=FACE_OUTER_BOUND('',#5562,.T.);
#4194=FACE_OUTER_BOUND('',#5563,.T.);
#4195=FACE_OUTER_BOUND('',#5564,.T.);
#4196=FACE_OUTER_BOUND('',#5566,.T.);
#4197=FACE_OUTER_BOUND('',#5567,.T.);
#4198=FACE_OUTER_BOUND('',#5568,.T.);
#4199=FACE_OUTER_BOUND('',#5569,.T.);
#4200=FACE_OUTER_BOUND('',#5570,.T.);
#4201=FACE_OUTER_BOUND('',#5571,.T.);
#4202=FACE_OUTER_BOUND('',#5575,.T.);
#4203=FACE_OUTER_BOUND('',#5576,.T.);
#4204=FACE_OUTER_BOUND('',#5577,.T.);
#4205=FACE_OUTER_BOUND('',#5578,.T.);
#4206=FACE_OUTER_BOUND('',#5579,.T.);
#4207=FACE_OUTER_BOUND('',#5580,.T.);
#4208=FACE_OUTER_BOUND('',#5581,.T.);
#4209=FACE_OUTER_BOUND('',#5582,.T.);
#4210=FACE_OUTER_BOUND('',#5583,.T.);
#4211=FACE_OUTER_BOUND('',#5585,.T.);
#4212=FACE_OUTER_BOUND('',#5586,.T.);
#4213=FACE_OUTER_BOUND('',#5587,.T.);
#4214=FACE_OUTER_BOUND('',#5588,.T.);
#4215=FACE_OUTER_BOUND('',#5589,.T.);
#4216=FACE_OUTER_BOUND('',#5590,.T.);
#4217=FACE_OUTER_BOUND('',#5591,.T.);
#4218=FACE_OUTER_BOUND('',#5592,.T.);
#4219=FACE_OUTER_BOUND('',#5593,.T.);
#4220=FACE_OUTER_BOUND('',#5594,.T.);
#4221=FACE_OUTER_BOUND('',#5595,.T.);
#4222=FACE_OUTER_BOUND('',#5596,.T.);
#4223=FACE_OUTER_BOUND('',#5597,.T.);
#4224=FACE_OUTER_BOUND('',#5601,.T.);
#4225=FACE_OUTER_BOUND('',#5602,.T.);
#4226=FACE_OUTER_BOUND('',#5603,.T.);
#4227=FACE_OUTER_BOUND('',#5604,.T.);
#4228=FACE_OUTER_BOUND('',#5605,.T.);
#4229=FACE_OUTER_BOUND('',#5606,.T.);
#4230=FACE_OUTER_BOUND('',#5607,.T.);
#4231=FACE_OUTER_BOUND('',#5608,.T.);
#4232=FACE_OUTER_BOUND('',#5609,.T.);
#4233=FACE_OUTER_BOUND('',#5611,.T.);
#4234=FACE_OUTER_BOUND('',#5612,.T.);
#4235=FACE_OUTER_BOUND('',#5613,.T.);
#4236=FACE_OUTER_BOUND('',#5614,.T.);
#4237=FACE_OUTER_BOUND('',#5615,.T.);
#4238=FACE_OUTER_BOUND('',#5616,.T.);
#4239=FACE_OUTER_BOUND('',#5617,.T.);
#4240=FACE_OUTER_BOUND('',#5618,.T.);
#4241=FACE_OUTER_BOUND('',#5619,.T.);
#4242=FACE_OUTER_BOUND('',#5621,.T.);
#4243=FACE_OUTER_BOUND('',#5622,.T.);
#4244=FACE_OUTER_BOUND('',#5623,.T.);
#4245=FACE_OUTER_BOUND('',#5626,.T.);
#4246=FACE_OUTER_BOUND('',#5627,.T.);
#4247=FACE_OUTER_BOUND('',#5628,.T.);
#4248=FACE_OUTER_BOUND('',#5629,.T.);
#4249=FACE_OUTER_BOUND('',#5630,.T.);
#4250=FACE_OUTER_BOUND('',#5631,.T.);
#4251=FACE_OUTER_BOUND('',#5632,.T.);
#4252=FACE_OUTER_BOUND('',#5633,.T.);
#4253=FACE_OUTER_BOUND('',#5634,.T.);
#4254=FACE_OUTER_BOUND('',#5635,.T.);
#4255=FACE_OUTER_BOUND('',#5636,.T.);
#4256=FACE_OUTER_BOUND('',#5637,.T.);
#4257=FACE_OUTER_BOUND('',#5638,.T.);
#4258=FACE_OUTER_BOUND('',#5639,.T.);
#4259=FACE_OUTER_BOUND('',#5640,.T.);
#4260=FACE_OUTER_BOUND('',#5641,.T.);
#4261=FACE_OUTER_BOUND('',#5642,.T.);
#4262=FACE_OUTER_BOUND('',#5643,.T.);
#4263=FACE_OUTER_BOUND('',#5644,.T.);
#4264=FACE_OUTER_BOUND('',#5645,.T.);
#4265=FACE_OUTER_BOUND('',#5646,.T.);
#4266=FACE_OUTER_BOUND('',#5647,.T.);
#4267=FACE_OUTER_BOUND('',#5650,.T.);
#4268=FACE_OUTER_BOUND('',#5651,.T.);
#4269=FACE_OUTER_BOUND('',#5652,.T.);
#4270=FACE_OUTER_BOUND('',#5653,.T.);
#4271=FACE_OUTER_BOUND('',#5654,.T.);
#4272=FACE_OUTER_BOUND('',#5655,.T.);
#4273=FACE_OUTER_BOUND('',#5656,.T.);
#4274=FACE_OUTER_BOUND('',#5657,.T.);
#4275=FACE_OUTER_BOUND('',#5658,.T.);
#4276=FACE_OUTER_BOUND('',#5659,.T.);
#4277=EDGE_LOOP('',(#17529,#17530,#17531,#17532,#17533,#17534,#17535,#17536,
#17537,#17538,#17539,#17540,#17541,#17542,#17543,#17544,#17545,#17546,#17547,
#17548,#17549,#17550,#17551,#17552,#17553));
#4278=EDGE_LOOP('',(#17554,#17555,#17556,#17557));
#4279=EDGE_LOOP('',(#17558,#17559,#17560,#17561));
#4280=EDGE_LOOP('',(#17562,#17563,#17564,#17565));
#4281=EDGE_LOOP('',(#17566,#17567,#17568,#17569));
#4282=EDGE_LOOP('',(#17570,#17571,#17572,#17573));
#4283=EDGE_LOOP('',(#17574,#17575,#17576,#17577));
#4284=EDGE_LOOP('',(#17578,#17579,#17580,#17581));
#4285=EDGE_LOOP('',(#17582,#17583,#17584,#17585));
#4286=EDGE_LOOP('',(#17586,#17587,#17588,#17589));
#4287=EDGE_LOOP('',(#17590,#17591,#17592,#17593));
#4288=EDGE_LOOP('',(#17594,#17595,#17596,#17597));
#4289=EDGE_LOOP('',(#17598,#17599,#17600,#17601));
#4290=EDGE_LOOP('',(#17602,#17603,#17604,#17605));
#4291=EDGE_LOOP('',(#17606,#17607,#17608,#17609));
#4292=EDGE_LOOP('',(#17610,#17611,#17612,#17613));
#4293=EDGE_LOOP('',(#17614,#17615,#17616,#17617));
#4294=EDGE_LOOP('',(#17618,#17619,#17620,#17621));
#4295=EDGE_LOOP('',(#17622,#17623,#17624,#17625));
#4296=EDGE_LOOP('',(#17626,#17627,#17628,#17629));
#4297=EDGE_LOOP('',(#17630,#17631,#17632,#17633));
#4298=EDGE_LOOP('',(#17634,#17635,#17636,#17637));
#4299=EDGE_LOOP('',(#17638,#17639,#17640,#17641));
#4300=EDGE_LOOP('',(#17642,#17643,#17644,#17645));
#4301=EDGE_LOOP('',(#17646,#17647,#17648,#17649));
#4302=EDGE_LOOP('',(#17650,#17651,#17652,#17653));
#4303=EDGE_LOOP('',(#17654,#17655,#17656,#17657,#17658,#17659,#17660,#17661,
#17662,#17663,#17664,#17665,#17666,#17667,#17668,#17669,#17670,#17671,#17672,
#17673,#17674,#17675,#17676,#17677,#17678));
#4304=EDGE_LOOP('',(#17679,#17680,#17681,#17682,#17683,#17684,#17685,#17686,
#17687,#17688,#17689,#17690,#17691,#17692,#17693,#17694,#17695,#17696,#17697,
#17698,#17699,#17700,#17701,#17702,#17703,#17704));
#4305=EDGE_LOOP('',(#17705,#17706,#17707,#17708));
#4306=EDGE_LOOP('',(#17709,#17710,#17711,#17712));
#4307=EDGE_LOOP('',(#17713,#17714,#17715,#17716));
#4308=EDGE_LOOP('',(#17717,#17718,#17719,#17720));
#4309=EDGE_LOOP('',(#17721,#17722,#17723,#17724));
#4310=EDGE_LOOP('',(#17725,#17726,#17727,#17728));
#4311=EDGE_LOOP('',(#17729,#17730,#17731,#17732));
#4312=EDGE_LOOP('',(#17733,#17734,#17735,#17736));
#4313=EDGE_LOOP('',(#17737,#17738,#17739,#17740));
#4314=EDGE_LOOP('',(#17741,#17742,#17743,#17744));
#4315=EDGE_LOOP('',(#17745,#17746,#17747,#17748));
#4316=EDGE_LOOP('',(#17749,#17750,#17751,#17752));
#4317=EDGE_LOOP('',(#17753,#17754,#17755,#17756));
#4318=EDGE_LOOP('',(#17757,#17758,#17759,#17760));
#4319=EDGE_LOOP('',(#17761,#17762,#17763,#17764));
#4320=EDGE_LOOP('',(#17765,#17766,#17767,#17768));
#4321=EDGE_LOOP('',(#17769,#17770,#17771,#17772));
#4322=EDGE_LOOP('',(#17773,#17774,#17775,#17776));
#4323=EDGE_LOOP('',(#17777,#17778,#17779,#17780));
#4324=EDGE_LOOP('',(#17781,#17782,#17783,#17784));
#4325=EDGE_LOOP('',(#17785,#17786,#17787,#17788));
#4326=EDGE_LOOP('',(#17789,#17790,#17791,#17792));
#4327=EDGE_LOOP('',(#17793,#17794,#17795,#17796));
#4328=EDGE_LOOP('',(#17797,#17798,#17799,#17800));
#4329=EDGE_LOOP('',(#17801,#17802,#17803,#17804));
#4330=EDGE_LOOP('',(#17805,#17806,#17807,#17808));
#4331=EDGE_LOOP('',(#17809,#17810,#17811,#17812,#17813,#17814,#17815,#17816,
#17817,#17818,#17819,#17820,#17821,#17822,#17823,#17824,#17825,#17826,#17827,
#17828,#17829,#17830,#17831,#17832,#17833,#17834));
#4332=EDGE_LOOP('',(#17835,#17836,#17837,#17838));
#4333=EDGE_LOOP('',(#17839,#17840,#17841,#17842,#17843,#17844));
#4334=EDGE_LOOP('',(#17845,#17846,#17847,#17848,#17849,#17850));
#4335=EDGE_LOOP('',(#17851,#17852,#17853,#17854,#17855,#17856));
#4336=EDGE_LOOP('',(#17857,#17858,#17859,#17860));
#4337=EDGE_LOOP('',(#17861,#17862,#17863,#17864,#17865,#17866));
#4338=EDGE_LOOP('',(#17867,#17868,#17869,#17870,#17871,#17872));
#4339=EDGE_LOOP('',(#17873,#17874,#17875,#17876,#17877,#17878));
#4340=EDGE_LOOP('',(#17879,#17880,#17881,#17882,#17883,#17884));
#4341=EDGE_LOOP('',(#17885,#17886,#17887,#17888,#17889,#17890));
#4342=EDGE_LOOP('',(#17891,#17892,#17893,#17894,#17895,#17896));
#4343=EDGE_LOOP('',(#17897,#17898,#17899,#17900,#17901,#17902));
#4344=EDGE_LOOP('',(#17903,#17904,#17905,#17906,#17907,#17908));
#4345=EDGE_LOOP('',(#17909,#17910,#17911,#17912,#17913,#17914));
#4346=EDGE_LOOP('',(#17915,#17916,#17917,#17918,#17919,#17920));
#4347=EDGE_LOOP('',(#17921,#17922,#17923,#17924,#17925,#17926));
#4348=EDGE_LOOP('',(#17927,#17928,#17929,#17930,#17931,#17932));
#4349=EDGE_LOOP('',(#17933,#17934,#17935,#17936,#17937,#17938));
#4350=EDGE_LOOP('',(#17939,#17940,#17941,#17942,#17943,#17944));
#4351=EDGE_LOOP('',(#17945,#17946,#17947,#17948,#17949,#17950));
#4352=EDGE_LOOP('',(#17951,#17952,#17953,#17954,#17955,#17956));
#4353=EDGE_LOOP('',(#17957,#17958,#17959,#17960,#17961,#17962));
#4354=EDGE_LOOP('',(#17963,#17964,#17965,#17966,#17967,#17968));
#4355=EDGE_LOOP('',(#17969,#17970,#17971,#17972,#17973,#17974));
#4356=EDGE_LOOP('',(#17975,#17976,#17977,#17978,#17979,#17980));
#4357=EDGE_LOOP('',(#17981,#17982,#17983,#17984,#17985,#17986));
#4358=EDGE_LOOP('',(#17987,#17988,#17989,#17990,#17991,#17992));
#4359=EDGE_LOOP('',(#17993,#17994,#17995,#17996,#17997,#17998));
#4360=EDGE_LOOP('',(#17999,#18000,#18001,#18002,#18003,#18004));
#4361=EDGE_LOOP('',(#18005,#18006,#18007,#18008,#18009,#18010));
#4362=EDGE_LOOP('',(#18011,#18012,#18013,#18014,#18015,#18016));
#4363=EDGE_LOOP('',(#18017,#18018,#18019,#18020,#18021,#18022));
#4364=EDGE_LOOP('',(#18023,#18024,#18025,#18026,#18027,#18028));
#4365=EDGE_LOOP('',(#18029,#18030,#18031,#18032,#18033,#18034));
#4366=EDGE_LOOP('',(#18035,#18036,#18037,#18038,#18039,#18040));
#4367=EDGE_LOOP('',(#18041,#18042,#18043,#18044,#18045,#18046));
#4368=EDGE_LOOP('',(#18047,#18048,#18049,#18050,#18051,#18052));
#4369=EDGE_LOOP('',(#18053,#18054,#18055,#18056,#18057,#18058));
#4370=EDGE_LOOP('',(#18059,#18060,#18061,#18062,#18063,#18064));
#4371=EDGE_LOOP('',(#18065,#18066,#18067,#18068,#18069,#18070));
#4372=EDGE_LOOP('',(#18071,#18072,#18073,#18074,#18075,#18076));
#4373=EDGE_LOOP('',(#18077,#18078,#18079,#18080,#18081,#18082));
#4374=EDGE_LOOP('',(#18083,#18084,#18085,#18086,#18087,#18088));
#4375=EDGE_LOOP('',(#18089,#18090,#18091,#18092,#18093,#18094));
#4376=EDGE_LOOP('',(#18095,#18096,#18097,#18098,#18099,#18100));
#4377=EDGE_LOOP('',(#18101,#18102,#18103,#18104,#18105,#18106));
#4378=EDGE_LOOP('',(#18107,#18108,#18109,#18110,#18111,#18112));
#4379=EDGE_LOOP('',(#18113,#18114,#18115,#18116,#18117,#18118));
#4380=EDGE_LOOP('',(#18119,#18120,#18121,#18122,#18123,#18124));
#4381=EDGE_LOOP('',(#18125,#18126,#18127,#18128,#18129,#18130));
#4382=EDGE_LOOP('',(#18131,#18132,#18133,#18134,#18135,#18136));
#4383=EDGE_LOOP('',(#18137,#18138,#18139,#18140,#18141,#18142));
#4384=EDGE_LOOP('',(#18143,#18144,#18145,#18146,#18147,#18148));
#4385=EDGE_LOOP('',(#18149,#18150,#18151,#18152,#18153,#18154));
#4386=EDGE_LOOP('',(#18155,#18156,#18157,#18158,#18159,#18160));
#4387=EDGE_LOOP('',(#18161,#18162,#18163,#18164,#18165,#18166));
#4388=EDGE_LOOP('',(#18167,#18168,#18169,#18170,#18171,#18172));
#4389=EDGE_LOOP('',(#18173,#18174,#18175,#18176,#18177,#18178));
#4390=EDGE_LOOP('',(#18179,#18180,#18181,#18182,#18183,#18184));
#4391=EDGE_LOOP('',(#18185,#18186,#18187,#18188,#18189,#18190));
#4392=EDGE_LOOP('',(#18191,#18192,#18193,#18194,#18195,#18196));
#4393=EDGE_LOOP('',(#18197,#18198,#18199,#18200,#18201,#18202));
#4394=EDGE_LOOP('',(#18203,#18204,#18205,#18206,#18207,#18208));
#4395=EDGE_LOOP('',(#18209,#18210,#18211,#18212,#18213,#18214));
#4396=EDGE_LOOP('',(#18215,#18216,#18217,#18218,#18219,#18220));
#4397=EDGE_LOOP('',(#18221,#18222,#18223,#18224,#18225,#18226));
#4398=EDGE_LOOP('',(#18227,#18228,#18229,#18230,#18231,#18232));
#4399=EDGE_LOOP('',(#18233,#18234,#18235,#18236,#18237,#18238));
#4400=EDGE_LOOP('',(#18239,#18240,#18241,#18242,#18243,#18244));
#4401=EDGE_LOOP('',(#18245,#18246,#18247,#18248,#18249,#18250));
#4402=EDGE_LOOP('',(#18251,#18252,#18253,#18254,#18255,#18256));
#4403=EDGE_LOOP('',(#18257,#18258,#18259,#18260,#18261,#18262));
#4404=EDGE_LOOP('',(#18263,#18264,#18265,#18266,#18267,#18268));
#4405=EDGE_LOOP('',(#18269,#18270,#18271,#18272,#18273,#18274));
#4406=EDGE_LOOP('',(#18275,#18276,#18277,#18278,#18279,#18280));
#4407=EDGE_LOOP('',(#18281,#18282,#18283,#18284,#18285,#18286));
#4408=EDGE_LOOP('',(#18287,#18288,#18289,#18290,#18291,#18292));
#4409=EDGE_LOOP('',(#18293,#18294,#18295,#18296,#18297,#18298));
#4410=EDGE_LOOP('',(#18299,#18300,#18301,#18302,#18303,#18304));
#4411=EDGE_LOOP('',(#18305,#18306,#18307,#18308,#18309,#18310));
#4412=EDGE_LOOP('',(#18311,#18312,#18313,#18314,#18315,#18316));
#4413=EDGE_LOOP('',(#18317,#18318,#18319,#18320,#18321,#18322));
#4414=EDGE_LOOP('',(#18323,#18324,#18325,#18326,#18327,#18328));
#4415=EDGE_LOOP('',(#18329,#18330,#18331,#18332,#18333,#18334));
#4416=EDGE_LOOP('',(#18335,#18336,#18337,#18338,#18339,#18340));
#4417=EDGE_LOOP('',(#18341,#18342,#18343,#18344,#18345,#18346));
#4418=EDGE_LOOP('',(#18347,#18348,#18349,#18350,#18351,#18352));
#4419=EDGE_LOOP('',(#18353,#18354,#18355,#18356,#18357,#18358));
#4420=EDGE_LOOP('',(#18359,#18360,#18361,#18362,#18363,#18364));
#4421=EDGE_LOOP('',(#18365,#18366,#18367,#18368,#18369,#18370));
#4422=EDGE_LOOP('',(#18371,#18372,#18373,#18374,#18375,#18376));
#4423=EDGE_LOOP('',(#18377,#18378,#18379,#18380,#18381,#18382));
#4424=EDGE_LOOP('',(#18383,#18384,#18385,#18386,#18387,#18388));
#4425=EDGE_LOOP('',(#18389,#18390,#18391,#18392,#18393,#18394));
#4426=EDGE_LOOP('',(#18395,#18396,#18397,#18398,#18399,#18400));
#4427=EDGE_LOOP('',(#18401,#18402,#18403,#18404,#18405,#18406));
#4428=EDGE_LOOP('',(#18407,#18408,#18409,#18410,#18411,#18412));
#4429=EDGE_LOOP('',(#18413,#18414,#18415,#18416,#18417,#18418));
#4430=EDGE_LOOP('',(#18419,#18420,#18421,#18422,#18423,#18424));
#4431=EDGE_LOOP('',(#18425,#18426,#18427,#18428,#18429,#18430));
#4432=EDGE_LOOP('',(#18431,#18432,#18433,#18434,#18435,#18436));
#4433=EDGE_LOOP('',(#18437,#18438,#18439,#18440,#18441,#18442));
#4434=EDGE_LOOP('',(#18443,#18444,#18445,#18446,#18447,#18448));
#4435=EDGE_LOOP('',(#18449,#18450,#18451,#18452,#18453,#18454));
#4436=EDGE_LOOP('',(#18455,#18456,#18457,#18458,#18459,#18460));
#4437=EDGE_LOOP('',(#18461,#18462,#18463,#18464,#18465,#18466));
#4438=EDGE_LOOP('',(#18467,#18468,#18469,#18470,#18471,#18472));
#4439=EDGE_LOOP('',(#18473,#18474,#18475,#18476,#18477,#18478));
#4440=EDGE_LOOP('',(#18479,#18480,#18481,#18482,#18483,#18484));
#4441=EDGE_LOOP('',(#18485,#18486,#18487,#18488,#18489,#18490));
#4442=EDGE_LOOP('',(#18491,#18492,#18493,#18494,#18495,#18496));
#4443=EDGE_LOOP('',(#18497,#18498,#18499,#18500,#18501,#18502));
#4444=EDGE_LOOP('',(#18503,#18504,#18505,#18506,#18507,#18508));
#4445=EDGE_LOOP('',(#18509,#18510,#18511,#18512,#18513,#18514));
#4446=EDGE_LOOP('',(#18515,#18516,#18517,#18518,#18519,#18520));
#4447=EDGE_LOOP('',(#18521,#18522,#18523,#18524,#18525,#18526));
#4448=EDGE_LOOP('',(#18527,#18528,#18529,#18530,#18531));
#4449=EDGE_LOOP('',(#18532,#18533,#18534,#18535,#18536,#18537));
#4450=EDGE_LOOP('',(#18538,#18539,#18540,#18541,#18542,#18543));
#4451=EDGE_LOOP('',(#18544,#18545,#18546));
#4452=EDGE_LOOP('',(#18547,#18548,#18549));
#4453=EDGE_LOOP('',(#18550,#18551,#18552,#18553,#18554));
#4454=EDGE_LOOP('',(#18555,#18556,#18557,#18558,#18559,#18560));
#4455=EDGE_LOOP('',(#18561,#18562,#18563,#18564,#18565));
#4456=EDGE_LOOP('',(#18566,#18567,#18568,#18569,#18570,#18571));
#4457=EDGE_LOOP('',(#18572,#18573,#18574,#18575));
#4458=EDGE_LOOP('',(#18576,#18577,#18578,#18579,#18580,#18581));
#4459=EDGE_LOOP('',(#18582,#18583,#18584,#18585,#18586));
#4460=EDGE_LOOP('',(#18587,#18588,#18589,#18590,#18591,#18592));
#4461=EDGE_LOOP('',(#18593,#18594,#18595,#18596));
#4462=EDGE_LOOP('',(#18597,#18598,#18599,#18600,#18601,#18602));
#4463=EDGE_LOOP('',(#18603,#18604,#18605,#18606));
#4464=EDGE_LOOP('',(#18607,#18608,#18609,#18610,#18611,#18612));
#4465=EDGE_LOOP('',(#18613,#18614,#18615,#18616,#18617));
#4466=EDGE_LOOP('',(#18618,#18619,#18620,#18621,#18622,#18623));
#4467=EDGE_LOOP('',(#18624,#18625,#18626,#18627,#18628));
#4468=EDGE_LOOP('',(#18629,#18630,#18631,#18632,#18633,#18634));
#4469=EDGE_LOOP('',(#18635,#18636,#18637,#18638));
#4470=EDGE_LOOP('',(#18639,#18640,#18641,#18642,#18643,#18644));
#4471=EDGE_LOOP('',(#18645,#18646,#18647,#18648,#18649));
#4472=EDGE_LOOP('',(#18650,#18651,#18652,#18653,#18654,#18655));
#4473=EDGE_LOOP('',(#18656,#18657,#18658,#18659,#18660));
#4474=EDGE_LOOP('',(#18661,#18662,#18663,#18664,#18665,#18666));
#4475=EDGE_LOOP('',(#18667,#18668,#18669,#18670));
#4476=EDGE_LOOP('',(#18671,#18672,#18673,#18674,#18675,#18676));
#4477=EDGE_LOOP('',(#18677,#18678,#18679,#18680));
#4478=EDGE_LOOP('',(#18681,#18682,#18683,#18684,#18685,#18686));
#4479=EDGE_LOOP('',(#18687,#18688,#18689,#18690,#18691));
#4480=EDGE_LOOP('',(#18692,#18693,#18694,#18695,#18696,#18697));
#4481=EDGE_LOOP('',(#18698,#18699,#18700,#18701));
#4482=EDGE_LOOP('',(#18702,#18703,#18704,#18705));
#4483=EDGE_LOOP('',(#18706,#18707,#18708,#18709,#18710,#18711));
#4484=EDGE_LOOP('',(#18712,#18713,#18714,#18715));
#4485=EDGE_LOOP('',(#18716,#18717,#18718,#18719,#18720,#18721));
#4486=EDGE_LOOP('',(#18722,#18723,#18724,#18725,#18726));
#4487=EDGE_LOOP('',(#18727,#18728,#18729,#18730,#18731,#18732));
#4488=EDGE_LOOP('',(#18733,#18734,#18735,#18736));
#4489=EDGE_LOOP('',(#18737,#18738,#18739,#18740,#18741,#18742));
#4490=EDGE_LOOP('',(#18743,#18744,#18745,#18746));
#4491=EDGE_LOOP('',(#18747,#18748,#18749,#18750,#18751,#18752));
#4492=EDGE_LOOP('',(#18753,#18754,#18755,#18756,#18757));
#4493=EDGE_LOOP('',(#18758,#18759,#18760,#18761,#18762,#18763));
#4494=EDGE_LOOP('',(#18764,#18765,#18766,#18767,#18768));
#4495=EDGE_LOOP('',(#18769,#18770,#18771,#18772,#18773,#18774));
#4496=EDGE_LOOP('',(#18775,#18776,#18777,#18778));
#4497=EDGE_LOOP('',(#18779,#18780,#18781,#18782,#18783,#18784));
#4498=EDGE_LOOP('',(#18785,#18786,#18787,#18788,#18789));
#4499=EDGE_LOOP('',(#18790,#18791,#18792,#18793,#18794,#18795));
#4500=EDGE_LOOP('',(#18796,#18797,#18798,#18799,#18800));
#4501=EDGE_LOOP('',(#18801,#18802,#18803,#18804,#18805,#18806));
#4502=EDGE_LOOP('',(#18807,#18808,#18809,#18810));
#4503=EDGE_LOOP('',(#18811,#18812,#18813,#18814,#18815,#18816));
#4504=EDGE_LOOP('',(#18817,#18818,#18819,#18820));
#4505=EDGE_LOOP('',(#18821,#18822,#18823,#18824,#18825,#18826));
#4506=EDGE_LOOP('',(#18827,#18828,#18829,#18830,#18831));
#4507=EDGE_LOOP('',(#18832,#18833,#18834,#18835,#18836,#18837));
#4508=EDGE_LOOP('',(#18838,#18839,#18840,#18841));
#4509=EDGE_LOOP('',(#18842,#18843,#18844,#18845));
#4510=EDGE_LOOP('',(#18846,#18847,#18848,#18849,#18850,#18851));
#4511=EDGE_LOOP('',(#18852,#18853,#18854,#18855));
#4512=EDGE_LOOP('',(#18856,#18857,#18858,#18859,#18860,#18861));
#4513=EDGE_LOOP('',(#18862,#18863,#18864,#18865,#18866));
#4514=EDGE_LOOP('',(#18867,#18868,#18869,#18870,#18871,#18872));
#4515=EDGE_LOOP('',(#18873,#18874,#18875,#18876));
#4516=EDGE_LOOP('',(#18877,#18878,#18879,#18880,#18881,#18882));
#4517=EDGE_LOOP('',(#18883,#18884,#18885,#18886));
#4518=EDGE_LOOP('',(#18887,#18888,#18889,#18890,#18891,#18892));
#4519=EDGE_LOOP('',(#18893,#18894,#18895,#18896,#18897));
#4520=EDGE_LOOP('',(#18898,#18899,#18900,#18901,#18902,#18903));
#4521=EDGE_LOOP('',(#18904,#18905,#18906,#18907,#18908));
#4522=EDGE_LOOP('',(#18909,#18910,#18911,#18912,#18913,#18914));
#4523=EDGE_LOOP('',(#18915,#18916,#18917,#18918));
#4524=EDGE_LOOP('',(#18919,#18920,#18921,#18922,#18923,#18924));
#4525=EDGE_LOOP('',(#18925,#18926,#18927,#18928,#18929));
#4526=EDGE_LOOP('',(#18930,#18931,#18932,#18933,#18934,#18935));
#4527=EDGE_LOOP('',(#18936,#18937,#18938,#18939,#18940));
#4528=EDGE_LOOP('',(#18941,#18942,#18943,#18944,#18945,#18946));
#4529=EDGE_LOOP('',(#18947,#18948,#18949,#18950));
#4530=EDGE_LOOP('',(#18951,#18952,#18953,#18954,#18955,#18956));
#4531=EDGE_LOOP('',(#18957,#18958,#18959,#18960));
#4532=EDGE_LOOP('',(#18961,#18962,#18963,#18964,#18965,#18966));
#4533=EDGE_LOOP('',(#18967,#18968,#18969,#18970,#18971));
#4534=EDGE_LOOP('',(#18972,#18973,#18974,#18975,#18976,#18977));
#4535=EDGE_LOOP('',(#18978,#18979,#18980,#18981));
#4536=EDGE_LOOP('',(#18982,#18983,#18984,#18985));
#4537=EDGE_LOOP('',(#18986,#18987,#18988,#18989,#18990,#18991));
#4538=EDGE_LOOP('',(#18992,#18993,#18994,#18995));
#4539=EDGE_LOOP('',(#18996,#18997,#18998,#18999,#19000,#19001));
#4540=EDGE_LOOP('',(#19002,#19003,#19004,#19005,#19006));
#4541=EDGE_LOOP('',(#19007,#19008,#19009,#19010,#19011,#19012));
#4542=EDGE_LOOP('',(#19013,#19014,#19015,#19016));
#4543=EDGE_LOOP('',(#19017,#19018,#19019,#19020,#19021,#19022));
#4544=EDGE_LOOP('',(#19023,#19024,#19025,#19026));
#4545=EDGE_LOOP('',(#19027,#19028,#19029,#19030,#19031,#19032));
#4546=EDGE_LOOP('',(#19033,#19034,#19035,#19036,#19037));
#4547=EDGE_LOOP('',(#19038,#19039,#19040,#19041,#19042,#19043));
#4548=EDGE_LOOP('',(#19044,#19045,#19046,#19047,#19048));
#4549=EDGE_LOOP('',(#19049,#19050,#19051,#19052,#19053,#19054));
#4550=EDGE_LOOP('',(#19055,#19056,#19057,#19058));
#4551=EDGE_LOOP('',(#19059,#19060,#19061,#19062,#19063,#19064));
#4552=EDGE_LOOP('',(#19065,#19066,#19067,#19068,#19069));
#4553=EDGE_LOOP('',(#19070,#19071,#19072,#19073,#19074,#19075));
#4554=EDGE_LOOP('',(#19076,#19077,#19078,#19079,#19080));
#4555=EDGE_LOOP('',(#19081,#19082,#19083,#19084,#19085,#19086));
#4556=EDGE_LOOP('',(#19087,#19088,#19089,#19090));
#4557=EDGE_LOOP('',(#19091,#19092,#19093,#19094,#19095,#19096));
#4558=EDGE_LOOP('',(#19097,#19098,#19099,#19100));
#4559=EDGE_LOOP('',(#19101,#19102,#19103,#19104,#19105,#19106));
#4560=EDGE_LOOP('',(#19107,#19108,#19109,#19110,#19111));
#4561=EDGE_LOOP('',(#19112,#19113,#19114,#19115,#19116,#19117));
#4562=EDGE_LOOP('',(#19118,#19119,#19120,#19121));
#4563=EDGE_LOOP('',(#19122,#19123,#19124,#19125));
#4564=EDGE_LOOP('',(#19126,#19127,#19128,#19129,#19130,#19131));
#4565=EDGE_LOOP('',(#19132,#19133,#19134,#19135,#19136,#19137));
#4566=EDGE_LOOP('',(#19138,#19139,#19140,#19141,#19142,#19143));
#4567=EDGE_LOOP('',(#19144,#19145,#19146,#19147,#19148,#19149));
#4568=EDGE_LOOP('',(#19150,#19151,#19152,#19153,#19154,#19155));
#4569=EDGE_LOOP('',(#19156,#19157,#19158,#19159,#19160));
#4570=EDGE_LOOP('',(#19161,#19162,#19163,#19164,#19165,#19166));
#4571=EDGE_LOOP('',(#19167,#19168,#19169,#19170,#19171,#19172));
#4572=EDGE_LOOP('',(#19173,#19174,#19175,#19176,#19177,#19178));
#4573=EDGE_LOOP('',(#19179,#19180,#19181,#19182,#19183,#19184));
#4574=EDGE_LOOP('',(#19185,#19186,#19187,#19188,#19189,#19190));
#4575=EDGE_LOOP('',(#19191,#19192,#19193,#19194,#19195,#19196));
#4576=EDGE_LOOP('',(#19197,#19198,#19199,#19200));
#4577=EDGE_LOOP('',(#19201));
#4578=EDGE_LOOP('',(#19202,#19203,#19204,#19205));
#4579=EDGE_LOOP('',(#19206,#19207,#19208,#19209,#19210));
#4580=EDGE_LOOP('',(#19211,#19212,#19213,#19214));
#4581=EDGE_LOOP('',(#19215));
#4582=EDGE_LOOP('',(#19216,#19217,#19218,#19219));
#4583=EDGE_LOOP('',(#19220,#19221,#19222,#19223,#19224));
#4584=EDGE_LOOP('',(#19225,#19226,#19227,#19228));
#4585=EDGE_LOOP('',(#19229));
#4586=EDGE_LOOP('',(#19230,#19231,#19232,#19233));
#4587=EDGE_LOOP('',(#19234,#19235,#19236,#19237,#19238,#19239));
#4588=EDGE_LOOP('',(#19240,#19241,#19242,#19243,#19244,#19245,#19246,#19247));
#4589=EDGE_LOOP('',(#19248,#19249,#19250,#19251,#19252,#19253,#19254,#19255,
#19256,#19257,#19258,#19259,#19260,#19261,#19262,#19263,#19264,#19265,#19266,
#19267,#19268,#19269,#19270,#19271,#19272,#19273,#19274,#19275,#19276,#19277,
#19278,#19279));
#4590=EDGE_LOOP('',(#19280));
#4591=EDGE_LOOP('',(#19281));
#4592=EDGE_LOOP('',(#19282,#19283,#19284,#19285));
#4593=EDGE_LOOP('',(#19286,#19287,#19288,#19289));
#4594=EDGE_LOOP('',(#19290,#19291,#19292,#19293));
#4595=EDGE_LOOP('',(#19294,#19295,#19296,#19297));
#4596=EDGE_LOOP('',(#19298));
#4597=EDGE_LOOP('',(#19299));
#4598=EDGE_LOOP('',(#19300));
#4599=EDGE_LOOP('',(#19301,#19302,#19303,#19304,#19305,#19306,#19307,#19308,
#19309,#19310,#19311,#19312,#19313,#19314,#19315,#19316,#19317,#19318));
#4600=EDGE_LOOP('',(#19319,#19320,#19321,#19322,#19323,#19324,#19325,#19326,
#19327,#19328,#19329,#19330,#19331,#19332,#19333,#19334,#19335,#19336));
#4601=EDGE_LOOP('',(#19337,#19338,#19339,#19340,#19341,#19342,#19343,#19344,
#19345,#19346,#19347,#19348,#19349,#19350,#19351,#19352,#19353,#19354));
#4602=EDGE_LOOP('',(#19355,#19356,#19357,#19358,#19359,#19360,#19361,#19362,
#19363,#19364,#19365,#19366,#19367,#19368,#19369,#19370,#19371,#19372));
#4603=EDGE_LOOP('',(#19373,#19374,#19375,#19376,#19377,#19378,#19379,#19380,
#19381,#19382,#19383,#19384,#19385,#19386,#19387,#19388,#19389,#19390,#19391,
#19392,#19393,#19394,#19395,#19396,#19397,#19398,#19399,#19400,#19401,#19402,
#19403,#19404,#19405,#19406,#19407,#19408,#19409,#19410,#19411,#19412,#19413,
#19414,#19415,#19416,#19417,#19418,#19419,#19420,#19421,#19422,#19423,#19424,
#19425,#19426,#19427,#19428,#19429,#19430,#19431,#19432,#19433,#19434,#19435,
#19436,#19437,#19438,#19439,#19440,#19441,#19442,#19443,#19444,#19445,#19446,
#19447,#19448,#19449,#19450,#19451,#19452,#19453,#19454,#19455,#19456,#19457,
#19458,#19459,#19460,#19461,#19462,#19463,#19464,#19465,#19466,#19467,#19468,
#19469,#19470,#19471,#19472,#19473,#19474,#19475));
#4604=EDGE_LOOP('',(#19476,#19477,#19478,#19479,#19480,#19481,#19482,#19483,
#19484,#19485,#19486,#19487,#19488,#19489,#19490,#19491,#19492,#19493,#19494,
#19495,#19496,#19497,#19498,#19499,#19500,#19501,#19502,#19503,#19504,#19505,
#19506,#19507,#19508,#19509,#19510,#19511,#19512,#19513,#19514,#19515,#19516,
#19517,#19518,#19519,#19520,#19521,#19522,#19523,#19524,#19525,#19526,#19527,
#19528,#19529,#19530,#19531,#19532,#19533,#19534,#19535,#19536,#19537,#19538,
#19539,#19540,#19541,#19542,#19543,#19544,#19545,#19546,#19547,#19548,#19549,
#19550,#19551,#19552,#19553,#19554,#19555,#19556,#19557,#19558,#19559,#19560,
#19561,#19562,#19563,#19564,#19565,#19566,#19567,#19568,#19569,#19570,#19571,
#19572,#19573,#19574,#19575,#19576,#19577,#19578));
#4605=EDGE_LOOP('',(#19579,#19580,#19581,#19582,#19583,#19584,#19585,#19586,
#19587,#19588,#19589,#19590,#19591,#19592,#19593,#19594,#19595,#19596,#19597,
#19598,#19599,#19600,#19601,#19602,#19603,#19604,#19605,#19606,#19607,#19608,
#19609,#19610,#19611,#19612,#19613,#19614,#19615,#19616,#19617,#19618,#19619,
#19620,#19621,#19622,#19623,#19624,#19625,#19626,#19627,#19628,#19629,#19630,
#19631,#19632,#19633,#19634,#19635,#19636,#19637,#19638,#19639,#19640,#19641,
#19642,#19643,#19644,#19645,#19646,#19647,#19648,#19649,#19650,#19651,#19652,
#19653,#19654,#19655,#19656,#19657,#19658,#19659,#19660,#19661,#19662,#19663,
#19664,#19665,#19666,#19667,#19668,#19669,#19670,#19671,#19672,#19673,#19674,
#19675,#19676,#19677,#19678,#19679,#19680,#19681));
#4606=EDGE_LOOP('',(#19682,#19683,#19684,#19685,#19686,#19687,#19688,#19689,
#19690,#19691,#19692,#19693,#19694,#19695,#19696,#19697,#19698,#19699,#19700,
#19701,#19702,#19703,#19704,#19705,#19706,#19707,#19708,#19709,#19710,#19711,
#19712,#19713,#19714,#19715,#19716,#19717,#19718,#19719,#19720,#19721,#19722,
#19723,#19724,#19725,#19726,#19727,#19728,#19729,#19730,#19731,#19732,#19733,
#19734,#19735,#19736,#19737,#19738,#19739,#19740,#19741,#19742,#19743,#19744,
#19745,#19746,#19747,#19748,#19749,#19750,#19751,#19752,#19753,#19754,#19755,
#19756,#19757,#19758,#19759,#19760,#19761,#19762,#19763,#19764,#19765,#19766,
#19767,#19768,#19769,#19770,#19771,#19772,#19773,#19774,#19775,#19776,#19777,
#19778,#19779,#19780,#19781,#19782,#19783,#19784));
#4607=EDGE_LOOP('',(#19785,#19786,#19787,#19788,#19789,#19790,#19791,#19792,
#19793,#19794,#19795,#19796,#19797,#19798,#19799,#19800,#19801,#19802,#19803,
#19804,#19805,#19806,#19807,#19808,#19809,#19810,#19811,#19812,#19813,#19814,
#19815,#19816,#19817,#19818,#19819,#19820,#19821,#19822,#19823,#19824,#19825,
#19826,#19827,#19828,#19829,#19830,#19831,#19832,#19833,#19834,#19835,#19836,
#19837,#19838,#19839,#19840,#19841,#19842,#19843,#19844,#19845,#19846,#19847,
#19848,#19849,#19850,#19851,#19852,#19853,#19854,#19855,#19856,#19857,#19858,
#19859,#19860,#19861,#19862,#19863,#19864,#19865,#19866,#19867,#19868,#19869,
#19870,#19871,#19872,#19873,#19874,#19875,#19876,#19877,#19878,#19879,#19880,
#19881,#19882,#19883,#19884,#19885,#19886,#19887));
#4608=EDGE_LOOP('',(#19888,#19889,#19890,#19891,#19892,#19893,#19894,#19895,
#19896,#19897,#19898,#19899,#19900,#19901,#19902,#19903,#19904,#19905,#19906,
#19907,#19908,#19909,#19910,#19911,#19912,#19913,#19914,#19915,#19916,#19917,
#19918,#19919,#19920,#19921,#19922,#19923,#19924,#19925,#19926,#19927,#19928,
#19929,#19930,#19931,#19932,#19933,#19934,#19935,#19936,#19937,#19938,#19939,
#19940,#19941,#19942,#19943,#19944,#19945,#19946,#19947,#19948,#19949,#19950,
#19951,#19952,#19953,#19954,#19955,#19956,#19957,#19958,#19959,#19960,#19961,
#19962,#19963,#19964,#19965,#19966,#19967,#19968,#19969,#19970,#19971,#19972,
#19973,#19974,#19975,#19976,#19977,#19978,#19979,#19980,#19981,#19982,#19983,
#19984,#19985,#19986,#19987,#19988,#19989,#19990));
#4609=EDGE_LOOP('',(#19991,#19992,#19993,#19994,#19995,#19996,#19997,#19998,
#19999,#20000,#20001,#20002,#20003,#20004,#20005,#20006,#20007,#20008,#20009,
#20010,#20011,#20012,#20013,#20014,#20015,#20016,#20017,#20018,#20019,#20020,
#20021,#20022,#20023,#20024,#20025,#20026,#20027,#20028,#20029,#20030,#20031,
#20032,#20033,#20034,#20035,#20036,#20037,#20038,#20039,#20040,#20041,#20042,
#20043,#20044,#20045,#20046,#20047,#20048,#20049,#20050,#20051,#20052,#20053,
#20054,#20055,#20056,#20057,#20058,#20059,#20060,#20061,#20062,#20063,#20064,
#20065,#20066,#20067,#20068,#20069,#20070,#20071,#20072,#20073,#20074,#20075,
#20076,#20077,#20078,#20079,#20080,#20081,#20082,#20083,#20084,#20085,#20086,
#20087,#20088,#20089,#20090,#20091,#20092,#20093));
#4610=EDGE_LOOP('',(#20094,#20095,#20096,#20097,#20098,#20099,#20100,#20101,
#20102,#20103,#20104,#20105,#20106,#20107,#20108,#20109,#20110,#20111,#20112,
#20113,#20114,#20115,#20116,#20117,#20118,#20119,#20120,#20121,#20122,#20123,
#20124,#20125,#20126,#20127,#20128,#20129,#20130,#20131,#20132,#20133,#20134,
#20135,#20136,#20137,#20138,#20139,#20140,#20141,#20142,#20143,#20144,#20145,
#20146,#20147,#20148,#20149,#20150,#20151,#20152,#20153,#20154,#20155,#20156,
#20157,#20158,#20159,#20160,#20161,#20162,#20163,#20164,#20165,#20166,#20167,
#20168,#20169,#20170,#20171,#20172,#20173,#20174,#20175,#20176,#20177,#20178,
#20179,#20180,#20181,#20182,#20183,#20184,#20185,#20186,#20187,#20188,#20189,
#20190,#20191,#20192,#20193,#20194,#20195,#20196));
#4611=EDGE_LOOP('',(#20197,#20198,#20199,#20200));
#4612=EDGE_LOOP('',(#20201,#20202,#20203,#20204));
#4613=EDGE_LOOP('',(#20205,#20206,#20207,#20208));
#4614=EDGE_LOOP('',(#20209,#20210,#20211,#20212));
#4615=EDGE_LOOP('',(#20213,#20214,#20215,#20216));
#4616=EDGE_LOOP('',(#20217,#20218,#20219,#20220));
#4617=EDGE_LOOP('',(#20221,#20222,#20223,#20224));
#4618=EDGE_LOOP('',(#20225,#20226,#20227,#20228));
#4619=EDGE_LOOP('',(#20229));
#4620=EDGE_LOOP('',(#20230,#20231,#20232,#20233,#20234,#20235,#20236));
#4621=EDGE_LOOP('',(#20237,#20238,#20239,#20240));
#4622=EDGE_LOOP('',(#20241,#20242,#20243,#20244));
#4623=EDGE_LOOP('',(#20245,#20246,#20247,#20248));
#4624=EDGE_LOOP('',(#20249,#20250,#20251,#20252));
#4625=EDGE_LOOP('',(#20253,#20254,#20255,#20256));
#4626=EDGE_LOOP('',(#20257,#20258,#20259,#20260,#20261,#20262));
#4627=EDGE_LOOP('',(#20263,#20264,#20265,#20266));
#4628=EDGE_LOOP('',(#20267));
#4629=EDGE_LOOP('',(#20268));
#4630=EDGE_LOOP('',(#20269,#20270,#20271,#20272));
#4631=EDGE_LOOP('',(#20273,#20274,#20275,#20276));
#4632=EDGE_LOOP('',(#20277,#20278,#20279,#20280));
#4633=EDGE_LOOP('',(#20281,#20282,#20283,#20284));
#4634=EDGE_LOOP('',(#20285,#20286,#20287,#20288));
#4635=EDGE_LOOP('',(#20289,#20290,#20291,#20292));
#4636=EDGE_LOOP('',(#20293,#20294,#20295,#20296));
#4637=EDGE_LOOP('',(#20297,#20298,#20299,#20300));
#4638=EDGE_LOOP('',(#20301));
#4639=EDGE_LOOP('',(#20302,#20303,#20304,#20305,#20306,#20307,#20308));
#4640=EDGE_LOOP('',(#20309,#20310,#20311,#20312,#20313,#20314,#20315));
#4641=EDGE_LOOP('',(#20316,#20317,#20318,#20319,#20320,#20321,#20322));
#4642=EDGE_LOOP('',(#20323,#20324,#20325,#20326));
#4643=EDGE_LOOP('',(#20327));
#4644=EDGE_LOOP('',(#20328,#20329,#20330,#20331,#20332));
#4645=EDGE_LOOP('',(#20333,#20334,#20335,#20336));
#4646=EDGE_LOOP('',(#20337));
#4647=EDGE_LOOP('',(#20338,#20339,#20340,#20341));
#4648=EDGE_LOOP('',(#20342,#20343,#20344,#20345));
#4649=EDGE_LOOP('',(#20346,#20347,#20348,#20349));
#4650=EDGE_LOOP('',(#20350,#20351,#20352,#20353));
#4651=EDGE_LOOP('',(#20354,#20355,#20356,#20357));
#4652=EDGE_LOOP('',(#20358,#20359,#20360,#20361,#20362,#20363));
#4653=EDGE_LOOP('',(#20364,#20365,#20366,#20367));
#4654=EDGE_LOOP('',(#20368));
#4655=EDGE_LOOP('',(#20369));
#4656=EDGE_LOOP('',(#20370,#20371,#20372,#20373));
#4657=EDGE_LOOP('',(#20374,#20375,#20376,#20377));
#4658=EDGE_LOOP('',(#20378,#20379,#20380,#20381));
#4659=EDGE_LOOP('',(#20382,#20383,#20384,#20385));
#4660=EDGE_LOOP('',(#20386,#20387,#20388,#20389));
#4661=EDGE_LOOP('',(#20390,#20391,#20392,#20393));
#4662=EDGE_LOOP('',(#20394,#20395,#20396,#20397));
#4663=EDGE_LOOP('',(#20398,#20399,#20400,#20401));
#4664=EDGE_LOOP('',(#20402));
#4665=EDGE_LOOP('',(#20403,#20404,#20405,#20406,#20407,#20408,#20409));
#4666=EDGE_LOOP('',(#20410,#20411,#20412,#20413));
#4667=EDGE_LOOP('',(#20414,#20415,#20416,#20417));
#4668=EDGE_LOOP('',(#20418,#20419,#20420,#20421));
#4669=EDGE_LOOP('',(#20422,#20423,#20424,#20425));
#4670=EDGE_LOOP('',(#20426,#20427,#20428,#20429));
#4671=EDGE_LOOP('',(#20430,#20431,#20432,#20433));
#4672=EDGE_LOOP('',(#20434,#20435,#20436,#20437));
#4673=EDGE_LOOP('',(#20438,#20439,#20440,#20441));
#4674=EDGE_LOOP('',(#20442));
#4675=EDGE_LOOP('',(#20443,#20444,#20445,#20446,#20447,#20448,#20449));
#4676=EDGE_LOOP('',(#20450,#20451,#20452,#20453,#20454,#20455,#20456));
#4677=EDGE_LOOP('',(#20457,#20458,#20459,#20460,#20461,#20462,#20463));
#4678=EDGE_LOOP('',(#20464,#20465,#20466,#20467,#20468,#20469,#20470,#20471,
#20472,#20473));
#4679=EDGE_LOOP('',(#20474));
#4680=EDGE_LOOP('',(#20475));
#4681=EDGE_LOOP('',(#20476,#20477,#20478,#20479,#20480));
#4682=EDGE_LOOP('',(#20481,#20482,#20483,#20484));
#4683=EDGE_LOOP('',(#20485));
#4684=EDGE_LOOP('',(#20486,#20487,#20488,#20489));
#4685=EDGE_LOOP('',(#20490));
#4686=EDGE_LOOP('',(#20491,#20492,#20493,#20494));
#4687=EDGE_LOOP('',(#20495));
#4688=EDGE_LOOP('',(#20496,#20497,#20498,#20499));
#4689=EDGE_LOOP('',(#20500));
#4690=EDGE_LOOP('',(#20501,#20502,#20503,#20504));
#4691=EDGE_LOOP('',(#20505,#20506,#20507,#20508));
#4692=EDGE_LOOP('',(#20509,#20510,#20511,#20512));
#4693=EDGE_LOOP('',(#20513,#20514,#20515,#20516));
#4694=EDGE_LOOP('',(#20517,#20518,#20519,#20520));
#4695=EDGE_LOOP('',(#20521,#20522,#20523,#20524));
#4696=EDGE_LOOP('',(#20525,#20526,#20527,#20528));
#4697=EDGE_LOOP('',(#20529,#20530,#20531,#20532));
#4698=EDGE_LOOP('',(#20533,#20534,#20535,#20536));
#4699=EDGE_LOOP('',(#20537,#20538,#20539,#20540));
#4700=EDGE_LOOP('',(#20541,#20542,#20543,#20544));
#4701=EDGE_LOOP('',(#20545,#20546,#20547,#20548));
#4702=EDGE_LOOP('',(#20549,#20550,#20551,#20552,#20553,#20554,#20555,#20556,
#20557,#20558));
#4703=EDGE_LOOP('',(#20559));
#4704=EDGE_LOOP('',(#20560));
#4705=EDGE_LOOP('',(#20561,#20562,#20563,#20564));
#4706=EDGE_LOOP('',(#20565,#20566,#20567,#20568));
#4707=EDGE_LOOP('',(#20569,#20570,#20571,#20572));
#4708=EDGE_LOOP('',(#20573,#20574,#20575,#20576));
#4709=EDGE_LOOP('',(#20577,#20578,#20579,#20580));
#4710=EDGE_LOOP('',(#20581,#20582,#20583,#20584));
#4711=EDGE_LOOP('',(#20585,#20586,#20587,#20588));
#4712=EDGE_LOOP('',(#20589,#20590,#20591,#20592,#20593,#20594));
#4713=EDGE_LOOP('',(#20595,#20596,#20597,#20598));
#4714=EDGE_LOOP('',(#20599,#20600,#20601,#20602,#20603,#20604,#20605,#20606,
#20607,#20608,#20609,#20610,#20611,#20612,#20613,#20614,#20615,#20616,#20617,
#20618,#20619,#20620,#20621,#20622,#20623,#20624));
#4715=EDGE_LOOP('',(#20625,#20626,#20627,#20628));
#4716=EDGE_LOOP('',(#20629,#20630,#20631,#20632));
#4717=EDGE_LOOP('',(#20633,#20634,#20635,#20636));
#4718=EDGE_LOOP('',(#20637,#20638,#20639,#20640));
#4719=EDGE_LOOP('',(#20641,#20642,#20643,#20644));
#4720=EDGE_LOOP('',(#20645));
#4721=EDGE_LOOP('',(#20646,#20647,#20648,#20649));
#4722=EDGE_LOOP('',(#20650));
#4723=EDGE_LOOP('',(#20651,#20652,#20653,#20654));
#4724=EDGE_LOOP('',(#20655,#20656,#20657,#20658));
#4725=EDGE_LOOP('',(#20659,#20660,#20661,#20662));
#4726=EDGE_LOOP('',(#20663,#20664,#20665,#20666));
#4727=EDGE_LOOP('',(#20667,#20668,#20669,#20670));
#4728=EDGE_LOOP('',(#20671,#20672,#20673,#20674));
#4729=EDGE_LOOP('',(#20675,#20676,#20677,#20678));
#4730=EDGE_LOOP('',(#20679,#20680,#20681,#20682));
#4731=EDGE_LOOP('',(#20683,#20684,#20685,#20686));
#4732=EDGE_LOOP('',(#20687,#20688,#20689,#20690));
#4733=EDGE_LOOP('',(#20691,#20692,#20693,#20694));
#4734=EDGE_LOOP('',(#20695,#20696,#20697,#20698));
#4735=EDGE_LOOP('',(#20699,#20700,#20701,#20702));
#4736=EDGE_LOOP('',(#20703,#20704,#20705,#20706));
#4737=EDGE_LOOP('',(#20707,#20708,#20709,#20710));
#4738=EDGE_LOOP('',(#20711,#20712,#20713,#20714));
#4739=EDGE_LOOP('',(#20715,#20716,#20717,#20718));
#4740=EDGE_LOOP('',(#20719,#20720,#20721,#20722));
#4741=EDGE_LOOP('',(#20723,#20724,#20725,#20726));
#4742=EDGE_LOOP('',(#20727,#20728,#20729,#20730));
#4743=EDGE_LOOP('',(#20731,#20732,#20733,#20734));
#4744=EDGE_LOOP('',(#20735,#20736,#20737,#20738));
#4745=EDGE_LOOP('',(#20739,#20740,#20741,#20742));
#4746=EDGE_LOOP('',(#20743,#20744,#20745,#20746));
#4747=EDGE_LOOP('',(#20747,#20748,#20749,#20750));
#4748=EDGE_LOOP('',(#20751,#20752,#20753,#20754));
#4749=EDGE_LOOP('',(#20755,#20756,#20757,#20758));
#4750=EDGE_LOOP('',(#20759,#20760,#20761,#20762));
#4751=EDGE_LOOP('',(#20763,#20764,#20765,#20766));
#4752=EDGE_LOOP('',(#20767,#20768,#20769,#20770));
#4753=EDGE_LOOP('',(#20771,#20772,#20773,#20774));
#4754=EDGE_LOOP('',(#20775,#20776,#20777,#20778));
#4755=EDGE_LOOP('',(#20779,#20780,#20781));
#4756=EDGE_LOOP('',(#20782,#20783,#20784));
#4757=EDGE_LOOP('',(#20785,#20786,#20787,#20788));
#4758=EDGE_LOOP('',(#20789,#20790,#20791,#20792));
#4759=EDGE_LOOP('',(#20793,#20794,#20795,#20796));
#4760=EDGE_LOOP('',(#20797,#20798,#20799,#20800));
#4761=EDGE_LOOP('',(#20801,#20802,#20803,#20804));
#4762=EDGE_LOOP('',(#20805,#20806,#20807,#20808));
#4763=EDGE_LOOP('',(#20809,#20810,#20811,#20812));
#4764=EDGE_LOOP('',(#20813));
#4765=EDGE_LOOP('',(#20814,#20815,#20816,#20817));
#4766=EDGE_LOOP('',(#20818,#20819,#20820,#20821));
#4767=EDGE_LOOP('',(#20822,#20823,#20824,#20825,#20826,#20827));
#4768=EDGE_LOOP('',(#20828,#20829,#20830,#20831));
#4769=EDGE_LOOP('',(#20832,#20833,#20834,#20835));
#4770=EDGE_LOOP('',(#20836,#20837,#20838,#20839,#20840,#20841));
#4771=EDGE_LOOP('',(#20842,#20843,#20844,#20845));
#4772=EDGE_LOOP('',(#20846,#20847,#20848,#20849));
#4773=EDGE_LOOP('',(#20850,#20851,#20852,#20853));
#4774=EDGE_LOOP('',(#20854,#20855,#20856,#20857));
#4775=EDGE_LOOP('',(#20858,#20859,#20860,#20861,#20862,#20863,#20864,#20865,
#20866,#20867,#20868,#20869,#20870,#20871,#20872,#20873,#20874,#20875,#20876,
#20877,#20878,#20879,#20880,#20881,#20882,#20883,#20884,#20885,#20886,#20887,
#20888,#20889));
#4776=EDGE_LOOP('',(#20890,#20891,#20892,#20893));
#4777=EDGE_LOOP('',(#20894,#20895,#20896,#20897,#20898));
#4778=EDGE_LOOP('',(#20899,#20900,#20901,#20902));
#4779=EDGE_LOOP('',(#20903,#20904,#20905,#20906));
#4780=EDGE_LOOP('',(#20907,#20908,#20909,#20910));
#4781=EDGE_LOOP('',(#20911,#20912,#20913));
#4782=EDGE_LOOP('',(#20914,#20915,#20916,#20917,#20918));
#4783=EDGE_LOOP('',(#20919,#20920,#20921,#20922));
#4784=EDGE_LOOP('',(#20923,#20924,#20925));
#4785=EDGE_LOOP('',(#20926,#20927,#20928,#20929,#20930));
#4786=EDGE_LOOP('',(#20931,#20932,#20933,#20934,#20935,#20936,#20937,#20938,
#20939,#20940,#20941,#20942,#20943,#20944,#20945,#20946,#20947,#20948,#20949,
#20950,#20951,#20952,#20953,#20954,#20955,#20956,#20957,#20958));
#4787=EDGE_LOOP('',(#20959,#20960,#20961,#20962,#20963));
#4788=EDGE_LOOP('',(#20964,#20965,#20966));
#4789=EDGE_LOOP('',(#20967,#20968,#20969,#20970));
#4790=EDGE_LOOP('',(#20971,#20972,#20973,#20974));
#4791=EDGE_LOOP('',(#20975,#20976,#20977,#20978));
#4792=EDGE_LOOP('',(#20979,#20980,#20981,#20982));
#4793=EDGE_LOOP('',(#20983,#20984,#20985));
#4794=EDGE_LOOP('',(#20986,#20987,#20988,#20989));
#4795=EDGE_LOOP('',(#20990,#20991,#20992,#20993));
#4796=EDGE_LOOP('',(#20994,#20995,#20996,#20997));
#4797=EDGE_LOOP('',(#20998,#20999,#21000,#21001));
#4798=EDGE_LOOP('',(#21002,#21003,#21004,#21005));
#4799=EDGE_LOOP('',(#21006,#21007,#21008,#21009));
#4800=EDGE_LOOP('',(#21010,#21011,#21012,#21013));
#4801=EDGE_LOOP('',(#21014,#21015,#21016,#21017));
#4802=EDGE_LOOP('',(#21018,#21019,#21020,#21021));
#4803=EDGE_LOOP('',(#21022,#21023,#21024,#21025));
#4804=EDGE_LOOP('',(#21026,#21027,#21028,#21029));
#4805=EDGE_LOOP('',(#21030,#21031,#21032,#21033));
#4806=EDGE_LOOP('',(#21034,#21035,#21036,#21037));
#4807=EDGE_LOOP('',(#21038,#21039,#21040,#21041));
#4808=EDGE_LOOP('',(#21042,#21043,#21044,#21045));
#4809=EDGE_LOOP('',(#21046,#21047,#21048,#21049));
#4810=EDGE_LOOP('',(#21050,#21051,#21052,#21053));
#4811=EDGE_LOOP('',(#21054,#21055,#21056,#21057));
#4812=EDGE_LOOP('',(#21058,#21059,#21060,#21061));
#4813=EDGE_LOOP('',(#21062,#21063,#21064,#21065));
#4814=EDGE_LOOP('',(#21066,#21067,#21068,#21069));
#4815=EDGE_LOOP('',(#21070,#21071,#21072,#21073));
#4816=EDGE_LOOP('',(#21074,#21075,#21076,#21077));
#4817=EDGE_LOOP('',(#21078,#21079,#21080,#21081));
#4818=EDGE_LOOP('',(#21082,#21083,#21084,#21085));
#4819=EDGE_LOOP('',(#21086));
#4820=EDGE_LOOP('',(#21087,#21088,#21089,#21090));
#4821=EDGE_LOOP('',(#21091,#21092,#21093,#21094));
#4822=EDGE_LOOP('',(#21095,#21096,#21097,#21098,#21099,#21100));
#4823=EDGE_LOOP('',(#21101,#21102,#21103,#21104));
#4824=EDGE_LOOP('',(#21105,#21106,#21107,#21108));
#4825=EDGE_LOOP('',(#21109,#21110,#21111,#21112,#21113));
#4826=EDGE_LOOP('',(#21114,#21115,#21116,#21117,#21118));
#4827=EDGE_LOOP('',(#21119,#21120,#21121,#21122));
#4828=EDGE_LOOP('',(#21123,#21124,#21125,#21126));
#4829=EDGE_LOOP('',(#21127,#21128,#21129,#21130,#21131,#21132));
#4830=EDGE_LOOP('',(#21133,#21134,#21135,#21136));
#4831=EDGE_LOOP('',(#21137,#21138,#21139,#21140));
#4832=EDGE_LOOP('',(#21141));
#4833=EDGE_LOOP('',(#21142,#21143,#21144,#21145));
#4834=EDGE_LOOP('',(#21146));
#4835=EDGE_LOOP('',(#21147,#21148,#21149,#21150));
#4836=EDGE_LOOP('',(#21151,#21152,#21153,#21154));
#4837=EDGE_LOOP('',(#21155,#21156,#21157,#21158));
#4838=EDGE_LOOP('',(#21159,#21160,#21161,#21162));
#4839=EDGE_LOOP('',(#21163,#21164,#21165,#21166));
#4840=EDGE_LOOP('',(#21167,#21168,#21169,#21170));
#4841=EDGE_LOOP('',(#21171,#21172,#21173,#21174));
#4842=EDGE_LOOP('',(#21175,#21176,#21177,#21178));
#4843=EDGE_LOOP('',(#21179,#21180,#21181,#21182));
#4844=EDGE_LOOP('',(#21183,#21184,#21185,#21186));
#4845=EDGE_LOOP('',(#21187,#21188,#21189,#21190));
#4846=EDGE_LOOP('',(#21191,#21192,#21193,#21194));
#4847=EDGE_LOOP('',(#21195,#21196,#21197,#21198));
#4848=EDGE_LOOP('',(#21199,#21200,#21201,#21202));
#4849=EDGE_LOOP('',(#21203,#21204,#21205,#21206));
#4850=EDGE_LOOP('',(#21207,#21208,#21209,#21210));
#4851=EDGE_LOOP('',(#21211,#21212,#21213,#21214));
#4852=EDGE_LOOP('',(#21215,#21216,#21217,#21218));
#4853=EDGE_LOOP('',(#21219,#21220,#21221,#21222));
#4854=EDGE_LOOP('',(#21223,#21224,#21225,#21226));
#4855=EDGE_LOOP('',(#21227,#21228,#21229,#21230));
#4856=EDGE_LOOP('',(#21231,#21232,#21233,#21234));
#4857=EDGE_LOOP('',(#21235,#21236,#21237,#21238));
#4858=EDGE_LOOP('',(#21239,#21240,#21241,#21242));
#4859=EDGE_LOOP('',(#21243,#21244,#21245,#21246));
#4860=EDGE_LOOP('',(#21247,#21248,#21249,#21250));
#4861=EDGE_LOOP('',(#21251,#21252,#21253,#21254));
#4862=EDGE_LOOP('',(#21255,#21256,#21257,#21258));
#4863=EDGE_LOOP('',(#21259,#21260,#21261,#21262));
#4864=EDGE_LOOP('',(#21263,#21264,#21265,#21266));
#4865=EDGE_LOOP('',(#21267,#21268,#21269,#21270));
#4866=EDGE_LOOP('',(#21271,#21272,#21273,#21274));
#4867=EDGE_LOOP('',(#21275,#21276,#21277));
#4868=EDGE_LOOP('',(#21278,#21279,#21280));
#4869=EDGE_LOOP('',(#21281,#21282,#21283,#21284));
#4870=EDGE_LOOP('',(#21285,#21286,#21287,#21288));
#4871=EDGE_LOOP('',(#21289,#21290,#21291,#21292));
#4872=EDGE_LOOP('',(#21293,#21294,#21295,#21296));
#4873=EDGE_LOOP('',(#21297,#21298,#21299,#21300));
#4874=EDGE_LOOP('',(#21301,#21302,#21303,#21304));
#4875=EDGE_LOOP('',(#21305,#21306,#21307,#21308));
#4876=EDGE_LOOP('',(#21309));
#4877=EDGE_LOOP('',(#21310,#21311,#21312,#21313));
#4878=EDGE_LOOP('',(#21314,#21315,#21316,#21317));
#4879=EDGE_LOOP('',(#21318,#21319,#21320,#21321,#21322,#21323));
#4880=EDGE_LOOP('',(#21324,#21325,#21326,#21327));
#4881=EDGE_LOOP('',(#21328,#21329,#21330,#21331));
#4882=EDGE_LOOP('',(#21332,#21333,#21334,#21335,#21336,#21337));
#4883=EDGE_LOOP('',(#21338,#21339,#21340,#21341));
#4884=EDGE_LOOP('',(#21342,#21343,#21344,#21345));
#4885=EDGE_LOOP('',(#21346,#21347,#21348,#21349));
#4886=EDGE_LOOP('',(#21350,#21351,#21352,#21353));
#4887=EDGE_LOOP('',(#21354,#21355,#21356,#21357,#21358,#21359,#21360,#21361,
#21362,#21363,#21364,#21365,#21366,#21367,#21368,#21369,#21370,#21371,#21372,
#21373,#21374,#21375,#21376,#21377,#21378,#21379,#21380,#21381,#21382,#21383,
#21384,#21385));
#4888=EDGE_LOOP('',(#21386,#21387,#21388,#21389));
#4889=EDGE_LOOP('',(#21390,#21391,#21392,#21393,#21394));
#4890=EDGE_LOOP('',(#21395,#21396,#21397,#21398));
#4891=EDGE_LOOP('',(#21399,#21400,#21401,#21402));
#4892=EDGE_LOOP('',(#21403,#21404,#21405,#21406));
#4893=EDGE_LOOP('',(#21407,#21408,#21409));
#4894=EDGE_LOOP('',(#21410,#21411,#21412,#21413,#21414));
#4895=EDGE_LOOP('',(#21415,#21416,#21417,#21418));
#4896=EDGE_LOOP('',(#21419,#21420,#21421));
#4897=EDGE_LOOP('',(#21422,#21423,#21424,#21425,#21426));
#4898=EDGE_LOOP('',(#21427,#21428,#21429,#21430,#21431,#21432,#21433,#21434,
#21435,#21436,#21437,#21438,#21439,#21440,#21441,#21442,#21443,#21444,#21445,
#21446,#21447,#21448,#21449,#21450,#21451,#21452,#21453,#21454));
#4899=EDGE_LOOP('',(#21455,#21456,#21457,#21458,#21459));
#4900=EDGE_LOOP('',(#21460,#21461,#21462));
#4901=EDGE_LOOP('',(#21463,#21464,#21465,#21466));
#4902=EDGE_LOOP('',(#21467,#21468,#21469,#21470));
#4903=EDGE_LOOP('',(#21471,#21472,#21473,#21474));
#4904=EDGE_LOOP('',(#21475,#21476,#21477,#21478));
#4905=EDGE_LOOP('',(#21479,#21480,#21481));
#4906=EDGE_LOOP('',(#21482,#21483,#21484,#21485));
#4907=EDGE_LOOP('',(#21486,#21487,#21488,#21489));
#4908=EDGE_LOOP('',(#21490,#21491,#21492,#21493));
#4909=EDGE_LOOP('',(#21494,#21495,#21496,#21497));
#4910=EDGE_LOOP('',(#21498,#21499,#21500,#21501));
#4911=EDGE_LOOP('',(#21502,#21503,#21504,#21505));
#4912=EDGE_LOOP('',(#21506,#21507,#21508,#21509));
#4913=EDGE_LOOP('',(#21510,#21511,#21512,#21513));
#4914=EDGE_LOOP('',(#21514,#21515,#21516,#21517));
#4915=EDGE_LOOP('',(#21518,#21519,#21520,#21521));
#4916=EDGE_LOOP('',(#21522,#21523,#21524,#21525));
#4917=EDGE_LOOP('',(#21526,#21527,#21528,#21529));
#4918=EDGE_LOOP('',(#21530,#21531,#21532,#21533));
#4919=EDGE_LOOP('',(#21534,#21535,#21536,#21537));
#4920=EDGE_LOOP('',(#21538,#21539,#21540,#21541));
#4921=EDGE_LOOP('',(#21542,#21543,#21544,#21545));
#4922=EDGE_LOOP('',(#21546,#21547,#21548,#21549));
#4923=EDGE_LOOP('',(#21550,#21551,#21552,#21553));
#4924=EDGE_LOOP('',(#21554,#21555,#21556,#21557));
#4925=EDGE_LOOP('',(#21558,#21559,#21560,#21561));
#4926=EDGE_LOOP('',(#21562,#21563,#21564,#21565));
#4927=EDGE_LOOP('',(#21566,#21567,#21568,#21569));
#4928=EDGE_LOOP('',(#21570,#21571,#21572,#21573));
#4929=EDGE_LOOP('',(#21574,#21575,#21576,#21577));
#4930=EDGE_LOOP('',(#21578,#21579,#21580,#21581));
#4931=EDGE_LOOP('',(#21582));
#4932=EDGE_LOOP('',(#21583,#21584,#21585,#21586));
#4933=EDGE_LOOP('',(#21587,#21588,#21589,#21590));
#4934=EDGE_LOOP('',(#21591,#21592,#21593,#21594,#21595,#21596));
#4935=EDGE_LOOP('',(#21597,#21598,#21599,#21600));
#4936=EDGE_LOOP('',(#21601,#21602,#21603,#21604));
#4937=EDGE_LOOP('',(#21605,#21606,#21607,#21608,#21609));
#4938=EDGE_LOOP('',(#21610,#21611,#21612,#21613,#21614));
#4939=EDGE_LOOP('',(#21615,#21616,#21617,#21618));
#4940=EDGE_LOOP('',(#21619,#21620,#21621,#21622));
#4941=EDGE_LOOP('',(#21623,#21624,#21625,#21626,#21627,#21628));
#4942=EDGE_LOOP('',(#21629,#21630,#21631,#21632));
#4943=EDGE_LOOP('',(#21633,#21634,#21635,#21636,#21637));
#4944=EDGE_LOOP('',(#21638));
#4945=EDGE_LOOP('',(#21639,#21640,#21641,#21642,#21643));
#4946=EDGE_LOOP('',(#21644));
#4947=EDGE_LOOP('',(#21645,#21646,#21647,#21648,#21649,#21650,#21651,#21652));
#4948=EDGE_LOOP('',(#21653,#21654));
#4949=EDGE_LOOP('',(#21655,#21656,#21657,#21658,#21659,#21660,#21661,#21662,
#21663,#21664,#21665,#21666,#21667,#21668,#21669,#21670,#21671,#21672,#21673,
#21674,#21675,#21676,#21677,#21678,#21679,#21680,#21681,#21682,#21683,#21684,
#21685,#21686,#21687,#21688,#21689,#21690,#21691,#21692,#21693,#21694,#21695,
#21696,#21697,#21698,#21699,#21700,#21701,#21702,#21703,#21704,#21705,#21706,
#21707,#21708,#21709,#21710,#21711,#21712,#21713,#21714,#21715,#21716));
#4950=EDGE_LOOP('',(#21717,#21718));
#4951=EDGE_LOOP('',(#21719,#21720,#21721,#21722,#21723,#21724,#21725,#21726,
#21727,#21728,#21729,#21730,#21731,#21732,#21733,#21734,#21735,#21736,#21737,
#21738,#21739,#21740,#21741,#21742,#21743,#21744,#21745,#21746,#21747,#21748,
#21749,#21750,#21751,#21752,#21753,#21754,#21755,#21756,#21757,#21758,#21759,
#21760,#21761,#21762,#21763,#21764,#21765,#21766,#21767,#21768,#21769,#21770,
#21771,#21772,#21773,#21774,#21775,#21776,#21777,#21778,#21779,#21780));
#4952=EDGE_LOOP('',(#21781,#21782));
#4953=EDGE_LOOP('',(#21783,#21784,#21785,#21786,#21787,#21788,#21789,#21790,
#21791,#21792,#21793,#21794,#21795,#21796,#21797,#21798,#21799,#21800,#21801,
#21802,#21803,#21804,#21805,#21806,#21807,#21808,#21809,#21810,#21811,#21812,
#21813,#21814,#21815,#21816,#21817,#21818,#21819,#21820,#21821,#21822,#21823,
#21824,#21825,#21826,#21827,#21828,#21829,#21830,#21831,#21832,#21833,#21834,
#21835,#21836,#21837,#21838,#21839,#21840,#21841,#21842,#21843,#21844));
#4954=EDGE_LOOP('',(#21845,#21846,#21847,#21848,#21849,#21850,#21851,#21852,
#21853,#21854));
#4955=EDGE_LOOP('',(#21855,#21856,#21857,#21858));
#4956=EDGE_LOOP('',(#21859,#21860,#21861,#21862));
#4957=EDGE_LOOP('',(#21863,#21864,#21865,#21866));
#4958=EDGE_LOOP('',(#21867,#21868,#21869,#21870));
#4959=EDGE_LOOP('',(#21871,#21872,#21873,#21874));
#4960=EDGE_LOOP('',(#21875,#21876,#21877,#21878));
#4961=EDGE_LOOP('',(#21879,#21880,#21881,#21882));
#4962=EDGE_LOOP('',(#21883,#21884,#21885,#21886));
#4963=EDGE_LOOP('',(#21887,#21888,#21889,#21890));
#4964=EDGE_LOOP('',(#21891,#21892,#21893,#21894,#21895));
#4965=EDGE_LOOP('',(#21896,#21897,#21898,#21899));
#4966=EDGE_LOOP('',(#21900,#21901,#21902,#21903,#21904));
#4967=EDGE_LOOP('',(#21905,#21906,#21907,#21908));
#4968=EDGE_LOOP('',(#21909,#21910,#21911,#21912));
#4969=EDGE_LOOP('',(#21913,#21914,#21915,#21916));
#4970=EDGE_LOOP('',(#21917,#21918,#21919,#21920));
#4971=EDGE_LOOP('',(#21921,#21922,#21923,#21924));
#4972=EDGE_LOOP('',(#21925,#21926,#21927,#21928));
#4973=EDGE_LOOP('',(#21929,#21930,#21931,#21932));
#4974=EDGE_LOOP('',(#21933,#21934,#21935,#21936));
#4975=EDGE_LOOP('',(#21937,#21938,#21939,#21940));
#4976=EDGE_LOOP('',(#21941,#21942,#21943,#21944));
#4977=EDGE_LOOP('',(#21945,#21946,#21947,#21948));
#4978=EDGE_LOOP('',(#21949,#21950,#21951,#21952));
#4979=EDGE_LOOP('',(#21953,#21954,#21955,#21956,#21957));
#4980=EDGE_LOOP('',(#21958,#21959,#21960,#21961));
#4981=EDGE_LOOP('',(#21962,#21963,#21964,#21965,#21966));
#4982=EDGE_LOOP('',(#21967,#21968,#21969,#21970));
#4983=EDGE_LOOP('',(#21971,#21972,#21973,#21974));
#4984=EDGE_LOOP('',(#21975,#21976,#21977,#21978));
#4985=EDGE_LOOP('',(#21979,#21980,#21981,#21982));
#4986=EDGE_LOOP('',(#21983,#21984,#21985,#21986));
#4987=EDGE_LOOP('',(#21987,#21988,#21989,#21990));
#4988=EDGE_LOOP('',(#21991,#21992,#21993,#21994,#21995,#21996,#21997,#21998,
#21999,#22000));
#4989=EDGE_LOOP('',(#22001,#22002,#22003,#22004));
#4990=EDGE_LOOP('',(#22005,#22006,#22007,#22008));
#4991=EDGE_LOOP('',(#22009,#22010,#22011,#22012));
#4992=EDGE_LOOP('',(#22013,#22014,#22015,#22016));
#4993=EDGE_LOOP('',(#22017,#22018,#22019,#22020));
#4994=EDGE_LOOP('',(#22021,#22022,#22023,#22024));
#4995=EDGE_LOOP('',(#22025,#22026,#22027,#22028));
#4996=EDGE_LOOP('',(#22029,#22030,#22031,#22032));
#4997=EDGE_LOOP('',(#22033,#22034,#22035,#22036));
#4998=EDGE_LOOP('',(#22037,#22038,#22039,#22040));
#4999=EDGE_LOOP('',(#22041,#22042,#22043,#22044,#22045));
#5000=EDGE_LOOP('',(#22046,#22047,#22048,#22049,#22050));
#5001=EDGE_LOOP('',(#22051,#22052,#22053,#22054));
#5002=EDGE_LOOP('',(#22055,#22056,#22057,#22058));
#5003=EDGE_LOOP('',(#22059,#22060,#22061,#22062));
#5004=EDGE_LOOP('',(#22063,#22064,#22065,#22066));
#5005=EDGE_LOOP('',(#22067,#22068,#22069,#22070));
#5006=EDGE_LOOP('',(#22071,#22072,#22073,#22074));
#5007=EDGE_LOOP('',(#22075,#22076,#22077,#22078));
#5008=EDGE_LOOP('',(#22079,#22080,#22081,#22082));
#5009=EDGE_LOOP('',(#22083,#22084,#22085,#22086));
#5010=EDGE_LOOP('',(#22087,#22088,#22089,#22090));
#5011=EDGE_LOOP('',(#22091,#22092,#22093,#22094));
#5012=EDGE_LOOP('',(#22095,#22096,#22097,#22098));
#5013=EDGE_LOOP('',(#22099,#22100,#22101,#22102));
#5014=EDGE_LOOP('',(#22103,#22104,#22105,#22106,#22107));
#5015=EDGE_LOOP('',(#22108,#22109,#22110,#22111,#22112));
#5016=EDGE_LOOP('',(#22113,#22114,#22115,#22116));
#5017=EDGE_LOOP('',(#22117,#22118,#22119,#22120));
#5018=EDGE_LOOP('',(#22121,#22122,#22123,#22124));
#5019=EDGE_LOOP('',(#22125,#22126,#22127,#22128));
#5020=EDGE_LOOP('',(#22129,#22130,#22131,#22132));
#5021=EDGE_LOOP('',(#22133,#22134,#22135,#22136));
#5022=EDGE_LOOP('',(#22137,#22138,#22139,#22140));
#5023=EDGE_LOOP('',(#22141,#22142,#22143,#22144));
#5024=EDGE_LOOP('',(#22145,#22146,#22147,#22148));
#5025=EDGE_LOOP('',(#22149,#22150,#22151,#22152));
#5026=EDGE_LOOP('',(#22153,#22154,#22155,#22156,#22157,#22158,#22159,#22160));
#5027=EDGE_LOOP('',(#22161,#22162,#22163,#22164));
#5028=EDGE_LOOP('',(#22165,#22166,#22167,#22168));
#5029=EDGE_LOOP('',(#22169,#22170,#22171,#22172,#22173,#22174,#22175,#22176,
#22177,#22178));
#5030=EDGE_LOOP('',(#22179,#22180,#22181,#22182));
#5031=EDGE_LOOP('',(#22183,#22184,#22185,#22186));
#5032=EDGE_LOOP('',(#22187,#22188,#22189,#22190,#22191));
#5033=EDGE_LOOP('',(#22192,#22193,#22194,#22195));
#5034=EDGE_LOOP('',(#22196,#22197,#22198,#22199));
#5035=EDGE_LOOP('',(#22200,#22201,#22202,#22203));
#5036=EDGE_LOOP('',(#22204,#22205,#22206,#22207));
#5037=EDGE_LOOP('',(#22208,#22209,#22210,#22211,#22212));
#5038=EDGE_LOOP('',(#22213,#22214,#22215,#22216));
#5039=EDGE_LOOP('',(#22217,#22218,#22219,#22220));
#5040=EDGE_LOOP('',(#22221,#22222,#22223,#22224));
#5041=EDGE_LOOP('',(#22225,#22226,#22227,#22228));
#5042=EDGE_LOOP('',(#22229,#22230,#22231,#22232));
#5043=EDGE_LOOP('',(#22233,#22234,#22235,#22236));
#5044=EDGE_LOOP('',(#22237,#22238,#22239,#22240));
#5045=EDGE_LOOP('',(#22241,#22242,#22243,#22244));
#5046=EDGE_LOOP('',(#22245));
#5047=EDGE_LOOP('',(#22246));
#5048=EDGE_LOOP('',(#22247));
#5049=EDGE_LOOP('',(#22248,#22249,#22250,#22251));
#5050=EDGE_LOOP('',(#22252,#22253,#22254,#22255));
#5051=EDGE_LOOP('',(#22256,#22257,#22258,#22259));
#5052=EDGE_LOOP('',(#22260,#22261,#22262,#22263));
#5053=EDGE_LOOP('',(#22264,#22265,#22266,#22267));
#5054=EDGE_LOOP('',(#22268,#22269,#22270,#22271));
#5055=EDGE_LOOP('',(#22272));
#5056=EDGE_LOOP('',(#22273));
#5057=EDGE_LOOP('',(#22274));
#5058=EDGE_LOOP('',(#22275,#22276,#22277,#22278));
#5059=EDGE_LOOP('',(#22279,#22280,#22281,#22282));
#5060=EDGE_LOOP('',(#22283,#22284,#22285,#22286));
#5061=EDGE_LOOP('',(#22287,#22288,#22289,#22290));
#5062=EDGE_LOOP('',(#22291));
#5063=EDGE_LOOP('',(#22292));
#5064=EDGE_LOOP('',(#22293));
#5065=EDGE_LOOP('',(#22294,#22295,#22296,#22297));
#5066=EDGE_LOOP('',(#22298,#22299,#22300,#22301));
#5067=EDGE_LOOP('',(#22302,#22303,#22304,#22305));
#5068=EDGE_LOOP('',(#22306,#22307,#22308,#22309));
#5069=EDGE_LOOP('',(#22310,#22311,#22312,#22313));
#5070=EDGE_LOOP('',(#22314,#22315,#22316,#22317));
#5071=EDGE_LOOP('',(#22318,#22319,#22320,#22321));
#5072=EDGE_LOOP('',(#22322,#22323,#22324,#22325,#22326,#22327,#22328,#22329,
#22330,#22331));
#5073=EDGE_LOOP('',(#22332,#22333,#22334,#22335));
#5074=EDGE_LOOP('',(#22336,#22337,#22338,#22339));
#5075=EDGE_LOOP('',(#22340,#22341,#22342,#22343,#22344));
#5076=EDGE_LOOP('',(#22345,#22346,#22347,#22348));
#5077=EDGE_LOOP('',(#22349,#22350,#22351,#22352));
#5078=EDGE_LOOP('',(#22353,#22354,#22355,#22356));
#5079=EDGE_LOOP('',(#22357,#22358,#22359,#22360));
#5080=EDGE_LOOP('',(#22361,#22362,#22363,#22364,#22365));
#5081=EDGE_LOOP('',(#22366,#22367,#22368,#22369));
#5082=EDGE_LOOP('',(#22370,#22371,#22372,#22373));
#5083=EDGE_LOOP('',(#22374,#22375,#22376,#22377));
#5084=EDGE_LOOP('',(#22378,#22379,#22380,#22381));
#5085=EDGE_LOOP('',(#22382,#22383,#22384,#22385));
#5086=EDGE_LOOP('',(#22386,#22387,#22388,#22389));
#5087=EDGE_LOOP('',(#22390,#22391,#22392,#22393));
#5088=EDGE_LOOP('',(#22394,#22395,#22396,#22397));
#5089=EDGE_LOOP('',(#22398,#22399,#22400));
#5090=EDGE_LOOP('',(#22401,#22402,#22403));
#5091=EDGE_LOOP('',(#22404,#22405,#22406));
#5092=EDGE_LOOP('',(#22407,#22408,#22409,#22410));
#5093=EDGE_LOOP('',(#22411,#22412,#22413,#22414));
#5094=EDGE_LOOP('',(#22415,#22416,#22417,#22418));
#5095=EDGE_LOOP('',(#22419,#22420,#22421,#22422));
#5096=EDGE_LOOP('',(#22423,#22424,#22425,#22426));
#5097=EDGE_LOOP('',(#22427,#22428,#22429,#22430));
#5098=EDGE_LOOP('',(#22431,#22432,#22433,#22434));
#5099=EDGE_LOOP('',(#22435,#22436,#22437,#22438));
#5100=EDGE_LOOP('',(#22439,#22440,#22441,#22442));
#5101=EDGE_LOOP('',(#22443,#22444,#22445,#22446));
#5102=EDGE_LOOP('',(#22447,#22448,#22449,#22450));
#5103=EDGE_LOOP('',(#22451,#22452,#22453,#22454));
#5104=EDGE_LOOP('',(#22455,#22456,#22457,#22458));
#5105=EDGE_LOOP('',(#22459,#22460,#22461,#22462));
#5106=EDGE_LOOP('',(#22463,#22464,#22465,#22466,#22467,#22468,#22469,#22470,
#22471,#22472,#22473,#22474,#22475,#22476,#22477,#22478,#22479,#22480,#22481,
#22482,#22483,#22484,#22485,#22486,#22487,#22488,#22489,#22490,#22491,#22492,
#22493,#22494,#22495,#22496,#22497,#22498,#22499,#22500,#22501,#22502,#22503,
#22504,#22505,#22506,#22507,#22508,#22509,#22510,#22511,#22512,#22513,#22514,
#22515,#22516,#22517,#22518,#22519,#22520,#22521,#22522,#22523,#22524,#22525,
#22526,#22527,#22528,#22529,#22530,#22531,#22532,#22533,#22534));
#5107=EDGE_LOOP('',(#22535,#22536,#22537,#22538,#22539,#22540,#22541,#22542,
#22543,#22544,#22545,#22546,#22547,#22548,#22549,#22550,#22551,#22552,#22553,
#22554,#22555,#22556,#22557,#22558,#22559,#22560,#22561,#22562,#22563,#22564,
#22565,#22566,#22567,#22568,#22569,#22570,#22571,#22572,#22573,#22574,#22575,
#22576,#22577,#22578,#22579,#22580,#22581,#22582,#22583,#22584,#22585,#22586,
#22587,#22588,#22589,#22590,#22591,#22592,#22593,#22594,#22595,#22596,#22597,
#22598,#22599,#22600,#22601,#22602,#22603,#22604,#22605,#22606));
#5108=EDGE_LOOP('',(#22607,#22608,#22609));
#5109=EDGE_LOOP('',(#22610,#22611,#22612));
#5110=EDGE_LOOP('',(#22613,#22614));
#5111=EDGE_LOOP('',(#22615,#22616,#22617,#22618));
#5112=EDGE_LOOP('',(#22619,#22620,#22621,#22622,#22623,#22624,#22625,#22626,
#22627,#22628,#22629,#22630,#22631,#22632,#22633,#22634));
#5113=EDGE_LOOP('',(#22635,#22636,#22637,#22638));
#5114=EDGE_LOOP('',(#22639,#22640,#22641,#22642));
#5115=EDGE_LOOP('',(#22643,#22644,#22645,#22646,#22647,#22648,#22649,#22650,
#22651,#22652,#22653,#22654,#22655,#22656,#22657,#22658,#22659,#22660,#22661,
#22662,#22663,#22664));
#5116=EDGE_LOOP('',(#22665,#22666,#22667,#22668));
#5117=EDGE_LOOP('',(#22669,#22670,#22671,#22672));
#5118=EDGE_LOOP('',(#22673,#22674,#22675,#22676));
#5119=EDGE_LOOP('',(#22677,#22678,#22679,#22680));
#5120=EDGE_LOOP('',(#22681,#22682,#22683,#22684));
#5121=EDGE_LOOP('',(#22685,#22686,#22687,#22688));
#5122=EDGE_LOOP('',(#22689,#22690,#22691,#22692));
#5123=EDGE_LOOP('',(#22693,#22694,#22695,#22696,#22697,#22698));
#5124=EDGE_LOOP('',(#22699,#22700,#22701,#22702,#22703,#22704,#22705));
#5125=EDGE_LOOP('',(#22706,#22707,#22708,#22709));
#5126=EDGE_LOOP('',(#22710,#22711,#22712,#22713));
#5127=EDGE_LOOP('',(#22714,#22715,#22716,#22717));
#5128=EDGE_LOOP('',(#22718,#22719,#22720,#22721));
#5129=EDGE_LOOP('',(#22722,#22723,#22724,#22725));
#5130=EDGE_LOOP('',(#22726,#22727,#22728,#22729,#22730));
#5131=EDGE_LOOP('',(#22731,#22732,#22733,#22734,#22735));
#5132=EDGE_LOOP('',(#22736,#22737,#22738,#22739));
#5133=EDGE_LOOP('',(#22740,#22741,#22742,#22743));
#5134=EDGE_LOOP('',(#22744,#22745,#22746,#22747));
#5135=EDGE_LOOP('',(#22748,#22749,#22750,#22751));
#5136=EDGE_LOOP('',(#22752,#22753,#22754,#22755));
#5137=EDGE_LOOP('',(#22756,#22757,#22758,#22759));
#5138=EDGE_LOOP('',(#22760,#22761,#22762,#22763));
#5139=EDGE_LOOP('',(#22764,#22765,#22766,#22767));
#5140=EDGE_LOOP('',(#22768,#22769,#22770));
#5141=EDGE_LOOP('',(#22771,#22772,#22773));
#5142=EDGE_LOOP('',(#22774,#22775));
#5143=EDGE_LOOP('',(#22776,#22777,#22778,#22779,#22780,#22781,#22782,#22783));
#5144=EDGE_LOOP('',(#22784,#22785,#22786,#22787));
#5145=EDGE_LOOP('',(#22788,#22789,#22790,#22791,#22792,#22793,#22794,#22795,
#22796,#22797,#22798,#22799,#22800,#22801,#22802,#22803));
#5146=EDGE_LOOP('',(#22804,#22805,#22806,#22807,#22808,#22809,#22810,#22811,
#22812,#22813));
#5147=EDGE_LOOP('',(#22814,#22815,#22816,#22817));
#5148=EDGE_LOOP('',(#22818,#22819,#22820,#22821));
#5149=EDGE_LOOP('',(#22822,#22823,#22824,#22825,#22826,#22827,#22828,#22829,
#22830,#22831,#22832,#22833,#22834,#22835,#22836,#22837,#22838,#22839,#22840,
#22841,#22842,#22843));
#5150=EDGE_LOOP('',(#22844,#22845,#22846,#22847,#22848,#22849,#22850,#22851,
#22852,#22853));
#5151=EDGE_LOOP('',(#22854,#22855,#22856,#22857));
#5152=EDGE_LOOP('',(#22858,#22859,#22860,#22861));
#5153=EDGE_LOOP('',(#22862,#22863,#22864,#22865));
#5154=EDGE_LOOP('',(#22866,#22867,#22868,#22869));
#5155=EDGE_LOOP('',(#22870,#22871,#22872,#22873));
#5156=EDGE_LOOP('',(#22874,#22875,#22876,#22877));
#5157=EDGE_LOOP('',(#22878,#22879,#22880,#22881));
#5158=EDGE_LOOP('',(#22882,#22883,#22884,#22885,#22886,#22887));
#5159=EDGE_LOOP('',(#22888,#22889,#22890,#22891,#22892,#22893,#22894));
#5160=EDGE_LOOP('',(#22895,#22896,#22897,#22898));
#5161=EDGE_LOOP('',(#22899,#22900,#22901,#22902));
#5162=EDGE_LOOP('',(#22903,#22904,#22905,#22906));
#5163=EDGE_LOOP('',(#22907,#22908,#22909,#22910));
#5164=EDGE_LOOP('',(#22911,#22912,#22913,#22914));
#5165=EDGE_LOOP('',(#22915,#22916,#22917,#22918));
#5166=EDGE_LOOP('',(#22919,#22920,#22921,#22922));
#5167=EDGE_LOOP('',(#22923,#22924,#22925,#22926));
#5168=EDGE_LOOP('',(#22927,#22928,#22929,#22930,#22931));
#5169=EDGE_LOOP('',(#22932,#22933,#22934,#22935,#22936));
#5170=EDGE_LOOP('',(#22937,#22938,#22939,#22940,#22941,#22942,#22943,#22944,
#22945,#22946));
#5171=EDGE_LOOP('',(#22947,#22948,#22949,#22950,#22951,#22952,#22953,#22954,
#22955,#22956,#22957,#22958));
#5172=EDGE_LOOP('',(#22959,#22960,#22961,#22962));
#5173=EDGE_LOOP('',(#22963,#22964,#22965,#22966));
#5174=EDGE_LOOP('',(#22967,#22968,#22969,#22970));
#5175=EDGE_LOOP('',(#22971,#22972,#22973,#22974));
#5176=EDGE_LOOP('',(#22975,#22976,#22977,#22978));
#5177=EDGE_LOOP('',(#22979,#22980,#22981,#22982));
#5178=EDGE_LOOP('',(#22983,#22984,#22985,#22986));
#5179=EDGE_LOOP('',(#22987,#22988,#22989,#22990));
#5180=EDGE_LOOP('',(#22991,#22992,#22993,#22994));
#5181=EDGE_LOOP('',(#22995,#22996,#22997,#22998));
#5182=EDGE_LOOP('',(#22999,#23000,#23001,#23002));
#5183=EDGE_LOOP('',(#23003,#23004,#23005,#23006));
#5184=EDGE_LOOP('',(#23007,#23008,#23009,#23010));
#5185=EDGE_LOOP('',(#23011,#23012,#23013,#23014));
#5186=EDGE_LOOP('',(#23015,#23016,#23017,#23018));
#5187=EDGE_LOOP('',(#23019,#23020,#23021,#23022));
#5188=EDGE_LOOP('',(#23023,#23024,#23025,#23026));
#5189=EDGE_LOOP('',(#23027,#23028,#23029,#23030));
#5190=EDGE_LOOP('',(#23031,#23032,#23033,#23034));
#5191=EDGE_LOOP('',(#23035,#23036,#23037,#23038));
#5192=EDGE_LOOP('',(#23039,#23040,#23041,#23042));
#5193=EDGE_LOOP('',(#23043,#23044,#23045,#23046));
#5194=EDGE_LOOP('',(#23047,#23048,#23049,#23050));
#5195=EDGE_LOOP('',(#23051,#23052,#23053,#23054));
#5196=EDGE_LOOP('',(#23055,#23056,#23057,#23058));
#5197=EDGE_LOOP('',(#23059,#23060,#23061,#23062));
#5198=EDGE_LOOP('',(#23063,#23064,#23065,#23066));
#5199=EDGE_LOOP('',(#23067,#23068,#23069,#23070));
#5200=EDGE_LOOP('',(#23071,#23072,#23073,#23074));
#5201=EDGE_LOOP('',(#23075,#23076,#23077,#23078));
#5202=EDGE_LOOP('',(#23079,#23080,#23081,#23082));
#5203=EDGE_LOOP('',(#23083,#23084,#23085,#23086));
#5204=EDGE_LOOP('',(#23087,#23088,#23089,#23090));
#5205=EDGE_LOOP('',(#23091,#23092,#23093,#23094));
#5206=EDGE_LOOP('',(#23095,#23096,#23097,#23098));
#5207=EDGE_LOOP('',(#23099,#23100,#23101,#23102));
#5208=EDGE_LOOP('',(#23103,#23104,#23105,#23106));
#5209=EDGE_LOOP('',(#23107,#23108,#23109,#23110));
#5210=EDGE_LOOP('',(#23111,#23112,#23113,#23114));
#5211=EDGE_LOOP('',(#23115,#23116,#23117,#23118));
#5212=EDGE_LOOP('',(#23119,#23120,#23121,#23122));
#5213=EDGE_LOOP('',(#23123,#23124,#23125,#23126));
#5214=EDGE_LOOP('',(#23127,#23128,#23129,#23130));
#5215=EDGE_LOOP('',(#23131,#23132,#23133,#23134));
#5216=EDGE_LOOP('',(#23135,#23136,#23137,#23138));
#5217=EDGE_LOOP('',(#23139,#23140,#23141,#23142));
#5218=EDGE_LOOP('',(#23143,#23144,#23145,#23146));
#5219=EDGE_LOOP('',(#23147,#23148,#23149,#23150));
#5220=EDGE_LOOP('',(#23151,#23152,#23153,#23154));
#5221=EDGE_LOOP('',(#23155,#23156,#23157,#23158));
#5222=EDGE_LOOP('',(#23159,#23160,#23161,#23162));
#5223=EDGE_LOOP('',(#23163,#23164,#23165,#23166));
#5224=EDGE_LOOP('',(#23167,#23168,#23169,#23170));
#5225=EDGE_LOOP('',(#23171,#23172,#23173,#23174));
#5226=EDGE_LOOP('',(#23175,#23176,#23177,#23178));
#5227=EDGE_LOOP('',(#23179,#23180,#23181,#23182));
#5228=EDGE_LOOP('',(#23183,#23184,#23185,#23186));
#5229=EDGE_LOOP('',(#23187,#23188,#23189,#23190));
#5230=EDGE_LOOP('',(#23191,#23192,#23193,#23194));
#5231=EDGE_LOOP('',(#23195,#23196,#23197,#23198));
#5232=EDGE_LOOP('',(#23199,#23200,#23201,#23202));
#5233=EDGE_LOOP('',(#23203,#23204,#23205,#23206));
#5234=EDGE_LOOP('',(#23207,#23208,#23209,#23210));
#5235=EDGE_LOOP('',(#23211,#23212,#23213,#23214));
#5236=EDGE_LOOP('',(#23215,#23216,#23217,#23218));
#5237=EDGE_LOOP('',(#23219,#23220,#23221,#23222));
#5238=EDGE_LOOP('',(#23223,#23224,#23225,#23226));
#5239=EDGE_LOOP('',(#23227,#23228,#23229,#23230));
#5240=EDGE_LOOP('',(#23231,#23232,#23233,#23234));
#5241=EDGE_LOOP('',(#23235,#23236,#23237,#23238));
#5242=EDGE_LOOP('',(#23239,#23240,#23241,#23242));
#5243=EDGE_LOOP('',(#23243,#23244,#23245,#23246));
#5244=EDGE_LOOP('',(#23247,#23248,#23249,#23250));
#5245=EDGE_LOOP('',(#23251,#23252,#23253,#23254));
#5246=EDGE_LOOP('',(#23255,#23256,#23257,#23258));
#5247=EDGE_LOOP('',(#23259,#23260,#23261,#23262));
#5248=EDGE_LOOP('',(#23263,#23264,#23265,#23266));
#5249=EDGE_LOOP('',(#23267,#23268,#23269,#23270));
#5250=EDGE_LOOP('',(#23271,#23272,#23273,#23274));
#5251=EDGE_LOOP('',(#23275,#23276,#23277,#23278));
#5252=EDGE_LOOP('',(#23279,#23280,#23281,#23282));
#5253=EDGE_LOOP('',(#23283,#23284,#23285,#23286));
#5254=EDGE_LOOP('',(#23287,#23288,#23289,#23290));
#5255=EDGE_LOOP('',(#23291,#23292,#23293,#23294));
#5256=EDGE_LOOP('',(#23295,#23296,#23297,#23298));
#5257=EDGE_LOOP('',(#23299,#23300,#23301,#23302));
#5258=EDGE_LOOP('',(#23303,#23304,#23305,#23306));
#5259=EDGE_LOOP('',(#23307,#23308,#23309,#23310));
#5260=EDGE_LOOP('',(#23311,#23312,#23313,#23314));
#5261=EDGE_LOOP('',(#23315,#23316,#23317,#23318));
#5262=EDGE_LOOP('',(#23319,#23320,#23321,#23322));
#5263=EDGE_LOOP('',(#23323,#23324,#23325,#23326));
#5264=EDGE_LOOP('',(#23327,#23328,#23329,#23330));
#5265=EDGE_LOOP('',(#23331,#23332,#23333,#23334));
#5266=EDGE_LOOP('',(#23335,#23336,#23337,#23338));
#5267=EDGE_LOOP('',(#23339,#23340,#23341,#23342));
#5268=EDGE_LOOP('',(#23343,#23344,#23345,#23346));
#5269=EDGE_LOOP('',(#23347,#23348,#23349,#23350));
#5270=EDGE_LOOP('',(#23351,#23352,#23353,#23354));
#5271=EDGE_LOOP('',(#23355,#23356,#23357,#23358));
#5272=EDGE_LOOP('',(#23359,#23360,#23361,#23362));
#5273=EDGE_LOOP('',(#23363,#23364,#23365,#23366,#23367,#23368,#23369,#23370,
#23371,#23372,#23373,#23374,#23375,#23376,#23377,#23378,#23379,#23380,#23381,
#23382,#23383,#23384,#23385,#23386,#23387,#23388,#23389,#23390,#23391,#23392,
#23393,#23394,#23395,#23396,#23397,#23398,#23399,#23400,#23401,#23402,#23403,
#23404,#23405,#23406,#23407,#23408,#23409,#23410,#23411,#23412,#23413,#23414,
#23415,#23416,#23417,#23418,#23419,#23420,#23421,#23422,#23423,#23424,#23425,
#23426,#23427,#23428,#23429,#23430,#23431,#23432,#23433,#23434,#23435,#23436,
#23437,#23438,#23439,#23440,#23441,#23442,#23443,#23444,#23445,#23446,#23447,
#23448,#23449,#23450,#23451,#23452,#23453,#23454));
#5274=EDGE_LOOP('',(#23455));
#5275=EDGE_LOOP('',(#23456,#23457,#23458,#23459,#23460,#23461,#23462,#23463,
#23464,#23465,#23466,#23467,#23468,#23469,#23470,#23471,#23472,#23473,#23474,
#23475,#23476,#23477,#23478,#23479,#23480,#23481,#23482,#23483,#23484,#23485,
#23486,#23487,#23488,#23489,#23490,#23491,#23492,#23493,#23494,#23495,#23496,
#23497,#23498,#23499,#23500,#23501,#23502,#23503,#23504,#23505,#23506,#23507,
#23508,#23509,#23510,#23511,#23512,#23513,#23514,#23515,#23516,#23517,#23518,
#23519,#23520,#23521,#23522,#23523,#23524,#23525,#23526,#23527,#23528,#23529,
#23530,#23531,#23532,#23533,#23534,#23535,#23536,#23537,#23538,#23539,#23540,
#23541,#23542,#23543,#23544,#23545,#23546,#23547));
#5276=EDGE_LOOP('',(#23548));
#5277=EDGE_LOOP('',(#23549,#23550,#23551,#23552));
#5278=EDGE_LOOP('',(#23553,#23554,#23555,#23556,#23557,#23558));
#5279=EDGE_LOOP('',(#23559,#23560,#23561,#23562,#23563,#23564));
#5280=EDGE_LOOP('',(#23565,#23566,#23567,#23568,#23569,#23570));
#5281=EDGE_LOOP('',(#23571,#23572,#23573,#23574));
#5282=EDGE_LOOP('',(#23575,#23576,#23577,#23578,#23579,#23580));
#5283=EDGE_LOOP('',(#23581,#23582,#23583,#23584,#23585,#23586));
#5284=EDGE_LOOP('',(#23587,#23588,#23589,#23590,#23591,#23592));
#5285=EDGE_LOOP('',(#23593,#23594,#23595,#23596,#23597,#23598));
#5286=EDGE_LOOP('',(#23599,#23600,#23601,#23602,#23603,#23604));
#5287=EDGE_LOOP('',(#23605,#23606,#23607,#23608,#23609,#23610));
#5288=EDGE_LOOP('',(#23611,#23612,#23613,#23614,#23615,#23616));
#5289=EDGE_LOOP('',(#23617,#23618,#23619,#23620,#23621,#23622));
#5290=EDGE_LOOP('',(#23623,#23624,#23625,#23626,#23627,#23628));
#5291=EDGE_LOOP('',(#23629,#23630,#23631,#23632,#23633,#23634));
#5292=EDGE_LOOP('',(#23635,#23636,#23637,#23638,#23639,#23640));
#5293=EDGE_LOOP('',(#23641,#23642,#23643,#23644,#23645,#23646));
#5294=EDGE_LOOP('',(#23647,#23648,#23649,#23650,#23651,#23652));
#5295=EDGE_LOOP('',(#23653,#23654,#23655,#23656,#23657,#23658));
#5296=EDGE_LOOP('',(#23659,#23660,#23661,#23662,#23663,#23664));
#5297=EDGE_LOOP('',(#23665,#23666,#23667,#23668,#23669,#23670));
#5298=EDGE_LOOP('',(#23671,#23672,#23673,#23674,#23675,#23676));
#5299=EDGE_LOOP('',(#23677,#23678,#23679,#23680,#23681,#23682));
#5300=EDGE_LOOP('',(#23683,#23684,#23685,#23686,#23687,#23688));
#5301=EDGE_LOOP('',(#23689,#23690,#23691,#23692,#23693,#23694));
#5302=EDGE_LOOP('',(#23695,#23696,#23697,#23698,#23699,#23700));
#5303=EDGE_LOOP('',(#23701,#23702,#23703,#23704,#23705,#23706));
#5304=EDGE_LOOP('',(#23707,#23708,#23709,#23710,#23711,#23712));
#5305=EDGE_LOOP('',(#23713,#23714,#23715,#23716,#23717,#23718));
#5306=EDGE_LOOP('',(#23719,#23720,#23721,#23722,#23723,#23724));
#5307=EDGE_LOOP('',(#23725,#23726,#23727,#23728,#23729,#23730));
#5308=EDGE_LOOP('',(#23731,#23732,#23733,#23734,#23735,#23736));
#5309=EDGE_LOOP('',(#23737,#23738,#23739,#23740,#23741,#23742));
#5310=EDGE_LOOP('',(#23743,#23744,#23745,#23746,#23747,#23748));
#5311=EDGE_LOOP('',(#23749,#23750,#23751,#23752,#23753,#23754));
#5312=EDGE_LOOP('',(#23755,#23756,#23757,#23758,#23759,#23760));
#5313=EDGE_LOOP('',(#23761,#23762,#23763,#23764,#23765,#23766));
#5314=EDGE_LOOP('',(#23767,#23768,#23769,#23770,#23771,#23772));
#5315=EDGE_LOOP('',(#23773,#23774,#23775,#23776,#23777,#23778));
#5316=EDGE_LOOP('',(#23779,#23780,#23781,#23782,#23783,#23784));
#5317=EDGE_LOOP('',(#23785,#23786,#23787,#23788,#23789,#23790));
#5318=EDGE_LOOP('',(#23791,#23792,#23793,#23794,#23795,#23796));
#5319=EDGE_LOOP('',(#23797,#23798,#23799,#23800,#23801,#23802));
#5320=EDGE_LOOP('',(#23803,#23804,#23805,#23806,#23807,#23808));
#5321=EDGE_LOOP('',(#23809,#23810,#23811,#23812,#23813,#23814));
#5322=EDGE_LOOP('',(#23815,#23816,#23817,#23818,#23819,#23820));
#5323=EDGE_LOOP('',(#23821,#23822,#23823,#23824,#23825,#23826));
#5324=EDGE_LOOP('',(#23827,#23828,#23829,#23830,#23831,#23832));
#5325=EDGE_LOOP('',(#23833,#23834,#23835,#23836,#23837,#23838));
#5326=EDGE_LOOP('',(#23839,#23840,#23841,#23842,#23843,#23844));
#5327=EDGE_LOOP('',(#23845,#23846,#23847,#23848,#23849,#23850));
#5328=EDGE_LOOP('',(#23851,#23852,#23853,#23854,#23855,#23856));
#5329=EDGE_LOOP('',(#23857,#23858,#23859,#23860,#23861,#23862));
#5330=EDGE_LOOP('',(#23863,#23864,#23865,#23866,#23867,#23868));
#5331=EDGE_LOOP('',(#23869,#23870,#23871,#23872,#23873,#23874));
#5332=EDGE_LOOP('',(#23875,#23876,#23877,#23878,#23879,#23880));
#5333=EDGE_LOOP('',(#23881,#23882,#23883,#23884,#23885,#23886));
#5334=EDGE_LOOP('',(#23887,#23888,#23889,#23890,#23891,#23892));
#5335=EDGE_LOOP('',(#23893,#23894,#23895,#23896,#23897,#23898));
#5336=EDGE_LOOP('',(#23899,#23900,#23901,#23902,#23903,#23904));
#5337=EDGE_LOOP('',(#23905,#23906,#23907,#23908,#23909,#23910));
#5338=EDGE_LOOP('',(#23911,#23912,#23913,#23914,#23915,#23916));
#5339=EDGE_LOOP('',(#23917,#23918,#23919,#23920,#23921,#23922));
#5340=EDGE_LOOP('',(#23923,#23924,#23925,#23926,#23927,#23928));
#5341=EDGE_LOOP('',(#23929,#23930,#23931,#23932,#23933,#23934));
#5342=EDGE_LOOP('',(#23935,#23936,#23937,#23938,#23939,#23940));
#5343=EDGE_LOOP('',(#23941,#23942,#23943,#23944,#23945,#23946));
#5344=EDGE_LOOP('',(#23947,#23948,#23949,#23950,#23951,#23952));
#5345=EDGE_LOOP('',(#23953,#23954,#23955,#23956,#23957,#23958));
#5346=EDGE_LOOP('',(#23959,#23960,#23961,#23962,#23963,#23964));
#5347=EDGE_LOOP('',(#23965,#23966,#23967,#23968,#23969,#23970));
#5348=EDGE_LOOP('',(#23971,#23972,#23973,#23974,#23975,#23976));
#5349=EDGE_LOOP('',(#23977,#23978,#23979,#23980,#23981,#23982));
#5350=EDGE_LOOP('',(#23983,#23984,#23985,#23986,#23987,#23988));
#5351=EDGE_LOOP('',(#23989,#23990,#23991,#23992,#23993,#23994));
#5352=EDGE_LOOP('',(#23995,#23996,#23997,#23998,#23999,#24000));
#5353=EDGE_LOOP('',(#24001,#24002,#24003,#24004,#24005,#24006));
#5354=EDGE_LOOP('',(#24007,#24008,#24009,#24010,#24011,#24012));
#5355=EDGE_LOOP('',(#24013,#24014,#24015,#24016,#24017,#24018));
#5356=EDGE_LOOP('',(#24019,#24020,#24021,#24022,#24023,#24024));
#5357=EDGE_LOOP('',(#24025,#24026,#24027,#24028,#24029,#24030));
#5358=EDGE_LOOP('',(#24031,#24032,#24033,#24034,#24035,#24036));
#5359=EDGE_LOOP('',(#24037,#24038,#24039,#24040,#24041,#24042));
#5360=EDGE_LOOP('',(#24043,#24044,#24045,#24046,#24047,#24048));
#5361=EDGE_LOOP('',(#24049,#24050,#24051,#24052,#24053,#24054));
#5362=EDGE_LOOP('',(#24055,#24056,#24057,#24058,#24059,#24060));
#5363=EDGE_LOOP('',(#24061,#24062,#24063,#24064,#24065,#24066));
#5364=EDGE_LOOP('',(#24067,#24068,#24069,#24070,#24071,#24072));
#5365=EDGE_LOOP('',(#24073,#24074,#24075,#24076,#24077,#24078));
#5366=EDGE_LOOP('',(#24079,#24080,#24081,#24082,#24083,#24084));
#5367=EDGE_LOOP('',(#24085,#24086,#24087,#24088,#24089,#24090));
#5368=EDGE_LOOP('',(#24091,#24092,#24093,#24094,#24095,#24096));
#5369=EDGE_LOOP('',(#24097,#24098,#24099,#24100,#24101,#24102));
#5370=EDGE_LOOP('',(#24103,#24104,#24105,#24106,#24107,#24108));
#5371=EDGE_LOOP('',(#24109,#24110,#24111,#24112,#24113,#24114));
#5372=EDGE_LOOP('',(#24115,#24116,#24117,#24118,#24119,#24120));
#5373=EDGE_LOOP('',(#24121,#24122,#24123,#24124,#24125,#24126));
#5374=EDGE_LOOP('',(#24127,#24128,#24129,#24130,#24131,#24132));
#5375=EDGE_LOOP('',(#24133,#24134,#24135,#24136,#24137,#24138));
#5376=EDGE_LOOP('',(#24139,#24140,#24141,#24142,#24143,#24144));
#5377=EDGE_LOOP('',(#24145,#24146,#24147,#24148,#24149,#24150));
#5378=EDGE_LOOP('',(#24151,#24152,#24153,#24154,#24155,#24156));
#5379=EDGE_LOOP('',(#24157,#24158,#24159,#24160,#24161,#24162));
#5380=EDGE_LOOP('',(#24163,#24164,#24165,#24166,#24167,#24168));
#5381=EDGE_LOOP('',(#24169,#24170,#24171,#24172,#24173,#24174));
#5382=EDGE_LOOP('',(#24175,#24176,#24177,#24178,#24179,#24180));
#5383=EDGE_LOOP('',(#24181,#24182,#24183,#24184,#24185,#24186));
#5384=EDGE_LOOP('',(#24187,#24188,#24189,#24190,#24191,#24192));
#5385=EDGE_LOOP('',(#24193,#24194,#24195,#24196,#24197,#24198));
#5386=EDGE_LOOP('',(#24199,#24200,#24201,#24202,#24203,#24204));
#5387=EDGE_LOOP('',(#24205,#24206,#24207,#24208,#24209,#24210));
#5388=EDGE_LOOP('',(#24211,#24212,#24213,#24214,#24215,#24216));
#5389=EDGE_LOOP('',(#24217,#24218,#24219,#24220,#24221,#24222));
#5390=EDGE_LOOP('',(#24223,#24224,#24225,#24226,#24227,#24228));
#5391=EDGE_LOOP('',(#24229,#24230,#24231,#24232,#24233,#24234));
#5392=EDGE_LOOP('',(#24235,#24236,#24237,#24238,#24239,#24240));
#5393=EDGE_LOOP('',(#24241,#24242,#24243));
#5394=EDGE_LOOP('',(#24244,#24245,#24246,#24247,#24248));
#5395=EDGE_LOOP('',(#24249,#24250,#24251,#24252));
#5396=EDGE_LOOP('',(#24253,#24254,#24255,#24256));
#5397=EDGE_LOOP('',(#24257,#24258,#24259,#24260));
#5398=EDGE_LOOP('',(#24261,#24262,#24263,#24264));
#5399=EDGE_LOOP('',(#24265,#24266,#24267,#24268));
#5400=EDGE_LOOP('',(#24269,#24270,#24271,#24272,#24273));
#5401=EDGE_LOOP('',(#24274,#24275,#24276,#24277,#24278,#24279));
#5402=EDGE_LOOP('',(#24280,#24281,#24282,#24283,#24284));
#5403=EDGE_LOOP('',(#24285,#24286,#24287,#24288,#24289));
#5404=EDGE_LOOP('',(#24290,#24291,#24292,#24293,#24294,#24295));
#5405=EDGE_LOOP('',(#24296,#24297,#24298,#24299));
#5406=EDGE_LOOP('',(#24300,#24301,#24302,#24303,#24304,#24305));
#5407=EDGE_LOOP('',(#24306,#24307,#24308,#24309));
#5408=EDGE_LOOP('',(#24310,#24311,#24312,#24313,#24314,#24315));
#5409=EDGE_LOOP('',(#24316,#24317,#24318,#24319,#24320));
#5410=EDGE_LOOP('',(#24321,#24322,#24323,#24324,#24325,#24326));
#5411=EDGE_LOOP('',(#24327,#24328,#24329,#24330));
#5412=EDGE_LOOP('',(#24331,#24332,#24333,#24334,#24335,#24336));
#5413=EDGE_LOOP('',(#24337,#24338,#24339,#24340,#24341));
#5414=EDGE_LOOP('',(#24342,#24343,#24344,#24345,#24346,#24347));
#5415=EDGE_LOOP('',(#24348,#24349,#24350,#24351,#24352));
#5416=EDGE_LOOP('',(#24353,#24354,#24355,#24356,#24357,#24358));
#5417=EDGE_LOOP('',(#24359,#24360,#24361,#24362));
#5418=EDGE_LOOP('',(#24363,#24364,#24365,#24366,#24367,#24368));
#5419=EDGE_LOOP('',(#24369,#24370,#24371,#24372,#24373));
#5420=EDGE_LOOP('',(#24374,#24375,#24376,#24377,#24378,#24379));
#5421=EDGE_LOOP('',(#24380,#24381,#24382,#24383));
#5422=EDGE_LOOP('',(#24384,#24385,#24386,#24387,#24388,#24389));
#5423=EDGE_LOOP('',(#24390,#24391,#24392,#24393));
#5424=EDGE_LOOP('',(#24394,#24395,#24396,#24397,#24398,#24399));
#5425=EDGE_LOOP('',(#24400,#24401,#24402,#24403,#24404));
#5426=EDGE_LOOP('',(#24405,#24406,#24407,#24408,#24409));
#5427=EDGE_LOOP('',(#24410,#24411,#24412,#24413,#24414,#24415));
#5428=EDGE_LOOP('',(#24416,#24417,#24418,#24419,#24420,#24421));
#5429=EDGE_LOOP('',(#24422,#24423,#24424,#24425,#24426));
#5430=EDGE_LOOP('',(#24427,#24428,#24429,#24430,#24431));
#5431=EDGE_LOOP('',(#24432,#24433,#24434,#24435,#24436,#24437));
#5432=EDGE_LOOP('',(#24438,#24439,#24440,#24441));
#5433=EDGE_LOOP('',(#24442,#24443,#24444,#24445,#24446,#24447));
#5434=EDGE_LOOP('',(#24448,#24449,#24450,#24451));
#5435=EDGE_LOOP('',(#24452,#24453,#24454,#24455,#24456,#24457));
#5436=EDGE_LOOP('',(#24458,#24459,#24460,#24461,#24462));
#5437=EDGE_LOOP('',(#24463,#24464,#24465,#24466,#24467,#24468));
#5438=EDGE_LOOP('',(#24469,#24470,#24471,#24472));
#5439=EDGE_LOOP('',(#24473,#24474,#24475,#24476,#24477,#24478));
#5440=EDGE_LOOP('',(#24479,#24480,#24481,#24482,#24483));
#5441=EDGE_LOOP('',(#24484,#24485,#24486,#24487,#24488,#24489));
#5442=EDGE_LOOP('',(#24490,#24491,#24492,#24493,#24494));
#5443=EDGE_LOOP('',(#24495,#24496,#24497,#24498,#24499,#24500));
#5444=EDGE_LOOP('',(#24501,#24502,#24503,#24504));
#5445=EDGE_LOOP('',(#24505,#24506,#24507,#24508,#24509,#24510));
#5446=EDGE_LOOP('',(#24511,#24512,#24513,#24514,#24515));
#5447=EDGE_LOOP('',(#24516,#24517,#24518,#24519,#24520,#24521));
#5448=EDGE_LOOP('',(#24522,#24523,#24524,#24525));
#5449=EDGE_LOOP('',(#24526,#24527,#24528,#24529,#24530,#24531));
#5450=EDGE_LOOP('',(#24532,#24533,#24534,#24535));
#5451=EDGE_LOOP('',(#24536,#24537,#24538,#24539,#24540,#24541));
#5452=EDGE_LOOP('',(#24542,#24543,#24544,#24545,#24546));
#5453=EDGE_LOOP('',(#24547,#24548,#24549,#24550,#24551));
#5454=EDGE_LOOP('',(#24552,#24553,#24554,#24555,#24556,#24557));
#5455=EDGE_LOOP('',(#24558,#24559,#24560,#24561,#24562,#24563));
#5456=EDGE_LOOP('',(#24564,#24565,#24566,#24567,#24568));
#5457=EDGE_LOOP('',(#24569,#24570,#24571,#24572,#24573));
#5458=EDGE_LOOP('',(#24574,#24575,#24576,#24577,#24578,#24579));
#5459=EDGE_LOOP('',(#24580,#24581,#24582,#24583));
#5460=EDGE_LOOP('',(#24584,#24585,#24586,#24587,#24588,#24589));
#5461=EDGE_LOOP('',(#24590,#24591,#24592,#24593));
#5462=EDGE_LOOP('',(#24594,#24595,#24596,#24597,#24598,#24599));
#5463=EDGE_LOOP('',(#24600,#24601,#24602,#24603,#24604));
#5464=EDGE_LOOP('',(#24605,#24606,#24607,#24608,#24609,#24610));
#5465=EDGE_LOOP('',(#24611,#24612,#24613,#24614));
#5466=EDGE_LOOP('',(#24615,#24616,#24617,#24618,#24619,#24620));
#5467=EDGE_LOOP('',(#24621,#24622,#24623,#24624,#24625));
#5468=EDGE_LOOP('',(#24626,#24627,#24628,#24629,#24630,#24631));
#5469=EDGE_LOOP('',(#24632,#24633,#24634,#24635,#24636));
#5470=EDGE_LOOP('',(#24637,#24638,#24639,#24640,#24641,#24642));
#5471=EDGE_LOOP('',(#24643,#24644,#24645,#24646));
#5472=EDGE_LOOP('',(#24647,#24648,#24649,#24650,#24651,#24652));
#5473=EDGE_LOOP('',(#24653,#24654,#24655,#24656,#24657));
#5474=EDGE_LOOP('',(#24658,#24659,#24660,#24661,#24662,#24663));
#5475=EDGE_LOOP('',(#24664,#24665,#24666,#24667));
#5476=EDGE_LOOP('',(#24668,#24669,#24670,#24671,#24672,#24673));
#5477=EDGE_LOOP('',(#24674,#24675,#24676,#24677));
#5478=EDGE_LOOP('',(#24678,#24679,#24680,#24681,#24682,#24683));
#5479=EDGE_LOOP('',(#24684,#24685,#24686,#24687,#24688));
#5480=EDGE_LOOP('',(#24689,#24690,#24691,#24692,#24693));
#5481=EDGE_LOOP('',(#24694,#24695,#24696,#24697,#24698,#24699));
#5482=EDGE_LOOP('',(#24700,#24701,#24702,#24703,#24704,#24705));
#5483=EDGE_LOOP('',(#24706,#24707,#24708,#24709,#24710));
#5484=EDGE_LOOP('',(#24711,#24712,#24713,#24714,#24715));
#5485=EDGE_LOOP('',(#24716,#24717,#24718,#24719,#24720,#24721));
#5486=EDGE_LOOP('',(#24722,#24723,#24724,#24725));
#5487=EDGE_LOOP('',(#24726,#24727,#24728,#24729,#24730,#24731));
#5488=EDGE_LOOP('',(#24732,#24733,#24734,#24735));
#5489=EDGE_LOOP('',(#24736,#24737,#24738,#24739,#24740,#24741));
#5490=EDGE_LOOP('',(#24742,#24743,#24744,#24745,#24746));
#5491=EDGE_LOOP('',(#24747,#24748,#24749,#24750,#24751,#24752));
#5492=EDGE_LOOP('',(#24753,#24754,#24755,#24756));
#5493=EDGE_LOOP('',(#24757,#24758,#24759,#24760,#24761,#24762));
#5494=EDGE_LOOP('',(#24763,#24764,#24765,#24766,#24767));
#5495=EDGE_LOOP('',(#24768,#24769,#24770,#24771,#24772,#24773));
#5496=EDGE_LOOP('',(#24774,#24775,#24776,#24777,#24778));
#5497=EDGE_LOOP('',(#24779,#24780,#24781,#24782,#24783,#24784));
#5498=EDGE_LOOP('',(#24785,#24786,#24787,#24788));
#5499=EDGE_LOOP('',(#24789,#24790,#24791,#24792,#24793,#24794));
#5500=EDGE_LOOP('',(#24795,#24796,#24797,#24798,#24799));
#5501=EDGE_LOOP('',(#24800,#24801,#24802,#24803,#24804,#24805));
#5502=EDGE_LOOP('',(#24806,#24807,#24808,#24809));
#5503=EDGE_LOOP('',(#24810,#24811,#24812,#24813,#24814,#24815));
#5504=EDGE_LOOP('',(#24816,#24817,#24818,#24819));
#5505=EDGE_LOOP('',(#24820,#24821,#24822,#24823,#24824,#24825));
#5506=EDGE_LOOP('',(#24826,#24827,#24828,#24829,#24830));
#5507=EDGE_LOOP('',(#24831,#24832,#24833,#24834,#24835));
#5508=EDGE_LOOP('',(#24836,#24837,#24838,#24839,#24840,#24841));
#5509=EDGE_LOOP('',(#24842,#24843,#24844,#24845));
#5510=EDGE_LOOP('',(#24846,#24847,#24848,#24849));
#5511=EDGE_LOOP('',(#24850,#24851,#24852,#24853));
#5512=EDGE_LOOP('',(#24854,#24855,#24856,#24857));
#5513=EDGE_LOOP('',(#24858,#24859,#24860));
#5514=EDGE_LOOP('',(#24861,#24862,#24863,#24864));
#5515=EDGE_LOOP('',(#24865,#24866,#24867,#24868,#24869,#24870));
#5516=EDGE_LOOP('',(#24871,#24872,#24873,#24874,#24875,#24876));
#5517=EDGE_LOOP('',(#24877,#24878,#24879,#24880,#24881,#24882));
#5518=EDGE_LOOP('',(#24883,#24884,#24885,#24886,#24887,#24888));
#5519=EDGE_LOOP('',(#24889,#24890,#24891,#24892,#24893,#24894));
#5520=EDGE_LOOP('',(#24895,#24896,#24897,#24898,#24899,#24900));
#5521=EDGE_LOOP('',(#24901,#24902,#24903,#24904));
#5522=EDGE_LOOP('',(#24905));
#5523=EDGE_LOOP('',(#24906,#24907,#24908,#24909));
#5524=EDGE_LOOP('',(#24910,#24911,#24912,#24913,#24914));
#5525=EDGE_LOOP('',(#24915,#24916,#24917,#24918));
#5526=EDGE_LOOP('',(#24919));
#5527=EDGE_LOOP('',(#24920,#24921,#24922,#24923));
#5528=EDGE_LOOP('',(#24924,#24925,#24926,#24927,#24928));
#5529=EDGE_LOOP('',(#24929,#24930,#24931,#24932));
#5530=EDGE_LOOP('',(#24933));
#5531=EDGE_LOOP('',(#24934,#24935,#24936,#24937));
#5532=EDGE_LOOP('',(#24938,#24939,#24940,#24941,#24942,#24943));
#5533=EDGE_LOOP('',(#24944,#24945,#24946,#24947,#24948,#24949,#24950,#24951));
#5534=EDGE_LOOP('',(#24952,#24953,#24954,#24955,#24956,#24957,#24958,#24959,
#24960,#24961,#24962,#24963,#24964,#24965,#24966,#24967,#24968,#24969,#24970,
#24971,#24972,#24973,#24974,#24975,#24976,#24977,#24978,#24979,#24980,#24981,
#24982,#24983));
#5535=EDGE_LOOP('',(#24984));
#5536=EDGE_LOOP('',(#24985));
#5537=EDGE_LOOP('',(#24986,#24987,#24988,#24989));
#5538=EDGE_LOOP('',(#24990,#24991,#24992,#24993));
#5539=EDGE_LOOP('',(#24994,#24995,#24996,#24997));
#5540=EDGE_LOOP('',(#24998,#24999,#25000,#25001));
#5541=EDGE_LOOP('',(#25002));
#5542=EDGE_LOOP('',(#25003));
#5543=EDGE_LOOP('',(#25004));
#5544=EDGE_LOOP('',(#25005,#25006,#25007,#25008,#25009,#25010,#25011,#25012,
#25013,#25014,#25015,#25016,#25017,#25018,#25019,#25020));
#5545=EDGE_LOOP('',(#25021,#25022,#25023,#25024,#25025,#25026,#25027,#25028,
#25029,#25030,#25031,#25032,#25033,#25034,#25035));
#5546=EDGE_LOOP('',(#25036,#25037,#25038,#25039,#25040,#25041,#25042,#25043,
#25044,#25045,#25046,#25047,#25048,#25049,#25050,#25051));
#5547=EDGE_LOOP('',(#25052,#25053,#25054,#25055,#25056,#25057,#25058,#25059,
#25060,#25061,#25062,#25063,#25064,#25065,#25066));
#5548=EDGE_LOOP('',(#25067,#25068,#25069,#25070,#25071,#25072,#25073,#25074,
#25075,#25076,#25077,#25078,#25079,#25080,#25081,#25082,#25083,#25084,#25085,
#25086,#25087,#25088,#25089,#25090,#25091,#25092,#25093,#25094,#25095,#25096,
#25097,#25098,#25099,#25100,#25101,#25102,#25103,#25104,#25105,#25106,#25107,
#25108,#25109,#25110,#25111,#25112,#25113,#25114,#25115,#25116,#25117,#25118,
#25119,#25120,#25121,#25122,#25123,#25124,#25125,#25126,#25127,#25128,#25129,
#25130,#25131,#25132,#25133,#25134,#25135,#25136,#25137,#25138,#25139,#25140,
#25141,#25142,#25143,#25144,#25145,#25146,#25147,#25148,#25149,#25150,#25151,
#25152,#25153,#25154,#25155,#25156,#25157,#25158,#25159,#25160,#25161,#25162,
#25163,#25164,#25165,#25166,#25167,#25168,#25169));
#5549=EDGE_LOOP('',(#25170,#25171,#25172,#25173,#25174,#25175,#25176,#25177,
#25178,#25179,#25180,#25181,#25182,#25183,#25184,#25185,#25186,#25187,#25188,
#25189,#25190,#25191,#25192,#25193,#25194,#25195,#25196,#25197,#25198,#25199,
#25200,#25201,#25202,#25203,#25204,#25205,#25206,#25207,#25208,#25209,#25210,
#25211,#25212,#25213,#25214,#25215,#25216,#25217,#25218,#25219,#25220,#25221,
#25222,#25223,#25224,#25225,#25226,#25227,#25228,#25229,#25230,#25231,#25232,
#25233,#25234,#25235,#25236,#25237,#25238,#25239,#25240,#25241,#25242,#25243,
#25244,#25245,#25246,#25247,#25248,#25249,#25250,#25251,#25252,#25253,#25254,
#25255,#25256,#25257,#25258,#25259,#25260,#25261,#25262,#25263,#25264,#25265,
#25266,#25267,#25268,#25269,#25270,#25271,#25272));
#5550=EDGE_LOOP('',(#25273,#25274,#25275,#25276,#25277,#25278,#25279,#25280,
#25281,#25282,#25283,#25284,#25285,#25286,#25287,#25288,#25289,#25290,#25291,
#25292,#25293,#25294,#25295,#25296,#25297,#25298,#25299,#25300,#25301,#25302,
#25303,#25304,#25305,#25306,#25307,#25308,#25309,#25310,#25311,#25312,#25313,
#25314,#25315,#25316,#25317,#25318,#25319,#25320,#25321,#25322,#25323,#25324,
#25325,#25326,#25327,#25328,#25329,#25330,#25331,#25332,#25333,#25334,#25335,
#25336,#25337,#25338,#25339,#25340,#25341,#25342,#25343,#25344,#25345,#25346,
#25347,#25348,#25349,#25350,#25351,#25352,#25353,#25354,#25355,#25356,#25357,
#25358,#25359,#25360,#25361,#25362,#25363,#25364,#25365,#25366,#25367,#25368,
#25369,#25370,#25371,#25372,#25373,#25374,#25375));
#5551=EDGE_LOOP('',(#25376,#25377,#25378,#25379,#25380,#25381,#25382,#25383,
#25384,#25385,#25386,#25387,#25388,#25389,#25390,#25391,#25392,#25393,#25394,
#25395,#25396,#25397,#25398,#25399,#25400,#25401,#25402,#25403,#25404,#25405,
#25406,#25407,#25408,#25409,#25410,#25411,#25412,#25413,#25414,#25415,#25416,
#25417,#25418,#25419,#25420,#25421,#25422,#25423,#25424,#25425,#25426,#25427,
#25428,#25429,#25430,#25431,#25432,#25433,#25434,#25435,#25436,#25437,#25438,
#25439,#25440,#25441,#25442,#25443,#25444,#25445,#25446,#25447,#25448,#25449,
#25450,#25451,#25452,#25453,#25454,#25455,#25456,#25457,#25458,#25459,#25460,
#25461,#25462,#25463,#25464,#25465,#25466,#25467,#25468,#25469,#25470,#25471,
#25472,#25473,#25474,#25475,#25476,#25477,#25478));
#5552=EDGE_LOOP('',(#25479,#25480,#25481,#25482,#25483,#25484,#25485,#25486,
#25487,#25488,#25489,#25490,#25491,#25492,#25493,#25494,#25495,#25496,#25497,
#25498,#25499,#25500,#25501,#25502,#25503,#25504,#25505,#25506,#25507,#25508,
#25509,#25510,#25511,#25512,#25513,#25514,#25515,#25516,#25517,#25518,#25519,
#25520,#25521,#25522,#25523,#25524,#25525,#25526,#25527,#25528,#25529,#25530,
#25531,#25532,#25533,#25534,#25535,#25536,#25537,#25538,#25539,#25540,#25541,
#25542,#25543,#25544,#25545,#25546,#25547,#25548,#25549,#25550,#25551,#25552,
#25553,#25554,#25555,#25556,#25557,#25558,#25559,#25560,#25561,#25562,#25563,
#25564,#25565,#25566,#25567,#25568,#25569,#25570,#25571,#25572,#25573,#25574,
#25575,#25576,#25577,#25578,#25579,#25580,#25581));
#5553=EDGE_LOOP('',(#25582,#25583,#25584,#25585,#25586,#25587,#25588,#25589,
#25590,#25591,#25592,#25593,#25594,#25595,#25596,#25597,#25598,#25599,#25600,
#25601,#25602,#25603,#25604,#25605,#25606,#25607,#25608,#25609,#25610,#25611,
#25612,#25613,#25614,#25615,#25616,#25617,#25618,#25619,#25620,#25621,#25622,
#25623,#25624,#25625,#25626,#25627,#25628,#25629,#25630,#25631,#25632,#25633,
#25634,#25635,#25636,#25637,#25638,#25639,#25640,#25641,#25642,#25643,#25644,
#25645,#25646,#25647,#25648,#25649,#25650,#25651,#25652,#25653,#25654,#25655,
#25656,#25657,#25658,#25659,#25660,#25661,#25662,#25663,#25664,#25665,#25666,
#25667,#25668,#25669,#25670,#25671,#25672,#25673,#25674,#25675,#25676,#25677,
#25678,#25679,#25680,#25681,#25682,#25683,#25684));
#5554=EDGE_LOOP('',(#25685,#25686,#25687,#25688,#25689,#25690,#25691,#25692,
#25693,#25694,#25695,#25696,#25697,#25698,#25699,#25700,#25701,#25702,#25703,
#25704,#25705,#25706,#25707,#25708,#25709,#25710,#25711,#25712,#25713,#25714,
#25715,#25716,#25717,#25718,#25719,#25720,#25721,#25722,#25723,#25724,#25725,
#25726,#25727,#25728,#25729,#25730,#25731,#25732,#25733,#25734,#25735,#25736,
#25737,#25738,#25739,#25740,#25741,#25742,#25743,#25744,#25745,#25746,#25747,
#25748,#25749,#25750,#25751,#25752,#25753,#25754,#25755,#25756,#25757,#25758,
#25759,#25760,#25761,#25762,#25763,#25764,#25765,#25766,#25767,#25768,#25769,
#25770,#25771,#25772,#25773,#25774,#25775,#25776,#25777,#25778,#25779,#25780,
#25781,#25782,#25783,#25784,#25785,#25786,#25787));
#5555=EDGE_LOOP('',(#25788,#25789,#25790,#25791,#25792,#25793,#25794,#25795,
#25796,#25797,#25798,#25799,#25800,#25801,#25802,#25803,#25804,#25805,#25806,
#25807,#25808,#25809,#25810,#25811,#25812,#25813,#25814,#25815,#25816,#25817,
#25818,#25819,#25820,#25821,#25822,#25823,#25824,#25825,#25826,#25827,#25828,
#25829,#25830,#25831,#25832,#25833,#25834,#25835,#25836,#25837,#25838,#25839,
#25840,#25841,#25842,#25843,#25844,#25845,#25846,#25847,#25848,#25849,#25850,
#25851,#25852,#25853,#25854,#25855,#25856,#25857,#25858,#25859,#25860,#25861,
#25862,#25863,#25864,#25865,#25866,#25867,#25868,#25869,#25870,#25871,#25872,
#25873,#25874,#25875,#25876,#25877,#25878,#25879,#25880,#25881,#25882,#25883,
#25884,#25885,#25886,#25887,#25888,#25889,#25890));
#5556=EDGE_LOOP('',(#25891,#25892,#25893,#25894));
#5557=EDGE_LOOP('',(#25895,#25896,#25897,#25898));
#5558=EDGE_LOOP('',(#25899,#25900,#25901,#25902));
#5559=EDGE_LOOP('',(#25903,#25904,#25905,#25906));
#5560=EDGE_LOOP('',(#25907,#25908,#25909,#25910));
#5561=EDGE_LOOP('',(#25911,#25912,#25913,#25914));
#5562=EDGE_LOOP('',(#25915,#25916,#25917,#25918));
#5563=EDGE_LOOP('',(#25919,#25920,#25921,#25922));
#5564=EDGE_LOOP('',(#25923));
#5565=EDGE_LOOP('',(#25924,#25925,#25926,#25927,#25928,#25929,#25930));
#5566=EDGE_LOOP('',(#25931,#25932,#25933,#25934));
#5567=EDGE_LOOP('',(#25935,#25936,#25937,#25938));
#5568=EDGE_LOOP('',(#25939,#25940,#25941,#25942));
#5569=EDGE_LOOP('',(#25943,#25944,#25945,#25946));
#5570=EDGE_LOOP('',(#25947,#25948,#25949,#25950));
#5571=EDGE_LOOP('',(#25951,#25952,#25953,#25954,#25955,#25956));
#5572=EDGE_LOOP('',(#25957,#25958,#25959,#25960));
#5573=EDGE_LOOP('',(#25961));
#5574=EDGE_LOOP('',(#25962));
#5575=EDGE_LOOP('',(#25963,#25964,#25965,#25966));
#5576=EDGE_LOOP('',(#25967,#25968,#25969,#25970));
#5577=EDGE_LOOP('',(#25971,#25972,#25973,#25974));
#5578=EDGE_LOOP('',(#25975,#25976,#25977,#25978));
#5579=EDGE_LOOP('',(#25979,#25980,#25981,#25982));
#5580=EDGE_LOOP('',(#25983,#25984,#25985,#25986));
#5581=EDGE_LOOP('',(#25987,#25988,#25989,#25990));
#5582=EDGE_LOOP('',(#25991,#25992,#25993,#25994));
#5583=EDGE_LOOP('',(#25995));
#5584=EDGE_LOOP('',(#25996,#25997,#25998,#25999,#26000,#26001,#26002));
#5585=EDGE_LOOP('',(#26003,#26004,#26005,#26006,#26007,#26008,#26009));
#5586=EDGE_LOOP('',(#26010,#26011,#26012,#26013,#26014,#26015,#26016));
#5587=EDGE_LOOP('',(#26017,#26018,#26019,#26020));
#5588=EDGE_LOOP('',(#26021));
#5589=EDGE_LOOP('',(#26022,#26023,#26024,#26025,#26026));
#5590=EDGE_LOOP('',(#26027,#26028,#26029,#26030));
#5591=EDGE_LOOP('',(#26031));
#5592=EDGE_LOOP('',(#26032,#26033,#26034,#26035));
#5593=EDGE_LOOP('',(#26036,#26037,#26038,#26039));
#5594=EDGE_LOOP('',(#26040,#26041,#26042,#26043));
#5595=EDGE_LOOP('',(#26044,#26045,#26046,#26047));
#5596=EDGE_LOOP('',(#26048,#26049,#26050,#26051));
#5597=EDGE_LOOP('',(#26052,#26053,#26054,#26055,#26056,#26057));
#5598=EDGE_LOOP('',(#26058,#26059,#26060,#26061));
#5599=EDGE_LOOP('',(#26062));
#5600=EDGE_LOOP('',(#26063));
#5601=EDGE_LOOP('',(#26064,#26065,#26066,#26067));
#5602=EDGE_LOOP('',(#26068,#26069,#26070,#26071));
#5603=EDGE_LOOP('',(#26072,#26073,#26074,#26075));
#5604=EDGE_LOOP('',(#26076,#26077,#26078,#26079));
#5605=EDGE_LOOP('',(#26080,#26081,#26082,#26083));
#5606=EDGE_LOOP('',(#26084,#26085,#26086,#26087));
#5607=EDGE_LOOP('',(#26088,#26089,#26090,#26091));
#5608=EDGE_LOOP('',(#26092,#26093,#26094,#26095));
#5609=EDGE_LOOP('',(#26096));
#5610=EDGE_LOOP('',(#26097,#26098,#26099,#26100,#26101,#26102,#26103));
#5611=EDGE_LOOP('',(#26104,#26105,#26106,#26107));
#5612=EDGE_LOOP('',(#26108,#26109,#26110,#26111));
#5613=EDGE_LOOP('',(#26112,#26113,#26114,#26115));
#5614=EDGE_LOOP('',(#26116,#26117,#26118,#26119));
#5615=EDGE_LOOP('',(#26120,#26121,#26122,#26123));
#5616=EDGE_LOOP('',(#26124,#26125,#26126,#26127));
#5617=EDGE_LOOP('',(#26128,#26129,#26130,#26131));
#5618=EDGE_LOOP('',(#26132,#26133,#26134,#26135));
#5619=EDGE_LOOP('',(#26136));
#5620=EDGE_LOOP('',(#26137,#26138,#26139,#26140,#26141,#26142,#26143));
#5621=EDGE_LOOP('',(#26144,#26145,#26146,#26147,#26148,#26149,#26150));
#5622=EDGE_LOOP('',(#26151,#26152,#26153,#26154,#26155,#26156,#26157));
#5623=EDGE_LOOP('',(#26158,#26159,#26160,#26161,#26162,#26163,#26164,#26165,
#26166,#26167));
#5624=EDGE_LOOP('',(#26168));
#5625=EDGE_LOOP('',(#26169));
#5626=EDGE_LOOP('',(#26170,#26171,#26172,#26173,#26174));
#5627=EDGE_LOOP('',(#26175,#26176,#26177,#26178));
#5628=EDGE_LOOP('',(#26179));
#5629=EDGE_LOOP('',(#26180,#26181,#26182,#26183));
#5630=EDGE_LOOP('',(#26184));
#5631=EDGE_LOOP('',(#26185,#26186,#26187,#26188));
#5632=EDGE_LOOP('',(#26189));
#5633=EDGE_LOOP('',(#26190,#26191,#26192,#26193));
#5634=EDGE_LOOP('',(#26194));
#5635=EDGE_LOOP('',(#26195,#26196,#26197,#26198));
#5636=EDGE_LOOP('',(#26199,#26200,#26201,#26202));
#5637=EDGE_LOOP('',(#26203,#26204,#26205,#26206));
#5638=EDGE_LOOP('',(#26207,#26208,#26209,#26210));
#5639=EDGE_LOOP('',(#26211,#26212,#26213,#26214));
#5640=EDGE_LOOP('',(#26215,#26216,#26217,#26218));
#5641=EDGE_LOOP('',(#26219,#26220,#26221,#26222));
#5642=EDGE_LOOP('',(#26223,#26224,#26225,#26226));
#5643=EDGE_LOOP('',(#26227,#26228,#26229,#26230));
#5644=EDGE_LOOP('',(#26231,#26232,#26233,#26234));
#5645=EDGE_LOOP('',(#26235,#26236,#26237,#26238));
#5646=EDGE_LOOP('',(#26239,#26240,#26241,#26242));
#5647=EDGE_LOOP('',(#26243,#26244,#26245,#26246,#26247,#26248,#26249,#26250,
#26251,#26252));
#5648=EDGE_LOOP('',(#26253));
#5649=EDGE_LOOP('',(#26254));
#5650=EDGE_LOOP('',(#26255,#26256,#26257,#26258));
#5651=EDGE_LOOP('',(#26259,#26260,#26261,#26262));
#5652=EDGE_LOOP('',(#26263,#26264,#26265,#26266));
#5653=EDGE_LOOP('',(#26267,#26268,#26269,#26270));
#5654=EDGE_LOOP('',(#26271,#26272,#26273,#26274));
#5655=EDGE_LOOP('',(#26275,#26276,#26277,#26278));
#5656=EDGE_LOOP('',(#26279,#26280,#26281,#26282));
#5657=EDGE_LOOP('',(#26283,#26284,#26285,#26286,#26287,#26288));
#5658=EDGE_LOOP('',(#26289,#26290,#26291,#26292));
#5659=EDGE_LOOP('',(#26293,#26294,#26295,#26296,#26297,#26298,#26299,#26300,
#26301,#26302,#26303,#26304,#26305,#26306,#26307,#26308,#26309,#26310,#26311,
#26312,#26313,#26314,#26315,#26316,#26317,#26318));
#5660=EDGE_LOOP('',(#26319,#26320,#26321,#26322));
#5661=EDGE_LOOP('',(#26323,#26324,#26325,#26326));
#5662=EDGE_LOOP('',(#26327,#26328,#26329,#26330));
#5663=EDGE_LOOP('',(#26331,#26332,#26333,#26334));
#5664=CIRCLE('',#28181,0.127);
#5665=CIRCLE('',#28182,0.202999999999999);
#5666=CIRCLE('',#28183,0.127000000000001);
#5667=CIRCLE('',#28184,0.159000000000001);
#5668=CIRCLE('',#28185,0.203000000000001);
#5669=CIRCLE('',#28186,0.203);
#5670=CIRCLE('',#28187,0.159000000000001);
#5671=CIRCLE('',#28188,0.127000000000001);
#5672=CIRCLE('',#28189,0.203);
#5673=CIRCLE('',#28190,0.126999999999999);
#5674=CIRCLE('',#28194,0.127);
#5675=CIRCLE('',#28197,0.202999999999999);
#5676=CIRCLE('',#28200,0.127000000000001);
#5677=CIRCLE('',#28203,0.159000000000001);
#5678=CIRCLE('',#28206,0.203000000000001);
#5679=CIRCLE('',#28210,0.203);
#5680=CIRCLE('',#28213,0.159000000000001);
#5681=CIRCLE('',#28216,0.127000000000001);
#5682=CIRCLE('',#28219,0.203);
#5683=CIRCLE('',#28222,0.126999999999999);
#5684=CIRCLE('',#28229,0.203000000000002);
#5685=CIRCLE('',#28230,0.203000000000002);
#5686=CIRCLE('',#28231,0.159);
#5687=CIRCLE('',#28232,0.381);
#5688=CIRCLE('',#28233,2.54);
#5689=CIRCLE('',#28234,2.54);
#5690=CIRCLE('',#28235,0.381);
#5691=CIRCLE('',#28236,0.159);
#5692=CIRCLE('',#28238,0.203000000000002);
#5693=CIRCLE('',#28241,0.203000000000002);
#5694=CIRCLE('',#28244,0.159);
#5695=CIRCLE('',#28252,0.381);
#5696=CIRCLE('',#28255,2.54);
#5697=CIRCLE('',#28258,2.54);
#5698=CIRCLE('',#28261,0.381);
#5699=CIRCLE('',#28269,0.159);
#5700=CIRCLE('',#28274,5.099);
#5701=CIRCLE('',#28278,5.099);
#5702=CIRCLE('',#28280,5.099);
#5703=CIRCLE('',#28284,5.099);
#5704=CIRCLE('',#28286,2.55999999999999);
#5705=CIRCLE('',#28313,2.55999999999999);
#5706=CIRCLE('',#28315,2.56);
#5707=CIRCLE('',#28342,2.56);
#5708=CIRCLE('',#28344,2.56);
#5709=CIRCLE('',#28371,2.56);
#5710=CIRCLE('',#28373,2.56);
#5711=CIRCLE('',#28400,2.56);
#5712=CIRCLE('',#28402,4.263);
#5713=CIRCLE('',#28406,4.263);
#5714=CIRCLE('',#28408,4.263);
#5715=CIRCLE('',#28410,4.263);
#5716=CIRCLE('',#28413,4.263);
#5717=CIRCLE('',#28415,2.117);
#5718=CIRCLE('',#28442,2.117);
#5719=CIRCLE('',#28444,2.117);
#5720=CIRCLE('',#28471,2.117);
#5721=CIRCLE('',#28473,2.117);
#5722=CIRCLE('',#28500,2.117);
#5723=CIRCLE('',#28502,2.117);
#5724=CIRCLE('',#28529,2.117);
#5725=CIRCLE('',#28536,4.263);
#5726=CIRCLE('',#28544,4.);
#5727=CIRCLE('',#28545,4.);
#5728=CIRCLE('',#28548,4.5);
#5729=CIRCLE('',#28549,4.5);
#5730=CIRCLE('',#28551,3.9914370845599);
#5731=CIRCLE('',#28553,4.);
#5732=CIRCLE('',#28554,4.);
#5733=CIRCLE('',#28557,4.5);
#5734=CIRCLE('',#28558,4.5);
#5735=CIRCLE('',#28560,3.99143708455989);
#5736=CIRCLE('',#28562,5.);
#5737=CIRCLE('',#28563,5.);
#5738=CIRCLE('',#28569,0.191);
#5739=CIRCLE('',#28570,0.190999999999999);
#5740=CIRCLE('',#28571,0.253999999999999);
#5741=CIRCLE('',#28572,5.);
#5742=CIRCLE('',#28573,5.);
#5743=CIRCLE('',#28574,5.);
#5744=CIRCLE('',#28575,5.);
#5745=CIRCLE('',#28576,0.254);
#5746=CIRCLE('',#28577,0.190999999999999);
#5747=CIRCLE('',#28578,0.190999999999999);
#5748=CIRCLE('',#28579,2.5);
#5749=CIRCLE('',#28580,2.5);
#5750=CIRCLE('',#28589,3.);
#5751=CIRCLE('',#28590,3.);
#5752=CIRCLE('',#28593,6.);
#5753=CIRCLE('',#28594,6.);
#5754=CIRCLE('',#28597,6.);
#5755=CIRCLE('',#28598,6.);
#5756=CIRCLE('',#28602,4.);
#5757=CIRCLE('',#28603,5.);
#5758=CIRCLE('',#28612,3.);
#5759=CIRCLE('',#28613,3.);
#5760=CIRCLE('',#28618,4.);
#5761=CIRCLE('',#28622,5.);
#5762=CIRCLE('',#28625,6.);
#5763=CIRCLE('',#28626,6.);
#5764=CIRCLE('',#28629,6.);
#5765=CIRCLE('',#28630,6.);
#5766=CIRCLE('',#28634,4.);
#5767=CIRCLE('',#28635,5.);
#5768=CIRCLE('',#28644,3.);
#5769=CIRCLE('',#28645,3.);
#5770=CIRCLE('',#28655,3.);
#5771=CIRCLE('',#28656,3.);
#5772=CIRCLE('',#28663,5.);
#5773=CIRCLE('',#28666,4.);
#5774=CIRCLE('',#28669,2.5);
#5775=CIRCLE('',#28672,2.5);
#5776=CIRCLE('',#28676,3.99143708455989);
#5777=CIRCLE('',#28678,0.190999999999999);
#5778=CIRCLE('',#28681,0.190999999999999);
#5779=CIRCLE('',#28684,0.254);
#5780=CIRCLE('',#28687,5.);
#5781=CIRCLE('',#28689,5.);
#5782=CIRCLE('',#28692,5.);
#5783=CIRCLE('',#28695,5.);
#5784=CIRCLE('',#28698,0.253999999999999);
#5785=CIRCLE('',#28701,0.190999999999999);
#5786=CIRCLE('',#28704,0.191);
#5787=CIRCLE('',#28707,3.9914370845599);
#5788=CIRCLE('',#28712,3.);
#5789=CIRCLE('',#28713,3.);
#5790=CIRCLE('',#28716,3.);
#5791=CIRCLE('',#28717,3.);
#5792=CIRCLE('',#28720,0.499999999999998);
#5793=CIRCLE('',#28723,0.499999999999999);
#5794=CIRCLE('',#28725,0.5);
#5795=CIRCLE('',#28726,0.499999999999998);
#5796=CIRCLE('',#28728,0.499999999999998);
#5797=CIRCLE('',#28729,0.508000000000002);
#5798=CIRCLE('',#28730,1.008);
#5799=CIRCLE('',#28732,0.499999999999998);
#5800=CIRCLE('',#28734,0.499999999999998);
#5801=CIRCLE('',#28735,3.);
#5802=CIRCLE('',#28736,2.5);
#5803=CIRCLE('',#28738,0.499999999999998);
#5804=CIRCLE('',#28740,0.499999999999998);
#5805=CIRCLE('',#28741,5.);
#5806=CIRCLE('',#28742,4.5);
#5807=CIRCLE('',#28744,0.499999999999998);
#5808=CIRCLE('',#28745,0.499999999999998);
#5809=CIRCLE('',#28746,1.);
#5810=CIRCLE('',#28747,0.500000000000001);
#5811=CIRCLE('',#28753,0.499999999999998);
#5812=CIRCLE('',#28755,0.499999999999998);
#5813=CIRCLE('',#28756,0.999999999999992);
#5814=CIRCLE('',#28757,1.49999999999999);
#5815=CIRCLE('',#28762,0.499999999999998);
#5816=CIRCLE('',#28764,0.499999999999998);
#5817=CIRCLE('',#28765,1.);
#5818=CIRCLE('',#28766,1.5);
#5819=CIRCLE('',#28772,0.499999999999998);
#5820=CIRCLE('',#28773,0.499999999999998);
#5821=CIRCLE('',#28774,1.);
#5822=CIRCLE('',#28775,0.5);
#5823=CIRCLE('',#28777,0.499999999999998);
#5824=CIRCLE('',#28779,0.499999999999998);
#5825=CIRCLE('',#28780,5.);
#5826=CIRCLE('',#28781,4.5);
#5827=CIRCLE('',#28783,0.499999999999998);
#5828=CIRCLE('',#28785,0.499999999999998);
#5829=CIRCLE('',#28786,3.);
#5830=CIRCLE('',#28787,2.5);
#5831=CIRCLE('',#28789,0.499999999999998);
#5832=CIRCLE('',#28791,0.499999999999998);
#5833=CIRCLE('',#28792,0.508000000000002);
#5834=CIRCLE('',#28793,1.008);
#5835=CIRCLE('',#28795,0.499999999999998);
#5836=CIRCLE('',#28797,0.499999999999998);
#5837=CIRCLE('',#28798,0.499999999999998);
#5838=CIRCLE('',#28800,0.500000000000004);
#5839=CIRCLE('',#28802,0.499999999999993);
#5840=CIRCLE('',#28804,0.5);
#5841=CIRCLE('',#28806,0.499999999999998);
#5842=CIRCLE('',#28809,1.);
#5843=CIRCLE('',#28814,1.);
#5844=CIRCLE('',#28817,5.);
#5845=CIRCLE('',#28820,3.);
#5846=CIRCLE('',#28821,3.);
#5847=CIRCLE('',#28824,0.508000000000002);
#5848=CIRCLE('',#28827,0.5);
#5849=CIRCLE('',#28833,0.5);
#5850=CIRCLE('',#28835,3.5);
#5851=CIRCLE('',#28836,3.);
#5852=CIRCLE('',#28838,0.500000000000002);
#5853=CIRCLE('',#28839,0.5);
#5854=CIRCLE('',#28841,0.500000000000004);
#5855=CIRCLE('',#28843,0.499999999999998);
#5856=CIRCLE('',#28846,3.);
#5857=CIRCLE('',#28847,3.5);
#5858=CIRCLE('',#28849,0.5);
#5859=CIRCLE('',#28851,0.499999999999998);
#5860=CIRCLE('',#28853,0.499999999999998);
#5861=CIRCLE('',#28854,0.500000000000001);
#5862=CIRCLE('',#28856,4.5);
#5863=CIRCLE('',#28857,0.500000000000001);
#5864=CIRCLE('',#28858,1.49999999999999);
#5865=CIRCLE('',#28859,1.5);
#5866=CIRCLE('',#28860,0.5);
#5867=CIRCLE('',#28861,4.5);
#5868=CIRCLE('',#28863,0.499999999999999);
#5869=CIRCLE('',#28864,0.499999999999999);
#5870=CIRCLE('',#28866,3.);
#5871=CIRCLE('',#28868,0.5);
#5872=CIRCLE('',#28870,0.500000000000002);
#5873=CIRCLE('',#28872,0.499999999999998);
#5874=CIRCLE('',#28878,0.499999999999995);
#5875=CIRCLE('',#28881,0.5);
#5876=CIRCLE('',#28884,0.499999999999998);
#5877=CIRCLE('',#28887,0.499999999999999);
#5878=CIRCLE('',#28890,0.5);
#5879=CIRCLE('',#28893,0.500000000000001);
#5880=CIRCLE('',#28894,0.999999999999992);
#5881=CIRCLE('',#28899,0.499999999999998);
#5882=CIRCLE('',#28900,5.);
#5883=CIRCLE('',#28902,0.499999999999998);
#5884=CIRCLE('',#28903,0.5);
#5885=CIRCLE('',#28904,1.);
#5886=CIRCLE('',#28919,3.);
#5887=CIRCLE('',#28921,3.);
#5888=CIRCLE('',#28923,3.);
#5889=CIRCLE('',#28926,0.508000000000002);
#5890=CIRCLE('',#28933,3.);
#5891=CIRCLE('',#28934,3.);
#5892=CIRCLE('',#28937,3.);
#5893=CIRCLE('',#28938,3.);
#5894=CIRCLE('',#28942,0.499999999999998);
#5895=CIRCLE('',#28944,0.499999999999999);
#5896=CIRCLE('',#28946,0.5);
#5897=CIRCLE('',#28947,0.499999999999998);
#5898=CIRCLE('',#28949,0.499999999999998);
#5899=CIRCLE('',#28950,1.008);
#5900=CIRCLE('',#28951,0.508000000000002);
#5901=CIRCLE('',#28953,0.499999999999998);
#5902=CIRCLE('',#28955,0.499999999999998);
#5903=CIRCLE('',#28956,2.5);
#5904=CIRCLE('',#28957,3.);
#5905=CIRCLE('',#28959,0.499999999999998);
#5906=CIRCLE('',#28961,0.499999999999998);
#5907=CIRCLE('',#28962,4.5);
#5908=CIRCLE('',#28963,5.);
#5909=CIRCLE('',#28965,0.499999999999998);
#5910=CIRCLE('',#28966,0.499999999999998);
#5911=CIRCLE('',#28967,0.500000000000001);
#5912=CIRCLE('',#28968,1.);
#5913=CIRCLE('',#28974,0.499999999999998);
#5914=CIRCLE('',#28976,0.499999999999998);
#5915=CIRCLE('',#28977,1.49999999999999);
#5916=CIRCLE('',#28978,0.999999999999992);
#5917=CIRCLE('',#28983,0.499999999999998);
#5918=CIRCLE('',#28985,0.499999999999998);
#5919=CIRCLE('',#28986,1.5);
#5920=CIRCLE('',#28987,1.);
#5921=CIRCLE('',#28993,0.499999999999998);
#5922=CIRCLE('',#28994,0.499999999999998);
#5923=CIRCLE('',#28995,0.5);
#5924=CIRCLE('',#28996,1.);
#5925=CIRCLE('',#28998,0.499999999999998);
#5926=CIRCLE('',#29000,0.499999999999998);
#5927=CIRCLE('',#29001,4.5);
#5928=CIRCLE('',#29002,5.);
#5929=CIRCLE('',#29004,0.499999999999998);
#5930=CIRCLE('',#29006,0.499999999999998);
#5931=CIRCLE('',#29007,2.5);
#5932=CIRCLE('',#29008,3.);
#5933=CIRCLE('',#29010,0.499999999999998);
#5934=CIRCLE('',#29012,0.499999999999998);
#5935=CIRCLE('',#29013,1.008);
#5936=CIRCLE('',#29014,0.508000000000002);
#5937=CIRCLE('',#29016,0.499999999999998);
#5938=CIRCLE('',#29018,0.499999999999998);
#5939=CIRCLE('',#29019,0.499999999999998);
#5940=CIRCLE('',#29021,0.500000000000004);
#5941=CIRCLE('',#29023,0.499999999999993);
#5942=CIRCLE('',#29025,0.5);
#5943=CIRCLE('',#29027,0.499999999999998);
#5944=CIRCLE('',#29030,1.);
#5945=CIRCLE('',#29035,1.);
#5946=CIRCLE('',#29038,5.);
#5947=CIRCLE('',#29041,3.);
#5948=CIRCLE('',#29042,3.);
#5949=CIRCLE('',#29045,0.508000000000002);
#5950=CIRCLE('',#29048,0.5);
#5951=CIRCLE('',#29054,0.5);
#5952=CIRCLE('',#29056,3.5);
#5953=CIRCLE('',#29057,3.);
#5954=CIRCLE('',#29059,0.500000000000002);
#5955=CIRCLE('',#29060,0.5);
#5956=CIRCLE('',#29062,0.500000000000004);
#5957=CIRCLE('',#29064,0.499999999999998);
#5958=CIRCLE('',#29067,3.);
#5959=CIRCLE('',#29068,3.5);
#5960=CIRCLE('',#29070,0.5);
#5961=CIRCLE('',#29072,0.499999999999998);
#5962=CIRCLE('',#29074,0.500000000000001);
#5963=CIRCLE('',#29075,0.499999999999998);
#5964=CIRCLE('',#29077,4.5);
#5965=CIRCLE('',#29078,0.5);
#5966=CIRCLE('',#29079,1.5);
#5967=CIRCLE('',#29080,1.49999999999999);
#5968=CIRCLE('',#29081,0.500000000000001);
#5969=CIRCLE('',#29082,4.5);
#5970=CIRCLE('',#29084,0.499999999999999);
#5971=CIRCLE('',#29085,0.499999999999999);
#5972=CIRCLE('',#29087,3.);
#5973=CIRCLE('',#29090,0.5);
#5974=CIRCLE('',#29091,0.500000000000002);
#5975=CIRCLE('',#29093,0.499999999999998);
#5976=CIRCLE('',#29100,0.499999999999995);
#5977=CIRCLE('',#29102,0.5);
#5978=CIRCLE('',#29106,0.499999999999998);
#5979=CIRCLE('',#29108,0.499999999999999);
#5980=CIRCLE('',#29112,0.5);
#5981=CIRCLE('',#29114,0.500000000000001);
#5982=CIRCLE('',#29115,0.999999999999992);
#5983=CIRCLE('',#29120,0.499999999999998);
#5984=CIRCLE('',#29121,5.);
#5985=CIRCLE('',#29123,0.499999999999998);
#5986=CIRCLE('',#29124,0.5);
#5987=CIRCLE('',#29125,1.);
#5988=CIRCLE('',#29140,3.);
#5989=CIRCLE('',#29142,3.);
#5990=CIRCLE('',#29144,3.);
#5991=CIRCLE('',#29147,0.508000000000002);
#5992=CIRCLE('',#29153,3.00000000191135);
#5993=CIRCLE('',#29154,3.);
#5994=CIRCLE('',#29155,3.);
#5995=CIRCLE('',#29158,3.00000000191136);
#5996=CIRCLE('',#29159,3.00000000000001);
#5997=CIRCLE('',#29160,3.00000000000001);
#5998=CIRCLE('',#29164,3.);
#5999=CIRCLE('',#29166,3.);
#6000=CIRCLE('',#29167,3.);
#6001=CIRCLE('',#29168,3.);
#6002=CIRCLE('',#29175,3.00000000191135);
#6003=CIRCLE('',#29176,3.00000000191135);
#6004=CIRCLE('',#29177,3.00000000191135);
#6005=CIRCLE('',#29178,3.00000000191135);
#6006=CIRCLE('',#29184,3.);
#6007=CIRCLE('',#29186,3.);
#6008=CIRCLE('',#29187,3.);
#6009=CIRCLE('',#29188,3.);
#6010=CIRCLE('',#29195,3.00000000191135);
#6011=CIRCLE('',#29196,3.00000000191135);
#6012=CIRCLE('',#29197,3.00000000191135);
#6013=CIRCLE('',#29198,3.00000000191135);
#6014=CIRCLE('',#29204,3.00000000000001);
#6015=CIRCLE('',#29206,3.00000000000001);
#6016=CIRCLE('',#29207,3.00000000000001);
#6017=CIRCLE('',#29208,3.00000000000001);
#6018=CIRCLE('',#29215,3.00000000191136);
#6019=CIRCLE('',#29216,3.00000000191136);
#6020=CIRCLE('',#29217,3.00000000191136);
#6021=CIRCLE('',#29218,3.00000000191136);
#6022=CIRCLE('',#29224,0.3);
#6023=CIRCLE('',#29225,0.3);
#6024=CIRCLE('',#29230,0.499999999999998);
#6025=CIRCLE('',#29232,0.499999999999998);
#6026=CIRCLE('',#29238,1.);
#6027=CIRCLE('',#29240,1.);
#6028=CIRCLE('',#29246,2.);
#6029=CIRCLE('',#29248,2.);
#6030=CIRCLE('',#29254,5.);
#6031=CIRCLE('',#29256,5.);
#6032=CIRCLE('',#29262,0.800000000000001);
#6033=CIRCLE('',#29264,0.800000000000001);
#6034=CIRCLE('',#29270,0.3);
#6035=CIRCLE('',#29271,0.3);
#6036=CIRCLE('',#29276,0.499999999999998);
#6037=CIRCLE('',#29283,1.);
#6038=CIRCLE('',#29290,2.);
#6039=CIRCLE('',#29297,5.);
#6040=CIRCLE('',#29304,0.800000000000001);
#6041=CIRCLE('',#29311,2.5);
#6042=CIRCLE('',#29312,2.5);
#6043=CIRCLE('',#29314,2.5);
#6044=CIRCLE('',#29315,2.5);
#6045=CIRCLE('',#29317,2.5);
#6046=CIRCLE('',#29318,2.5);
#6047=CIRCLE('',#29322,0.3);
#6048=CIRCLE('',#29323,0.3);
#6049=CIRCLE('',#29326,0.300000000000002);
#6050=CIRCLE('',#29327,0.300000000000002);
#6051=CIRCLE('',#29341,0.300000000000002);
#6052=CIRCLE('',#29342,0.300000000000002);
#6053=CIRCLE('',#29345,0.500000000000001);
#6054=CIRCLE('',#29346,0.500000000000001);
#6055=CIRCLE('',#29349,0.508000000000002);
#6056=CIRCLE('',#29350,0.508000000000002);
#6057=CIRCLE('',#29353,3.);
#6058=CIRCLE('',#29354,3.);
#6059=CIRCLE('',#29357,5.);
#6060=CIRCLE('',#29358,5.);
#6061=CIRCLE('',#29361,1.);
#6062=CIRCLE('',#29362,1.);
#6063=CIRCLE('',#29367,1.);
#6064=CIRCLE('',#29368,1.);
#6065=CIRCLE('',#29374,0.3);
#6066=CIRCLE('',#29375,0.3);
#6067=CIRCLE('',#29378,0.300000000000002);
#6068=CIRCLE('',#29379,0.300000000000002);
#6069=CIRCLE('',#29382,0.800000000000001);
#6070=CIRCLE('',#29385,5.);
#6071=CIRCLE('',#29388,2.);
#6072=CIRCLE('',#29391,1.);
#6073=CIRCLE('',#29394,0.499999999999998);
#6074=CIRCLE('',#29398,0.300000000000002);
#6075=CIRCLE('',#29399,0.300000000000002);
#6076=CIRCLE('',#29402,0.5);
#6077=CIRCLE('',#29403,0.5);
#6078=CIRCLE('',#29406,0.508000000000002);
#6079=CIRCLE('',#29407,0.508000000000002);
#6080=CIRCLE('',#29410,3.);
#6081=CIRCLE('',#29411,3.);
#6082=CIRCLE('',#29414,5.);
#6083=CIRCLE('',#29415,5.);
#6084=CIRCLE('',#29418,1.);
#6085=CIRCLE('',#29419,1.);
#6086=CIRCLE('',#29424,1.);
#6087=CIRCLE('',#29425,1.);
#6088=CIRCLE('',#29435,3.9858295958384);
#6089=CIRCLE('',#29437,3.9858295958384);
#6090=CIRCLE('',#29439,3.9858295958384);
#6091=CIRCLE('',#29442,3.9858295958384);
#6092=CIRCLE('',#29443,3.9858295958384);
#6093=CIRCLE('',#29444,0.191);
#6094=CIRCLE('',#29445,0.590999999999999);
#6095=CIRCLE('',#29446,0.590999999999999);
#6096=CIRCLE('',#29447,0.190999999999998);
#6097=CIRCLE('',#29449,0.190999999999998);
#6098=CIRCLE('',#29452,0.590999999999999);
#6099=CIRCLE('',#29453,0.590999999999999);
#6100=CIRCLE('',#29454,0.191);
#6101=CIRCLE('',#29455,3.9858295958384);
#6102=CIRCLE('',#29456,0.191000000000001);
#6103=CIRCLE('',#29457,0.190999999999999);
#6104=CIRCLE('',#29458,0.190999999999999);
#6105=CIRCLE('',#29459,0.191);
#6106=CIRCLE('',#29460,3.9858295958384);
#6107=CIRCLE('',#29475,0.191);
#6108=CIRCLE('',#29476,0.190999999999999);
#6109=CIRCLE('',#29478,0.190999999999999);
#6110=CIRCLE('',#29479,0.191000000000001);
#6111=CIRCLE('',#29489,3.9858295958384);
#6112=CIRCLE('',#29491,3.9858295958384);
#6113=CIRCLE('',#29493,3.9858295958384);
#6114=CIRCLE('',#29497,3.9858295958384);
#6115=CIRCLE('',#29498,0.190999999999998);
#6116=CIRCLE('',#29499,0.590999999999999);
#6117=CIRCLE('',#29500,0.590999999999999);
#6118=CIRCLE('',#29501,0.191);
#6119=CIRCLE('',#29502,3.9858295958384);
#6120=CIRCLE('',#29505,0.190999999999998);
#6121=CIRCLE('',#29508,3.9858295958384);
#6122=CIRCLE('',#29509,0.191);
#6123=CIRCLE('',#29510,0.190999999999999);
#6124=CIRCLE('',#29511,0.190999999999999);
#6125=CIRCLE('',#29512,0.191000000000001);
#6126=CIRCLE('',#29513,3.9858295958384);
#6127=CIRCLE('',#29514,0.191);
#6128=CIRCLE('',#29515,0.590999999999999);
#6129=CIRCLE('',#29516,0.590999999999999);
#6130=CIRCLE('',#29535,0.190999999999999);
#6131=CIRCLE('',#29536,0.191);
#6132=CIRCLE('',#29538,0.191000000000001);
#6133=CIRCLE('',#29539,0.190999999999999);
#6134=CIRCLE('',#29552,12.5);
#6135=CIRCLE('',#29553,12.5);
#6136=CIRCLE('',#29555,0.999999999999998);
#6137=CIRCLE('',#29556,0.999999999999998);
#6138=CIRCLE('',#29563,1.);
#6139=CIRCLE('',#29564,1.);
#6140=CIRCLE('',#29568,0.299999999999999);
#6141=CIRCLE('',#29569,0.299999999999999);
#6142=CIRCLE('',#29571,0.75);
#6143=CIRCLE('',#29572,0.75);
#6144=CIRCLE('',#29574,0.300000000000001);
#6145=CIRCLE('',#29575,0.300000000000001);
#6146=CIRCLE('',#29580,1.);
#6147=CIRCLE('',#29581,1.);
#6148=CIRCLE('',#29584,0.499999999999999);
#6149=CIRCLE('',#29585,0.499999999999999);
#6150=CIRCLE('',#29588,0.299999999999998);
#6151=CIRCLE('',#29589,0.299999999999998);
#6152=CIRCLE('',#29594,0.999999999999998);
#6153=CIRCLE('',#29595,0.999999999999998);
#6154=CIRCLE('',#29598,5.);
#6155=CIRCLE('',#29599,5.);
#6156=CIRCLE('',#29602,5.);
#6157=CIRCLE('',#29603,5.);
#6158=CIRCLE('',#29606,0.999999999999996);
#6159=CIRCLE('',#29607,0.999999999999996);
#6160=CIRCLE('',#29612,0.299999999999998);
#6161=CIRCLE('',#29613,0.299999999999998);
#6162=CIRCLE('',#29616,0.5);
#6163=CIRCLE('',#29617,0.5);
#6164=CIRCLE('',#29620,1.);
#6165=CIRCLE('',#29621,1.);
#6166=CIRCLE('',#29626,0.300000000000002);
#6167=CIRCLE('',#29627,0.300000000000002);
#6168=CIRCLE('',#29629,0.75000062202425);
#6169=CIRCLE('',#29630,0.75000062202425);
#6170=CIRCLE('',#29632,0.300000000000001);
#6171=CIRCLE('',#29633,0.300000000000001);
#6172=CIRCLE('',#29637,1.);
#6173=CIRCLE('',#29638,1.);
#6174=CIRCLE('',#29645,1.);
#6175=CIRCLE('',#29646,1.);
#6176=CIRCLE('',#29650,0.300000000000002);
#6177=CIRCLE('',#29651,0.300000000000002);
#6178=CIRCLE('',#29653,0.75);
#6179=CIRCLE('',#29654,0.75);
#6180=CIRCLE('',#29656,0.300000000000001);
#6181=CIRCLE('',#29657,0.300000000000001);
#6182=CIRCLE('',#29662,1.);
#6183=CIRCLE('',#29663,1.);
#6184=CIRCLE('',#29666,0.500000000000003);
#6185=CIRCLE('',#29667,0.500000000000003);
#6186=CIRCLE('',#29670,0.299999999999998);
#6187=CIRCLE('',#29671,0.299999999999998);
#6188=CIRCLE('',#29676,1.);
#6189=CIRCLE('',#29677,1.);
#6190=CIRCLE('',#29680,4.99999999999999);
#6191=CIRCLE('',#29681,4.99999999999999);
#6192=CIRCLE('',#29684,4.99999999999999);
#6193=CIRCLE('',#29685,4.99999999999999);
#6194=CIRCLE('',#29688,1.);
#6195=CIRCLE('',#29689,1.);
#6196=CIRCLE('',#29694,0.300000000000003);
#6197=CIRCLE('',#29695,0.300000000000003);
#6198=CIRCLE('',#29698,0.5);
#6199=CIRCLE('',#29699,0.5);
#6200=CIRCLE('',#29702,1.);
#6201=CIRCLE('',#29703,1.);
#6202=CIRCLE('',#29708,0.300000000000001);
#6203=CIRCLE('',#29709,0.300000000000001);
#6204=CIRCLE('',#29711,0.750000622024213);
#6205=CIRCLE('',#29712,0.750000622024213);
#6206=CIRCLE('',#29714,0.300000000000001);
#6207=CIRCLE('',#29715,0.300000000000001);
#6208=CIRCLE('',#29722,5.099);
#6209=CIRCLE('',#29727,5.099);
#6210=CIRCLE('',#29732,2.55999999999999);
#6211=CIRCLE('',#29760,2.56);
#6212=CIRCLE('',#29788,2.56);
#6213=CIRCLE('',#29816,2.56);
#6214=CIRCLE('',#29844,4.263);
#6215=CIRCLE('',#29846,4.263);
#6216=CIRCLE('',#29850,4.263);
#6217=CIRCLE('',#29854,4.263);
#6218=CIRCLE('',#29856,2.117);
#6219=CIRCLE('',#29884,2.117);
#6220=CIRCLE('',#29912,2.117);
#6221=CIRCLE('',#29940,2.117);
#6222=CIRCLE('',#29968,2.117);
#6223=CIRCLE('',#29970,2.117);
#6224=CIRCLE('',#29972,2.117);
#6225=CIRCLE('',#29974,2.117);
#6226=CIRCLE('',#29976,4.263);
#6227=CIRCLE('',#29978,4.263);
#6228=CIRCLE('',#29980,2.56);
#6229=CIRCLE('',#29982,2.56);
#6230=CIRCLE('',#29984,2.56);
#6231=CIRCLE('',#29986,2.55999999999999);
#6232=CIRCLE('',#29988,5.099);
#6233=CIRCLE('',#29990,5.099);
#6234=CIRCLE('',#29992,4.);
#6235=CIRCLE('',#29993,4.);
#6236=CIRCLE('',#29996,4.5);
#6237=CIRCLE('',#29997,4.5);
#6238=CIRCLE('',#29999,3.9914370845599);
#6239=CIRCLE('',#30001,4.);
#6240=CIRCLE('',#30002,4.);
#6241=CIRCLE('',#30005,4.5);
#6242=CIRCLE('',#30006,4.5);
#6243=CIRCLE('',#30008,3.99143708455989);
#6244=CIRCLE('',#30010,5.);
#6245=CIRCLE('',#30011,5.);
#6246=CIRCLE('',#30017,0.190999999999999);
#6247=CIRCLE('',#30018,0.190999999999999);
#6248=CIRCLE('',#30019,0.254);
#6249=CIRCLE('',#30020,5.);
#6250=CIRCLE('',#30021,5.);
#6251=CIRCLE('',#30022,5.);
#6252=CIRCLE('',#30023,5.);
#6253=CIRCLE('',#30024,0.253999999999999);
#6254=CIRCLE('',#30025,0.190999999999999);
#6255=CIRCLE('',#30026,0.191);
#6256=CIRCLE('',#30027,2.5);
#6257=CIRCLE('',#30028,2.5);
#6258=CIRCLE('',#30037,3.);
#6259=CIRCLE('',#30038,3.);
#6260=CIRCLE('',#30041,6.);
#6261=CIRCLE('',#30042,6.);
#6262=CIRCLE('',#30045,6.);
#6263=CIRCLE('',#30046,6.);
#6264=CIRCLE('',#30050,4.);
#6265=CIRCLE('',#30051,5.);
#6266=CIRCLE('',#30060,3.);
#6267=CIRCLE('',#30061,3.);
#6268=CIRCLE('',#30066,4.);
#6269=CIRCLE('',#30070,5.);
#6270=CIRCLE('',#30073,6.);
#6271=CIRCLE('',#30074,6.);
#6272=CIRCLE('',#30077,6.);
#6273=CIRCLE('',#30078,6.);
#6274=CIRCLE('',#30082,4.);
#6275=CIRCLE('',#30083,5.);
#6276=CIRCLE('',#30092,3.);
#6277=CIRCLE('',#30093,3.);
#6278=CIRCLE('',#30103,3.);
#6279=CIRCLE('',#30104,3.);
#6280=CIRCLE('',#30111,5.);
#6281=CIRCLE('',#30114,4.);
#6282=CIRCLE('',#30117,2.5);
#6283=CIRCLE('',#30120,2.5);
#6284=CIRCLE('',#30124,3.99143708455989);
#6285=CIRCLE('',#30126,0.190999999999999);
#6286=CIRCLE('',#30129,0.190999999999999);
#6287=CIRCLE('',#30132,0.254);
#6288=CIRCLE('',#30135,5.);
#6289=CIRCLE('',#30137,5.);
#6290=CIRCLE('',#30140,5.);
#6291=CIRCLE('',#30143,5.);
#6292=CIRCLE('',#30146,0.253999999999999);
#6293=CIRCLE('',#30149,0.190999999999999);
#6294=CIRCLE('',#30152,0.191);
#6295=CIRCLE('',#30155,3.9914370845599);
#6296=LINE('',#35986,#8141);
#6297=LINE('',#35988,#8142);
#6298=LINE('',#35990,#8143);
#6299=LINE('',#35994,#8144);
#6300=LINE('',#35998,#8145);
#6301=LINE('',#36002,#8146);
#6302=LINE('',#36006,#8147);
#6303=LINE('',#36010,#8148);
#6304=LINE('',#36012,#8149);
#6305=LINE('',#36016,#8150);
#6306=LINE('',#36020,#8151);
#6307=LINE('',#36024,#8152);
#6308=LINE('',#36028,#8153);
#6309=LINE('',#36032,#8154);
#6310=LINE('',#36033,#8155);
#6311=LINE('',#36036,#8156);
#6312=LINE('',#36038,#8157);
#6313=LINE('',#36039,#8158);
#6314=LINE('',#36042,#8159);
#6315=LINE('',#36043,#8160);
#6316=LINE('',#36047,#8161);
#6317=LINE('',#36050,#8162);
#6318=LINE('',#36051,#8163);
#6319=LINE('',#36055,#8164);
#6320=LINE('',#36058,#8165);
#6321=LINE('',#36059,#8166);
#6322=LINE('',#36063,#8167);
#6323=LINE('',#36066,#8168);
#6324=LINE('',#36067,#8169);
#6325=LINE('',#36071,#8170);
#6326=LINE('',#36074,#8171);
#6327=LINE('',#36075,#8172);
#6328=LINE('',#36079,#8173);
#6329=LINE('',#36082,#8174);
#6330=LINE('',#36083,#8175);
#6331=LINE('',#36086,#8176);
#6332=LINE('',#36087,#8177);
#6333=LINE('',#36091,#8178);
#6334=LINE('',#36094,#8179);
#6335=LINE('',#36095,#8180);
#6336=LINE('',#36099,#8181);
#6337=LINE('',#36102,#8182);
#6338=LINE('',#36103,#8183);
#6339=LINE('',#36107,#8184);
#6340=LINE('',#36110,#8185);
#6341=LINE('',#36111,#8186);
#6342=LINE('',#36115,#8187);
#6343=LINE('',#36118,#8188);
#6344=LINE('',#36119,#8189);
#6345=LINE('',#36123,#8190);
#6346=LINE('',#36126,#8191);
#6347=LINE('',#36127,#8192);
#6348=LINE('',#36130,#8193);
#6349=LINE('',#36131,#8194);
#6350=LINE('',#36133,#8195);
#6351=LINE('',#36139,#8196);
#6352=LINE('',#36143,#8197);
#6353=LINE('',#36147,#8198);
#6354=LINE('',#36151,#8199);
#6355=LINE('',#36153,#8200);
#6356=LINE('',#36155,#8201);
#6357=LINE('',#36157,#8202);
#6358=LINE('',#36159,#8203);
#6359=LINE('',#36161,#8204);
#6360=LINE('',#36165,#8205);
#6361=LINE('',#36169,#8206);
#6362=LINE('',#36173,#8207);
#6363=LINE('',#36177,#8208);
#6364=LINE('',#36179,#8209);
#6365=LINE('',#36181,#8210);
#6366=LINE('',#36183,#8211);
#6367=LINE('',#36185,#8212);
#6368=LINE('',#36187,#8213);
#6369=LINE('',#36191,#8214);
#6370=LINE('',#36194,#8215);
#6371=LINE('',#36197,#8216);
#6372=LINE('',#36198,#8217);
#6373=LINE('',#36202,#8218);
#6374=LINE('',#36205,#8219);
#6375=LINE('',#36206,#8220);
#6376=LINE('',#36210,#8221);
#6377=LINE('',#36213,#8222);
#6378=LINE('',#36214,#8223);
#6379=LINE('',#36217,#8224);
#6380=LINE('',#36218,#8225);
#6381=LINE('',#36221,#8226);
#6382=LINE('',#36222,#8227);
#6383=LINE('',#36225,#8228);
#6384=LINE('',#36226,#8229);
#6385=LINE('',#36229,#8230);
#6386=LINE('',#36230,#8231);
#6387=LINE('',#36233,#8232);
#6388=LINE('',#36234,#8233);
#6389=LINE('',#36238,#8234);
#6390=LINE('',#36241,#8235);
#6391=LINE('',#36242,#8236);
#6392=LINE('',#36246,#8237);
#6393=LINE('',#36249,#8238);
#6394=LINE('',#36250,#8239);
#6395=LINE('',#36254,#8240);
#6396=LINE('',#36257,#8241);
#6397=LINE('',#36258,#8242);
#6398=LINE('',#36262,#8243);
#6399=LINE('',#36265,#8244);
#6400=LINE('',#36266,#8245);
#6401=LINE('',#36269,#8246);
#6402=LINE('',#36270,#8247);
#6403=LINE('',#36273,#8248);
#6404=LINE('',#36274,#8249);
#6405=LINE('',#36277,#8250);
#6406=LINE('',#36278,#8251);
#6407=LINE('',#36281,#8252);
#6408=LINE('',#36282,#8253);
#6409=LINE('',#36285,#8254);
#6410=LINE('',#36286,#8255);
#6411=LINE('',#36290,#8256);
#6412=LINE('',#36292,#8257);
#6413=LINE('',#36298,#8258);
#6414=LINE('',#36384,#8259);
#6415=LINE('',#36647,#8260);
#6416=LINE('',#37045,#8261);
#6417=LINE('',#37221,#8262);
#6418=LINE('',#37307,#8263);
#6419=LINE('',#37570,#8264);
#6420=LINE('',#37968,#8265);
#6421=LINE('',#38144,#8266);
#6422=LINE('',#38232,#8267);
#6423=LINE('',#38383,#8268);
#6424=LINE('',#38716,#8269);
#6425=LINE('',#38997,#8270);
#6426=LINE('',#39333,#8271);
#6427=LINE('',#39495,#8272);
#6428=LINE('',#39765,#8273);
#6429=LINE('',#40040,#8274);
#6430=LINE('',#40374,#8275);
#6431=LINE('',#40536,#8276);
#6432=LINE('',#40803,#8277);
#6433=LINE('',#41081,#8278);
#6434=LINE('',#41414,#8279);
#6435=LINE('',#41579,#8280);
#6436=LINE('',#41848,#8281);
#6437=LINE('',#42129,#8282);
#6438=LINE('',#42462,#8283);
#6439=LINE('',#42621,#8284);
#6440=LINE('',#42891,#8285);
#6441=LINE('',#43172,#8286);
#6442=LINE('',#43503,#8287);
#6443=LINE('',#43666,#8288);
#6444=LINE('',#43932,#8289);
#6445=LINE('',#44213,#8290);
#6446=LINE('',#44546,#8291);
#6447=LINE('',#44827,#8292);
#6448=LINE('',#44912,#8293);
#6449=LINE('',#45000,#8294);
#6450=LINE('',#45151,#8295);
#6451=LINE('',#45484,#8296);
#6452=LINE('',#45765,#8297);
#6453=LINE('',#46101,#8298);
#6454=LINE('',#46263,#8299);
#6455=LINE('',#46533,#8300);
#6456=LINE('',#46808,#8301);
#6457=LINE('',#47142,#8302);
#6458=LINE('',#47304,#8303);
#6459=LINE('',#47571,#8304);
#6460=LINE('',#47849,#8305);
#6461=LINE('',#48182,#8306);
#6462=LINE('',#48347,#8307);
#6463=LINE('',#48616,#8308);
#6464=LINE('',#48897,#8309);
#6465=LINE('',#49230,#8310);
#6466=LINE('',#49389,#8311);
#6467=LINE('',#49659,#8312);
#6468=LINE('',#49940,#8313);
#6469=LINE('',#50271,#8314);
#6470=LINE('',#50434,#8315);
#6471=LINE('',#50700,#8316);
#6472=LINE('',#50981,#8317);
#6473=LINE('',#51314,#8318);
#6474=LINE('',#51595,#8319);
#6475=LINE('',#51680,#8320);
#6476=LINE('',#51768,#8321);
#6477=LINE('',#51919,#8322);
#6478=LINE('',#52252,#8323);
#6479=LINE('',#52533,#8324);
#6480=LINE('',#52869,#8325);
#6481=LINE('',#53031,#8326);
#6482=LINE('',#53301,#8327);
#6483=LINE('',#53576,#8328);
#6484=LINE('',#53910,#8329);
#6485=LINE('',#54072,#8330);
#6486=LINE('',#54339,#8331);
#6487=LINE('',#54617,#8332);
#6488=LINE('',#54950,#8333);
#6489=LINE('',#55115,#8334);
#6490=LINE('',#55384,#8335);
#6491=LINE('',#55665,#8336);
#6492=LINE('',#55998,#8337);
#6493=LINE('',#56157,#8338);
#6494=LINE('',#56427,#8339);
#6495=LINE('',#56708,#8340);
#6496=LINE('',#57039,#8341);
#6497=LINE('',#57202,#8342);
#6498=LINE('',#57468,#8343);
#6499=LINE('',#57749,#8344);
#6500=LINE('',#58082,#8345);
#6501=LINE('',#58363,#8346);
#6502=LINE('',#58448,#8347);
#6503=LINE('',#58536,#8348);
#6504=LINE('',#58687,#8349);
#6505=LINE('',#59020,#8350);
#6506=LINE('',#59301,#8351);
#6507=LINE('',#59637,#8352);
#6508=LINE('',#59799,#8353);
#6509=LINE('',#60069,#8354);
#6510=LINE('',#60344,#8355);
#6511=LINE('',#60678,#8356);
#6512=LINE('',#60840,#8357);
#6513=LINE('',#61107,#8358);
#6514=LINE('',#61385,#8359);
#6515=LINE('',#61718,#8360);
#6516=LINE('',#61883,#8361);
#6517=LINE('',#62152,#8362);
#6518=LINE('',#62433,#8363);
#6519=LINE('',#62766,#8364);
#6520=LINE('',#62925,#8365);
#6521=LINE('',#63195,#8366);
#6522=LINE('',#63476,#8367);
#6523=LINE('',#63807,#8368);
#6524=LINE('',#63970,#8369);
#6525=LINE('',#64236,#8370);
#6526=LINE('',#64517,#8371);
#6527=LINE('',#64850,#8372);
#6528=LINE('',#65131,#8373);
#6529=LINE('',#65216,#8374);
#6530=LINE('',#65293,#8375);
#6531=LINE('',#65593,#8376);
#6532=LINE('',#66046,#8377);
#6533=LINE('',#66066,#8378);
#6534=LINE('',#66086,#8379);
#6535=LINE('',#66360,#8380);
#6536=LINE('',#66813,#8381);
#6537=LINE('',#66890,#8382);
#6538=LINE('',#67220,#8383);
#6539=LINE('',#67690,#8384);
#6540=LINE('',#68146,#8385);
#6541=LINE('',#68404,#8386);
#6542=LINE('',#68851,#8387);
#6543=LINE('',#69361,#8388);
#6544=LINE('',#69867,#8389);
#6545=LINE('',#70343,#8390);
#6546=LINE('',#70827,#8391);
#6547=LINE('',#71119,#8392);
#6548=LINE('',#71555,#8393);
#6549=LINE('',#71966,#8394);
#6550=LINE('',#72236,#8395);
#6551=LINE('',#72746,#8396);
#6552=LINE('',#73249,#8397);
#6553=LINE('',#73513,#8398);
#6554=LINE('',#73947,#8399);
#6555=LINE('',#74370,#8400);
#6556=LINE('',#74664,#8401);
#6557=LINE('',#75138,#8402);
#6558=LINE('',#75624,#8403);
#6559=LINE('',#76124,#8404);
#6560=LINE('',#76638,#8405);
#6561=LINE('',#77058,#8406);
#6562=LINE('',#77316,#8407);
#6563=LINE('',#77778,#8408);
#6564=LINE('',#78051,#8409);
#6565=LINE('',#78381,#8410);
#6566=LINE('',#78845,#8411);
#6567=LINE('',#79303,#8412);
#6568=LINE('',#79559,#8413);
#6569=LINE('',#80004,#8414);
#6570=LINE('',#80514,#8415);
#6571=LINE('',#81018,#8416);
#6572=LINE('',#81528,#8417);
#6573=LINE('',#82002,#8418);
#6574=LINE('',#82294,#8419);
#6575=LINE('',#82726,#8420);
#6576=LINE('',#83137,#8421);
#6577=LINE('',#83411,#8422);
#6578=LINE('',#83903,#8423);
#6579=LINE('',#84404,#8424);
#6580=LINE('',#84660,#8425);
#6581=LINE('',#85092,#8426);
#6582=LINE('',#85515,#8427);
#6583=LINE('',#85811,#8428);
#6584=LINE('',#86289,#8429);
#6585=LINE('',#86819,#8430);
#6586=LINE('',#87315,#8431);
#6587=LINE('',#87849,#8432);
#6588=LINE('',#88269,#8433);
#6589=LINE('',#88529,#8434);
#6590=LINE('',#88995,#8435);
#6591=LINE('',#89268,#8436);
#6592=LINE('',#89598,#8437);
#6593=LINE('',#90060,#8438);
#6594=LINE('',#90516,#8439);
#6595=LINE('',#90766,#8440);
#6596=LINE('',#91211,#8441);
#6597=LINE('',#91733,#8442);
#6598=LINE('',#92237,#8443);
#6599=LINE('',#92703,#8444);
#6600=LINE('',#93177,#8445);
#6601=LINE('',#93469,#8446);
#6602=LINE('',#93901,#8447);
#6603=LINE('',#94312,#8448);
#6604=LINE('',#94580,#8449);
#6605=LINE('',#95074,#8450);
#6606=LINE('',#95575,#8451);
#6607=LINE('',#95839,#8452);
#6608=LINE('',#96273,#8453);
#6609=LINE('',#96694,#8454);
#6610=LINE('',#96988,#8455);
#6611=LINE('',#97466,#8456);
#6612=LINE('',#97952,#8457);
#6613=LINE('',#98448,#8458);
#6614=LINE('',#98962,#8459);
#6615=LINE('',#99382,#8460);
#6616=LINE('',#99644,#8461);
#6617=LINE('',#100106,#8462);
#6618=LINE('',#100379,#8463);
#6619=LINE('',#100709,#8464);
#6620=LINE('',#101179,#8465);
#6621=LINE('',#101637,#8466);
#6622=LINE('',#101891,#8467);
#6623=LINE('',#102336,#8468);
#6624=LINE('',#102844,#8469);
#6625=LINE('',#103348,#8470);
#6626=LINE('',#103870,#8471);
#6627=LINE('',#104354,#8472);
#6628=LINE('',#104648,#8473);
#6629=LINE('',#105084,#8474);
#6630=LINE('',#105495,#8475);
#6631=LINE('',#105759,#8476);
#6632=LINE('',#106251,#8477);
#6633=LINE('',#106804,#8478);
#6634=LINE('',#107064,#8479);
#6635=LINE('',#107496,#8480);
#6636=LINE('',#107919,#8481);
#6637=LINE('',#108215,#8482);
#6638=LINE('',#108689,#8483);
#6639=LINE('',#109167,#8484);
#6640=LINE('',#109663,#8485);
#6641=LINE('',#110187,#8486);
#6642=LINE('',#110607,#8487);
#6643=LINE('',#110867,#8488);
#6644=LINE('',#111329,#8489);
#6645=LINE('',#115117,#8490);
#6646=LINE('',#115125,#8491);
#6647=LINE('',#115128,#8492);
#6648=LINE('',#115131,#8493);
#6649=LINE('',#115133,#8494);
#6650=LINE('',#115135,#8495);
#6651=LINE('',#115141,#8496);
#6652=LINE('',#115149,#8497);
#6653=LINE('',#115152,#8498);
#6654=LINE('',#115156,#8499);
#6655=LINE('',#115157,#8500);
#6656=LINE('',#115159,#8501);
#6657=LINE('',#115165,#8502);
#6658=LINE('',#115170,#8503);
#6659=LINE('',#115172,#8504);
#6660=LINE('',#115173,#8505);
#6661=LINE('',#115176,#8506);
#6662=LINE('',#115178,#8507);
#6663=LINE('',#115180,#8508);
#6664=LINE('',#115181,#8509);
#6665=LINE('',#115183,#8510);
#6666=LINE('',#115185,#8511);
#6667=LINE('',#115186,#8512);
#6668=LINE('',#115189,#8513);
#6669=LINE('',#115193,#8514);
#6670=LINE('',#115197,#8515);
#6671=LINE('',#115201,#8516);
#6672=LINE('',#115205,#8517);
#6673=LINE('',#115207,#8518);
#6674=LINE('',#115209,#8519);
#6675=LINE('',#115211,#8520);
#6676=LINE('',#115213,#8521);
#6677=LINE('',#115217,#8522);
#6678=LINE('',#115221,#8523);
#6679=LINE('',#115223,#8524);
#6680=LINE('',#115225,#8525);
#6681=LINE('',#115227,#8526);
#6682=LINE('',#115229,#8527);
#6683=LINE('',#115233,#8528);
#6684=LINE('',#115237,#8529);
#6685=LINE('',#115241,#8530);
#6686=LINE('',#124045,#8531);
#6687=LINE('',#124047,#8532);
#6688=LINE('',#124049,#8533);
#6689=LINE('',#124050,#8534);
#6690=LINE('',#124053,#8535);
#6691=LINE('',#124055,#8536);
#6692=LINE('',#124056,#8537);
#6693=LINE('',#124059,#8538);
#6694=LINE('',#124061,#8539);
#6695=LINE('',#124062,#8540);
#6696=LINE('',#124065,#8541);
#6697=LINE('',#124067,#8542);
#6698=LINE('',#124068,#8543);
#6699=LINE('',#124071,#8544);
#6700=LINE('',#124073,#8545);
#6701=LINE('',#124074,#8546);
#6702=LINE('',#124077,#8547);
#6703=LINE('',#124079,#8548);
#6704=LINE('',#124080,#8549);
#6705=LINE('',#124082,#8550);
#6706=LINE('',#124083,#8551);
#6707=LINE('',#124088,#8552);
#6708=LINE('',#124096,#8553);
#6709=LINE('',#124099,#8554);
#6710=LINE('',#124102,#8555);
#6711=LINE('',#124104,#8556);
#6712=LINE('',#124105,#8557);
#6713=LINE('',#124111,#8558);
#6714=LINE('',#124113,#8559);
#6715=LINE('',#124114,#8560);
#6716=LINE('',#124116,#8561);
#6717=LINE('',#124117,#8562);
#6718=LINE('',#124126,#8563);
#6719=LINE('',#124128,#8564);
#6720=LINE('',#124130,#8565);
#6721=LINE('',#124131,#8566);
#6722=LINE('',#124134,#8567);
#6723=LINE('',#124136,#8568);
#6724=LINE('',#124137,#8569);
#6725=LINE('',#124140,#8570);
#6726=LINE('',#124142,#8571);
#6727=LINE('',#124143,#8572);
#6728=LINE('',#124146,#8573);
#6729=LINE('',#124148,#8574);
#6730=LINE('',#124149,#8575);
#6731=LINE('',#124152,#8576);
#6732=LINE('',#124154,#8577);
#6733=LINE('',#124155,#8578);
#6734=LINE('',#124158,#8579);
#6735=LINE('',#124160,#8580);
#6736=LINE('',#124161,#8581);
#6737=LINE('',#124163,#8582);
#6738=LINE('',#124164,#8583);
#6739=LINE('',#124169,#8584);
#6740=LINE('',#124177,#8585);
#6741=LINE('',#124183,#8586);
#6742=LINE('',#124190,#8587);
#6743=LINE('',#124193,#8588);
#6744=LINE('',#124196,#8589);
#6745=LINE('',#124198,#8590);
#6746=LINE('',#124199,#8591);
#6747=LINE('',#124204,#8592);
#6748=LINE('',#124207,#8593);
#6749=LINE('',#124208,#8594);
#6750=LINE('',#124210,#8595);
#6751=LINE('',#124211,#8596);
#6752=LINE('',#124220,#8597);
#6753=LINE('',#124222,#8598);
#6754=LINE('',#124224,#8599);
#6755=LINE('',#124225,#8600);
#6756=LINE('',#124228,#8601);
#6757=LINE('',#124230,#8602);
#6758=LINE('',#124231,#8603);
#6759=LINE('',#124234,#8604);
#6760=LINE('',#124236,#8605);
#6761=LINE('',#124237,#8606);
#6762=LINE('',#124240,#8607);
#6763=LINE('',#124242,#8608);
#6764=LINE('',#124243,#8609);
#6765=LINE('',#124246,#8610);
#6766=LINE('',#124248,#8611);
#6767=LINE('',#124249,#8612);
#6768=LINE('',#124252,#8613);
#6769=LINE('',#124254,#8614);
#6770=LINE('',#124255,#8615);
#6771=LINE('',#124257,#8616);
#6772=LINE('',#124258,#8617);
#6773=LINE('',#124263,#8618);
#6774=LINE('',#124269,#8619);
#6775=LINE('',#124271,#8620);
#6776=LINE('',#124273,#8621);
#6777=LINE('',#124274,#8622);
#6778=LINE('',#124277,#8623);
#6779=LINE('',#124279,#8624);
#6780=LINE('',#124280,#8625);
#6781=LINE('',#124283,#8626);
#6782=LINE('',#124285,#8627);
#6783=LINE('',#124286,#8628);
#6784=LINE('',#124289,#8629);
#6785=LINE('',#124291,#8630);
#6786=LINE('',#124292,#8631);
#6787=LINE('',#124295,#8632);
#6788=LINE('',#124297,#8633);
#6789=LINE('',#124298,#8634);
#6790=LINE('',#124301,#8635);
#6791=LINE('',#124303,#8636);
#6792=LINE('',#124304,#8637);
#6793=LINE('',#124306,#8638);
#6794=LINE('',#124307,#8639);
#6795=LINE('',#124312,#8640);
#6796=LINE('',#124319,#8641);
#6797=LINE('',#124321,#8642);
#6798=LINE('',#124322,#8643);
#6799=LINE('',#124326,#8644);
#6800=LINE('',#124331,#8645);
#6801=LINE('',#124336,#8646);
#6802=LINE('',#124341,#8647);
#6803=LINE('',#124346,#8648);
#6804=LINE('',#124347,#8649);
#6805=LINE('',#124353,#8650);
#6806=LINE('',#124356,#8651);
#6807=LINE('',#124357,#8652);
#6808=LINE('',#124361,#8653);
#6809=LINE('',#124364,#8654);
#6810=LINE('',#124365,#8655);
#6811=LINE('',#124369,#8656);
#6812=LINE('',#124372,#8657);
#6813=LINE('',#124373,#8658);
#6814=LINE('',#124379,#8659);
#6815=LINE('',#124382,#8660);
#6816=LINE('',#124383,#8661);
#6817=LINE('',#124387,#8662);
#6818=LINE('',#124390,#8663);
#6819=LINE('',#124391,#8664);
#6820=LINE('',#124395,#8665);
#6821=LINE('',#124398,#8666);
#6822=LINE('',#124399,#8667);
#6823=LINE('',#124403,#8668);
#6824=LINE('',#124406,#8669);
#6825=LINE('',#124407,#8670);
#6826=LINE('',#124411,#8671);
#6827=LINE('',#124414,#8672);
#6828=LINE('',#124415,#8673);
#6829=LINE('',#124419,#8674);
#6830=LINE('',#124422,#8675);
#6831=LINE('',#124423,#8676);
#6832=LINE('',#124433,#8677);
#6833=LINE('',#124440,#8678);
#6834=LINE('',#124446,#8679);
#6835=LINE('',#124450,#8680);
#6836=LINE('',#124454,#8681);
#6837=LINE('',#124457,#8682);
#6838=LINE('',#124463,#8683);
#6839=LINE('',#124466,#8684);
#6840=LINE('',#124477,#8685);
#6841=LINE('',#124478,#8686);
#6842=LINE('',#124489,#8687);
#6843=LINE('',#124490,#8688);
#6844=LINE('',#124501,#8689);
#6845=LINE('',#124502,#8690);
#6846=LINE('',#124519,#8691);
#6847=LINE('',#124521,#8692);
#6848=LINE('',#124525,#8693);
#6849=LINE('',#124527,#8694);
#6850=LINE('',#124531,#8695);
#6851=LINE('',#124534,#8696);
#6852=LINE('',#124543,#8697);
#6853=LINE('',#124545,#8698);
#6854=LINE('',#124548,#8699);
#6855=LINE('',#124549,#8700);
#6856=LINE('',#124552,#8701);
#6857=LINE('',#124555,#8702);
#6858=LINE('',#124564,#8703);
#6859=LINE('',#124566,#8704);
#6860=LINE('',#124570,#8705);
#6861=LINE('',#124573,#8706);
#6862=LINE('',#124576,#8707);
#6863=LINE('',#124579,#8708);
#6864=LINE('',#124598,#8709);
#6865=LINE('',#124599,#8710);
#6866=LINE('',#124610,#8711);
#6867=LINE('',#124611,#8712);
#6868=LINE('',#124622,#8713);
#6869=LINE('',#124623,#8714);
#6870=LINE('',#124634,#8715);
#6871=LINE('',#124635,#8716);
#6872=LINE('',#124640,#8717);
#6873=LINE('',#124643,#8718);
#6874=LINE('',#124646,#8719);
#6875=LINE('',#124649,#8720);
#6876=LINE('',#124652,#8721);
#6877=LINE('',#124654,#8722);
#6878=LINE('',#124661,#8723);
#6879=LINE('',#124663,#8724);
#6880=LINE('',#124664,#8725);
#6881=LINE('',#124667,#8726);
#6882=LINE('',#124671,#8727);
#6883=LINE('',#124672,#8728);
#6884=LINE('',#124675,#8729);
#6885=LINE('',#124676,#8730);
#6886=LINE('',#124679,#8731);
#6887=LINE('',#124680,#8732);
#6888=LINE('',#124683,#8733);
#6889=LINE('',#124687,#8734);
#6890=LINE('',#124688,#8735);
#6891=LINE('',#124691,#8736);
#6892=LINE('',#124695,#8737);
#6893=LINE('',#124696,#8738);
#6894=LINE('',#124699,#8739);
#6895=LINE('',#124703,#8740);
#6896=LINE('',#124707,#8741);
#6897=LINE('',#124708,#8742);
#6898=LINE('',#124711,#8743);
#6899=LINE('',#124715,#8744);
#6900=LINE('',#124717,#8745);
#6901=LINE('',#124719,#8746);
#6902=LINE('',#124720,#8747);
#6903=LINE('',#124723,#8748);
#6904=LINE('',#124727,#8749);
#6905=LINE('',#124728,#8750);
#6906=LINE('',#124731,#8751);
#6907=LINE('',#124732,#8752);
#6908=LINE('',#124735,#8753);
#6909=LINE('',#124736,#8754);
#6910=LINE('',#124742,#8755);
#6911=LINE('',#124785,#8756);
#6912=LINE('',#124790,#8757);
#6913=LINE('',#124794,#8758);
#6914=LINE('',#124839,#8759);
#6915=LINE('',#124842,#8760);
#6916=LINE('',#124847,#8761);
#6917=LINE('',#124852,#8762);
#6918=LINE('',#124856,#8763);
#6919=LINE('',#124860,#8764);
#6920=LINE('',#124862,#8765);
#6921=LINE('',#124864,#8766);
#6922=LINE('',#124868,#8767);
#6923=LINE('',#124870,#8768);
#6924=LINE('',#124872,#8769);
#6925=LINE('',#124874,#8770);
#6926=LINE('',#124876,#8771);
#6927=LINE('',#124880,#8772);
#6928=LINE('',#124882,#8773);
#6929=LINE('',#124884,#8774);
#6930=LINE('',#124888,#8775);
#6931=LINE('',#124894,#8776);
#6932=LINE('',#124926,#8777);
#6933=LINE('',#124932,#8778);
#6934=LINE('',#124934,#8779);
#6935=LINE('',#124938,#8780);
#6936=LINE('',#124946,#8781);
#6937=LINE('',#124949,#8782);
#6938=LINE('',#124958,#8783);
#6939=LINE('',#124972,#8784);
#6940=LINE('',#124974,#8785);
#6941=LINE('',#124976,#8786);
#6942=LINE('',#124978,#8787);
#6943=LINE('',#124980,#8788);
#6944=LINE('',#124982,#8789);
#6945=LINE('',#124984,#8790);
#6946=LINE('',#124986,#8791);
#6947=LINE('',#124988,#8792);
#6948=LINE('',#124990,#8793);
#6949=LINE('',#124992,#8794);
#6950=LINE('',#124994,#8795);
#6951=LINE('',#124996,#8796);
#6952=LINE('',#124999,#8797);
#6953=LINE('',#125002,#8798);
#6954=LINE('',#125005,#8799);
#6955=LINE('',#125012,#8800);
#6956=LINE('',#125014,#8801);
#6957=LINE('',#125017,#8802);
#6958=LINE('',#125019,#8803);
#6959=LINE('',#125021,#8804);
#6960=LINE('',#125028,#8805);
#6961=LINE('',#125035,#8806);
#6962=LINE('',#125041,#8807);
#6963=LINE('',#125045,#8808);
#6964=LINE('',#125049,#8809);
#6965=LINE('',#125052,#8810);
#6966=LINE('',#125058,#8811);
#6967=LINE('',#125061,#8812);
#6968=LINE('',#125072,#8813);
#6969=LINE('',#125073,#8814);
#6970=LINE('',#125084,#8815);
#6971=LINE('',#125085,#8816);
#6972=LINE('',#125096,#8817);
#6973=LINE('',#125097,#8818);
#6974=LINE('',#125114,#8819);
#6975=LINE('',#125117,#8820);
#6976=LINE('',#125120,#8821);
#6977=LINE('',#125123,#8822);
#6978=LINE('',#125126,#8823);
#6979=LINE('',#125128,#8824);
#6980=LINE('',#125138,#8825);
#6981=LINE('',#125141,#8826);
#6982=LINE('',#125143,#8827);
#6983=LINE('',#125144,#8828);
#6984=LINE('',#125147,#8829);
#6985=LINE('',#125149,#8830);
#6986=LINE('',#125159,#8831);
#6987=LINE('',#125162,#8832);
#6988=LINE('',#125165,#8833);
#6989=LINE('',#125167,#8834);
#6990=LINE('',#125171,#8835);
#6991=LINE('',#125173,#8836);
#6992=LINE('',#125193,#8837);
#6993=LINE('',#125194,#8838);
#6994=LINE('',#125205,#8839);
#6995=LINE('',#125206,#8840);
#6996=LINE('',#125217,#8841);
#6997=LINE('',#125218,#8842);
#6998=LINE('',#125229,#8843);
#6999=LINE('',#125230,#8844);
#7000=LINE('',#125236,#8845);
#7001=LINE('',#125238,#8846);
#7002=LINE('',#125241,#8847);
#7003=LINE('',#125244,#8848);
#7004=LINE('',#125246,#8849);
#7005=LINE('',#125249,#8850);
#7006=LINE('',#125256,#8851);
#7007=LINE('',#125258,#8852);
#7008=LINE('',#125259,#8853);
#7009=LINE('',#125263,#8854);
#7010=LINE('',#125266,#8855);
#7011=LINE('',#125267,#8856);
#7012=LINE('',#125270,#8857);
#7013=LINE('',#125271,#8858);
#7014=LINE('',#125274,#8859);
#7015=LINE('',#125275,#8860);
#7016=LINE('',#125279,#8861);
#7017=LINE('',#125282,#8862);
#7018=LINE('',#125283,#8863);
#7019=LINE('',#125287,#8864);
#7020=LINE('',#125290,#8865);
#7021=LINE('',#125291,#8866);
#7022=LINE('',#125296,#8867);
#7023=LINE('',#125299,#8868);
#7024=LINE('',#125302,#8869);
#7025=LINE('',#125303,#8870);
#7026=LINE('',#125307,#8871);
#7027=LINE('',#125310,#8872);
#7028=LINE('',#125312,#8873);
#7029=LINE('',#125314,#8874);
#7030=LINE('',#125315,#8875);
#7031=LINE('',#125319,#8876);
#7032=LINE('',#125322,#8877);
#7033=LINE('',#125323,#8878);
#7034=LINE('',#125326,#8879);
#7035=LINE('',#125327,#8880);
#7036=LINE('',#125330,#8881);
#7037=LINE('',#125331,#8882);
#7038=LINE('',#125350,#8883);
#7039=LINE('',#125381,#8884);
#7040=LINE('',#125385,#8885);
#7041=LINE('',#125388,#8886);
#7042=LINE('',#125434,#8887);
#7043=LINE('',#125436,#8888);
#7044=LINE('',#125444,#8889);
#7045=LINE('',#125449,#8890);
#7046=LINE('',#125453,#8891);
#7047=LINE('',#125455,#8892);
#7048=LINE('',#125457,#8893);
#7049=LINE('',#125461,#8894);
#7050=LINE('',#125463,#8895);
#7051=LINE('',#125465,#8896);
#7052=LINE('',#125467,#8897);
#7053=LINE('',#125469,#8898);
#7054=LINE('',#125473,#8899);
#7055=LINE('',#125475,#8900);
#7056=LINE('',#125477,#8901);
#7057=LINE('',#125481,#8902);
#7058=LINE('',#125484,#8903);
#7059=LINE('',#125489,#8904);
#7060=LINE('',#125521,#8905);
#7061=LINE('',#125527,#8906);
#7062=LINE('',#125529,#8907);
#7063=LINE('',#125533,#8908);
#7064=LINE('',#125541,#8909);
#7065=LINE('',#125544,#8910);
#7066=LINE('',#125553,#8911);
#7067=LINE('',#125567,#8912);
#7068=LINE('',#125569,#8913);
#7069=LINE('',#125571,#8914);
#7070=LINE('',#125573,#8915);
#7071=LINE('',#125575,#8916);
#7072=LINE('',#125577,#8917);
#7073=LINE('',#125579,#8918);
#7074=LINE('',#125581,#8919);
#7075=LINE('',#125583,#8920);
#7076=LINE('',#125585,#8921);
#7077=LINE('',#125587,#8922);
#7078=LINE('',#125589,#8923);
#7079=LINE('',#125591,#8924);
#7080=LINE('',#125594,#8925);
#7081=LINE('',#125597,#8926);
#7082=LINE('',#125601,#8927);
#7083=LINE('',#125607,#8928);
#7084=LINE('',#125610,#8929);
#7085=LINE('',#125612,#8930);
#7086=LINE('',#125614,#8931);
#7087=LINE('',#125616,#8932);
#7088=LINE('',#125624,#8933);
#7089=LINE('',#125633,#8934);
#7090=LINE('',#125637,#8935);
#7091=LINE('',#125639,#8936);
#7092=LINE('',#125641,#8937);
#7093=LINE('',#125643,#8938);
#7094=LINE('',#125645,#8939);
#7095=LINE('',#125646,#8940);
#7096=LINE('',#125650,#8941);
#7097=LINE('',#125656,#8942);
#7098=LINE('',#125676,#8943);
#7099=LINE('',#125705,#8944);
#7100=LINE('',#125736,#8945);
#7101=LINE('',#125764,#8946);
#7102=LINE('',#125793,#8947);
#7103=LINE('',#125814,#8948);
#7104=LINE('',#125835,#8949);
#7105=LINE('',#125864,#8950);
#7106=LINE('',#125894,#8951);
#7107=LINE('',#125933,#8952);
#7108=LINE('',#125967,#8953);
#7109=LINE('',#125993,#8954);
#7110=LINE('',#126015,#8955);
#7111=LINE('',#126037,#8956);
#7112=LINE('',#126056,#8957);
#7113=LINE('',#126062,#8958);
#7114=LINE('',#126082,#8959);
#7115=LINE('',#126111,#8960);
#7116=LINE('',#126142,#8961);
#7117=LINE('',#126170,#8962);
#7118=LINE('',#126199,#8963);
#7119=LINE('',#126220,#8964);
#7120=LINE('',#126241,#8965);
#7121=LINE('',#126270,#8966);
#7122=LINE('',#126300,#8967);
#7123=LINE('',#126339,#8968);
#7124=LINE('',#126373,#8969);
#7125=LINE('',#126399,#8970);
#7126=LINE('',#126421,#8971);
#7127=LINE('',#126443,#8972);
#7128=LINE('',#126462,#8973);
#7129=LINE('',#126468,#8974);
#7130=LINE('',#126490,#8975);
#7131=LINE('',#126519,#8976);
#7132=LINE('',#126552,#8977);
#7133=LINE('',#126580,#8978);
#7134=LINE('',#126609,#8979);
#7135=LINE('',#126630,#8980);
#7136=LINE('',#126651,#8981);
#7137=LINE('',#126680,#8982);
#7138=LINE('',#126710,#8983);
#7139=LINE('',#126749,#8984);
#7140=LINE('',#126783,#8985);
#7141=LINE('',#126809,#8986);
#7142=LINE('',#126831,#8987);
#7143=LINE('',#126853,#8988);
#7144=LINE('',#126871,#8989);
#7145=LINE('',#126875,#8990);
#7146=LINE('',#126878,#8991);
#7147=LINE('',#126879,#8992);
#7148=LINE('',#126880,#8993);
#7149=LINE('',#126883,#8994);
#7150=LINE('',#126884,#8995);
#7151=LINE('',#126887,#8996);
#7152=LINE('',#126888,#8997);
#7153=LINE('',#126890,#8998);
#7154=LINE('',#126893,#8999);
#7155=LINE('',#126898,#9000);
#7156=LINE('',#126900,#9001);
#7157=LINE('',#126903,#9002);
#7158=LINE('',#126904,#9003);
#7159=LINE('',#126907,#9004);
#7160=LINE('',#126908,#9005);
#7161=LINE('',#126910,#9006);
#7162=LINE('',#126913,#9007);
#7163=LINE('',#126918,#9008);
#7164=LINE('',#126920,#9009);
#7165=LINE('',#126923,#9010);
#7166=LINE('',#126924,#9011);
#7167=LINE('',#126927,#9012);
#7168=LINE('',#126928,#9013);
#7169=LINE('',#126930,#9014);
#7170=LINE('',#126933,#9015);
#7171=LINE('',#126938,#9016);
#7172=LINE('',#126940,#9017);
#7173=LINE('',#126943,#9018);
#7174=LINE('',#126944,#9019);
#7175=LINE('',#126947,#9020);
#7176=LINE('',#126948,#9021);
#7177=LINE('',#126950,#9022);
#7178=LINE('',#126953,#9023);
#7179=LINE('',#126958,#9024);
#7180=LINE('',#126960,#9025);
#7181=LINE('',#126963,#9026);
#7182=LINE('',#126964,#9027);
#7183=LINE('',#126967,#9028);
#7184=LINE('',#126968,#9029);
#7185=LINE('',#126970,#9030);
#7186=LINE('',#126973,#9031);
#7187=LINE('',#126978,#9032);
#7188=LINE('',#126980,#9033);
#7189=LINE('',#126983,#9034);
#7190=LINE('',#126984,#9035);
#7191=LINE('',#126987,#9036);
#7192=LINE('',#126988,#9037);
#7193=LINE('',#126990,#9038);
#7194=LINE('',#126992,#9039);
#7195=LINE('',#126993,#9040);
#7196=LINE('',#126995,#9041);
#7197=LINE('',#126999,#9042);
#7198=LINE('',#127002,#9043);
#7199=LINE('',#127005,#9044);
#7200=LINE('',#127006,#9045);
#7201=LINE('',#127008,#9046);
#7202=LINE('',#127010,#9047);
#7203=LINE('',#127013,#9048);
#7204=LINE('',#127016,#9049);
#7205=LINE('',#127018,#9050);
#7206=LINE('',#127021,#9051);
#7207=LINE('',#127022,#9052);
#7208=LINE('',#127024,#9053);
#7209=LINE('',#127026,#9054);
#7210=LINE('',#127029,#9055);
#7211=LINE('',#127032,#9056);
#7212=LINE('',#127034,#9057);
#7213=LINE('',#127037,#9058);
#7214=LINE('',#127038,#9059);
#7215=LINE('',#127040,#9060);
#7216=LINE('',#127042,#9061);
#7217=LINE('',#127045,#9062);
#7218=LINE('',#127048,#9063);
#7219=LINE('',#127050,#9064);
#7220=LINE('',#127053,#9065);
#7221=LINE('',#127054,#9066);
#7222=LINE('',#127056,#9067);
#7223=LINE('',#127058,#9068);
#7224=LINE('',#127061,#9069);
#7225=LINE('',#127064,#9070);
#7226=LINE('',#127066,#9071);
#7227=LINE('',#127069,#9072);
#7228=LINE('',#127070,#9073);
#7229=LINE('',#127072,#9074);
#7230=LINE('',#127074,#9075);
#7231=LINE('',#127077,#9076);
#7232=LINE('',#127080,#9077);
#7233=LINE('',#127082,#9078);
#7234=LINE('',#127085,#9079);
#7235=LINE('',#127086,#9080);
#7236=LINE('',#127088,#9081);
#7237=LINE('',#127090,#9082);
#7238=LINE('',#127095,#9083);
#7239=LINE('',#127101,#9084);
#7240=LINE('',#127107,#9085);
#7241=LINE('',#127112,#9086);
#7242=LINE('',#127114,#9087);
#7243=LINE('',#127116,#9088);
#7244=LINE('',#127117,#9089);
#7245=LINE('',#127120,#9090);
#7246=LINE('',#127122,#9091);
#7247=LINE('',#127123,#9092);
#7248=LINE('',#127128,#9093);
#7249=LINE('',#127132,#9094);
#7250=LINE('',#127134,#9095);
#7251=LINE('',#127135,#9096);
#7252=LINE('',#127137,#9097);
#7253=LINE('',#127141,#9098);
#7254=LINE('',#127143,#9099);
#7255=LINE('',#127145,#9100);
#7256=LINE('',#127147,#9101);
#7257=LINE('',#127149,#9102);
#7258=LINE('',#127151,#9103);
#7259=LINE('',#127153,#9104);
#7260=LINE('',#127155,#9105);
#7261=LINE('',#127157,#9106);
#7262=LINE('',#127159,#9107);
#7263=LINE('',#127163,#9108);
#7264=LINE('',#127165,#9109);
#7265=LINE('',#127166,#9110);
#7266=LINE('',#127171,#9111);
#7267=LINE('',#127175,#9112);
#7268=LINE('',#127177,#9113);
#7269=LINE('',#127178,#9114);
#7270=LINE('',#127183,#9115);
#7271=LINE('',#127187,#9116);
#7272=LINE('',#127189,#9117);
#7273=LINE('',#127190,#9118);
#7274=LINE('',#127195,#9119);
#7275=LINE('',#127199,#9120);
#7276=LINE('',#127201,#9121);
#7277=LINE('',#127202,#9122);
#7278=LINE('',#127207,#9123);
#7279=LINE('',#127211,#9124);
#7280=LINE('',#127213,#9125);
#7281=LINE('',#127214,#9126);
#7282=LINE('',#127219,#9127);
#7283=LINE('',#127223,#9128);
#7284=LINE('',#127225,#9129);
#7285=LINE('',#127226,#9130);
#7286=LINE('',#127231,#9131);
#7287=LINE('',#127235,#9132);
#7288=LINE('',#127237,#9133);
#7289=LINE('',#127238,#9134);
#7290=LINE('',#127241,#9135);
#7291=LINE('',#127243,#9136);
#7292=LINE('',#127244,#9137);
#7293=LINE('',#127247,#9138);
#7294=LINE('',#127249,#9139);
#7295=LINE('',#127250,#9140);
#7296=LINE('',#127255,#9141);
#7297=LINE('',#127259,#9142);
#7298=LINE('',#127261,#9143);
#7299=LINE('',#127262,#9144);
#7300=LINE('',#127265,#9145);
#7301=LINE('',#127267,#9146);
#7302=LINE('',#127268,#9147);
#7303=LINE('',#127270,#9148);
#7304=LINE('',#127271,#9149);
#7305=LINE('',#127274,#9150);
#7306=LINE('',#127276,#9151);
#7307=LINE('',#127277,#9152);
#7308=LINE('',#127283,#9153);
#7309=LINE('',#127286,#9154);
#7310=LINE('',#127288,#9155);
#7311=LINE('',#127289,#9156);
#7312=LINE('',#127292,#9157);
#7313=LINE('',#127297,#9158);
#7314=LINE('',#127298,#9159);
#7315=LINE('',#127301,#9160);
#7316=LINE('',#127305,#9161);
#7317=LINE('',#127306,#9162);
#7318=LINE('',#127309,#9163);
#7319=LINE('',#127313,#9164);
#7320=LINE('',#127314,#9165);
#7321=LINE('',#127317,#9166);
#7322=LINE('',#127321,#9167);
#7323=LINE('',#127322,#9168);
#7324=LINE('',#127325,#9169);
#7325=LINE('',#127329,#9170);
#7326=LINE('',#127330,#9171);
#7327=LINE('',#127333,#9172);
#7328=LINE('',#127336,#9173);
#7329=LINE('',#127339,#9174);
#7330=LINE('',#127341,#9175);
#7331=LINE('',#127342,#9176);
#7332=LINE('',#127348,#9177);
#7333=LINE('',#127351,#9178);
#7334=LINE('',#127353,#9179);
#7335=LINE('',#127354,#9180);
#7336=LINE('',#127360,#9181);
#7337=LINE('',#127363,#9182);
#7338=LINE('',#127365,#9183);
#7339=LINE('',#127366,#9184);
#7340=LINE('',#127372,#9185);
#7341=LINE('',#127375,#9186);
#7342=LINE('',#127377,#9187);
#7343=LINE('',#127378,#9188);
#7344=LINE('',#127384,#9189);
#7345=LINE('',#127387,#9190);
#7346=LINE('',#127389,#9191);
#7347=LINE('',#127390,#9192);
#7348=LINE('',#127396,#9193);
#7349=LINE('',#127399,#9194);
#7350=LINE('',#127401,#9195);
#7351=LINE('',#127402,#9196);
#7352=LINE('',#127408,#9197);
#7353=LINE('',#127411,#9198);
#7354=LINE('',#127413,#9199);
#7355=LINE('',#127414,#9200);
#7356=LINE('',#127417,#9201);
#7357=LINE('',#127419,#9202);
#7358=LINE('',#127420,#9203);
#7359=LINE('',#127423,#9204);
#7360=LINE('',#127425,#9205);
#7361=LINE('',#127426,#9206);
#7362=LINE('',#127432,#9207);
#7363=LINE('',#127435,#9208);
#7364=LINE('',#127437,#9209);
#7365=LINE('',#127438,#9210);
#7366=LINE('',#127441,#9211);
#7367=LINE('',#127443,#9212);
#7368=LINE('',#127444,#9213);
#7369=LINE('',#127446,#9214);
#7370=LINE('',#127447,#9215);
#7371=LINE('',#127456,#9216);
#7372=LINE('',#127458,#9217);
#7373=LINE('',#127463,#9218);
#7374=LINE('',#127466,#9219);
#7375=LINE('',#127470,#9220);
#7376=LINE('',#127474,#9221);
#7377=LINE('',#127476,#9222);
#7378=LINE('',#127478,#9223);
#7379=LINE('',#127479,#9224);
#7380=LINE('',#127485,#9225);
#7381=LINE('',#127487,#9226);
#7382=LINE('',#127489,#9227);
#7383=LINE('',#127494,#9228);
#7384=LINE('',#127498,#9229);
#7385=LINE('',#127500,#9230);
#7386=LINE('',#127502,#9231);
#7387=LINE('',#127506,#9232);
#7388=LINE('',#127508,#9233);
#7389=LINE('',#127514,#9234);
#7390=LINE('',#127515,#9235);
#7391=LINE('',#127518,#9236);
#7392=LINE('',#127519,#9237);
#7393=LINE('',#127522,#9238);
#7394=LINE('',#127526,#9239);
#7395=LINE('',#127528,#9240);
#7396=LINE('',#127530,#9241);
#7397=LINE('',#127533,#9242);
#7398=LINE('',#127539,#9243);
#7399=LINE('',#127543,#9244);
#7400=LINE('',#127547,#9245);
#7401=LINE('',#127551,#9246);
#7402=LINE('',#127555,#9247);
#7403=LINE('',#127558,#9248);
#7404=LINE('',#127560,#9249);
#7405=LINE('',#127562,#9250);
#7406=LINE('',#127563,#9251);
#7407=LINE('',#127566,#9252);
#7408=LINE('',#127568,#9253);
#7409=LINE('',#127570,#9254);
#7410=LINE('',#127571,#9255);
#7411=LINE('',#127573,#9256);
#7412=LINE('',#127575,#9257);
#7413=LINE('',#127577,#9258);
#7414=LINE('',#127579,#9259);
#7415=LINE('',#127580,#9260);
#7416=LINE('',#127582,#9261);
#7417=LINE('',#127583,#9262);
#7418=LINE('',#127586,#9263);
#7419=LINE('',#127588,#9264);
#7420=LINE('',#127589,#9265);
#7421=LINE('',#127592,#9266);
#7422=LINE('',#127593,#9267);
#7423=LINE('',#127596,#9268);
#7424=LINE('',#127597,#9269);
#7425=LINE('',#127599,#9270);
#7426=LINE('',#127604,#9271);
#7427=LINE('',#127608,#9272);
#7428=LINE('',#127611,#9273);
#7429=LINE('',#127615,#9274);
#7430=LINE('',#127617,#9275);
#7431=LINE('',#127621,#9276);
#7432=LINE('',#127624,#9277);
#7433=LINE('',#127625,#9278);
#7434=LINE('',#127627,#9279);
#7435=LINE('',#127629,#9280);
#7436=LINE('',#127633,#9281);
#7437=LINE('',#127634,#9282);
#7438=LINE('',#127636,#9283);
#7439=LINE('',#127638,#9284);
#7440=LINE('',#127642,#9285);
#7441=LINE('',#127645,#9286);
#7442=LINE('',#127649,#9287);
#7443=LINE('',#127651,#9288);
#7444=LINE('',#127656,#9289);
#7445=LINE('',#127659,#9290);
#7446=LINE('',#127661,#9291);
#7447=LINE('',#127662,#9292);
#7448=LINE('',#127663,#9293);
#7449=LINE('',#127667,#9294);
#7450=LINE('',#127669,#9295);
#7451=LINE('',#127671,#9296);
#7452=LINE('',#127672,#9297);
#7453=LINE('',#127679,#9298);
#7454=LINE('',#127681,#9299);
#7455=LINE('',#127685,#9300);
#7456=LINE('',#127687,#9301);
#7457=LINE('',#127689,#9302);
#7458=LINE('',#127692,#9303);
#7459=LINE('',#127698,#9304);
#7460=LINE('',#127699,#9305);
#7461=LINE('',#127701,#9306);
#7462=LINE('',#127702,#9307);
#7463=LINE('',#127703,#9308);
#7464=LINE('',#127708,#9309);
#7465=LINE('',#127709,#9310);
#7466=LINE('',#127712,#9311);
#7467=LINE('',#127713,#9312);
#7468=LINE('',#127718,#9313);
#7469=LINE('',#127722,#9314);
#7470=LINE('',#127726,#9315);
#7471=LINE('',#127730,#9316);
#7472=LINE('',#127734,#9317);
#7473=LINE('',#127739,#9318);
#7474=LINE('',#127743,#9319);
#7475=LINE('',#127745,#9320);
#7476=LINE('',#127747,#9321);
#7477=LINE('',#127750,#9322);
#7478=LINE('',#127753,#9323);
#7479=LINE('',#127754,#9324);
#7480=LINE('',#127755,#9325);
#7481=LINE('',#127757,#9326);
#7482=LINE('',#127759,#9327);
#7483=LINE('',#127761,#9328);
#7484=LINE('',#127762,#9329);
#7485=LINE('',#127765,#9330);
#7486=LINE('',#127767,#9331);
#7487=LINE('',#127769,#9332);
#7488=LINE('',#127770,#9333);
#7489=LINE('',#127772,#9334);
#7490=LINE('',#127774,#9335);
#7491=LINE('',#127776,#9336);
#7492=LINE('',#127779,#9337);
#7493=LINE('',#127782,#9338);
#7494=LINE('',#127784,#9339);
#7495=LINE('',#127785,#9340);
#7496=LINE('',#127788,#9341);
#7497=LINE('',#127789,#9342);
#7498=LINE('',#127792,#9343);
#7499=LINE('',#127793,#9344);
#7500=LINE('',#127795,#9345);
#7501=LINE('',#127800,#9346);
#7502=LINE('',#127801,#9347);
#7503=LINE('',#127805,#9348);
#7504=LINE('',#127806,#9349);
#7505=LINE('',#127807,#9350);
#7506=LINE('',#127810,#9351);
#7507=LINE('',#127814,#9352);
#7508=LINE('',#127820,#9353);
#7509=LINE('',#127823,#9354);
#7510=LINE('',#127825,#9355);
#7511=LINE('',#127827,#9356);
#7512=LINE('',#127828,#9357);
#7513=LINE('',#127830,#9358);
#7514=LINE('',#127832,#9359);
#7515=LINE('',#127837,#9360);
#7516=LINE('',#127839,#9361);
#7517=LINE('',#127846,#9362);
#7518=LINE('',#127853,#9363);
#7519=LINE('',#127856,#9364);
#7520=LINE('',#127859,#9365);
#7521=LINE('',#127861,#9366);
#7522=LINE('',#127862,#9367);
#7523=LINE('',#127865,#9368);
#7524=LINE('',#127867,#9369);
#7525=LINE('',#127868,#9370);
#7526=LINE('',#127871,#9371);
#7527=LINE('',#127873,#9372);
#7528=LINE('',#127874,#9373);
#7529=LINE('',#127877,#9374);
#7530=LINE('',#127879,#9375);
#7531=LINE('',#127880,#9376);
#7532=LINE('',#127883,#9377);
#7533=LINE('',#127885,#9378);
#7534=LINE('',#127886,#9379);
#7535=LINE('',#127892,#9380);
#7536=LINE('',#127895,#9381);
#7537=LINE('',#127897,#9382);
#7538=LINE('',#127898,#9383);
#7539=LINE('',#127901,#9384);
#7540=LINE('',#127903,#9385);
#7541=LINE('',#127904,#9386);
#7542=LINE('',#127910,#9387);
#7543=LINE('',#127916,#9388);
#7544=LINE('',#127922,#9389);
#7545=LINE('',#127925,#9390);
#7546=LINE('',#127927,#9391);
#7547=LINE('',#127928,#9392);
#7548=LINE('',#127931,#9393);
#7549=LINE('',#127933,#9394);
#7550=LINE('',#127934,#9395);
#7551=LINE('',#127937,#9396);
#7552=LINE('',#127939,#9397);
#7553=LINE('',#127940,#9398);
#7554=LINE('',#127946,#9399);
#7555=LINE('',#127949,#9400);
#7556=LINE('',#127951,#9401);
#7557=LINE('',#127952,#9402);
#7558=LINE('',#127958,#9403);
#7559=LINE('',#127961,#9404);
#7560=LINE('',#127963,#9405);
#7561=LINE('',#127964,#9406);
#7562=LINE('',#127970,#9407);
#7563=LINE('',#127973,#9408);
#7564=LINE('',#127975,#9409);
#7565=LINE('',#127976,#9410);
#7566=LINE('',#127979,#9411);
#7567=LINE('',#127981,#9412);
#7568=LINE('',#127982,#9413);
#7569=LINE('',#127985,#9414);
#7570=LINE('',#127987,#9415);
#7571=LINE('',#127988,#9416);
#7572=LINE('',#127994,#9417);
#7573=LINE('',#127997,#9418);
#7574=LINE('',#127999,#9419);
#7575=LINE('',#128000,#9420);
#7576=LINE('',#128006,#9421);
#7577=LINE('',#128009,#9422);
#7578=LINE('',#128011,#9423);
#7579=LINE('',#128012,#9424);
#7580=LINE('',#128018,#9425);
#7581=LINE('',#128021,#9426);
#7582=LINE('',#128023,#9427);
#7583=LINE('',#128024,#9428);
#7584=LINE('',#128030,#9429);
#7585=LINE('',#128033,#9430);
#7586=LINE('',#128035,#9431);
#7587=LINE('',#128036,#9432);
#7588=LINE('',#128039,#9433);
#7589=LINE('',#128041,#9434);
#7590=LINE('',#128042,#9435);
#7591=LINE('',#128045,#9436);
#7592=LINE('',#128047,#9437);
#7593=LINE('',#128048,#9438);
#7594=LINE('',#128054,#9439);
#7595=LINE('',#128057,#9440);
#7596=LINE('',#128059,#9441);
#7597=LINE('',#128060,#9442);
#7598=LINE('',#128066,#9443);
#7599=LINE('',#128069,#9444);
#7600=LINE('',#128071,#9445);
#7601=LINE('',#128072,#9446);
#7602=LINE('',#128078,#9447);
#7603=LINE('',#128081,#9448);
#7604=LINE('',#128083,#9449);
#7605=LINE('',#128084,#9450);
#7606=LINE('',#128087,#9451);
#7607=LINE('',#128089,#9452);
#7608=LINE('',#128090,#9453);
#7609=LINE('',#128093,#9454);
#7610=LINE('',#128095,#9455);
#7611=LINE('',#128096,#9456);
#7612=LINE('',#128102,#9457);
#7613=LINE('',#128108,#9458);
#7614=LINE('',#128114,#9459);
#7615=LINE('',#128117,#9460);
#7616=LINE('',#128119,#9461);
#7617=LINE('',#128120,#9462);
#7618=LINE('',#128123,#9463);
#7619=LINE('',#128125,#9464);
#7620=LINE('',#128126,#9465);
#7621=LINE('',#128132,#9466);
#7622=LINE('',#128135,#9467);
#7623=LINE('',#128137,#9468);
#7624=LINE('',#128138,#9469);
#7625=LINE('',#128141,#9470);
#7626=LINE('',#128143,#9471);
#7627=LINE('',#128144,#9472);
#7628=LINE('',#128147,#9473);
#7629=LINE('',#128149,#9474);
#7630=LINE('',#128150,#9475);
#7631=LINE('',#128153,#9476);
#7632=LINE('',#128155,#9477);
#7633=LINE('',#128156,#9478);
#7634=LINE('',#128159,#9479);
#7635=LINE('',#128161,#9480);
#7636=LINE('',#128162,#9481);
#7637=LINE('',#128168,#9482);
#7638=LINE('',#128171,#9483);
#7639=LINE('',#128173,#9484);
#7640=LINE('',#128174,#9485);
#7641=LINE('',#128177,#9486);
#7642=LINE('',#128179,#9487);
#7643=LINE('',#128180,#9488);
#7644=LINE('',#128186,#9489);
#7645=LINE('',#128192,#9490);
#7646=LINE('',#128198,#9491);
#7647=LINE('',#128201,#9492);
#7648=LINE('',#128203,#9493);
#7649=LINE('',#128204,#9494);
#7650=LINE('',#128207,#9495);
#7651=LINE('',#128209,#9496);
#7652=LINE('',#128210,#9497);
#7653=LINE('',#128213,#9498);
#7654=LINE('',#128215,#9499);
#7655=LINE('',#128216,#9500);
#7656=LINE('',#128222,#9501);
#7657=LINE('',#128225,#9502);
#7658=LINE('',#128227,#9503);
#7659=LINE('',#128228,#9504);
#7660=LINE('',#128234,#9505);
#7661=LINE('',#128237,#9506);
#7662=LINE('',#128239,#9507);
#7663=LINE('',#128240,#9508);
#7664=LINE('',#128246,#9509);
#7665=LINE('',#128249,#9510);
#7666=LINE('',#128251,#9511);
#7667=LINE('',#128252,#9512);
#7668=LINE('',#128255,#9513);
#7669=LINE('',#128257,#9514);
#7670=LINE('',#128258,#9515);
#7671=LINE('',#128261,#9516);
#7672=LINE('',#128263,#9517);
#7673=LINE('',#128264,#9518);
#7674=LINE('',#128270,#9519);
#7675=LINE('',#128273,#9520);
#7676=LINE('',#128275,#9521);
#7677=LINE('',#128276,#9522);
#7678=LINE('',#128282,#9523);
#7679=LINE('',#128285,#9524);
#7680=LINE('',#128287,#9525);
#7681=LINE('',#128288,#9526);
#7682=LINE('',#128294,#9527);
#7683=LINE('',#128297,#9528);
#7684=LINE('',#128299,#9529);
#7685=LINE('',#128300,#9530);
#7686=LINE('',#128306,#9531);
#7687=LINE('',#128309,#9532);
#7688=LINE('',#128311,#9533);
#7689=LINE('',#128312,#9534);
#7690=LINE('',#128315,#9535);
#7691=LINE('',#128317,#9536);
#7692=LINE('',#128318,#9537);
#7693=LINE('',#128321,#9538);
#7694=LINE('',#128323,#9539);
#7695=LINE('',#128324,#9540);
#7696=LINE('',#128330,#9541);
#7697=LINE('',#128333,#9542);
#7698=LINE('',#128335,#9543);
#7699=LINE('',#128336,#9544);
#7700=LINE('',#128342,#9545);
#7701=LINE('',#128345,#9546);
#7702=LINE('',#128347,#9547);
#7703=LINE('',#128348,#9548);
#7704=LINE('',#128354,#9549);
#7705=LINE('',#128357,#9550);
#7706=LINE('',#128359,#9551);
#7707=LINE('',#128360,#9552);
#7708=LINE('',#128363,#9553);
#7709=LINE('',#128365,#9554);
#7710=LINE('',#128366,#9555);
#7711=LINE('',#128369,#9556);
#7712=LINE('',#128371,#9557);
#7713=LINE('',#128372,#9558);
#7714=LINE('',#128378,#9559);
#7715=LINE('',#128384,#9560);
#7716=LINE('',#128390,#9561);
#7717=LINE('',#128393,#9562);
#7718=LINE('',#128395,#9563);
#7719=LINE('',#128396,#9564);
#7720=LINE('',#128398,#9565);
#7721=LINE('',#128399,#9566);
#7722=LINE('',#128406,#9567);
#7723=LINE('',#128445,#9568);
#7724=LINE('',#128705,#9569);
#7725=LINE('',#129149,#9570);
#7726=LINE('',#129445,#9571);
#7727=LINE('',#129484,#9572);
#7728=LINE('',#129744,#9573);
#7729=LINE('',#130188,#9574);
#7730=LINE('',#130484,#9575);
#7731=LINE('',#130572,#9576);
#7732=LINE('',#130723,#9577);
#7733=LINE('',#131056,#9578);
#7734=LINE('',#131337,#9579);
#7735=LINE('',#131673,#9580);
#7736=LINE('',#131835,#9581);
#7737=LINE('',#132105,#9582);
#7738=LINE('',#132380,#9583);
#7739=LINE('',#132714,#9584);
#7740=LINE('',#132876,#9585);
#7741=LINE('',#133143,#9586);
#7742=LINE('',#133421,#9587);
#7743=LINE('',#133754,#9588);
#7744=LINE('',#133919,#9589);
#7745=LINE('',#134188,#9590);
#7746=LINE('',#134469,#9591);
#7747=LINE('',#134802,#9592);
#7748=LINE('',#134961,#9593);
#7749=LINE('',#135231,#9594);
#7750=LINE('',#135512,#9595);
#7751=LINE('',#135843,#9596);
#7752=LINE('',#136006,#9597);
#7753=LINE('',#136272,#9598);
#7754=LINE('',#136553,#9599);
#7755=LINE('',#136886,#9600);
#7756=LINE('',#137167,#9601);
#7757=LINE('',#137265,#9602);
#7758=LINE('',#137353,#9603);
#7759=LINE('',#137504,#9604);
#7760=LINE('',#137837,#9605);
#7761=LINE('',#138118,#9606);
#7762=LINE('',#138454,#9607);
#7763=LINE('',#138616,#9608);
#7764=LINE('',#138886,#9609);
#7765=LINE('',#139161,#9610);
#7766=LINE('',#139495,#9611);
#7767=LINE('',#139657,#9612);
#7768=LINE('',#139924,#9613);
#7769=LINE('',#140202,#9614);
#7770=LINE('',#140535,#9615);
#7771=LINE('',#140700,#9616);
#7772=LINE('',#140969,#9617);
#7773=LINE('',#141250,#9618);
#7774=LINE('',#141583,#9619);
#7775=LINE('',#141742,#9620);
#7776=LINE('',#142012,#9621);
#7777=LINE('',#142293,#9622);
#7778=LINE('',#142624,#9623);
#7779=LINE('',#142787,#9624);
#7780=LINE('',#143053,#9625);
#7781=LINE('',#143334,#9626);
#7782=LINE('',#143667,#9627);
#7783=LINE('',#143948,#9628);
#7784=LINE('',#144046,#9629);
#7785=LINE('',#144134,#9630);
#7786=LINE('',#144285,#9631);
#7787=LINE('',#144618,#9632);
#7788=LINE('',#144899,#9633);
#7789=LINE('',#145235,#9634);
#7790=LINE('',#145397,#9635);
#7791=LINE('',#145667,#9636);
#7792=LINE('',#145942,#9637);
#7793=LINE('',#146276,#9638);
#7794=LINE('',#146438,#9639);
#7795=LINE('',#146705,#9640);
#7796=LINE('',#146983,#9641);
#7797=LINE('',#147316,#9642);
#7798=LINE('',#147481,#9643);
#7799=LINE('',#147750,#9644);
#7800=LINE('',#148031,#9645);
#7801=LINE('',#148364,#9646);
#7802=LINE('',#148523,#9647);
#7803=LINE('',#148793,#9648);
#7804=LINE('',#149074,#9649);
#7805=LINE('',#149405,#9650);
#7806=LINE('',#149568,#9651);
#7807=LINE('',#149834,#9652);
#7808=LINE('',#150115,#9653);
#7809=LINE('',#150448,#9654);
#7810=LINE('',#150729,#9655);
#7811=LINE('',#150827,#9656);
#7812=LINE('',#150915,#9657);
#7813=LINE('',#151066,#9658);
#7814=LINE('',#151399,#9659);
#7815=LINE('',#151680,#9660);
#7816=LINE('',#152016,#9661);
#7817=LINE('',#152178,#9662);
#7818=LINE('',#152448,#9663);
#7819=LINE('',#152723,#9664);
#7820=LINE('',#153057,#9665);
#7821=LINE('',#153219,#9666);
#7822=LINE('',#153486,#9667);
#7823=LINE('',#153764,#9668);
#7824=LINE('',#154097,#9669);
#7825=LINE('',#154262,#9670);
#7826=LINE('',#154531,#9671);
#7827=LINE('',#154812,#9672);
#7828=LINE('',#155145,#9673);
#7829=LINE('',#155304,#9674);
#7830=LINE('',#155574,#9675);
#7831=LINE('',#155855,#9676);
#7832=LINE('',#156186,#9677);
#7833=LINE('',#156349,#9678);
#7834=LINE('',#156615,#9679);
#7835=LINE('',#156896,#9680);
#7836=LINE('',#157229,#9681);
#7837=LINE('',#157510,#9682);
#7838=LINE('',#157608,#9683);
#7839=LINE('',#157630,#9684);
#7840=LINE('',#157742,#9685);
#7841=LINE('',#158030,#9686);
#7842=LINE('',#158316,#9687);
#7843=LINE('',#158372,#9688);
#7844=LINE('',#158658,#9689);
#7845=LINE('',#158948,#9690);
#7846=LINE('',#159060,#9691);
#7847=LINE('',#159392,#9692);
#7848=LINE('',#159828,#9693);
#7849=LINE('',#160287,#9694);
#7850=LINE('',#160589,#9695);
#7851=LINE('',#161061,#9696);
#7852=LINE('',#161551,#9697);
#7853=LINE('',#162069,#9698);
#7854=LINE('',#162548,#9699);
#7855=LINE('',#162967,#9700);
#7856=LINE('',#163235,#9701);
#7857=LINE('',#163693,#9702);
#7858=LINE('',#164156,#9703);
#7859=LINE('',#164456,#9704);
#7860=LINE('',#164897,#9705);
#7861=LINE('',#165320,#9706);
#7862=LINE('',#165618,#9707);
#7863=LINE('',#166082,#9708);
#7864=LINE('',#166550,#9709);
#7865=LINE('',#166793,#9710);
#7866=LINE('',#167225,#9711);
#7867=LINE('',#167693,#9712);
#7868=LINE('',#168203,#9713);
#7869=LINE('',#168673,#9714);
#7870=LINE('',#169139,#9715);
#7871=LINE('',#169438,#9716);
#7872=LINE('',#169916,#9717);
#7873=LINE('',#170351,#9718);
#7874=LINE('',#170683,#9719);
#7875=LINE('',#171119,#9720);
#7876=LINE('',#171574,#9721);
#7877=LINE('',#171878,#9722);
#7878=LINE('',#172350,#9723);
#7879=LINE('',#172832,#9724);
#7880=LINE('',#173338,#9725);
#7881=LINE('',#173819,#9726);
#7882=LINE('',#174284,#9727);
#7883=LINE('',#174552,#9728);
#7884=LINE('',#175010,#9729);
#7885=LINE('',#175473,#9730);
#7886=LINE('',#175773,#9731);
#7887=LINE('',#176224,#9732);
#7888=LINE('',#176649,#9733);
#7889=LINE('',#176935,#9734);
#7890=LINE('',#177403,#9735);
#7891=LINE('',#177871,#9736);
#7892=LINE('',#178114,#9737);
#7893=LINE('',#178546,#9738);
#7894=LINE('',#179016,#9739);
#7895=LINE('',#179546,#9740);
#7896=LINE('',#180016,#9741);
#7897=LINE('',#180480,#9742);
#7898=LINE('',#180749,#9743);
#7899=LINE('',#181227,#9744);
#7900=LINE('',#181662,#9745);
#7901=LINE('',#181994,#9746);
#7902=LINE('',#182430,#9747);
#7903=LINE('',#182889,#9748);
#7904=LINE('',#183191,#9749);
#7905=LINE('',#183651,#9750);
#7906=LINE('',#184133,#9751);
#7907=LINE('',#184643,#9752);
#7908=LINE('',#185114,#9753);
#7909=LINE('',#185537,#9754);
#7910=LINE('',#185805,#9755);
#7911=LINE('',#186265,#9756);
#7912=LINE('',#186728,#9757);
#7913=LINE('',#187052,#9758);
#7914=LINE('',#187537,#9759);
#7915=LINE('',#187998,#9760);
#7916=LINE('',#188298,#9761);
#7917=LINE('',#188762,#9762);
#7918=LINE('',#189230,#9763);
#7919=LINE('',#189473,#9764);
#7920=LINE('',#189905,#9765);
#7921=LINE('',#190381,#9766);
#7922=LINE('',#190891,#9767);
#7923=LINE('',#191365,#9768);
#7924=LINE('',#191823,#9769);
#7925=LINE('',#192078,#9770);
#7926=LINE('',#192558,#9771);
#7927=LINE('',#192993,#9772);
#7928=LINE('',#193325,#9773);
#7929=LINE('',#193761,#9774);
#7930=LINE('',#194218,#9775);
#7931=LINE('',#194522,#9776);
#7932=LINE('',#194984,#9777);
#7933=LINE('',#195462,#9778);
#7934=LINE('',#195954,#9779);
#7935=LINE('',#196425,#9780);
#7936=LINE('',#196894,#9781);
#7937=LINE('',#197162,#9782);
#7938=LINE('',#197628,#9783);
#7939=LINE('',#198093,#9784);
#7940=LINE('',#198391,#9785);
#7941=LINE('',#198842,#9786);
#7942=LINE('',#199267,#9787);
#7943=LINE('',#199561,#9788);
#7944=LINE('',#200027,#9789);
#7945=LINE('',#200495,#9790);
#7946=LINE('',#200738,#9791);
#7947=LINE('',#201216,#9792);
#7948=LINE('',#201694,#9793);
#7949=LINE('',#202222,#9794);
#7950=LINE('',#202696,#9795);
#7951=LINE('',#203142,#9796);
#7952=LINE('',#203439,#9797);
#7953=LINE('',#203915,#9798);
#7954=LINE('',#206271,#9799);
#7955=LINE('',#206279,#9800);
#7956=LINE('',#206282,#9801);
#7957=LINE('',#206285,#9802);
#7958=LINE('',#206289,#9803);
#7959=LINE('',#206290,#9804);
#7960=LINE('',#206295,#9805);
#7961=LINE('',#206303,#9806);
#7962=LINE('',#206306,#9807);
#7963=LINE('',#206310,#9808);
#7964=LINE('',#206313,#9809);
#7965=LINE('',#206314,#9810);
#7966=LINE('',#206319,#9811);
#7967=LINE('',#206324,#9812);
#7968=LINE('',#206326,#9813);
#7969=LINE('',#206327,#9814);
#7970=LINE('',#206330,#9815);
#7971=LINE('',#206332,#9816);
#7972=LINE('',#206334,#9817);
#7973=LINE('',#206335,#9818);
#7974=LINE('',#206338,#9819);
#7975=LINE('',#206339,#9820);
#7976=LINE('',#206340,#9821);
#7977=LINE('',#206345,#9822);
#7978=LINE('',#206349,#9823);
#7979=LINE('',#206353,#9824);
#7980=LINE('',#206357,#9825);
#7981=LINE('',#206359,#9826);
#7982=LINE('',#206361,#9827);
#7983=LINE('',#206363,#9828);
#7984=LINE('',#206365,#9829);
#7985=LINE('',#206369,#9830);
#7986=LINE('',#206373,#9831);
#7987=LINE('',#206375,#9832);
#7988=LINE('',#206377,#9833);
#7989=LINE('',#206379,#9834);
#7990=LINE('',#206381,#9835);
#7991=LINE('',#206385,#9836);
#7992=LINE('',#206389,#9837);
#7993=LINE('',#206393,#9838);
#7994=LINE('',#206396,#9839);
#7995=LINE('',#215199,#9840);
#7996=LINE('',#215201,#9841);
#7997=LINE('',#215203,#9842);
#7998=LINE('',#215204,#9843);
#7999=LINE('',#215207,#9844);
#8000=LINE('',#215209,#9845);
#8001=LINE('',#215210,#9846);
#8002=LINE('',#215213,#9847);
#8003=LINE('',#215215,#9848);
#8004=LINE('',#215216,#9849);
#8005=LINE('',#215219,#9850);
#8006=LINE('',#215221,#9851);
#8007=LINE('',#215222,#9852);
#8008=LINE('',#215225,#9853);
#8009=LINE('',#215227,#9854);
#8010=LINE('',#215228,#9855);
#8011=LINE('',#215231,#9856);
#8012=LINE('',#215233,#9857);
#8013=LINE('',#215234,#9858);
#8014=LINE('',#215236,#9859);
#8015=LINE('',#215237,#9860);
#8016=LINE('',#215242,#9861);
#8017=LINE('',#215250,#9862);
#8018=LINE('',#215253,#9863);
#8019=LINE('',#215256,#9864);
#8020=LINE('',#215258,#9865);
#8021=LINE('',#215259,#9866);
#8022=LINE('',#215264,#9867);
#8023=LINE('',#215267,#9868);
#8024=LINE('',#215268,#9869);
#8025=LINE('',#215270,#9870);
#8026=LINE('',#215271,#9871);
#8027=LINE('',#215280,#9872);
#8028=LINE('',#215282,#9873);
#8029=LINE('',#215284,#9874);
#8030=LINE('',#215285,#9875);
#8031=LINE('',#215288,#9876);
#8032=LINE('',#215290,#9877);
#8033=LINE('',#215291,#9878);
#8034=LINE('',#215294,#9879);
#8035=LINE('',#215296,#9880);
#8036=LINE('',#215297,#9881);
#8037=LINE('',#215300,#9882);
#8038=LINE('',#215302,#9883);
#8039=LINE('',#215303,#9884);
#8040=LINE('',#215306,#9885);
#8041=LINE('',#215308,#9886);
#8042=LINE('',#215309,#9887);
#8043=LINE('',#215312,#9888);
#8044=LINE('',#215314,#9889);
#8045=LINE('',#215315,#9890);
#8046=LINE('',#215317,#9891);
#8047=LINE('',#215318,#9892);
#8048=LINE('',#215323,#9893);
#8049=LINE('',#215330,#9894);
#8050=LINE('',#215336,#9895);
#8051=LINE('',#215344,#9896);
#8052=LINE('',#215347,#9897);
#8053=LINE('',#215350,#9898);
#8054=LINE('',#215352,#9899);
#8055=LINE('',#215353,#9900);
#8056=LINE('',#215359,#9901);
#8057=LINE('',#215361,#9902);
#8058=LINE('',#215362,#9903);
#8059=LINE('',#215364,#9904);
#8060=LINE('',#215365,#9905);
#8061=LINE('',#215374,#9906);
#8062=LINE('',#215376,#9907);
#8063=LINE('',#215378,#9908);
#8064=LINE('',#215379,#9909);
#8065=LINE('',#215382,#9910);
#8066=LINE('',#215384,#9911);
#8067=LINE('',#215385,#9912);
#8068=LINE('',#215388,#9913);
#8069=LINE('',#215390,#9914);
#8070=LINE('',#215391,#9915);
#8071=LINE('',#215394,#9916);
#8072=LINE('',#215396,#9917);
#8073=LINE('',#215397,#9918);
#8074=LINE('',#215400,#9919);
#8075=LINE('',#215402,#9920);
#8076=LINE('',#215403,#9921);
#8077=LINE('',#215406,#9922);
#8078=LINE('',#215408,#9923);
#8079=LINE('',#215409,#9924);
#8080=LINE('',#215411,#9925);
#8081=LINE('',#215412,#9926);
#8082=LINE('',#215417,#9927);
#8083=LINE('',#215423,#9928);
#8084=LINE('',#215425,#9929);
#8085=LINE('',#215427,#9930);
#8086=LINE('',#215428,#9931);
#8087=LINE('',#215431,#9932);
#8088=LINE('',#215433,#9933);
#8089=LINE('',#215434,#9934);
#8090=LINE('',#215437,#9935);
#8091=LINE('',#215439,#9936);
#8092=LINE('',#215440,#9937);
#8093=LINE('',#215443,#9938);
#8094=LINE('',#215445,#9939);
#8095=LINE('',#215446,#9940);
#8096=LINE('',#215449,#9941);
#8097=LINE('',#215451,#9942);
#8098=LINE('',#215452,#9943);
#8099=LINE('',#215455,#9944);
#8100=LINE('',#215457,#9945);
#8101=LINE('',#215458,#9946);
#8102=LINE('',#215460,#9947);
#8103=LINE('',#215461,#9948);
#8104=LINE('',#215466,#9949);
#8105=LINE('',#215473,#9950);
#8106=LINE('',#215475,#9951);
#8107=LINE('',#215476,#9952);
#8108=LINE('',#215481,#9953);
#8109=LINE('',#215486,#9954);
#8110=LINE('',#215491,#9955);
#8111=LINE('',#215496,#9956);
#8112=LINE('',#215500,#9957);
#8113=LINE('',#215501,#9958);
#8114=LINE('',#215507,#9959);
#8115=LINE('',#215510,#9960);
#8116=LINE('',#215511,#9961);
#8117=LINE('',#215515,#9962);
#8118=LINE('',#215518,#9963);
#8119=LINE('',#215519,#9964);
#8120=LINE('',#215523,#9965);
#8121=LINE('',#215526,#9966);
#8122=LINE('',#215527,#9967);
#8123=LINE('',#215533,#9968);
#8124=LINE('',#215536,#9969);
#8125=LINE('',#215537,#9970);
#8126=LINE('',#215541,#9971);
#8127=LINE('',#215544,#9972);
#8128=LINE('',#215545,#9973);
#8129=LINE('',#215549,#9974);
#8130=LINE('',#215552,#9975);
#8131=LINE('',#215553,#9976);
#8132=LINE('',#215557,#9977);
#8133=LINE('',#215560,#9978);
#8134=LINE('',#215561,#9979);
#8135=LINE('',#215565,#9980);
#8136=LINE('',#215568,#9981);
#8137=LINE('',#215569,#9982);
#8138=LINE('',#215573,#9983);
#8139=LINE('',#215576,#9984);
#8140=LINE('',#215577,#9985);
#8141=VECTOR('',#30170,10.);
#8142=VECTOR('',#30171,10.);
#8143=VECTOR('',#30172,10.);
#8144=VECTOR('',#30175,10.);
#8145=VECTOR('',#30178,9.99999999999999);
#8146=VECTOR('',#30181,10.);
#8147=VECTOR('',#30184,10.);
#8148=VECTOR('',#30187,9.99999999999999);
#8149=VECTOR('',#30188,9.99999999999999);
#8150=VECTOR('',#30191,10.);
#8151=VECTOR('',#30194,10.);
#8152=VECTOR('',#30197,9.99999999999999);
#8153=VECTOR('',#30200,10.);
#8154=VECTOR('',#30203,10.);
#8155=VECTOR('',#30204,10.);
#8156=VECTOR('',#30207,10.);
#8157=VECTOR('',#30208,10.);
#8158=VECTOR('',#30209,10.);
#8159=VECTOR('',#30212,10.);
#8160=VECTOR('',#30213,10.);
#8161=VECTOR('',#30218,10.);
#8162=VECTOR('',#30221,10.);
#8163=VECTOR('',#30222,10.);
#8164=VECTOR('',#30227,10.);
#8165=VECTOR('',#30230,9.99999999999999);
#8166=VECTOR('',#30231,10.);
#8167=VECTOR('',#30236,10.);
#8168=VECTOR('',#30239,10.);
#8169=VECTOR('',#30240,10.);
#8170=VECTOR('',#30245,10.);
#8171=VECTOR('',#30248,10.);
#8172=VECTOR('',#30249,10.);
#8173=VECTOR('',#30254,10.);
#8174=VECTOR('',#30257,9.99999999999999);
#8175=VECTOR('',#30258,10.);
#8176=VECTOR('',#30261,9.99999999999999);
#8177=VECTOR('',#30262,10.);
#8178=VECTOR('',#30267,10.);
#8179=VECTOR('',#30270,10.);
#8180=VECTOR('',#30271,10.);
#8181=VECTOR('',#30276,10.);
#8182=VECTOR('',#30279,10.);
#8183=VECTOR('',#30280,10.);
#8184=VECTOR('',#30285,10.);
#8185=VECTOR('',#30288,9.99999999999999);
#8186=VECTOR('',#30289,10.);
#8187=VECTOR('',#30294,10.);
#8188=VECTOR('',#30297,10.);
#8189=VECTOR('',#30298,10.);
#8190=VECTOR('',#30303,10.);
#8191=VECTOR('',#30306,10.);
#8192=VECTOR('',#30307,10.);
#8193=VECTOR('',#30310,10.);
#8194=VECTOR('',#30311,10.);
#8195=VECTOR('',#30314,10.);
#8196=VECTOR('',#30321,10.);
#8197=VECTOR('',#30324,10.);
#8198=VECTOR('',#30327,10.);
#8199=VECTOR('',#30330,10.);
#8200=VECTOR('',#30331,10.);
#8201=VECTOR('',#30332,10.);
#8202=VECTOR('',#30333,10.);
#8203=VECTOR('',#30334,10.);
#8204=VECTOR('',#30335,10.);
#8205=VECTOR('',#30338,10.);
#8206=VECTOR('',#30341,10.);
#8207=VECTOR('',#30344,10.);
#8208=VECTOR('',#30347,10.);
#8209=VECTOR('',#30348,10.);
#8210=VECTOR('',#30349,10.);
#8211=VECTOR('',#30350,10.);
#8212=VECTOR('',#30351,10.);
#8213=VECTOR('',#30352,10.);
#8214=VECTOR('',#30357,10.);
#8215=VECTOR('',#30360,10.);
#8216=VECTOR('',#30363,10.);
#8217=VECTOR('',#30364,10.);
#8218=VECTOR('',#30369,10.);
#8219=VECTOR('',#30372,10.);
#8220=VECTOR('',#30373,10.);
#8221=VECTOR('',#30378,10.);
#8222=VECTOR('',#30381,10.);
#8223=VECTOR('',#30382,10.);
#8224=VECTOR('',#30385,10.);
#8225=VECTOR('',#30386,10.);
#8226=VECTOR('',#30389,10.);
#8227=VECTOR('',#30390,10.);
#8228=VECTOR('',#30393,10.);
#8229=VECTOR('',#30394,10.);
#8230=VECTOR('',#30397,10.);
#8231=VECTOR('',#30398,10.);
#8232=VECTOR('',#30401,10.);
#8233=VECTOR('',#30402,10.);
#8234=VECTOR('',#30407,10.);
#8235=VECTOR('',#30410,10.);
#8236=VECTOR('',#30411,10.);
#8237=VECTOR('',#30416,10.);
#8238=VECTOR('',#30419,10.);
#8239=VECTOR('',#30420,10.);
#8240=VECTOR('',#30425,10.);
#8241=VECTOR('',#30428,10.);
#8242=VECTOR('',#30429,10.);
#8243=VECTOR('',#30434,10.);
#8244=VECTOR('',#30437,10.);
#8245=VECTOR('',#30438,10.);
#8246=VECTOR('',#30441,10.);
#8247=VECTOR('',#30442,10.);
#8248=VECTOR('',#30445,10.);
#8249=VECTOR('',#30446,10.);
#8250=VECTOR('',#30449,10.);
#8251=VECTOR('',#30450,10.);
#8252=VECTOR('',#30453,10.);
#8253=VECTOR('',#30454,10.);
#8254=VECTOR('',#30457,10.);
#8255=VECTOR('',#30458,10.);
#8256=VECTOR('',#30463,10.);
#8257=VECTOR('',#30466,10.);
#8258=VECTOR('',#30473,5.099);
#8259=VECTOR('',#30478,5.099);
#8260=VECTOR('',#30481,5.099);
#8261=VECTOR('',#30484,5.099);
#8262=VECTOR('',#30489,5.099);
#8263=VECTOR('',#30494,5.099);
#8264=VECTOR('',#30497,5.099);
#8265=VECTOR('',#30500,5.099);
#8266=VECTOR('',#30505,2.55999999999999);
#8267=VECTOR('',#30510,2.55999999999999);
#8268=VECTOR('',#30513,2.55999999999999);
#8269=VECTOR('',#30516,2.55999999999999);
#8270=VECTOR('',#30519,2.55999999999999);
#8271=VECTOR('',#30522,2.55999999999999);
#8272=VECTOR('',#30525,2.55999999999999);
#8273=VECTOR('',#30528,2.55999999999999);
#8274=VECTOR('',#30531,2.55999999999999);
#8275=VECTOR('',#30534,2.55999999999999);
#8276=VECTOR('',#30537,2.55999999999999);
#8277=VECTOR('',#30540,2.55999999999999);
#8278=VECTOR('',#30543,2.55999999999999);
#8279=VECTOR('',#30546,2.55999999999999);
#8280=VECTOR('',#30549,2.55999999999999);
#8281=VECTOR('',#30552,2.55999999999999);
#8282=VECTOR('',#30555,2.55999999999999);
#8283=VECTOR('',#30558,2.55999999999999);
#8284=VECTOR('',#30561,2.55999999999999);
#8285=VECTOR('',#30564,2.55999999999999);
#8286=VECTOR('',#30567,2.55999999999999);
#8287=VECTOR('',#30570,2.55999999999999);
#8288=VECTOR('',#30573,2.55999999999999);
#8289=VECTOR('',#30576,2.55999999999999);
#8290=VECTOR('',#30579,2.55999999999999);
#8291=VECTOR('',#30582,2.55999999999999);
#8292=VECTOR('',#30585,2.55999999999999);
#8293=VECTOR('',#30590,2.56);
#8294=VECTOR('',#30595,2.56);
#8295=VECTOR('',#30598,2.56);
#8296=VECTOR('',#30601,2.56);
#8297=VECTOR('',#30604,2.56);
#8298=VECTOR('',#30607,2.56);
#8299=VECTOR('',#30610,2.56);
#8300=VECTOR('',#30613,2.56);
#8301=VECTOR('',#30616,2.56);
#8302=VECTOR('',#30619,2.56);
#8303=VECTOR('',#30622,2.56);
#8304=VECTOR('',#30625,2.56);
#8305=VECTOR('',#30628,2.56);
#8306=VECTOR('',#30631,2.56);
#8307=VECTOR('',#30634,2.56);
#8308=VECTOR('',#30637,2.56);
#8309=VECTOR('',#30640,2.56);
#8310=VECTOR('',#30643,2.56);
#8311=VECTOR('',#30646,2.56);
#8312=VECTOR('',#30649,2.56);
#8313=VECTOR('',#30652,2.56);
#8314=VECTOR('',#30655,2.56);
#8315=VECTOR('',#30658,2.56);
#8316=VECTOR('',#30661,2.56);
#8317=VECTOR('',#30664,2.56);
#8318=VECTOR('',#30667,2.56);
#8319=VECTOR('',#30670,2.56);
#8320=VECTOR('',#30675,2.56);
#8321=VECTOR('',#30680,2.56);
#8322=VECTOR('',#30683,2.56);
#8323=VECTOR('',#30686,2.56);
#8324=VECTOR('',#30689,2.56);
#8325=VECTOR('',#30692,2.56);
#8326=VECTOR('',#30695,2.56);
#8327=VECTOR('',#30698,2.56);
#8328=VECTOR('',#30701,2.56);
#8329=VECTOR('',#30704,2.56);
#8330=VECTOR('',#30707,2.56);
#8331=VECTOR('',#30710,2.56);
#8332=VECTOR('',#30713,2.56);
#8333=VECTOR('',#30716,2.56);
#8334=VECTOR('',#30719,2.56);
#8335=VECTOR('',#30722,2.56);
#8336=VECTOR('',#30725,2.56);
#8337=VECTOR('',#30728,2.56);
#8338=VECTOR('',#30731,2.56);
#8339=VECTOR('',#30734,2.56);
#8340=VECTOR('',#30737,2.56);
#8341=VECTOR('',#30740,2.56);
#8342=VECTOR('',#30743,2.56);
#8343=VECTOR('',#30746,2.56);
#8344=VECTOR('',#30749,2.56);
#8345=VECTOR('',#30752,2.56);
#8346=VECTOR('',#30755,2.56);
#8347=VECTOR('',#30760,2.56);
#8348=VECTOR('',#30765,2.56);
#8349=VECTOR('',#30768,2.56);
#8350=VECTOR('',#30771,2.56);
#8351=VECTOR('',#30774,2.56);
#8352=VECTOR('',#30777,2.56);
#8353=VECTOR('',#30780,2.56);
#8354=VECTOR('',#30783,2.56);
#8355=VECTOR('',#30786,2.56);
#8356=VECTOR('',#30789,2.56);
#8357=VECTOR('',#30792,2.56);
#8358=VECTOR('',#30795,2.56);
#8359=VECTOR('',#30798,2.56);
#8360=VECTOR('',#30801,2.56);
#8361=VECTOR('',#30804,2.56);
#8362=VECTOR('',#30807,2.56);
#8363=VECTOR('',#30810,2.56);
#8364=VECTOR('',#30813,2.56);
#8365=VECTOR('',#30816,2.56);
#8366=VECTOR('',#30819,2.56);
#8367=VECTOR('',#30822,2.56);
#8368=VECTOR('',#30825,2.56);
#8369=VECTOR('',#30828,2.56);
#8370=VECTOR('',#30831,2.56);
#8371=VECTOR('',#30834,2.56);
#8372=VECTOR('',#30837,2.56);
#8373=VECTOR('',#30840,2.56);
#8374=VECTOR('',#30845,4.263);
#8375=VECTOR('',#30850,4.263);
#8376=VECTOR('',#30853,4.263);
#8377=VECTOR('',#30856,4.263);
#8378=VECTOR('',#30861,4.263);
#8379=VECTOR('',#30866,4.263);
#8380=VECTOR('',#30871,4.263);
#8381=VECTOR('',#30874,4.263);
#8382=VECTOR('',#30879,2.117);
#8383=VECTOR('',#30884,2.117);
#8384=VECTOR('',#30887,2.117);
#8385=VECTOR('',#30890,2.117);
#8386=VECTOR('',#30893,2.117);
#8387=VECTOR('',#30896,2.117);
#8388=VECTOR('',#30899,2.117);
#8389=VECTOR('',#30902,2.117);
#8390=VECTOR('',#30905,2.117);
#8391=VECTOR('',#30908,2.117);
#8392=VECTOR('',#30911,2.117);
#8393=VECTOR('',#30914,2.117);
#8394=VECTOR('',#30917,2.117);
#8395=VECTOR('',#30920,2.117);
#8396=VECTOR('',#30923,2.117);
#8397=VECTOR('',#30926,2.117);
#8398=VECTOR('',#30929,2.117);
#8399=VECTOR('',#30932,2.117);
#8400=VECTOR('',#30935,2.117);
#8401=VECTOR('',#30938,2.117);
#8402=VECTOR('',#30941,2.117);
#8403=VECTOR('',#30944,2.117);
#8404=VECTOR('',#30947,2.117);
#8405=VECTOR('',#30950,2.117);
#8406=VECTOR('',#30953,2.117);
#8407=VECTOR('',#30956,2.117);
#8408=VECTOR('',#30959,2.117);
#8409=VECTOR('',#30964,2.117);
#8410=VECTOR('',#30969,2.117);
#8411=VECTOR('',#30972,2.117);
#8412=VECTOR('',#30975,2.117);
#8413=VECTOR('',#30978,2.117);
#8414=VECTOR('',#30981,2.117);
#8415=VECTOR('',#30984,2.117);
#8416=VECTOR('',#30987,2.117);
#8417=VECTOR('',#30990,2.117);
#8418=VECTOR('',#30993,2.117);
#8419=VECTOR('',#30996,2.117);
#8420=VECTOR('',#30999,2.117);
#8421=VECTOR('',#31002,2.117);
#8422=VECTOR('',#31005,2.117);
#8423=VECTOR('',#31008,2.117);
#8424=VECTOR('',#31011,2.117);
#8425=VECTOR('',#31014,2.117);
#8426=VECTOR('',#31017,2.117);
#8427=VECTOR('',#31020,2.117);
#8428=VECTOR('',#31023,2.117);
#8429=VECTOR('',#31026,2.117);
#8430=VECTOR('',#31029,2.117);
#8431=VECTOR('',#31032,2.117);
#8432=VECTOR('',#31035,2.117);
#8433=VECTOR('',#31038,2.117);
#8434=VECTOR('',#31041,2.117);
#8435=VECTOR('',#31044,2.117);
#8436=VECTOR('',#31049,2.117);
#8437=VECTOR('',#31054,2.117);
#8438=VECTOR('',#31057,2.117);
#8439=VECTOR('',#31060,2.117);
#8440=VECTOR('',#31063,2.117);
#8441=VECTOR('',#31066,2.117);
#8442=VECTOR('',#31069,2.117);
#8443=VECTOR('',#31072,2.117);
#8444=VECTOR('',#31075,2.117);
#8445=VECTOR('',#31078,2.117);
#8446=VECTOR('',#31081,2.117);
#8447=VECTOR('',#31084,2.117);
#8448=VECTOR('',#31087,2.117);
#8449=VECTOR('',#31090,2.117);
#8450=VECTOR('',#31093,2.117);
#8451=VECTOR('',#31096,2.117);
#8452=VECTOR('',#31099,2.117);
#8453=VECTOR('',#31102,2.117);
#8454=VECTOR('',#31105,2.117);
#8455=VECTOR('',#31108,2.117);
#8456=VECTOR('',#31111,2.117);
#8457=VECTOR('',#31114,2.117);
#8458=VECTOR('',#31117,2.117);
#8459=VECTOR('',#31120,2.117);
#8460=VECTOR('',#31123,2.117);
#8461=VECTOR('',#31126,2.117);
#8462=VECTOR('',#31129,2.117);
#8463=VECTOR('',#31134,2.117);
#8464=VECTOR('',#31139,2.117);
#8465=VECTOR('',#31142,2.117);
#8466=VECTOR('',#31145,2.117);
#8467=VECTOR('',#31148,2.117);
#8468=VECTOR('',#31151,2.117);
#8469=VECTOR('',#31154,2.117);
#8470=VECTOR('',#31157,2.117);
#8471=VECTOR('',#31160,2.117);
#8472=VECTOR('',#31163,2.117);
#8473=VECTOR('',#31166,2.117);
#8474=VECTOR('',#31169,2.117);
#8475=VECTOR('',#31172,2.117);
#8476=VECTOR('',#31175,2.117);
#8477=VECTOR('',#31178,2.117);
#8478=VECTOR('',#31181,2.117);
#8479=VECTOR('',#31184,2.117);
#8480=VECTOR('',#31187,2.117);
#8481=VECTOR('',#31190,2.117);
#8482=VECTOR('',#31193,2.117);
#8483=VECTOR('',#31196,2.117);
#8484=VECTOR('',#31199,2.117);
#8485=VECTOR('',#31202,2.117);
#8486=VECTOR('',#31205,2.117);
#8487=VECTOR('',#31208,2.117);
#8488=VECTOR('',#31211,2.117);
#8489=VECTOR('',#31214,2.117);
#8490=VECTOR('',#31247,4.);
#8491=VECTOR('',#31256,10.);
#8492=VECTOR('',#31259,10.);
#8493=VECTOR('',#31262,10.);
#8494=VECTOR('',#31263,10.);
#8495=VECTOR('',#31264,10.);
#8496=VECTOR('',#31271,4.);
#8497=VECTOR('',#31280,10.);
#8498=VECTOR('',#31283,10.);
#8499=VECTOR('',#31286,10.);
#8500=VECTOR('',#31287,10.);
#8501=VECTOR('',#31288,10.);
#8502=VECTOR('',#31295,5.);
#8503=VECTOR('',#31302,10.);
#8504=VECTOR('',#31303,10.);
#8505=VECTOR('',#31304,10.);
#8506=VECTOR('',#31307,10.);
#8507=VECTOR('',#31308,10.);
#8508=VECTOR('',#31309,10.);
#8509=VECTOR('',#31310,10.);
#8510=VECTOR('',#31313,10.);
#8511=VECTOR('',#31314,10.);
#8512=VECTOR('',#31315,10.);
#8513=VECTOR('',#31318,10.);
#8514=VECTOR('',#31321,10.);
#8515=VECTOR('',#31324,10.);
#8516=VECTOR('',#31327,10.);
#8517=VECTOR('',#31330,10.);
#8518=VECTOR('',#31331,10.);
#8519=VECTOR('',#31332,10.);
#8520=VECTOR('',#31333,10.);
#8521=VECTOR('',#31334,10.);
#8522=VECTOR('',#31337,10.);
#8523=VECTOR('',#31340,10.);
#8524=VECTOR('',#31341,10.);
#8525=VECTOR('',#31342,10.);
#8526=VECTOR('',#31343,10.);
#8527=VECTOR('',#31344,10.);
#8528=VECTOR('',#31347,10.);
#8529=VECTOR('',#31350,10.);
#8530=VECTOR('',#31353,10.);
#8531=VECTOR('',#31362,10.);
#8532=VECTOR('',#31363,10.);
#8533=VECTOR('',#31364,10.);
#8534=VECTOR('',#31365,10.);
#8535=VECTOR('',#31368,10.);
#8536=VECTOR('',#31369,10.);
#8537=VECTOR('',#31370,10.);
#8538=VECTOR('',#31373,10.);
#8539=VECTOR('',#31374,10.);
#8540=VECTOR('',#31375,10.);
#8541=VECTOR('',#31378,10.);
#8542=VECTOR('',#31379,10.);
#8543=VECTOR('',#31380,10.);
#8544=VECTOR('',#31383,10.);
#8545=VECTOR('',#31384,10.);
#8546=VECTOR('',#31385,10.);
#8547=VECTOR('',#31388,10.);
#8548=VECTOR('',#31389,10.);
#8549=VECTOR('',#31390,10.);
#8550=VECTOR('',#31393,10.);
#8551=VECTOR('',#31394,10.);
#8552=VECTOR('',#31399,3.);
#8553=VECTOR('',#31408,10.);
#8554=VECTOR('',#31411,10.);
#8555=VECTOR('',#31414,10.);
#8556=VECTOR('',#31415,10.);
#8557=VECTOR('',#31416,10.);
#8558=VECTOR('',#31423,10.);
#8559=VECTOR('',#31426,10.);
#8560=VECTOR('',#31427,10.);
#8561=VECTOR('',#31430,10.);
#8562=VECTOR('',#31431,10.);
#8563=VECTOR('',#31440,10.);
#8564=VECTOR('',#31441,10.);
#8565=VECTOR('',#31442,10.);
#8566=VECTOR('',#31443,10.);
#8567=VECTOR('',#31446,10.);
#8568=VECTOR('',#31447,10.);
#8569=VECTOR('',#31448,10.);
#8570=VECTOR('',#31451,10.);
#8571=VECTOR('',#31452,10.);
#8572=VECTOR('',#31453,10.);
#8573=VECTOR('',#31456,10.);
#8574=VECTOR('',#31457,10.);
#8575=VECTOR('',#31458,10.);
#8576=VECTOR('',#31461,10.);
#8577=VECTOR('',#31462,10.);
#8578=VECTOR('',#31463,10.);
#8579=VECTOR('',#31466,10.);
#8580=VECTOR('',#31467,10.);
#8581=VECTOR('',#31468,10.);
#8582=VECTOR('',#31471,10.);
#8583=VECTOR('',#31472,10.);
#8584=VECTOR('',#31477,3.);
#8585=VECTOR('',#31490,4.);
#8586=VECTOR('',#31499,5.);
#8587=VECTOR('',#31506,10.);
#8588=VECTOR('',#31509,10.);
#8589=VECTOR('',#31512,10.);
#8590=VECTOR('',#31513,10.);
#8591=VECTOR('',#31514,10.);
#8592=VECTOR('',#31519,10.);
#8593=VECTOR('',#31524,10.);
#8594=VECTOR('',#31525,10.);
#8595=VECTOR('',#31528,10.);
#8596=VECTOR('',#31529,10.);
#8597=VECTOR('',#31538,10.);
#8598=VECTOR('',#31539,10.);
#8599=VECTOR('',#31540,10.);
#8600=VECTOR('',#31541,10.);
#8601=VECTOR('',#31544,10.);
#8602=VECTOR('',#31545,10.);
#8603=VECTOR('',#31546,10.);
#8604=VECTOR('',#31549,10.);
#8605=VECTOR('',#31550,10.);
#8606=VECTOR('',#31551,10.);
#8607=VECTOR('',#31554,10.);
#8608=VECTOR('',#31555,10.);
#8609=VECTOR('',#31556,10.);
#8610=VECTOR('',#31559,10.);
#8611=VECTOR('',#31560,10.);
#8612=VECTOR('',#31561,10.);
#8613=VECTOR('',#31564,10.);
#8614=VECTOR('',#31565,10.);
#8615=VECTOR('',#31566,10.);
#8616=VECTOR('',#31569,10.);
#8617=VECTOR('',#31570,10.);
#8618=VECTOR('',#31575,3.);
#8619=VECTOR('',#31582,10.);
#8620=VECTOR('',#31583,10.);
#8621=VECTOR('',#31584,10.);
#8622=VECTOR('',#31585,10.);
#8623=VECTOR('',#31588,10.);
#8624=VECTOR('',#31589,10.);
#8625=VECTOR('',#31590,10.);
#8626=VECTOR('',#31593,10.);
#8627=VECTOR('',#31594,10.);
#8628=VECTOR('',#31595,10.);
#8629=VECTOR('',#31598,10.);
#8630=VECTOR('',#31599,10.);
#8631=VECTOR('',#31600,10.);
#8632=VECTOR('',#31603,10.);
#8633=VECTOR('',#31604,10.);
#8634=VECTOR('',#31605,10.);
#8635=VECTOR('',#31608,10.);
#8636=VECTOR('',#31609,10.);
#8637=VECTOR('',#31610,10.);
#8638=VECTOR('',#31613,10.);
#8639=VECTOR('',#31614,10.);
#8640=VECTOR('',#31619,3.);
#8641=VECTOR('',#31630,10.);
#8642=VECTOR('',#31631,10.);
#8643=VECTOR('',#31632,10.);
#8644=VECTOR('',#31637,5.);
#8645=VECTOR('',#31644,4.);
#8646=VECTOR('',#31651,2.5);
#8647=VECTOR('',#31658,2.5);
#8648=VECTOR('',#31665,10.);
#8649=VECTOR('',#31666,10.);
#8650=VECTOR('',#31675,10.);
#8651=VECTOR('',#31678,10.);
#8652=VECTOR('',#31679,10.);
#8653=VECTOR('',#31684,10.);
#8654=VECTOR('',#31687,10.);
#8655=VECTOR('',#31688,10.);
#8656=VECTOR('',#31693,10.);
#8657=VECTOR('',#31696,10.);
#8658=VECTOR('',#31697,10.);
#8659=VECTOR('',#31706,10.);
#8660=VECTOR('',#31709,10.);
#8661=VECTOR('',#31710,10.);
#8662=VECTOR('',#31715,10.);
#8663=VECTOR('',#31718,10.);
#8664=VECTOR('',#31719,10.);
#8665=VECTOR('',#31724,10.);
#8666=VECTOR('',#31727,10.);
#8667=VECTOR('',#31728,10.);
#8668=VECTOR('',#31733,10.);
#8669=VECTOR('',#31736,10.);
#8670=VECTOR('',#31737,10.);
#8671=VECTOR('',#31742,10.);
#8672=VECTOR('',#31745,10.);
#8673=VECTOR('',#31746,10.);
#8674=VECTOR('',#31751,10.);
#8675=VECTOR('',#31754,10.);
#8676=VECTOR('',#31755,10.);
#8677=VECTOR('',#31770,3.);
#8678=VECTOR('',#31779,3.);
#8679=VECTOR('',#31786,10.);
#8680=VECTOR('',#31789,10.);
#8681=VECTOR('',#31794,10.);
#8682=VECTOR('',#31797,10.);
#8683=VECTOR('',#31802,10.);
#8684=VECTOR('',#31805,10.);
#8685=VECTOR('',#31818,10.);
#8686=VECTOR('',#31819,10.);
#8687=VECTOR('',#31832,10.);
#8688=VECTOR('',#31833,10.);
#8689=VECTOR('',#31846,10.);
#8690=VECTOR('',#31847,10.);
#8691=VECTOR('',#31856,10.);
#8692=VECTOR('',#31857,10.);
#8693=VECTOR('',#31862,10.);
#8694=VECTOR('',#31863,10.);
#8695=VECTOR('',#31868,10.);
#8696=VECTOR('',#31871,10.);
#8697=VECTOR('',#31882,10.);
#8698=VECTOR('',#31883,10.);
#8699=VECTOR('',#31888,10.);
#8700=VECTOR('',#31889,10.);
#8701=VECTOR('',#31892,10.);
#8702=VECTOR('',#31895,10.);
#8703=VECTOR('',#31906,10.);
#8704=VECTOR('',#31907,10.);
#8705=VECTOR('',#31912,10.);
#8706=VECTOR('',#31915,10.);
#8707=VECTOR('',#31918,10.);
#8708=VECTOR('',#31921,10.);
#8709=VECTOR('',#31932,10.);
#8710=VECTOR('',#31933,10.);
#8711=VECTOR('',#31946,10.);
#8712=VECTOR('',#31947,10.);
#8713=VECTOR('',#31960,10.);
#8714=VECTOR('',#31961,10.);
#8715=VECTOR('',#31974,10.);
#8716=VECTOR('',#31975,10.);
#8717=VECTOR('',#31980,10.);
#8718=VECTOR('',#31983,10.);
#8719=VECTOR('',#31986,10.);
#8720=VECTOR('',#31989,10.);
#8721=VECTOR('',#31992,10.);
#8722=VECTOR('',#31995,10.);
#8723=VECTOR('',#32006,10.);
#8724=VECTOR('',#32007,10.);
#8725=VECTOR('',#32008,10.);
#8726=VECTOR('',#32011,10.);
#8727=VECTOR('',#32016,10.);
#8728=VECTOR('',#32017,10.);
#8729=VECTOR('',#32020,10.);
#8730=VECTOR('',#32021,10.);
#8731=VECTOR('',#32024,10.);
#8732=VECTOR('',#32025,10.);
#8733=VECTOR('',#32028,10.);
#8734=VECTOR('',#32033,10.);
#8735=VECTOR('',#32034,10.);
#8736=VECTOR('',#32037,10.);
#8737=VECTOR('',#32042,10.);
#8738=VECTOR('',#32043,10.);
#8739=VECTOR('',#32046,10.);
#8740=VECTOR('',#32049,10.);
#8741=VECTOR('',#32054,10.);
#8742=VECTOR('',#32055,10.);
#8743=VECTOR('',#32058,10.);
#8744=VECTOR('',#32063,10.);
#8745=VECTOR('',#32064,10.);
#8746=VECTOR('',#32065,10.);
#8747=VECTOR('',#32066,10.);
#8748=VECTOR('',#32069,10.);
#8749=VECTOR('',#32074,10.);
#8750=VECTOR('',#32075,10.);
#8751=VECTOR('',#32078,10.);
#8752=VECTOR('',#32079,10.);
#8753=VECTOR('',#32082,10.);
#8754=VECTOR('',#32083,10.);
#8755=VECTOR('',#32090,10.);
#8756=VECTOR('',#32101,10.);
#8757=VECTOR('',#32108,10.);
#8758=VECTOR('',#32113,10.);
#8759=VECTOR('',#32124,10.);
#8760=VECTOR('',#32127,10.);
#8761=VECTOR('',#32134,10.);
#8762=VECTOR('',#32141,10.);
#8763=VECTOR('',#32144,10.);
#8764=VECTOR('',#32147,10.);
#8765=VECTOR('',#32148,10.);
#8766=VECTOR('',#32149,10.);
#8767=VECTOR('',#32152,10.);
#8768=VECTOR('',#32153,10.);
#8769=VECTOR('',#32154,10.);
#8770=VECTOR('',#32155,10.);
#8771=VECTOR('',#32156,10.);
#8772=VECTOR('',#32159,10.);
#8773=VECTOR('',#32160,10.);
#8774=VECTOR('',#32161,10.);
#8775=VECTOR('',#32164,10.);
#8776=VECTOR('',#32171,10.);
#8777=VECTOR('',#32212,10.);
#8778=VECTOR('',#32221,10.);
#8779=VECTOR('',#32224,10.);
#8780=VECTOR('',#32227,10.);
#8781=VECTOR('',#32240,10.);
#8782=VECTOR('',#32243,10.);
#8783=VECTOR('',#32256,10.);
#8784=VECTOR('',#32263,10.);
#8785=VECTOR('',#32266,10.);
#8786=VECTOR('',#32269,10.);
#8787=VECTOR('',#32272,10.);
#8788=VECTOR('',#32275,10.);
#8789=VECTOR('',#32278,10.);
#8790=VECTOR('',#32281,10.);
#8791=VECTOR('',#32284,10.);
#8792=VECTOR('',#32287,10.);
#8793=VECTOR('',#32290,10.);
#8794=VECTOR('',#32293,10.);
#8795=VECTOR('',#32296,10.);
#8796=VECTOR('',#32299,10.);
#8797=VECTOR('',#32302,10.);
#8798=VECTOR('',#32305,10.);
#8799=VECTOR('',#32308,10.);
#8800=VECTOR('',#32319,10.);
#8801=VECTOR('',#32320,10.);
#8802=VECTOR('',#32325,10.);
#8803=VECTOR('',#32328,10.);
#8804=VECTOR('',#32331,10.);
#8805=VECTOR('',#32340,3.);
#8806=VECTOR('',#32349,3.);
#8807=VECTOR('',#32356,10.);
#8808=VECTOR('',#32359,10.);
#8809=VECTOR('',#32364,10.);
#8810=VECTOR('',#32367,10.);
#8811=VECTOR('',#32372,10.);
#8812=VECTOR('',#32375,10.);
#8813=VECTOR('',#32388,10.);
#8814=VECTOR('',#32389,10.);
#8815=VECTOR('',#32402,10.);
#8816=VECTOR('',#32403,10.);
#8817=VECTOR('',#32416,10.);
#8818=VECTOR('',#32417,10.);
#8819=VECTOR('',#32426,10.);
#8820=VECTOR('',#32429,10.);
#8821=VECTOR('',#32432,10.);
#8822=VECTOR('',#32435,10.);
#8823=VECTOR('',#32438,10.);
#8824=VECTOR('',#32439,10.);
#8825=VECTOR('',#32452,10.);
#8826=VECTOR('',#32455,10.);
#8827=VECTOR('',#32458,10.);
#8828=VECTOR('',#32459,10.);
#8829=VECTOR('',#32462,10.);
#8830=VECTOR('',#32463,10.);
#8831=VECTOR('',#32476,10.);
#8832=VECTOR('',#32479,10.);
#8833=VECTOR('',#32482,10.);
#8834=VECTOR('',#32483,10.);
#8835=VECTOR('',#32488,10.);
#8836=VECTOR('',#32489,10.);
#8837=VECTOR('',#32502,10.);
#8838=VECTOR('',#32503,10.);
#8839=VECTOR('',#32516,10.);
#8840=VECTOR('',#32517,10.);
#8841=VECTOR('',#32530,10.);
#8842=VECTOR('',#32531,10.);
#8843=VECTOR('',#32544,10.);
#8844=VECTOR('',#32545,10.);
#8845=VECTOR('',#32550,10.);
#8846=VECTOR('',#32553,10.);
#8847=VECTOR('',#32556,10.);
#8848=VECTOR('',#32559,10.);
#8849=VECTOR('',#32562,10.);
#8850=VECTOR('',#32565,10.);
#8851=VECTOR('',#32576,10.);
#8852=VECTOR('',#32577,10.);
#8853=VECTOR('',#32578,10.);
#8854=VECTOR('',#32583,10.);
#8855=VECTOR('',#32586,10.);
#8856=VECTOR('',#32587,10.);
#8857=VECTOR('',#32590,10.);
#8858=VECTOR('',#32591,10.);
#8859=VECTOR('',#32594,10.);
#8860=VECTOR('',#32595,10.);
#8861=VECTOR('',#32600,10.);
#8862=VECTOR('',#32603,10.);
#8863=VECTOR('',#32604,10.);
#8864=VECTOR('',#32609,10.);
#8865=VECTOR('',#32612,10.);
#8866=VECTOR('',#32613,10.);
#8867=VECTOR('',#32618,10.);
#8868=VECTOR('',#32621,10.);
#8869=VECTOR('',#32624,10.);
#8870=VECTOR('',#32625,10.);
#8871=VECTOR('',#32630,10.);
#8872=VECTOR('',#32633,10.);
#8873=VECTOR('',#32634,10.);
#8874=VECTOR('',#32635,10.);
#8875=VECTOR('',#32636,10.);
#8876=VECTOR('',#32641,10.);
#8877=VECTOR('',#32644,10.);
#8878=VECTOR('',#32645,10.);
#8879=VECTOR('',#32648,10.);
#8880=VECTOR('',#32649,10.);
#8881=VECTOR('',#32652,10.);
#8882=VECTOR('',#32653,10.);
#8883=VECTOR('',#32658,10.);
#8884=VECTOR('',#32673,10.);
#8885=VECTOR('',#32678,10.);
#8886=VECTOR('',#32681,10.);
#8887=VECTOR('',#32694,10.);
#8888=VECTOR('',#32695,10.);
#8889=VECTOR('',#32708,10.);
#8890=VECTOR('',#32713,10.);
#8891=VECTOR('',#32716,10.);
#8892=VECTOR('',#32717,10.);
#8893=VECTOR('',#32718,10.);
#8894=VECTOR('',#32721,10.);
#8895=VECTOR('',#32722,10.);
#8896=VECTOR('',#32723,10.);
#8897=VECTOR('',#32724,10.);
#8898=VECTOR('',#32725,10.);
#8899=VECTOR('',#32728,10.);
#8900=VECTOR('',#32729,10.);
#8901=VECTOR('',#32730,10.);
#8902=VECTOR('',#32733,10.);
#8903=VECTOR('',#32736,10.);
#8904=VECTOR('',#32741,10.);
#8905=VECTOR('',#32782,10.);
#8906=VECTOR('',#32791,10.);
#8907=VECTOR('',#32794,10.);
#8908=VECTOR('',#32797,10.);
#8909=VECTOR('',#32810,10.);
#8910=VECTOR('',#32813,10.);
#8911=VECTOR('',#32826,10.);
#8912=VECTOR('',#32833,10.);
#8913=VECTOR('',#32836,10.);
#8914=VECTOR('',#32839,10.);
#8915=VECTOR('',#32842,10.);
#8916=VECTOR('',#32845,10.);
#8917=VECTOR('',#32848,10.);
#8918=VECTOR('',#32851,10.);
#8919=VECTOR('',#32854,10.);
#8920=VECTOR('',#32857,10.);
#8921=VECTOR('',#32860,10.);
#8922=VECTOR('',#32863,10.);
#8923=VECTOR('',#32866,10.);
#8924=VECTOR('',#32869,10.);
#8925=VECTOR('',#32872,10.);
#8926=VECTOR('',#32875,10.);
#8927=VECTOR('',#32880,10.);
#8928=VECTOR('',#32889,10.);
#8929=VECTOR('',#32892,10.);
#8930=VECTOR('',#32895,10.);
#8931=VECTOR('',#32898,10.);
#8932=VECTOR('',#32901,10.);
#8933=VECTOR('',#32910,3.);
#8934=VECTOR('',#32921,3.00000000000001);
#8935=VECTOR('',#32928,10.);
#8936=VECTOR('',#32929,10.);
#8937=VECTOR('',#32930,10.);
#8938=VECTOR('',#32931,10.);
#8939=VECTOR('',#32932,10.);
#8940=VECTOR('',#32933,10.);
#8941=VECTOR('',#32936,10.);
#8942=VECTOR('',#32943,3.);
#8943=VECTOR('',#32946,10.);
#8944=VECTOR('',#32947,10.);
#8945=VECTOR('',#32952,10.);
#8946=VECTOR('',#32955,10.);
#8947=VECTOR('',#32956,10.);
#8948=VECTOR('',#32959,3.);
#8949=VECTOR('',#32962,10.);
#8950=VECTOR('',#32963,10.);
#8951=VECTOR('',#32966,10.);
#8952=VECTOR('',#32971,10.);
#8953=VECTOR('',#32972,10.);
#8954=VECTOR('',#32975,3.);
#8955=VECTOR('',#32982,10.);
#8956=VECTOR('',#32987,10.);
#8957=VECTOR('',#32992,10.);
#8958=VECTOR('',#32999,3.);
#8959=VECTOR('',#33002,10.);
#8960=VECTOR('',#33003,10.);
#8961=VECTOR('',#33008,10.);
#8962=VECTOR('',#33011,10.);
#8963=VECTOR('',#33012,10.);
#8964=VECTOR('',#33015,3.);
#8965=VECTOR('',#33018,10.);
#8966=VECTOR('',#33019,10.);
#8967=VECTOR('',#33022,10.);
#8968=VECTOR('',#33027,10.);
#8969=VECTOR('',#33028,10.);
#8970=VECTOR('',#33031,3.);
#8971=VECTOR('',#33038,10.);
#8972=VECTOR('',#33043,10.);
#8973=VECTOR('',#33048,10.);
#8974=VECTOR('',#33055,3.00000000000001);
#8975=VECTOR('',#33058,10.);
#8976=VECTOR('',#33059,10.);
#8977=VECTOR('',#33064,10.);
#8978=VECTOR('',#33067,10.);
#8979=VECTOR('',#33068,10.);
#8980=VECTOR('',#33071,3.00000000000001);
#8981=VECTOR('',#33074,10.);
#8982=VECTOR('',#33075,10.);
#8983=VECTOR('',#33078,10.);
#8984=VECTOR('',#33083,10.);
#8985=VECTOR('',#33084,10.);
#8986=VECTOR('',#33087,3.00000000000001);
#8987=VECTOR('',#33094,10.);
#8988=VECTOR('',#33099,10.);
#8989=VECTOR('',#33104,10.);
#8990=VECTOR('',#33107,10.);
#8991=VECTOR('',#33110,10.);
#8992=VECTOR('',#33111,10.);
#8993=VECTOR('',#33112,10.);
#8994=VECTOR('',#33115,10.);
#8995=VECTOR('',#33116,10.);
#8996=VECTOR('',#33119,10.);
#8997=VECTOR('',#33120,10.);
#8998=VECTOR('',#33123,10.);
#8999=VECTOR('',#33126,10.);
#9000=VECTOR('',#33133,10.);
#9001=VECTOR('',#33136,10.);
#9002=VECTOR('',#33139,10.);
#9003=VECTOR('',#33140,10.);
#9004=VECTOR('',#33143,10.);
#9005=VECTOR('',#33144,10.);
#9006=VECTOR('',#33147,10.);
#9007=VECTOR('',#33150,10.);
#9008=VECTOR('',#33157,10.);
#9009=VECTOR('',#33160,10.);
#9010=VECTOR('',#33163,10.);
#9011=VECTOR('',#33164,10.);
#9012=VECTOR('',#33167,10.);
#9013=VECTOR('',#33168,10.);
#9014=VECTOR('',#33171,10.);
#9015=VECTOR('',#33174,10.);
#9016=VECTOR('',#33181,10.);
#9017=VECTOR('',#33184,10.);
#9018=VECTOR('',#33187,10.);
#9019=VECTOR('',#33188,10.);
#9020=VECTOR('',#33191,10.);
#9021=VECTOR('',#33192,10.);
#9022=VECTOR('',#33195,10.);
#9023=VECTOR('',#33198,10.);
#9024=VECTOR('',#33205,10.);
#9025=VECTOR('',#33208,10.);
#9026=VECTOR('',#33211,10.);
#9027=VECTOR('',#33212,10.);
#9028=VECTOR('',#33215,10.);
#9029=VECTOR('',#33216,10.);
#9030=VECTOR('',#33219,10.);
#9031=VECTOR('',#33222,10.);
#9032=VECTOR('',#33229,10.);
#9033=VECTOR('',#33232,10.);
#9034=VECTOR('',#33235,10.);
#9035=VECTOR('',#33236,10.);
#9036=VECTOR('',#33239,10.);
#9037=VECTOR('',#33240,10.);
#9038=VECTOR('',#33243,10.);
#9039=VECTOR('',#33246,10.);
#9040=VECTOR('',#33247,10.);
#9041=VECTOR('',#33248,10.);
#9042=VECTOR('',#33251,10.);
#9043=VECTOR('',#33254,10.);
#9044=VECTOR('',#33257,10.);
#9045=VECTOR('',#33258,10.);
#9046=VECTOR('',#33261,10.);
#9047=VECTOR('',#33264,10.);
#9048=VECTOR('',#33267,10.);
#9049=VECTOR('',#33272,10.);
#9050=VECTOR('',#33275,10.);
#9051=VECTOR('',#33278,10.);
#9052=VECTOR('',#33279,10.);
#9053=VECTOR('',#33282,10.);
#9054=VECTOR('',#33285,10.);
#9055=VECTOR('',#33288,10.);
#9056=VECTOR('',#33293,10.);
#9057=VECTOR('',#33296,10.);
#9058=VECTOR('',#33299,10.);
#9059=VECTOR('',#33300,10.);
#9060=VECTOR('',#33303,10.);
#9061=VECTOR('',#33306,10.);
#9062=VECTOR('',#33309,10.);
#9063=VECTOR('',#33314,10.);
#9064=VECTOR('',#33317,10.);
#9065=VECTOR('',#33320,10.);
#9066=VECTOR('',#33321,10.);
#9067=VECTOR('',#33324,10.);
#9068=VECTOR('',#33327,10.);
#9069=VECTOR('',#33330,10.);
#9070=VECTOR('',#33335,10.);
#9071=VECTOR('',#33338,10.);
#9072=VECTOR('',#33341,10.);
#9073=VECTOR('',#33342,10.);
#9074=VECTOR('',#33345,10.);
#9075=VECTOR('',#33348,10.);
#9076=VECTOR('',#33351,10.);
#9077=VECTOR('',#33356,10.);
#9078=VECTOR('',#33359,10.);
#9079=VECTOR('',#33362,10.);
#9080=VECTOR('',#33363,10.);
#9081=VECTOR('',#33366,10.);
#9082=VECTOR('',#33369,10.);
#9083=VECTOR('',#33374,2.5);
#9084=VECTOR('',#33381,2.5);
#9085=VECTOR('',#33388,2.5);
#9086=VECTOR('',#33393,10.);
#9087=VECTOR('',#33394,10.);
#9088=VECTOR('',#33395,10.);
#9089=VECTOR('',#33396,10.);
#9090=VECTOR('',#33399,10.);
#9091=VECTOR('',#33400,10.);
#9092=VECTOR('',#33401,10.);
#9093=VECTOR('',#33406,10.);
#9094=VECTOR('',#33411,10.);
#9095=VECTOR('',#33412,10.);
#9096=VECTOR('',#33413,10.);
#9097=VECTOR('',#33416,10.);
#9098=VECTOR('',#33423,10.);
#9099=VECTOR('',#33426,10.);
#9100=VECTOR('',#33429,10.);
#9101=VECTOR('',#33432,10.);
#9102=VECTOR('',#33435,10.);
#9103=VECTOR('',#33438,10.);
#9104=VECTOR('',#33441,10.);
#9105=VECTOR('',#33444,10.);
#9106=VECTOR('',#33447,10.);
#9107=VECTOR('',#33450,10.);
#9108=VECTOR('',#33455,10.);
#9109=VECTOR('',#33456,10.);
#9110=VECTOR('',#33457,10.);
#9111=VECTOR('',#33462,10.);
#9112=VECTOR('',#33467,10.);
#9113=VECTOR('',#33468,10.);
#9114=VECTOR('',#33469,10.);
#9115=VECTOR('',#33474,10.);
#9116=VECTOR('',#33479,10.);
#9117=VECTOR('',#33480,10.);
#9118=VECTOR('',#33481,10.);
#9119=VECTOR('',#33486,10.);
#9120=VECTOR('',#33491,10.);
#9121=VECTOR('',#33492,10.);
#9122=VECTOR('',#33493,10.);
#9123=VECTOR('',#33498,10.);
#9124=VECTOR('',#33503,10.);
#9125=VECTOR('',#33504,10.);
#9126=VECTOR('',#33505,10.);
#9127=VECTOR('',#33510,10.);
#9128=VECTOR('',#33515,10.);
#9129=VECTOR('',#33516,10.);
#9130=VECTOR('',#33517,10.);
#9131=VECTOR('',#33522,10.);
#9132=VECTOR('',#33527,10.);
#9133=VECTOR('',#33528,10.);
#9134=VECTOR('',#33529,10.);
#9135=VECTOR('',#33532,10.);
#9136=VECTOR('',#33533,10.);
#9137=VECTOR('',#33534,10.);
#9138=VECTOR('',#33537,10.);
#9139=VECTOR('',#33538,10.);
#9140=VECTOR('',#33539,10.);
#9141=VECTOR('',#33544,10.);
#9142=VECTOR('',#33549,10.);
#9143=VECTOR('',#33550,10.);
#9144=VECTOR('',#33551,10.);
#9145=VECTOR('',#33554,10.);
#9146=VECTOR('',#33555,10.);
#9147=VECTOR('',#33556,10.);
#9148=VECTOR('',#33559,10.);
#9149=VECTOR('',#33560,10.);
#9150=VECTOR('',#33563,10.);
#9151=VECTOR('',#33564,10.);
#9152=VECTOR('',#33565,10.);
#9153=VECTOR('',#33572,10.);
#9154=VECTOR('',#33575,10.);
#9155=VECTOR('',#33576,10.);
#9156=VECTOR('',#33577,10.);
#9157=VECTOR('',#33580,10.);
#9158=VECTOR('',#33587,10.);
#9159=VECTOR('',#33588,10.);
#9160=VECTOR('',#33591,10.);
#9161=VECTOR('',#33596,10.);
#9162=VECTOR('',#33597,10.);
#9163=VECTOR('',#33600,10.);
#9164=VECTOR('',#33605,10.);
#9165=VECTOR('',#33606,10.);
#9166=VECTOR('',#33609,10.);
#9167=VECTOR('',#33614,10.);
#9168=VECTOR('',#33615,10.);
#9169=VECTOR('',#33618,10.);
#9170=VECTOR('',#33623,10.);
#9171=VECTOR('',#33624,10.);
#9172=VECTOR('',#33627,10.);
#9173=VECTOR('',#33632,10.);
#9174=VECTOR('',#33635,10.);
#9175=VECTOR('',#33636,10.);
#9176=VECTOR('',#33637,10.);
#9177=VECTOR('',#33644,10.);
#9178=VECTOR('',#33647,10.);
#9179=VECTOR('',#33648,10.);
#9180=VECTOR('',#33649,10.);
#9181=VECTOR('',#33656,10.);
#9182=VECTOR('',#33659,10.);
#9183=VECTOR('',#33660,10.);
#9184=VECTOR('',#33661,10.);
#9185=VECTOR('',#33668,10.);
#9186=VECTOR('',#33671,10.);
#9187=VECTOR('',#33672,10.);
#9188=VECTOR('',#33673,10.);
#9189=VECTOR('',#33680,10.);
#9190=VECTOR('',#33683,10.);
#9191=VECTOR('',#33684,10.);
#9192=VECTOR('',#33685,10.);
#9193=VECTOR('',#33692,10.);
#9194=VECTOR('',#33695,10.);
#9195=VECTOR('',#33696,10.);
#9196=VECTOR('',#33697,10.);
#9197=VECTOR('',#33704,10.);
#9198=VECTOR('',#33707,10.);
#9199=VECTOR('',#33708,10.);
#9200=VECTOR('',#33709,10.);
#9201=VECTOR('',#33712,10.);
#9202=VECTOR('',#33713,10.);
#9203=VECTOR('',#33714,10.);
#9204=VECTOR('',#33717,10.);
#9205=VECTOR('',#33718,10.);
#9206=VECTOR('',#33719,10.);
#9207=VECTOR('',#33726,10.);
#9208=VECTOR('',#33729,10.);
#9209=VECTOR('',#33730,10.);
#9210=VECTOR('',#33731,10.);
#9211=VECTOR('',#33734,10.);
#9212=VECTOR('',#33735,10.);
#9213=VECTOR('',#33736,10.);
#9214=VECTOR('',#33739,10.);
#9215=VECTOR('',#33740,10.);
#9216=VECTOR('',#33753,10.);
#9217=VECTOR('',#33754,10.);
#9218=VECTOR('',#33759,10.);
#9219=VECTOR('',#33762,10.);
#9220=VECTOR('',#33767,10.);
#9221=VECTOR('',#33770,10.);
#9222=VECTOR('',#33771,10.);
#9223=VECTOR('',#33772,10.);
#9224=VECTOR('',#33773,10.);
#9225=VECTOR('',#33778,10.);
#9226=VECTOR('',#33779,10.);
#9227=VECTOR('',#33780,10.);
#9228=VECTOR('',#33785,10.);
#9229=VECTOR('',#33788,10.);
#9230=VECTOR('',#33789,10.);
#9231=VECTOR('',#33790,10.);
#9232=VECTOR('',#33793,10.);
#9233=VECTOR('',#33794,10.);
#9234=VECTOR('',#33801,10.);
#9235=VECTOR('',#33802,10.);
#9236=VECTOR('',#33805,10.);
#9237=VECTOR('',#33806,10.);
#9238=VECTOR('',#33809,10.);
#9239=VECTOR('',#33812,10.);
#9240=VECTOR('',#33813,10.);
#9241=VECTOR('',#33814,10.);
#9242=VECTOR('',#33817,10.);
#9243=VECTOR('',#33822,10.);
#9244=VECTOR('',#33825,10.);
#9245=VECTOR('',#33828,10.);
#9246=VECTOR('',#33831,10.);
#9247=VECTOR('',#33834,10.);
#9248=VECTOR('',#33839,10.);
#9249=VECTOR('',#33842,10.);
#9250=VECTOR('',#33845,10.);
#9251=VECTOR('',#33846,10.);
#9252=VECTOR('',#33847,10.);
#9253=VECTOR('',#33848,10.);
#9254=VECTOR('',#33849,10.);
#9255=VECTOR('',#33850,10.);
#9256=VECTOR('',#33853,10.);
#9257=VECTOR('',#33856,10.);
#9258=VECTOR('',#33859,10.);
#9259=VECTOR('',#33862,10.);
#9260=VECTOR('',#33863,10.);
#9261=VECTOR('',#33866,10.);
#9262=VECTOR('',#33867,10.);
#9263=VECTOR('',#33870,10.);
#9264=VECTOR('',#33871,10.);
#9265=VECTOR('',#33872,10.);
#9266=VECTOR('',#33875,10.);
#9267=VECTOR('',#33876,10.);
#9268=VECTOR('',#33879,10.);
#9269=VECTOR('',#33880,10.);
#9270=VECTOR('',#33883,10.);
#9271=VECTOR('',#33888,10.);
#9272=VECTOR('',#33891,10.);
#9273=VECTOR('',#33894,10.);
#9274=VECTOR('',#33897,10.);
#9275=VECTOR('',#33898,10.);
#9276=VECTOR('',#33901,10.);
#9277=VECTOR('',#33906,10.);
#9278=VECTOR('',#33907,10.);
#9279=VECTOR('',#33910,10.);
#9280=VECTOR('',#33913,10.);
#9281=VECTOR('',#33920,10.);
#9282=VECTOR('',#33921,10.);
#9283=VECTOR('',#33924,10.);
#9284=VECTOR('',#33927,10.);
#9285=VECTOR('',#33930,10.);
#9286=VECTOR('',#33933,10.);
#9287=VECTOR('',#33936,10.);
#9288=VECTOR('',#33937,10.);
#9289=VECTOR('',#33944,10.);
#9290=VECTOR('',#33947,10.);
#9291=VECTOR('',#33948,10.);
#9292=VECTOR('',#33949,10.);
#9293=VECTOR('',#33950,10.);
#9294=VECTOR('',#33953,10.);
#9295=VECTOR('',#33954,10.);
#9296=VECTOR('',#33955,10.);
#9297=VECTOR('',#33956,10.);
#9298=VECTOR('',#33963,10.);
#9299=VECTOR('',#33964,10.);
#9300=VECTOR('',#33967,10.);
#9301=VECTOR('',#33968,10.);
#9302=VECTOR('',#33969,10.);
#9303=VECTOR('',#33972,10.);
#9304=VECTOR('',#33977,10.);
#9305=VECTOR('',#33978,10.);
#9306=VECTOR('',#33981,10.);
#9307=VECTOR('',#33982,10.);
#9308=VECTOR('',#33983,10.);
#9309=VECTOR('',#33988,10.);
#9310=VECTOR('',#33989,10.);
#9311=VECTOR('',#33992,10.);
#9312=VECTOR('',#33993,10.);
#9313=VECTOR('',#33998,10.);
#9314=VECTOR('',#34001,10.);
#9315=VECTOR('',#34004,10.);
#9316=VECTOR('',#34007,10.);
#9317=VECTOR('',#34010,10.);
#9318=VECTOR('',#34015,10.);
#9319=VECTOR('',#34018,10.);
#9320=VECTOR('',#34019,10.);
#9321=VECTOR('',#34020,10.);
#9322=VECTOR('',#34023,10.);
#9323=VECTOR('',#34026,10.);
#9324=VECTOR('',#34027,10.);
#9325=VECTOR('',#34028,10.);
#9326=VECTOR('',#34031,10.);
#9327=VECTOR('',#34034,10.);
#9328=VECTOR('',#34037,10.);
#9329=VECTOR('',#34038,10.);
#9330=VECTOR('',#34039,10.);
#9331=VECTOR('',#34040,10.);
#9332=VECTOR('',#34041,10.);
#9333=VECTOR('',#34042,10.);
#9334=VECTOR('',#34045,10.);
#9335=VECTOR('',#34048,10.);
#9336=VECTOR('',#34051,10.);
#9337=VECTOR('',#34056,10.);
#9338=VECTOR('',#34059,10.);
#9339=VECTOR('',#34060,10.);
#9340=VECTOR('',#34061,10.);
#9341=VECTOR('',#34064,10.);
#9342=VECTOR('',#34065,10.);
#9343=VECTOR('',#34068,10.);
#9344=VECTOR('',#34069,10.);
#9345=VECTOR('',#34072,10.);
#9346=VECTOR('',#34079,10.);
#9347=VECTOR('',#34080,10.);
#9348=VECTOR('',#34083,10.);
#9349=VECTOR('',#34084,10.);
#9350=VECTOR('',#34085,10.);
#9351=VECTOR('',#34088,10.);
#9352=VECTOR('',#34091,10.);
#9353=VECTOR('',#34098,10.);
#9354=VECTOR('',#34101,10.);
#9355=VECTOR('',#34104,10.);
#9356=VECTOR('',#34107,10.);
#9357=VECTOR('',#34108,10.);
#9358=VECTOR('',#34111,10.);
#9359=VECTOR('',#34114,10.);
#9360=VECTOR('',#34123,10.);
#9361=VECTOR('',#34126,10.);
#9362=VECTOR('',#34135,12.5);
#9363=VECTOR('',#34142,10.);
#9364=VECTOR('',#34145,10.);
#9365=VECTOR('',#34148,10.);
#9366=VECTOR('',#34149,10.);
#9367=VECTOR('',#34150,10.);
#9368=VECTOR('',#34153,10.);
#9369=VECTOR('',#34154,10.);
#9370=VECTOR('',#34155,10.);
#9371=VECTOR('',#34158,10.);
#9372=VECTOR('',#34159,10.);
#9373=VECTOR('',#34160,10.);
#9374=VECTOR('',#34163,10.);
#9375=VECTOR('',#34164,10.);
#9376=VECTOR('',#34165,10.);
#9377=VECTOR('',#34168,10.);
#9378=VECTOR('',#34169,10.);
#9379=VECTOR('',#34170,10.);
#9380=VECTOR('',#34177,10.);
#9381=VECTOR('',#34180,10.);
#9382=VECTOR('',#34181,10.);
#9383=VECTOR('',#34182,10.);
#9384=VECTOR('',#34185,10.);
#9385=VECTOR('',#34186,10.);
#9386=VECTOR('',#34187,10.);
#9387=VECTOR('',#34194,10.);
#9388=VECTOR('',#34201,10.);
#9389=VECTOR('',#34208,10.);
#9390=VECTOR('',#34211,10.);
#9391=VECTOR('',#34212,10.);
#9392=VECTOR('',#34213,10.);
#9393=VECTOR('',#34216,10.);
#9394=VECTOR('',#34217,10.);
#9395=VECTOR('',#34218,10.);
#9396=VECTOR('',#34221,10.);
#9397=VECTOR('',#34222,10.);
#9398=VECTOR('',#34223,10.);
#9399=VECTOR('',#34230,10.);
#9400=VECTOR('',#34233,10.);
#9401=VECTOR('',#34234,10.);
#9402=VECTOR('',#34235,10.);
#9403=VECTOR('',#34242,10.);
#9404=VECTOR('',#34245,10.);
#9405=VECTOR('',#34246,10.);
#9406=VECTOR('',#34247,10.);
#9407=VECTOR('',#34254,10.);
#9408=VECTOR('',#34257,10.);
#9409=VECTOR('',#34258,10.);
#9410=VECTOR('',#34259,10.);
#9411=VECTOR('',#34262,10.);
#9412=VECTOR('',#34263,10.);
#9413=VECTOR('',#34264,10.);
#9414=VECTOR('',#34267,10.);
#9415=VECTOR('',#34268,10.);
#9416=VECTOR('',#34269,10.);
#9417=VECTOR('',#34276,10.);
#9418=VECTOR('',#34279,10.);
#9419=VECTOR('',#34280,10.);
#9420=VECTOR('',#34281,10.);
#9421=VECTOR('',#34288,10.);
#9422=VECTOR('',#34291,10.);
#9423=VECTOR('',#34292,10.);
#9424=VECTOR('',#34293,10.);
#9425=VECTOR('',#34300,10.);
#9426=VECTOR('',#34303,10.);
#9427=VECTOR('',#34304,10.);
#9428=VECTOR('',#34305,10.);
#9429=VECTOR('',#34312,10.);
#9430=VECTOR('',#34315,10.);
#9431=VECTOR('',#34316,10.);
#9432=VECTOR('',#34317,10.);
#9433=VECTOR('',#34320,10.);
#9434=VECTOR('',#34321,10.);
#9435=VECTOR('',#34322,10.);
#9436=VECTOR('',#34325,10.);
#9437=VECTOR('',#34326,10.);
#9438=VECTOR('',#34327,10.);
#9439=VECTOR('',#34334,10.);
#9440=VECTOR('',#34337,10.);
#9441=VECTOR('',#34338,10.);
#9442=VECTOR('',#34339,10.);
#9443=VECTOR('',#34346,10.);
#9444=VECTOR('',#34349,10.);
#9445=VECTOR('',#34350,10.);
#9446=VECTOR('',#34351,10.);
#9447=VECTOR('',#34358,10.);
#9448=VECTOR('',#34361,10.);
#9449=VECTOR('',#34362,10.);
#9450=VECTOR('',#34363,10.);
#9451=VECTOR('',#34366,10.);
#9452=VECTOR('',#34367,10.);
#9453=VECTOR('',#34368,10.);
#9454=VECTOR('',#34371,9.99999999999999);
#9455=VECTOR('',#34372,9.99999999999999);
#9456=VECTOR('',#34373,10.);
#9457=VECTOR('',#34380,10.);
#9458=VECTOR('',#34387,10.);
#9459=VECTOR('',#34394,10.);
#9460=VECTOR('',#34397,9.99999999999999);
#9461=VECTOR('',#34398,9.99999999999999);
#9462=VECTOR('',#34399,10.);
#9463=VECTOR('',#34402,10.);
#9464=VECTOR('',#34403,10.);
#9465=VECTOR('',#34404,10.);
#9466=VECTOR('',#34411,10.);
#9467=VECTOR('',#34414,10.);
#9468=VECTOR('',#34415,10.);
#9469=VECTOR('',#34416,10.);
#9470=VECTOR('',#34419,10.);
#9471=VECTOR('',#34420,10.);
#9472=VECTOR('',#34421,10.);
#9473=VECTOR('',#34424,10.);
#9474=VECTOR('',#34425,10.);
#9475=VECTOR('',#34426,10.);
#9476=VECTOR('',#34429,10.);
#9477=VECTOR('',#34430,10.);
#9478=VECTOR('',#34431,10.);
#9479=VECTOR('',#34434,10.);
#9480=VECTOR('',#34435,10.);
#9481=VECTOR('',#34436,10.);
#9482=VECTOR('',#34443,10.);
#9483=VECTOR('',#34446,10.);
#9484=VECTOR('',#34447,10.);
#9485=VECTOR('',#34448,10.);
#9486=VECTOR('',#34451,9.99999999999999);
#9487=VECTOR('',#34452,9.99999999999999);
#9488=VECTOR('',#34453,10.);
#9489=VECTOR('',#34460,10.);
#9490=VECTOR('',#34467,10.);
#9491=VECTOR('',#34474,10.);
#9492=VECTOR('',#34477,9.99999999999999);
#9493=VECTOR('',#34478,9.99999999999999);
#9494=VECTOR('',#34479,10.);
#9495=VECTOR('',#34482,10.);
#9496=VECTOR('',#34483,10.);
#9497=VECTOR('',#34484,10.);
#9498=VECTOR('',#34487,10.);
#9499=VECTOR('',#34488,10.);
#9500=VECTOR('',#34489,10.);
#9501=VECTOR('',#34496,10.);
#9502=VECTOR('',#34499,10.);
#9503=VECTOR('',#34500,10.);
#9504=VECTOR('',#34501,10.);
#9505=VECTOR('',#34508,10.);
#9506=VECTOR('',#34511,10.);
#9507=VECTOR('',#34512,10.);
#9508=VECTOR('',#34513,10.);
#9509=VECTOR('',#34520,10.);
#9510=VECTOR('',#34523,10.);
#9511=VECTOR('',#34524,10.);
#9512=VECTOR('',#34525,10.);
#9513=VECTOR('',#34528,10.);
#9514=VECTOR('',#34529,10.);
#9515=VECTOR('',#34530,10.);
#9516=VECTOR('',#34533,10.);
#9517=VECTOR('',#34534,10.);
#9518=VECTOR('',#34535,10.);
#9519=VECTOR('',#34542,10.);
#9520=VECTOR('',#34545,10.);
#9521=VECTOR('',#34546,10.);
#9522=VECTOR('',#34547,10.);
#9523=VECTOR('',#34554,10.);
#9524=VECTOR('',#34557,10.);
#9525=VECTOR('',#34558,10.);
#9526=VECTOR('',#34559,10.);
#9527=VECTOR('',#34566,10.);
#9528=VECTOR('',#34569,10.);
#9529=VECTOR('',#34570,10.);
#9530=VECTOR('',#34571,10.);
#9531=VECTOR('',#34578,10.);
#9532=VECTOR('',#34581,10.);
#9533=VECTOR('',#34582,10.);
#9534=VECTOR('',#34583,10.);
#9535=VECTOR('',#34586,10.);
#9536=VECTOR('',#34587,10.);
#9537=VECTOR('',#34588,10.);
#9538=VECTOR('',#34591,10.);
#9539=VECTOR('',#34592,10.);
#9540=VECTOR('',#34593,10.);
#9541=VECTOR('',#34600,10.);
#9542=VECTOR('',#34603,10.);
#9543=VECTOR('',#34604,10.);
#9544=VECTOR('',#34605,10.);
#9545=VECTOR('',#34612,10.);
#9546=VECTOR('',#34615,10.);
#9547=VECTOR('',#34616,10.);
#9548=VECTOR('',#34617,10.);
#9549=VECTOR('',#34624,10.);
#9550=VECTOR('',#34627,10.);
#9551=VECTOR('',#34628,10.);
#9552=VECTOR('',#34629,10.);
#9553=VECTOR('',#34632,10.);
#9554=VECTOR('',#34633,10.);
#9555=VECTOR('',#34634,10.);
#9556=VECTOR('',#34637,10.);
#9557=VECTOR('',#34638,10.);
#9558=VECTOR('',#34639,10.);
#9559=VECTOR('',#34646,10.);
#9560=VECTOR('',#34653,10.);
#9561=VECTOR('',#34660,10.);
#9562=VECTOR('',#34663,10.);
#9563=VECTOR('',#34664,10.);
#9564=VECTOR('',#34665,10.);
#9565=VECTOR('',#34668,10.);
#9566=VECTOR('',#34669,10.);
#9567=VECTOR('',#34678,5.099);
#9568=VECTOR('',#34683,5.099);
#9569=VECTOR('',#34686,5.099);
#9570=VECTOR('',#34689,5.099);
#9571=VECTOR('',#34692,5.099);
#9572=VECTOR('',#34697,5.099);
#9573=VECTOR('',#34700,5.099);
#9574=VECTOR('',#34703,5.099);
#9575=VECTOR('',#34706,2.55999999999999);
#9576=VECTOR('',#34711,2.55999999999999);
#9577=VECTOR('',#34714,2.55999999999999);
#9578=VECTOR('',#34717,2.55999999999999);
#9579=VECTOR('',#34720,2.55999999999999);
#9580=VECTOR('',#34723,2.55999999999999);
#9581=VECTOR('',#34726,2.55999999999999);
#9582=VECTOR('',#34729,2.55999999999999);
#9583=VECTOR('',#34732,2.55999999999999);
#9584=VECTOR('',#34735,2.55999999999999);
#9585=VECTOR('',#34738,2.55999999999999);
#9586=VECTOR('',#34741,2.55999999999999);
#9587=VECTOR('',#34744,2.55999999999999);
#9588=VECTOR('',#34747,2.55999999999999);
#9589=VECTOR('',#34750,2.55999999999999);
#9590=VECTOR('',#34753,2.55999999999999);
#9591=VECTOR('',#34756,2.55999999999999);
#9592=VECTOR('',#34759,2.55999999999999);
#9593=VECTOR('',#34762,2.55999999999999);
#9594=VECTOR('',#34765,2.55999999999999);
#9595=VECTOR('',#34768,2.55999999999999);
#9596=VECTOR('',#34771,2.55999999999999);
#9597=VECTOR('',#34774,2.55999999999999);
#9598=VECTOR('',#34777,2.55999999999999);
#9599=VECTOR('',#34780,2.55999999999999);
#9600=VECTOR('',#34783,2.55999999999999);
#9601=VECTOR('',#34786,2.55999999999999);
#9602=VECTOR('',#34789,2.56);
#9603=VECTOR('',#34794,2.56);
#9604=VECTOR('',#34797,2.56);
#9605=VECTOR('',#34800,2.56);
#9606=VECTOR('',#34803,2.56);
#9607=VECTOR('',#34806,2.56);
#9608=VECTOR('',#34809,2.56);
#9609=VECTOR('',#34812,2.56);
#9610=VECTOR('',#34815,2.56);
#9611=VECTOR('',#34818,2.56);
#9612=VECTOR('',#34821,2.56);
#9613=VECTOR('',#34824,2.56);
#9614=VECTOR('',#34827,2.56);
#9615=VECTOR('',#34830,2.56);
#9616=VECTOR('',#34833,2.56);
#9617=VECTOR('',#34836,2.56);
#9618=VECTOR('',#34839,2.56);
#9619=VECTOR('',#34842,2.56);
#9620=VECTOR('',#34845,2.56);
#9621=VECTOR('',#34848,2.56);
#9622=VECTOR('',#34851,2.56);
#9623=VECTOR('',#34854,2.56);
#9624=VECTOR('',#34857,2.56);
#9625=VECTOR('',#34860,2.56);
#9626=VECTOR('',#34863,2.56);
#9627=VECTOR('',#34866,2.56);
#9628=VECTOR('',#34869,2.56);
#9629=VECTOR('',#34872,2.56);
#9630=VECTOR('',#34877,2.56);
#9631=VECTOR('',#34880,2.56);
#9632=VECTOR('',#34883,2.56);
#9633=VECTOR('',#34886,2.56);
#9634=VECTOR('',#34889,2.56);
#9635=VECTOR('',#34892,2.56);
#9636=VECTOR('',#34895,2.56);
#9637=VECTOR('',#34898,2.56);
#9638=VECTOR('',#34901,2.56);
#9639=VECTOR('',#34904,2.56);
#9640=VECTOR('',#34907,2.56);
#9641=VECTOR('',#34910,2.56);
#9642=VECTOR('',#34913,2.56);
#9643=VECTOR('',#34916,2.56);
#9644=VECTOR('',#34919,2.56);
#9645=VECTOR('',#34922,2.56);
#9646=VECTOR('',#34925,2.56);
#9647=VECTOR('',#34928,2.56);
#9648=VECTOR('',#34931,2.56);
#9649=VECTOR('',#34934,2.56);
#9650=VECTOR('',#34937,2.56);
#9651=VECTOR('',#34940,2.56);
#9652=VECTOR('',#34943,2.56);
#9653=VECTOR('',#34946,2.56);
#9654=VECTOR('',#34949,2.56);
#9655=VECTOR('',#34952,2.56);
#9656=VECTOR('',#34955,2.56);
#9657=VECTOR('',#34960,2.56);
#9658=VECTOR('',#34963,2.56);
#9659=VECTOR('',#34966,2.56);
#9660=VECTOR('',#34969,2.56);
#9661=VECTOR('',#34972,2.56);
#9662=VECTOR('',#34975,2.56);
#9663=VECTOR('',#34978,2.56);
#9664=VECTOR('',#34981,2.56);
#9665=VECTOR('',#34984,2.56);
#9666=VECTOR('',#34987,2.56);
#9667=VECTOR('',#34990,2.56);
#9668=VECTOR('',#34993,2.56);
#9669=VECTOR('',#34996,2.56);
#9670=VECTOR('',#34999,2.56);
#9671=VECTOR('',#35002,2.56);
#9672=VECTOR('',#35005,2.56);
#9673=VECTOR('',#35008,2.56);
#9674=VECTOR('',#35011,2.56);
#9675=VECTOR('',#35014,2.56);
#9676=VECTOR('',#35017,2.56);
#9677=VECTOR('',#35020,2.56);
#9678=VECTOR('',#35023,2.56);
#9679=VECTOR('',#35026,2.56);
#9680=VECTOR('',#35029,2.56);
#9681=VECTOR('',#35032,2.56);
#9682=VECTOR('',#35035,2.56);
#9683=VECTOR('',#35038,4.263);
#9684=VECTOR('',#35043,4.263);
#9685=VECTOR('',#35048,4.263);
#9686=VECTOR('',#35051,4.263);
#9687=VECTOR('',#35054,4.263);
#9688=VECTOR('',#35059,4.263);
#9689=VECTOR('',#35062,4.263);
#9690=VECTOR('',#35065,4.263);
#9691=VECTOR('',#35070,2.117);
#9692=VECTOR('',#35075,2.117);
#9693=VECTOR('',#35078,2.117);
#9694=VECTOR('',#35081,2.117);
#9695=VECTOR('',#35084,2.117);
#9696=VECTOR('',#35087,2.117);
#9697=VECTOR('',#35090,2.117);
#9698=VECTOR('',#35093,2.117);
#9699=VECTOR('',#35096,2.117);
#9700=VECTOR('',#35099,2.117);
#9701=VECTOR('',#35102,2.117);
#9702=VECTOR('',#35105,2.117);
#9703=VECTOR('',#35108,2.117);
#9704=VECTOR('',#35111,2.117);
#9705=VECTOR('',#35114,2.117);
#9706=VECTOR('',#35117,2.117);
#9707=VECTOR('',#35120,2.117);
#9708=VECTOR('',#35123,2.117);
#9709=VECTOR('',#35126,2.117);
#9710=VECTOR('',#35129,2.117);
#9711=VECTOR('',#35132,2.117);
#9712=VECTOR('',#35135,2.117);
#9713=VECTOR('',#35138,2.117);
#9714=VECTOR('',#35141,2.117);
#9715=VECTOR('',#35144,2.117);
#9716=VECTOR('',#35147,2.117);
#9717=VECTOR('',#35150,2.117);
#9718=VECTOR('',#35153,2.117);
#9719=VECTOR('',#35158,2.117);
#9720=VECTOR('',#35161,2.117);
#9721=VECTOR('',#35164,2.117);
#9722=VECTOR('',#35167,2.117);
#9723=VECTOR('',#35170,2.117);
#9724=VECTOR('',#35173,2.117);
#9725=VECTOR('',#35176,2.117);
#9726=VECTOR('',#35179,2.117);
#9727=VECTOR('',#35182,2.117);
#9728=VECTOR('',#35185,2.117);
#9729=VECTOR('',#35188,2.117);
#9730=VECTOR('',#35191,2.117);
#9731=VECTOR('',#35194,2.117);
#9732=VECTOR('',#35197,2.117);
#9733=VECTOR('',#35200,2.117);
#9734=VECTOR('',#35203,2.117);
#9735=VECTOR('',#35206,2.117);
#9736=VECTOR('',#35209,2.117);
#9737=VECTOR('',#35212,2.117);
#9738=VECTOR('',#35215,2.117);
#9739=VECTOR('',#35218,2.117);
#9740=VECTOR('',#35221,2.117);
#9741=VECTOR('',#35224,2.117);
#9742=VECTOR('',#35227,2.117);
#9743=VECTOR('',#35230,2.117);
#9744=VECTOR('',#35233,2.117);
#9745=VECTOR('',#35236,2.117);
#9746=VECTOR('',#35241,2.117);
#9747=VECTOR('',#35244,2.117);
#9748=VECTOR('',#35247,2.117);
#9749=VECTOR('',#35250,2.117);
#9750=VECTOR('',#35253,2.117);
#9751=VECTOR('',#35256,2.117);
#9752=VECTOR('',#35259,2.117);
#9753=VECTOR('',#35262,2.117);
#9754=VECTOR('',#35265,2.117);
#9755=VECTOR('',#35268,2.117);
#9756=VECTOR('',#35271,2.117);
#9757=VECTOR('',#35274,2.117);
#9758=VECTOR('',#35277,2.117);
#9759=VECTOR('',#35280,2.117);
#9760=VECTOR('',#35283,2.117);
#9761=VECTOR('',#35286,2.117);
#9762=VECTOR('',#35289,2.117);
#9763=VECTOR('',#35292,2.117);
#9764=VECTOR('',#35295,2.117);
#9765=VECTOR('',#35298,2.117);
#9766=VECTOR('',#35301,2.117);
#9767=VECTOR('',#35304,2.117);
#9768=VECTOR('',#35307,2.117);
#9769=VECTOR('',#35310,2.117);
#9770=VECTOR('',#35313,2.117);
#9771=VECTOR('',#35316,2.117);
#9772=VECTOR('',#35319,2.117);
#9773=VECTOR('',#35324,2.117);
#9774=VECTOR('',#35327,2.117);
#9775=VECTOR('',#35330,2.117);
#9776=VECTOR('',#35333,2.117);
#9777=VECTOR('',#35336,2.117);
#9778=VECTOR('',#35339,2.117);
#9779=VECTOR('',#35342,2.117);
#9780=VECTOR('',#35345,2.117);
#9781=VECTOR('',#35348,2.117);
#9782=VECTOR('',#35351,2.117);
#9783=VECTOR('',#35354,2.117);
#9784=VECTOR('',#35357,2.117);
#9785=VECTOR('',#35360,2.117);
#9786=VECTOR('',#35363,2.117);
#9787=VECTOR('',#35366,2.117);
#9788=VECTOR('',#35369,2.117);
#9789=VECTOR('',#35372,2.117);
#9790=VECTOR('',#35375,2.117);
#9791=VECTOR('',#35378,2.117);
#9792=VECTOR('',#35381,2.117);
#9793=VECTOR('',#35384,2.117);
#9794=VECTOR('',#35387,2.117);
#9795=VECTOR('',#35390,2.117);
#9796=VECTOR('',#35393,2.117);
#9797=VECTOR('',#35396,2.117);
#9798=VECTOR('',#35399,2.117);
#9799=VECTOR('',#35452,4.);
#9800=VECTOR('',#35461,10.);
#9801=VECTOR('',#35464,10.);
#9802=VECTOR('',#35467,10.);
#9803=VECTOR('',#35470,10.);
#9804=VECTOR('',#35471,10.);
#9805=VECTOR('',#35476,4.);
#9806=VECTOR('',#35485,10.);
#9807=VECTOR('',#35488,10.);
#9808=VECTOR('',#35491,10.);
#9809=VECTOR('',#35494,10.);
#9810=VECTOR('',#35495,10.);
#9811=VECTOR('',#35500,5.);
#9812=VECTOR('',#35507,10.);
#9813=VECTOR('',#35508,10.);
#9814=VECTOR('',#35509,10.);
#9815=VECTOR('',#35512,10.);
#9816=VECTOR('',#35513,10.);
#9817=VECTOR('',#35514,10.);
#9818=VECTOR('',#35515,10.);
#9819=VECTOR('',#35518,10.);
#9820=VECTOR('',#35519,10.);
#9821=VECTOR('',#35520,10.);
#9822=VECTOR('',#35525,10.);
#9823=VECTOR('',#35528,10.);
#9824=VECTOR('',#35531,10.);
#9825=VECTOR('',#35534,10.);
#9826=VECTOR('',#35535,10.);
#9827=VECTOR('',#35536,10.);
#9828=VECTOR('',#35537,10.);
#9829=VECTOR('',#35538,10.);
#9830=VECTOR('',#35541,10.);
#9831=VECTOR('',#35544,10.);
#9832=VECTOR('',#35545,10.);
#9833=VECTOR('',#35546,10.);
#9834=VECTOR('',#35547,10.);
#9835=VECTOR('',#35548,10.);
#9836=VECTOR('',#35551,10.);
#9837=VECTOR('',#35554,10.);
#9838=VECTOR('',#35557,10.);
#9839=VECTOR('',#35560,10.);
#9840=VECTOR('',#35567,10.);
#9841=VECTOR('',#35568,10.);
#9842=VECTOR('',#35569,10.);
#9843=VECTOR('',#35570,10.);
#9844=VECTOR('',#35573,10.);
#9845=VECTOR('',#35574,10.);
#9846=VECTOR('',#35575,10.);
#9847=VECTOR('',#35578,10.);
#9848=VECTOR('',#35579,10.);
#9849=VECTOR('',#35580,10.);
#9850=VECTOR('',#35583,10.);
#9851=VECTOR('',#35584,10.);
#9852=VECTOR('',#35585,10.);
#9853=VECTOR('',#35588,10.);
#9854=VECTOR('',#35589,10.);
#9855=VECTOR('',#35590,10.);
#9856=VECTOR('',#35593,10.);
#9857=VECTOR('',#35594,10.);
#9858=VECTOR('',#35595,10.);
#9859=VECTOR('',#35598,10.);
#9860=VECTOR('',#35599,10.);
#9861=VECTOR('',#35604,3.);
#9862=VECTOR('',#35613,10.);
#9863=VECTOR('',#35616,10.);
#9864=VECTOR('',#35619,10.);
#9865=VECTOR('',#35620,10.);
#9866=VECTOR('',#35621,10.);
#9867=VECTOR('',#35626,10.);
#9868=VECTOR('',#35631,10.);
#9869=VECTOR('',#35632,10.);
#9870=VECTOR('',#35635,10.);
#9871=VECTOR('',#35636,10.);
#9872=VECTOR('',#35645,10.);
#9873=VECTOR('',#35646,10.);
#9874=VECTOR('',#35647,10.);
#9875=VECTOR('',#35648,10.);
#9876=VECTOR('',#35651,10.);
#9877=VECTOR('',#35652,10.);
#9878=VECTOR('',#35653,10.);
#9879=VECTOR('',#35656,10.);
#9880=VECTOR('',#35657,10.);
#9881=VECTOR('',#35658,10.);
#9882=VECTOR('',#35661,10.);
#9883=VECTOR('',#35662,10.);
#9884=VECTOR('',#35663,10.);
#9885=VECTOR('',#35666,10.);
#9886=VECTOR('',#35667,10.);
#9887=VECTOR('',#35668,10.);
#9888=VECTOR('',#35671,10.);
#9889=VECTOR('',#35672,10.);
#9890=VECTOR('',#35673,10.);
#9891=VECTOR('',#35676,10.);
#9892=VECTOR('',#35677,10.);
#9893=VECTOR('',#35682,3.);
#9894=VECTOR('',#35693,4.);
#9895=VECTOR('',#35702,5.);
#9896=VECTOR('',#35711,10.);
#9897=VECTOR('',#35714,10.);
#9898=VECTOR('',#35717,10.);
#9899=VECTOR('',#35718,10.);
#9900=VECTOR('',#35719,10.);
#9901=VECTOR('',#35726,10.);
#9902=VECTOR('',#35729,10.);
#9903=VECTOR('',#35730,10.);
#9904=VECTOR('',#35733,10.);
#9905=VECTOR('',#35734,10.);
#9906=VECTOR('',#35743,10.);
#9907=VECTOR('',#35744,10.);
#9908=VECTOR('',#35745,10.);
#9909=VECTOR('',#35746,10.);
#9910=VECTOR('',#35749,10.);
#9911=VECTOR('',#35750,10.);
#9912=VECTOR('',#35751,10.);
#9913=VECTOR('',#35754,10.);
#9914=VECTOR('',#35755,10.);
#9915=VECTOR('',#35756,10.);
#9916=VECTOR('',#35759,10.);
#9917=VECTOR('',#35760,10.);
#9918=VECTOR('',#35761,10.);
#9919=VECTOR('',#35764,10.);
#9920=VECTOR('',#35765,10.);
#9921=VECTOR('',#35766,10.);
#9922=VECTOR('',#35769,10.);
#9923=VECTOR('',#35770,10.);
#9924=VECTOR('',#35771,10.);
#9925=VECTOR('',#35774,10.);
#9926=VECTOR('',#35775,10.);
#9927=VECTOR('',#35780,3.);
#9928=VECTOR('',#35787,10.);
#9929=VECTOR('',#35788,10.);
#9930=VECTOR('',#35789,10.);
#9931=VECTOR('',#35790,10.);
#9932=VECTOR('',#35793,10.);
#9933=VECTOR('',#35794,10.);
#9934=VECTOR('',#35795,10.);
#9935=VECTOR('',#35798,10.);
#9936=VECTOR('',#35799,10.);
#9937=VECTOR('',#35800,10.);
#9938=VECTOR('',#35803,10.);
#9939=VECTOR('',#35804,10.);
#9940=VECTOR('',#35805,10.);
#9941=VECTOR('',#35808,10.);
#9942=VECTOR('',#35809,10.);
#9943=VECTOR('',#35810,10.);
#9944=VECTOR('',#35813,10.);
#9945=VECTOR('',#35814,10.);
#9946=VECTOR('',#35815,10.);
#9947=VECTOR('',#35818,10.);
#9948=VECTOR('',#35819,10.);
#9949=VECTOR('',#35824,3.);
#9950=VECTOR('',#35835,10.);
#9951=VECTOR('',#35836,10.);
#9952=VECTOR('',#35837,10.);
#9953=VECTOR('',#35844,5.);
#9954=VECTOR('',#35851,4.);
#9955=VECTOR('',#35858,2.5);
#9956=VECTOR('',#35865,2.5);
#9957=VECTOR('',#35870,10.);
#9958=VECTOR('',#35871,10.);
#9959=VECTOR('',#35880,10.);
#9960=VECTOR('',#35883,10.);
#9961=VECTOR('',#35884,10.);
#9962=VECTOR('',#35889,10.);
#9963=VECTOR('',#35892,10.);
#9964=VECTOR('',#35893,10.);
#9965=VECTOR('',#35898,10.);
#9966=VECTOR('',#35901,10.);
#9967=VECTOR('',#35902,10.);
#9968=VECTOR('',#35911,10.);
#9969=VECTOR('',#35914,10.);
#9970=VECTOR('',#35915,10.);
#9971=VECTOR('',#35920,10.);
#9972=VECTOR('',#35923,10.);
#9973=VECTOR('',#35924,10.);
#9974=VECTOR('',#35929,10.);
#9975=VECTOR('',#35932,10.);
#9976=VECTOR('',#35933,10.);
#9977=VECTOR('',#35938,10.);
#9978=VECTOR('',#35941,10.);
#9979=VECTOR('',#35942,10.);
#9980=VECTOR('',#35947,10.);
#9981=VECTOR('',#35950,10.);
#9982=VECTOR('',#35951,10.);
#9983=VECTOR('',#35956,10.);
#9984=VECTOR('',#35959,10.);
#9985=VECTOR('',#35960,10.);
#9986=VERTEX_POINT('',#35984);
#9987=VERTEX_POINT('',#35985);
#9988=VERTEX_POINT('',#35987);
#9989=VERTEX_POINT('',#35989);
#9990=VERTEX_POINT('',#35991);
#9991=VERTEX_POINT('',#35993);
#9992=VERTEX_POINT('',#35995);
#9993=VERTEX_POINT('',#35997);
#9994=VERTEX_POINT('',#35999);
#9995=VERTEX_POINT('',#36001);
#9996=VERTEX_POINT('',#36003);
#9997=VERTEX_POINT('',#36005);
#9998=VERTEX_POINT('',#36007);
#9999=VERTEX_POINT('',#36009);
#10000=VERTEX_POINT('',#36011);
#10001=VERTEX_POINT('',#36013);
#10002=VERTEX_POINT('',#36015);
#10003=VERTEX_POINT('',#36017);
#10004=VERTEX_POINT('',#36019);
#10005=VERTEX_POINT('',#36021);
#10006=VERTEX_POINT('',#36023);
#10007=VERTEX_POINT('',#36025);
#10008=VERTEX_POINT('',#36027);
#10009=VERTEX_POINT('',#36029);
#10010=VERTEX_POINT('',#36031);
#10011=VERTEX_POINT('',#36035);
#10012=VERTEX_POINT('',#36037);
#10013=VERTEX_POINT('',#36041);
#10014=VERTEX_POINT('',#36045);
#10015=VERTEX_POINT('',#36049);
#10016=VERTEX_POINT('',#36053);
#10017=VERTEX_POINT('',#36057);
#10018=VERTEX_POINT('',#36061);
#10019=VERTEX_POINT('',#36065);
#10020=VERTEX_POINT('',#36069);
#10021=VERTEX_POINT('',#36073);
#10022=VERTEX_POINT('',#36077);
#10023=VERTEX_POINT('',#36081);
#10024=VERTEX_POINT('',#36085);
#10025=VERTEX_POINT('',#36089);
#10026=VERTEX_POINT('',#36093);
#10027=VERTEX_POINT('',#36097);
#10028=VERTEX_POINT('',#36101);
#10029=VERTEX_POINT('',#36105);
#10030=VERTEX_POINT('',#36109);
#10031=VERTEX_POINT('',#36113);
#10032=VERTEX_POINT('',#36117);
#10033=VERTEX_POINT('',#36121);
#10034=VERTEX_POINT('',#36125);
#10035=VERTEX_POINT('',#36129);
#10036=VERTEX_POINT('',#36137);
#10037=VERTEX_POINT('',#36138);
#10038=VERTEX_POINT('',#36140);
#10039=VERTEX_POINT('',#36142);
#10040=VERTEX_POINT('',#36144);
#10041=VERTEX_POINT('',#36146);
#10042=VERTEX_POINT('',#36148);
#10043=VERTEX_POINT('',#36150);
#10044=VERTEX_POINT('',#36152);
#10045=VERTEX_POINT('',#36154);
#10046=VERTEX_POINT('',#36156);
#10047=VERTEX_POINT('',#36158);
#10048=VERTEX_POINT('',#36160);
#10049=VERTEX_POINT('',#36162);
#10050=VERTEX_POINT('',#36164);
#10051=VERTEX_POINT('',#36166);
#10052=VERTEX_POINT('',#36168);
#10053=VERTEX_POINT('',#36170);
#10054=VERTEX_POINT('',#36172);
#10055=VERTEX_POINT('',#36174);
#10056=VERTEX_POINT('',#36176);
#10057=VERTEX_POINT('',#36178);
#10058=VERTEX_POINT('',#36180);
#10059=VERTEX_POINT('',#36182);
#10060=VERTEX_POINT('',#36184);
#10061=VERTEX_POINT('',#36186);
#10062=VERTEX_POINT('',#36190);
#10063=VERTEX_POINT('',#36192);
#10064=VERTEX_POINT('',#36196);
#10065=VERTEX_POINT('',#36200);
#10066=VERTEX_POINT('',#36204);
#10067=VERTEX_POINT('',#36208);
#10068=VERTEX_POINT('',#36212);
#10069=VERTEX_POINT('',#36216);
#10070=VERTEX_POINT('',#36220);
#10071=VERTEX_POINT('',#36224);
#10072=VERTEX_POINT('',#36228);
#10073=VERTEX_POINT('',#36232);
#10074=VERTEX_POINT('',#36236);
#10075=VERTEX_POINT('',#36240);
#10076=VERTEX_POINT('',#36244);
#10077=VERTEX_POINT('',#36248);
#10078=VERTEX_POINT('',#36252);
#10079=VERTEX_POINT('',#36256);
#10080=VERTEX_POINT('',#36260);
#10081=VERTEX_POINT('',#36264);
#10082=VERTEX_POINT('',#36268);
#10083=VERTEX_POINT('',#36272);
#10084=VERTEX_POINT('',#36276);
#10085=VERTEX_POINT('',#36280);
#10086=VERTEX_POINT('',#36284);
#10087=VERTEX_POINT('',#36288);
#10088=VERTEX_POINT('',#36296);
#10089=VERTEX_POINT('',#36297);
#10090=VERTEX_POINT('',#36299);
#10091=VERTEX_POINT('',#36306);
#10092=VERTEX_POINT('',#36382);
#10093=VERTEX_POINT('',#36383);
#10094=VERTEX_POINT('',#36385);
#10095=VERTEX_POINT('',#36546);
#10096=VERTEX_POINT('',#36645);
#10097=VERTEX_POINT('',#36646);
#10098=VERTEX_POINT('',#36648);
#10099=VERTEX_POINT('',#36885);
#10100=VERTEX_POINT('',#37043);
#10101=VERTEX_POINT('',#37044);
#10102=VERTEX_POINT('',#37046);
#10103=VERTEX_POINT('',#37132);
#10104=VERTEX_POINT('',#37139);
#10105=VERTEX_POINT('',#37141);
#10106=VERTEX_POINT('',#37219);
#10107=VERTEX_POINT('',#37220);
#10108=VERTEX_POINT('',#37222);
#10109=VERTEX_POINT('',#37229);
#10110=VERTEX_POINT('',#37305);
#10111=VERTEX_POINT('',#37306);
#10112=VERTEX_POINT('',#37308);
#10113=VERTEX_POINT('',#37469);
#10114=VERTEX_POINT('',#37568);
#10115=VERTEX_POINT('',#37569);
#10116=VERTEX_POINT('',#37571);
#10117=VERTEX_POINT('',#37808);
#10118=VERTEX_POINT('',#37966);
#10119=VERTEX_POINT('',#37967);
#10120=VERTEX_POINT('',#37969);
#10121=VERTEX_POINT('',#38055);
#10122=VERTEX_POINT('',#38062);
#10123=VERTEX_POINT('',#38064);
#10124=VERTEX_POINT('',#38142);
#10125=VERTEX_POINT('',#38143);
#10126=VERTEX_POINT('',#38145);
#10127=VERTEX_POINT('',#38154);
#10128=VERTEX_POINT('',#38160);
#10129=VERTEX_POINT('',#38162);
#10130=VERTEX_POINT('',#38230);
#10131=VERTEX_POINT('',#38231);
#10132=VERTEX_POINT('',#38233);
#10133=VERTEX_POINT('',#38364);
#10134=VERTEX_POINT('',#38381);
#10135=VERTEX_POINT('',#38382);
#10136=VERTEX_POINT('',#38384);
#10137=VERTEX_POINT('',#38582);
#10138=VERTEX_POINT('',#38714);
#10139=VERTEX_POINT('',#38715);
#10140=VERTEX_POINT('',#38717);
#10141=VERTEX_POINT('',#38796);
#10142=VERTEX_POINT('',#38995);
#10143=VERTEX_POINT('',#38996);
#10144=VERTEX_POINT('',#38998);
#10145=VERTEX_POINT('',#39132);
#10146=VERTEX_POINT('',#39331);
#10147=VERTEX_POINT('',#39332);
#10148=VERTEX_POINT('',#39334);
#10149=VERTEX_POINT('',#39413);
#10150=VERTEX_POINT('',#39493);
#10151=VERTEX_POINT('',#39494);
#10152=VERTEX_POINT('',#39496);
#10153=VERTEX_POINT('',#39631);
#10154=VERTEX_POINT('',#39763);
#10155=VERTEX_POINT('',#39764);
#10156=VERTEX_POINT('',#39766);
#10157=VERTEX_POINT('',#39958);
#10158=VERTEX_POINT('',#40038);
#10159=VERTEX_POINT('',#40039);
#10160=VERTEX_POINT('',#40041);
#10161=VERTEX_POINT('',#40236);
#10162=VERTEX_POINT('',#40372);
#10163=VERTEX_POINT('',#40373);
#10164=VERTEX_POINT('',#40375);
#10165=VERTEX_POINT('',#40454);
#10166=VERTEX_POINT('',#40534);
#10167=VERTEX_POINT('',#40535);
#10168=VERTEX_POINT('',#40537);
#10169=VERTEX_POINT('',#40669);
#10170=VERTEX_POINT('',#40801);
#10171=VERTEX_POINT('',#40802);
#10172=VERTEX_POINT('',#40804);
#10173=VERTEX_POINT('',#40999);
#10174=VERTEX_POINT('',#41079);
#10175=VERTEX_POINT('',#41080);
#10176=VERTEX_POINT('',#41082);
#10177=VERTEX_POINT('',#41280);
#10178=VERTEX_POINT('',#41412);
#10179=VERTEX_POINT('',#41413);
#10180=VERTEX_POINT('',#41415);
#10181=VERTEX_POINT('',#41494);
#10182=VERTEX_POINT('',#41577);
#10183=VERTEX_POINT('',#41578);
#10184=VERTEX_POINT('',#41580);
#10185=VERTEX_POINT('',#41714);
#10186=VERTEX_POINT('',#41846);
#10187=VERTEX_POINT('',#41847);
#10188=VERTEX_POINT('',#41849);
#10189=VERTEX_POINT('',#41928);
#10190=VERTEX_POINT('',#42127);
#10191=VERTEX_POINT('',#42128);
#10192=VERTEX_POINT('',#42130);
#10193=VERTEX_POINT('',#42264);
#10194=VERTEX_POINT('',#42460);
#10195=VERTEX_POINT('',#42461);
#10196=VERTEX_POINT('',#42463);
#10197=VERTEX_POINT('',#42539);
#10198=VERTEX_POINT('',#42619);
#10199=VERTEX_POINT('',#42620);
#10200=VERTEX_POINT('',#42622);
#10201=VERTEX_POINT('',#42753);
#10202=VERTEX_POINT('',#42889);
#10203=VERTEX_POINT('',#42890);
#10204=VERTEX_POINT('',#42892);
#10205=VERTEX_POINT('',#42971);
#10206=VERTEX_POINT('',#43170);
#10207=VERTEX_POINT('',#43171);
#10208=VERTEX_POINT('',#43173);
#10209=VERTEX_POINT('',#43305);
#10210=VERTEX_POINT('',#43501);
#10211=VERTEX_POINT('',#43502);
#10212=VERTEX_POINT('',#43504);
#10213=VERTEX_POINT('',#43583);
#10214=VERTEX_POINT('',#43664);
#10215=VERTEX_POINT('',#43665);
#10216=VERTEX_POINT('',#43667);
#10217=VERTEX_POINT('',#43798);
#10218=VERTEX_POINT('',#43930);
#10219=VERTEX_POINT('',#43931);
#10220=VERTEX_POINT('',#43933);
#10221=VERTEX_POINT('',#44131);
#10222=VERTEX_POINT('',#44211);
#10223=VERTEX_POINT('',#44212);
#10224=VERTEX_POINT('',#44214);
#10225=VERTEX_POINT('',#44412);
#10226=VERTEX_POINT('',#44544);
#10227=VERTEX_POINT('',#44545);
#10228=VERTEX_POINT('',#44547);
#10229=VERTEX_POINT('',#44626);
#10230=VERTEX_POINT('',#44825);
#10231=VERTEX_POINT('',#44826);
#10232=VERTEX_POINT('',#44828);
#10233=VERTEX_POINT('',#44835);
#10234=VERTEX_POINT('',#44841);
#10235=VERTEX_POINT('',#44843);
#10236=VERTEX_POINT('',#44910);
#10237=VERTEX_POINT('',#44911);
#10238=VERTEX_POINT('',#44913);
#10239=VERTEX_POINT('',#44922);
#10240=VERTEX_POINT('',#44928);
#10241=VERTEX_POINT('',#44930);
#10242=VERTEX_POINT('',#44998);
#10243=VERTEX_POINT('',#44999);
#10244=VERTEX_POINT('',#45001);
#10245=VERTEX_POINT('',#45132);
#10246=VERTEX_POINT('',#45149);
#10247=VERTEX_POINT('',#45150);
#10248=VERTEX_POINT('',#45152);
#10249=VERTEX_POINT('',#45350);
#10250=VERTEX_POINT('',#45482);
#10251=VERTEX_POINT('',#45483);
#10252=VERTEX_POINT('',#45485);
#10253=VERTEX_POINT('',#45564);
#10254=VERTEX_POINT('',#45763);
#10255=VERTEX_POINT('',#45764);
#10256=VERTEX_POINT('',#45766);
#10257=VERTEX_POINT('',#45900);
#10258=VERTEX_POINT('',#46099);
#10259=VERTEX_POINT('',#46100);
#10260=VERTEX_POINT('',#46102);
#10261=VERTEX_POINT('',#46181);
#10262=VERTEX_POINT('',#46261);
#10263=VERTEX_POINT('',#46262);
#10264=VERTEX_POINT('',#46264);
#10265=VERTEX_POINT('',#46399);
#10266=VERTEX_POINT('',#46531);
#10267=VERTEX_POINT('',#46532);
#10268=VERTEX_POINT('',#46534);
#10269=VERTEX_POINT('',#46726);
#10270=VERTEX_POINT('',#46806);
#10271=VERTEX_POINT('',#46807);
#10272=VERTEX_POINT('',#46809);
#10273=VERTEX_POINT('',#47004);
#10274=VERTEX_POINT('',#47140);
#10275=VERTEX_POINT('',#47141);
#10276=VERTEX_POINT('',#47143);
#10277=VERTEX_POINT('',#47222);
#10278=VERTEX_POINT('',#47302);
#10279=VERTEX_POINT('',#47303);
#10280=VERTEX_POINT('',#47305);
#10281=VERTEX_POINT('',#47437);
#10282=VERTEX_POINT('',#47569);
#10283=VERTEX_POINT('',#47570);
#10284=VERTEX_POINT('',#47572);
#10285=VERTEX_POINT('',#47767);
#10286=VERTEX_POINT('',#47847);
#10287=VERTEX_POINT('',#47848);
#10288=VERTEX_POINT('',#47850);
#10289=VERTEX_POINT('',#48048);
#10290=VERTEX_POINT('',#48180);
#10291=VERTEX_POINT('',#48181);
#10292=VERTEX_POINT('',#48183);
#10293=VERTEX_POINT('',#48262);
#10294=VERTEX_POINT('',#48345);
#10295=VERTEX_POINT('',#48346);
#10296=VERTEX_POINT('',#48348);
#10297=VERTEX_POINT('',#48482);
#10298=VERTEX_POINT('',#48614);
#10299=VERTEX_POINT('',#48615);
#10300=VERTEX_POINT('',#48617);
#10301=VERTEX_POINT('',#48696);
#10302=VERTEX_POINT('',#48895);
#10303=VERTEX_POINT('',#48896);
#10304=VERTEX_POINT('',#48898);
#10305=VERTEX_POINT('',#49032);
#10306=VERTEX_POINT('',#49228);
#10307=VERTEX_POINT('',#49229);
#10308=VERTEX_POINT('',#49231);
#10309=VERTEX_POINT('',#49307);
#10310=VERTEX_POINT('',#49387);
#10311=VERTEX_POINT('',#49388);
#10312=VERTEX_POINT('',#49390);
#10313=VERTEX_POINT('',#49521);
#10314=VERTEX_POINT('',#49657);
#10315=VERTEX_POINT('',#49658);
#10316=VERTEX_POINT('',#49660);
#10317=VERTEX_POINT('',#49739);
#10318=VERTEX_POINT('',#49938);
#10319=VERTEX_POINT('',#49939);
#10320=VERTEX_POINT('',#49941);
#10321=VERTEX_POINT('',#50073);
#10322=VERTEX_POINT('',#50269);
#10323=VERTEX_POINT('',#50270);
#10324=VERTEX_POINT('',#50272);
#10325=VERTEX_POINT('',#50351);
#10326=VERTEX_POINT('',#50432);
#10327=VERTEX_POINT('',#50433);
#10328=VERTEX_POINT('',#50435);
#10329=VERTEX_POINT('',#50566);
#10330=VERTEX_POINT('',#50698);
#10331=VERTEX_POINT('',#50699);
#10332=VERTEX_POINT('',#50701);
#10333=VERTEX_POINT('',#50899);
#10334=VERTEX_POINT('',#50979);
#10335=VERTEX_POINT('',#50980);
#10336=VERTEX_POINT('',#50982);
#10337=VERTEX_POINT('',#51180);
#10338=VERTEX_POINT('',#51312);
#10339=VERTEX_POINT('',#51313);
#10340=VERTEX_POINT('',#51315);
#10341=VERTEX_POINT('',#51394);
#10342=VERTEX_POINT('',#51593);
#10343=VERTEX_POINT('',#51594);
#10344=VERTEX_POINT('',#51596);
#10345=VERTEX_POINT('',#51603);
#10346=VERTEX_POINT('',#51609);
#10347=VERTEX_POINT('',#51611);
#10348=VERTEX_POINT('',#51678);
#10349=VERTEX_POINT('',#51679);
#10350=VERTEX_POINT('',#51681);
#10351=VERTEX_POINT('',#51690);
#10352=VERTEX_POINT('',#51696);
#10353=VERTEX_POINT('',#51698);
#10354=VERTEX_POINT('',#51766);
#10355=VERTEX_POINT('',#51767);
#10356=VERTEX_POINT('',#51769);
#10357=VERTEX_POINT('',#51900);
#10358=VERTEX_POINT('',#51917);
#10359=VERTEX_POINT('',#51918);
#10360=VERTEX_POINT('',#51920);
#10361=VERTEX_POINT('',#52118);
#10362=VERTEX_POINT('',#52250);
#10363=VERTEX_POINT('',#52251);
#10364=VERTEX_POINT('',#52253);
#10365=VERTEX_POINT('',#52332);
#10366=VERTEX_POINT('',#52531);
#10367=VERTEX_POINT('',#52532);
#10368=VERTEX_POINT('',#52534);
#10369=VERTEX_POINT('',#52668);
#10370=VERTEX_POINT('',#52867);
#10371=VERTEX_POINT('',#52868);
#10372=VERTEX_POINT('',#52870);
#10373=VERTEX_POINT('',#52949);
#10374=VERTEX_POINT('',#53029);
#10375=VERTEX_POINT('',#53030);
#10376=VERTEX_POINT('',#53032);
#10377=VERTEX_POINT('',#53167);
#10378=VERTEX_POINT('',#53299);
#10379=VERTEX_POINT('',#53300);
#10380=VERTEX_POINT('',#53302);
#10381=VERTEX_POINT('',#53494);
#10382=VERTEX_POINT('',#53574);
#10383=VERTEX_POINT('',#53575);
#10384=VERTEX_POINT('',#53577);
#10385=VERTEX_POINT('',#53772);
#10386=VERTEX_POINT('',#53908);
#10387=VERTEX_POINT('',#53909);
#10388=VERTEX_POINT('',#53911);
#10389=VERTEX_POINT('',#53990);
#10390=VERTEX_POINT('',#54070);
#10391=VERTEX_POINT('',#54071);
#10392=VERTEX_POINT('',#54073);
#10393=VERTEX_POINT('',#54205);
#10394=VERTEX_POINT('',#54337);
#10395=VERTEX_POINT('',#54338);
#10396=VERTEX_POINT('',#54340);
#10397=VERTEX_POINT('',#54535);
#10398=VERTEX_POINT('',#54615);
#10399=VERTEX_POINT('',#54616);
#10400=VERTEX_POINT('',#54618);
#10401=VERTEX_POINT('',#54816);
#10402=VERTEX_POINT('',#54948);
#10403=VERTEX_POINT('',#54949);
#10404=VERTEX_POINT('',#54951);
#10405=VERTEX_POINT('',#55030);
#10406=VERTEX_POINT('',#55113);
#10407=VERTEX_POINT('',#55114);
#10408=VERTEX_POINT('',#55116);
#10409=VERTEX_POINT('',#55250);
#10410=VERTEX_POINT('',#55382);
#10411=VERTEX_POINT('',#55383);
#10412=VERTEX_POINT('',#55385);
#10413=VERTEX_POINT('',#55464);
#10414=VERTEX_POINT('',#55663);
#10415=VERTEX_POINT('',#55664);
#10416=VERTEX_POINT('',#55666);
#10417=VERTEX_POINT('',#55800);
#10418=VERTEX_POINT('',#55996);
#10419=VERTEX_POINT('',#55997);
#10420=VERTEX_POINT('',#55999);
#10421=VERTEX_POINT('',#56075);
#10422=VERTEX_POINT('',#56155);
#10423=VERTEX_POINT('',#56156);
#10424=VERTEX_POINT('',#56158);
#10425=VERTEX_POINT('',#56289);
#10426=VERTEX_POINT('',#56425);
#10427=VERTEX_POINT('',#56426);
#10428=VERTEX_POINT('',#56428);
#10429=VERTEX_POINT('',#56507);
#10430=VERTEX_POINT('',#56706);
#10431=VERTEX_POINT('',#56707);
#10432=VERTEX_POINT('',#56709);
#10433=VERTEX_POINT('',#56841);
#10434=VERTEX_POINT('',#57037);
#10435=VERTEX_POINT('',#57038);
#10436=VERTEX_POINT('',#57040);
#10437=VERTEX_POINT('',#57119);
#10438=VERTEX_POINT('',#57200);
#10439=VERTEX_POINT('',#57201);
#10440=VERTEX_POINT('',#57203);
#10441=VERTEX_POINT('',#57334);
#10442=VERTEX_POINT('',#57466);
#10443=VERTEX_POINT('',#57467);
#10444=VERTEX_POINT('',#57469);
#10445=VERTEX_POINT('',#57667);
#10446=VERTEX_POINT('',#57747);
#10447=VERTEX_POINT('',#57748);
#10448=VERTEX_POINT('',#57750);
#10449=VERTEX_POINT('',#57948);
#10450=VERTEX_POINT('',#58080);
#10451=VERTEX_POINT('',#58081);
#10452=VERTEX_POINT('',#58083);
#10453=VERTEX_POINT('',#58162);
#10454=VERTEX_POINT('',#58361);
#10455=VERTEX_POINT('',#58362);
#10456=VERTEX_POINT('',#58364);
#10457=VERTEX_POINT('',#58371);
#10458=VERTEX_POINT('',#58377);
#10459=VERTEX_POINT('',#58379);
#10460=VERTEX_POINT('',#58446);
#10461=VERTEX_POINT('',#58447);
#10462=VERTEX_POINT('',#58449);
#10463=VERTEX_POINT('',#58458);
#10464=VERTEX_POINT('',#58464);
#10465=VERTEX_POINT('',#58466);
#10466=VERTEX_POINT('',#58534);
#10467=VERTEX_POINT('',#58535);
#10468=VERTEX_POINT('',#58537);
#10469=VERTEX_POINT('',#58668);
#10470=VERTEX_POINT('',#58685);
#10471=VERTEX_POINT('',#58686);
#10472=VERTEX_POINT('',#58688);
#10473=VERTEX_POINT('',#58886);
#10474=VERTEX_POINT('',#59018);
#10475=VERTEX_POINT('',#59019);
#10476=VERTEX_POINT('',#59021);
#10477=VERTEX_POINT('',#59100);
#10478=VERTEX_POINT('',#59299);
#10479=VERTEX_POINT('',#59300);
#10480=VERTEX_POINT('',#59302);
#10481=VERTEX_POINT('',#59436);
#10482=VERTEX_POINT('',#59635);
#10483=VERTEX_POINT('',#59636);
#10484=VERTEX_POINT('',#59638);
#10485=VERTEX_POINT('',#59717);
#10486=VERTEX_POINT('',#59797);
#10487=VERTEX_POINT('',#59798);
#10488=VERTEX_POINT('',#59800);
#10489=VERTEX_POINT('',#59935);
#10490=VERTEX_POINT('',#60067);
#10491=VERTEX_POINT('',#60068);
#10492=VERTEX_POINT('',#60070);
#10493=VERTEX_POINT('',#60262);
#10494=VERTEX_POINT('',#60342);
#10495=VERTEX_POINT('',#60343);
#10496=VERTEX_POINT('',#60345);
#10497=VERTEX_POINT('',#60540);
#10498=VERTEX_POINT('',#60676);
#10499=VERTEX_POINT('',#60677);
#10500=VERTEX_POINT('',#60679);
#10501=VERTEX_POINT('',#60758);
#10502=VERTEX_POINT('',#60838);
#10503=VERTEX_POINT('',#60839);
#10504=VERTEX_POINT('',#60841);
#10505=VERTEX_POINT('',#60973);
#10506=VERTEX_POINT('',#61105);
#10507=VERTEX_POINT('',#61106);
#10508=VERTEX_POINT('',#61108);
#10509=VERTEX_POINT('',#61303);
#10510=VERTEX_POINT('',#61383);
#10511=VERTEX_POINT('',#61384);
#10512=VERTEX_POINT('',#61386);
#10513=VERTEX_POINT('',#61584);
#10514=VERTEX_POINT('',#61716);
#10515=VERTEX_POINT('',#61717);
#10516=VERTEX_POINT('',#61719);
#10517=VERTEX_POINT('',#61798);
#10518=VERTEX_POINT('',#61881);
#10519=VERTEX_POINT('',#61882);
#10520=VERTEX_POINT('',#61884);
#10521=VERTEX_POINT('',#62018);
#10522=VERTEX_POINT('',#62150);
#10523=VERTEX_POINT('',#62151);
#10524=VERTEX_POINT('',#62153);
#10525=VERTEX_POINT('',#62232);
#10526=VERTEX_POINT('',#62431);
#10527=VERTEX_POINT('',#62432);
#10528=VERTEX_POINT('',#62434);
#10529=VERTEX_POINT('',#62568);
#10530=VERTEX_POINT('',#62764);
#10531=VERTEX_POINT('',#62765);
#10532=VERTEX_POINT('',#62767);
#10533=VERTEX_POINT('',#62843);
#10534=VERTEX_POINT('',#62923);
#10535=VERTEX_POINT('',#62924);
#10536=VERTEX_POINT('',#62926);
#10537=VERTEX_POINT('',#63057);
#10538=VERTEX_POINT('',#63193);
#10539=VERTEX_POINT('',#63194);
#10540=VERTEX_POINT('',#63196);
#10541=VERTEX_POINT('',#63275);
#10542=VERTEX_POINT('',#63474);
#10543=VERTEX_POINT('',#63475);
#10544=VERTEX_POINT('',#63477);
#10545=VERTEX_POINT('',#63609);
#10546=VERTEX_POINT('',#63805);
#10547=VERTEX_POINT('',#63806);
#10548=VERTEX_POINT('',#63808);
#10549=VERTEX_POINT('',#63887);
#10550=VERTEX_POINT('',#63968);
#10551=VERTEX_POINT('',#63969);
#10552=VERTEX_POINT('',#63971);
#10553=VERTEX_POINT('',#64102);
#10554=VERTEX_POINT('',#64234);
#10555=VERTEX_POINT('',#64235);
#10556=VERTEX_POINT('',#64237);
#10557=VERTEX_POINT('',#64435);
#10558=VERTEX_POINT('',#64515);
#10559=VERTEX_POINT('',#64516);
#10560=VERTEX_POINT('',#64518);
#10561=VERTEX_POINT('',#64716);
#10562=VERTEX_POINT('',#64848);
#10563=VERTEX_POINT('',#64849);
#10564=VERTEX_POINT('',#64851);
#10565=VERTEX_POINT('',#64930);
#10566=VERTEX_POINT('',#65129);
#10567=VERTEX_POINT('',#65130);
#10568=VERTEX_POINT('',#65132);
#10569=VERTEX_POINT('',#65139);
#10570=VERTEX_POINT('',#65145);
#10571=VERTEX_POINT('',#65147);
#10572=VERTEX_POINT('',#65214);
#10573=VERTEX_POINT('',#65215);
#10574=VERTEX_POINT('',#65217);
#10575=VERTEX_POINT('',#65256);
#10576=VERTEX_POINT('',#65258);
#10577=VERTEX_POINT('',#65291);
#10578=VERTEX_POINT('',#65292);
#10579=VERTEX_POINT('',#65294);
#10580=VERTEX_POINT('',#65362);
#10581=VERTEX_POINT('',#65591);
#10582=VERTEX_POINT('',#65592);
#10583=VERTEX_POINT('',#65594);
#10584=VERTEX_POINT('',#65809);
#10585=VERTEX_POINT('',#66044);
#10586=VERTEX_POINT('',#66045);
#10587=VERTEX_POINT('',#66047);
#10588=VERTEX_POINT('',#66064);
#10589=VERTEX_POINT('',#66065);
#10590=VERTEX_POINT('',#66067);
#10591=VERTEX_POINT('',#66084);
#10592=VERTEX_POINT('',#66085);
#10593=VERTEX_POINT('',#66087);
#10594=VERTEX_POINT('',#66358);
#10595=VERTEX_POINT('',#66359);
#10596=VERTEX_POINT('',#66361);
#10597=VERTEX_POINT('',#66595);
#10598=VERTEX_POINT('',#66811);
#10599=VERTEX_POINT('',#66812);
#10600=VERTEX_POINT('',#66814);
#10601=VERTEX_POINT('',#66853);
#10602=VERTEX_POINT('',#66855);
#10603=VERTEX_POINT('',#66888);
#10604=VERTEX_POINT('',#66889);
#10605=VERTEX_POINT('',#66891);
#10606=VERTEX_POINT('',#66918);
#10607=VERTEX_POINT('',#67037);
#10608=VERTEX_POINT('',#67039);
#10609=VERTEX_POINT('',#67218);
#10610=VERTEX_POINT('',#67219);
#10611=VERTEX_POINT('',#67688);
#10612=VERTEX_POINT('',#67689);
#10613=VERTEX_POINT('',#67691);
#10614=VERTEX_POINT('',#67906);
#10615=VERTEX_POINT('',#68144);
#10616=VERTEX_POINT('',#68145);
#10617=VERTEX_POINT('',#68147);
#10618=VERTEX_POINT('',#68402);
#10619=VERTEX_POINT('',#68403);
#10620=VERTEX_POINT('',#68405);
#10621=VERTEX_POINT('',#68601);
#10622=VERTEX_POINT('',#68849);
#10623=VERTEX_POINT('',#68850);
#10624=VERTEX_POINT('',#69359);
#10625=VERTEX_POINT('',#69360);
#10626=VERTEX_POINT('',#69362);
#10627=VERTEX_POINT('',#69629);
#10628=VERTEX_POINT('',#69865);
#10629=VERTEX_POINT('',#69866);
#10630=VERTEX_POINT('',#70341);
#10631=VERTEX_POINT('',#70342);
#10632=VERTEX_POINT('',#70344);
#10633=VERTEX_POINT('',#70577);
#10634=VERTEX_POINT('',#70825);
#10635=VERTEX_POINT('',#70826);
#10636=VERTEX_POINT('',#70828);
#10637=VERTEX_POINT('',#71117);
#10638=VERTEX_POINT('',#71118);
#10639=VERTEX_POINT('',#71120);
#10640=VERTEX_POINT('',#71322);
#10641=VERTEX_POINT('',#71553);
#10642=VERTEX_POINT('',#71554);
#10643=VERTEX_POINT('',#71776);
#10644=VERTEX_POINT('',#71964);
#10645=VERTEX_POINT('',#71965);
#10646=VERTEX_POINT('',#71967);
#10647=VERTEX_POINT('',#72214);
#10648=VERTEX_POINT('',#72234);
#10649=VERTEX_POINT('',#72235);
#10650=VERTEX_POINT('',#72744);
#10651=VERTEX_POINT('',#72745);
#10652=VERTEX_POINT('',#72747);
#10653=VERTEX_POINT('',#73011);
#10654=VERTEX_POINT('',#73247);
#10655=VERTEX_POINT('',#73248);
#10656=VERTEX_POINT('',#73250);
#10657=VERTEX_POINT('',#73511);
#10658=VERTEX_POINT('',#73512);
#10659=VERTEX_POINT('',#73514);
#10660=VERTEX_POINT('',#73714);
#10661=VERTEX_POINT('',#73945);
#10662=VERTEX_POINT('',#73946);
#10663=VERTEX_POINT('',#74184);
#10664=VERTEX_POINT('',#74368);
#10665=VERTEX_POINT('',#74369);
#10666=VERTEX_POINT('',#74371);
#10667=VERTEX_POINT('',#74628);
#10668=VERTEX_POINT('',#74662);
#10669=VERTEX_POINT('',#74663);
#10670=VERTEX_POINT('',#75136);
#10671=VERTEX_POINT('',#75137);
#10672=VERTEX_POINT('',#75139);
#10673=VERTEX_POINT('',#75380);
#10674=VERTEX_POINT('',#75622);
#10675=VERTEX_POINT('',#75623);
#10676=VERTEX_POINT('',#76122);
#10677=VERTEX_POINT('',#76123);
#10678=VERTEX_POINT('',#76125);
#10679=VERTEX_POINT('',#76370);
#10680=VERTEX_POINT('',#76636);
#10681=VERTEX_POINT('',#76637);
#10682=VERTEX_POINT('',#76869);
#10683=VERTEX_POINT('',#77056);
#10684=VERTEX_POINT('',#77057);
#10685=VERTEX_POINT('',#77059);
#10686=VERTEX_POINT('',#77296);
#10687=VERTEX_POINT('',#77314);
#10688=VERTEX_POINT('',#77315);
#10689=VERTEX_POINT('',#77776);
#10690=VERTEX_POINT('',#77777);
#10691=VERTEX_POINT('',#77779);
#10692=VERTEX_POINT('',#77886);
#10693=VERTEX_POINT('',#78049);
#10694=VERTEX_POINT('',#78050);
#10695=VERTEX_POINT('',#78052);
#10696=VERTEX_POINT('',#78079);
#10697=VERTEX_POINT('',#78198);
#10698=VERTEX_POINT('',#78200);
#10699=VERTEX_POINT('',#78379);
#10700=VERTEX_POINT('',#78380);
#10701=VERTEX_POINT('',#78843);
#10702=VERTEX_POINT('',#78844);
#10703=VERTEX_POINT('',#78846);
#10704=VERTEX_POINT('',#79061);
#10705=VERTEX_POINT('',#79301);
#10706=VERTEX_POINT('',#79302);
#10707=VERTEX_POINT('',#79304);
#10708=VERTEX_POINT('',#79557);
#10709=VERTEX_POINT('',#79558);
#10710=VERTEX_POINT('',#79560);
#10711=VERTEX_POINT('',#79756);
#10712=VERTEX_POINT('',#80002);
#10713=VERTEX_POINT('',#80003);
#10714=VERTEX_POINT('',#80512);
#10715=VERTEX_POINT('',#80513);
#10716=VERTEX_POINT('',#80515);
#10717=VERTEX_POINT('',#80782);
#10718=VERTEX_POINT('',#81016);
#10719=VERTEX_POINT('',#81017);
#10720=VERTEX_POINT('',#81526);
#10721=VERTEX_POINT('',#81527);
#10722=VERTEX_POINT('',#81529);
#10723=VERTEX_POINT('',#81752);
#10724=VERTEX_POINT('',#82000);
#10725=VERTEX_POINT('',#82001);
#10726=VERTEX_POINT('',#82003);
#10727=VERTEX_POINT('',#82292);
#10728=VERTEX_POINT('',#82293);
#10729=VERTEX_POINT('',#82295);
#10730=VERTEX_POINT('',#82497);
#10731=VERTEX_POINT('',#82724);
#10732=VERTEX_POINT('',#82725);
#10733=VERTEX_POINT('',#82947);
#10734=VERTEX_POINT('',#83135);
#10735=VERTEX_POINT('',#83136);
#10736=VERTEX_POINT('',#83138);
#10737=VERTEX_POINT('',#83389);
#10738=VERTEX_POINT('',#83409);
#10739=VERTEX_POINT('',#83410);
#10740=VERTEX_POINT('',#83901);
#10741=VERTEX_POINT('',#83902);
#10742=VERTEX_POINT('',#83904);
#10743=VERTEX_POINT('',#84166);
#10744=VERTEX_POINT('',#84402);
#10745=VERTEX_POINT('',#84403);
#10746=VERTEX_POINT('',#84405);
#10747=VERTEX_POINT('',#84658);
#10748=VERTEX_POINT('',#84659);
#10749=VERTEX_POINT('',#84661);
#10750=VERTEX_POINT('',#84859);
#10751=VERTEX_POINT('',#85090);
#10752=VERTEX_POINT('',#85091);
#10753=VERTEX_POINT('',#85329);
#10754=VERTEX_POINT('',#85513);
#10755=VERTEX_POINT('',#85514);
#10756=VERTEX_POINT('',#85516);
#10757=VERTEX_POINT('',#85775);
#10758=VERTEX_POINT('',#85809);
#10759=VERTEX_POINT('',#85810);
#10760=VERTEX_POINT('',#86287);
#10761=VERTEX_POINT('',#86288);
#10762=VERTEX_POINT('',#86290);
#10763=VERTEX_POINT('',#86575);
#10764=VERTEX_POINT('',#86817);
#10765=VERTEX_POINT('',#86818);
#10766=VERTEX_POINT('',#87313);
#10767=VERTEX_POINT('',#87314);
#10768=VERTEX_POINT('',#87316);
#10769=VERTEX_POINT('',#87557);
#10770=VERTEX_POINT('',#87847);
#10771=VERTEX_POINT('',#87848);
#10772=VERTEX_POINT('',#88080);
#10773=VERTEX_POINT('',#88267);
#10774=VERTEX_POINT('',#88268);
#10775=VERTEX_POINT('',#88270);
#10776=VERTEX_POINT('',#88509);
#10777=VERTEX_POINT('',#88527);
#10778=VERTEX_POINT('',#88528);
#10779=VERTEX_POINT('',#88993);
#10780=VERTEX_POINT('',#88994);
#10781=VERTEX_POINT('',#88996);
#10782=VERTEX_POINT('',#89103);
#10783=VERTEX_POINT('',#89266);
#10784=VERTEX_POINT('',#89267);
#10785=VERTEX_POINT('',#89269);
#10786=VERTEX_POINT('',#89296);
#10787=VERTEX_POINT('',#89415);
#10788=VERTEX_POINT('',#89417);
#10789=VERTEX_POINT('',#89596);
#10790=VERTEX_POINT('',#89597);
#10791=VERTEX_POINT('',#90058);
#10792=VERTEX_POINT('',#90059);
#10793=VERTEX_POINT('',#90061);
#10794=VERTEX_POINT('',#90276);
#10795=VERTEX_POINT('',#90514);
#10796=VERTEX_POINT('',#90515);
#10797=VERTEX_POINT('',#90517);
#10798=VERTEX_POINT('',#90764);
#10799=VERTEX_POINT('',#90765);
#10800=VERTEX_POINT('',#90767);
#10801=VERTEX_POINT('',#90963);
#10802=VERTEX_POINT('',#91209);
#10803=VERTEX_POINT('',#91210);
#10804=VERTEX_POINT('',#91731);
#10805=VERTEX_POINT('',#91732);
#10806=VERTEX_POINT('',#91734);
#10807=VERTEX_POINT('',#92001);
#10808=VERTEX_POINT('',#92235);
#10809=VERTEX_POINT('',#92236);
#10810=VERTEX_POINT('',#92701);
#10811=VERTEX_POINT('',#92702);
#10812=VERTEX_POINT('',#92704);
#10813=VERTEX_POINT('',#92927);
#10814=VERTEX_POINT('',#93175);
#10815=VERTEX_POINT('',#93176);
#10816=VERTEX_POINT('',#93178);
#10817=VERTEX_POINT('',#93467);
#10818=VERTEX_POINT('',#93468);
#10819=VERTEX_POINT('',#93470);
#10820=VERTEX_POINT('',#93672);
#10821=VERTEX_POINT('',#93899);
#10822=VERTEX_POINT('',#93900);
#10823=VERTEX_POINT('',#94122);
#10824=VERTEX_POINT('',#94310);
#10825=VERTEX_POINT('',#94311);
#10826=VERTEX_POINT('',#94313);
#10827=VERTEX_POINT('',#94558);
#10828=VERTEX_POINT('',#94578);
#10829=VERTEX_POINT('',#94579);
#10830=VERTEX_POINT('',#95072);
#10831=VERTEX_POINT('',#95073);
#10832=VERTEX_POINT('',#95075);
#10833=VERTEX_POINT('',#95337);
#10834=VERTEX_POINT('',#95573);
#10835=VERTEX_POINT('',#95574);
#10836=VERTEX_POINT('',#95576);
#10837=VERTEX_POINT('',#95837);
#10838=VERTEX_POINT('',#95838);
#10839=VERTEX_POINT('',#95840);
#10840=VERTEX_POINT('',#96040);
#10841=VERTEX_POINT('',#96271);
#10842=VERTEX_POINT('',#96272);
#10843=VERTEX_POINT('',#96508);
#10844=VERTEX_POINT('',#96692);
#10845=VERTEX_POINT('',#96693);
#10846=VERTEX_POINT('',#96695);
#10847=VERTEX_POINT('',#96952);
#10848=VERTEX_POINT('',#96986);
#10849=VERTEX_POINT('',#96987);
#10850=VERTEX_POINT('',#97464);
#10851=VERTEX_POINT('',#97465);
#10852=VERTEX_POINT('',#97467);
#10853=VERTEX_POINT('',#97708);
#10854=VERTEX_POINT('',#97950);
#10855=VERTEX_POINT('',#97951);
#10856=VERTEX_POINT('',#98446);
#10857=VERTEX_POINT('',#98447);
#10858=VERTEX_POINT('',#98449);
#10859=VERTEX_POINT('',#98692);
#10860=VERTEX_POINT('',#98960);
#10861=VERTEX_POINT('',#98961);
#10862=VERTEX_POINT('',#99193);
#10863=VERTEX_POINT('',#99380);
#10864=VERTEX_POINT('',#99381);
#10865=VERTEX_POINT('',#99383);
#10866=VERTEX_POINT('',#99624);
#10867=VERTEX_POINT('',#99642);
#10868=VERTEX_POINT('',#99643);
#10869=VERTEX_POINT('',#100104);
#10870=VERTEX_POINT('',#100105);
#10871=VERTEX_POINT('',#100107);
#10872=VERTEX_POINT('',#100214);
#10873=VERTEX_POINT('',#100377);
#10874=VERTEX_POINT('',#100378);
#10875=VERTEX_POINT('',#100380);
#10876=VERTEX_POINT('',#100407);
#10877=VERTEX_POINT('',#100526);
#10878=VERTEX_POINT('',#100528);
#10879=VERTEX_POINT('',#100707);
#10880=VERTEX_POINT('',#100708);
#10881=VERTEX_POINT('',#101177);
#10882=VERTEX_POINT('',#101178);
#10883=VERTEX_POINT('',#101180);
#10884=VERTEX_POINT('',#101395);
#10885=VERTEX_POINT('',#101635);
#10886=VERTEX_POINT('',#101636);
#10887=VERTEX_POINT('',#101638);
#10888=VERTEX_POINT('',#101889);
#10889=VERTEX_POINT('',#101890);
#10890=VERTEX_POINT('',#101892);
#10891=VERTEX_POINT('',#102088);
#10892=VERTEX_POINT('',#102334);
#10893=VERTEX_POINT('',#102335);
#10894=VERTEX_POINT('',#102842);
#10895=VERTEX_POINT('',#102843);
#10896=VERTEX_POINT('',#102845);
#10897=VERTEX_POINT('',#103112);
#10898=VERTEX_POINT('',#103346);
#10899=VERTEX_POINT('',#103347);
#10900=VERTEX_POINT('',#103868);
#10901=VERTEX_POINT('',#103869);
#10902=VERTEX_POINT('',#103871);
#10903=VERTEX_POINT('',#104102);
#10904=VERTEX_POINT('',#104352);
#10905=VERTEX_POINT('',#104353);
#10906=VERTEX_POINT('',#104355);
#10907=VERTEX_POINT('',#104646);
#10908=VERTEX_POINT('',#104647);
#10909=VERTEX_POINT('',#104649);
#10910=VERTEX_POINT('',#104851);
#10911=VERTEX_POINT('',#105082);
#10912=VERTEX_POINT('',#105083);
#10913=VERTEX_POINT('',#105305);
#10914=VERTEX_POINT('',#105493);
#10915=VERTEX_POINT('',#105494);
#10916=VERTEX_POINT('',#105496);
#10917=VERTEX_POINT('',#105737);
#10918=VERTEX_POINT('',#105757);
#10919=VERTEX_POINT('',#105758);
#10920=VERTEX_POINT('',#106249);
#10921=VERTEX_POINT('',#106250);
#10922=VERTEX_POINT('',#106252);
#10923=VERTEX_POINT('',#106518);
#10924=VERTEX_POINT('',#106802);
#10925=VERTEX_POINT('',#106803);
#10926=VERTEX_POINT('',#106805);
#10927=VERTEX_POINT('',#107062);
#10928=VERTEX_POINT('',#107063);
#10929=VERTEX_POINT('',#107065);
#10930=VERTEX_POINT('',#107263);
#10931=VERTEX_POINT('',#107494);
#10932=VERTEX_POINT('',#107495);
#10933=VERTEX_POINT('',#107733);
#10934=VERTEX_POINT('',#107917);
#10935=VERTEX_POINT('',#107918);
#10936=VERTEX_POINT('',#107920);
#10937=VERTEX_POINT('',#108179);
#10938=VERTEX_POINT('',#108213);
#10939=VERTEX_POINT('',#108214);
#10940=VERTEX_POINT('',#108687);
#10941=VERTEX_POINT('',#108688);
#10942=VERTEX_POINT('',#108690);
#10943=VERTEX_POINT('',#108931);
#10944=VERTEX_POINT('',#109165);
#10945=VERTEX_POINT('',#109166);
#10946=VERTEX_POINT('',#109661);
#10947=VERTEX_POINT('',#109662);
#10948=VERTEX_POINT('',#109664);
#10949=VERTEX_POINT('',#109911);
#10950=VERTEX_POINT('',#110185);
#10951=VERTEX_POINT('',#110186);
#10952=VERTEX_POINT('',#110418);
#10953=VERTEX_POINT('',#110605);
#10954=VERTEX_POINT('',#110606);
#10955=VERTEX_POINT('',#110608);
#10956=VERTEX_POINT('',#110847);
#10957=VERTEX_POINT('',#110865);
#10958=VERTEX_POINT('',#110866);
#10959=VERTEX_POINT('',#111327);
#10960=VERTEX_POINT('',#111328);
#10961=VERTEX_POINT('',#111330);
#10962=VERTEX_POINT('',#111437);
#10963=VERTEX_POINT('',#111600);
#10964=VERTEX_POINT('',#111838);
#10965=VERTEX_POINT('',#112075);
#10966=VERTEX_POINT('',#112315);
#10967=VERTEX_POINT('',#112552);
#10968=VERTEX_POINT('',#112792);
#10969=VERTEX_POINT('',#113029);
#10970=VERTEX_POINT('',#113259);
#10971=VERTEX_POINT('',#113496);
#10972=VERTEX_POINT('',#113724);
#10973=VERTEX_POINT('',#113845);
#10974=VERTEX_POINT('',#114062);
#10975=VERTEX_POINT('',#114077);
#10976=VERTEX_POINT('',#114157);
#10977=VERTEX_POINT('',#114172);
#10978=VERTEX_POINT('',#114252);
#10979=VERTEX_POINT('',#114267);
#10980=VERTEX_POINT('',#114347);
#10981=VERTEX_POINT('',#114362);
#10982=VERTEX_POINT('',#114442);
#10983=VERTEX_POINT('',#114537);
#10984=VERTEX_POINT('',#114778);
#10985=VERTEX_POINT('',#114873);
#10986=VERTEX_POINT('',#115114);
#10987=VERTEX_POINT('',#115116);
#10988=VERTEX_POINT('',#115121);
#10989=VERTEX_POINT('',#115122);
#10990=VERTEX_POINT('',#115124);
#10991=VERTEX_POINT('',#115126);
#10992=VERTEX_POINT('',#115130);
#10993=VERTEX_POINT('',#115132);
#10994=VERTEX_POINT('',#115134);
#10995=VERTEX_POINT('',#115138);
#10996=VERTEX_POINT('',#115140);
#10997=VERTEX_POINT('',#115145);
#10998=VERTEX_POINT('',#115146);
#10999=VERTEX_POINT('',#115148);
#11000=VERTEX_POINT('',#115150);
#11001=VERTEX_POINT('',#115154);
#11002=VERTEX_POINT('',#115155);
#11003=VERTEX_POINT('',#115158);
#11004=VERTEX_POINT('',#115162);
#11005=VERTEX_POINT('',#115164);
#11006=VERTEX_POINT('',#115169);
#11007=VERTEX_POINT('',#115171);
#11008=VERTEX_POINT('',#115175);
#11009=VERTEX_POINT('',#115177);
#11010=VERTEX_POINT('',#115179);
#11011=VERTEX_POINT('',#115184);
#11012=VERTEX_POINT('',#115188);
#11013=VERTEX_POINT('',#115190);
#11014=VERTEX_POINT('',#115192);
#11015=VERTEX_POINT('',#115194);
#11016=VERTEX_POINT('',#115196);
#11017=VERTEX_POINT('',#115198);
#11018=VERTEX_POINT('',#115200);
#11019=VERTEX_POINT('',#115202);
#11020=VERTEX_POINT('',#115204);
#11021=VERTEX_POINT('',#115206);
#11022=VERTEX_POINT('',#115208);
#11023=VERTEX_POINT('',#115210);
#11024=VERTEX_POINT('',#115212);
#11025=VERTEX_POINT('',#115214);
#11026=VERTEX_POINT('',#115216);
#11027=VERTEX_POINT('',#115218);
#11028=VERTEX_POINT('',#115220);
#11029=VERTEX_POINT('',#115222);
#11030=VERTEX_POINT('',#115224);
#11031=VERTEX_POINT('',#115226);
#11032=VERTEX_POINT('',#115228);
#11033=VERTEX_POINT('',#115230);
#11034=VERTEX_POINT('',#115232);
#11035=VERTEX_POINT('',#115234);
#11036=VERTEX_POINT('',#115236);
#11037=VERTEX_POINT('',#115238);
#11038=VERTEX_POINT('',#115240);
#11039=VERTEX_POINT('',#115243);
#11040=VERTEX_POINT('',#115245);
#11041=VERTEX_POINT('',#124043);
#11042=VERTEX_POINT('',#124044);
#11043=VERTEX_POINT('',#124046);
#11044=VERTEX_POINT('',#124048);
#11045=VERTEX_POINT('',#124052);
#11046=VERTEX_POINT('',#124054);
#11047=VERTEX_POINT('',#124058);
#11048=VERTEX_POINT('',#124060);
#11049=VERTEX_POINT('',#124064);
#11050=VERTEX_POINT('',#124066);
#11051=VERTEX_POINT('',#124070);
#11052=VERTEX_POINT('',#124072);
#11053=VERTEX_POINT('',#124076);
#11054=VERTEX_POINT('',#124078);
#11055=VERTEX_POINT('',#124085);
#11056=VERTEX_POINT('',#124087);
#11057=VERTEX_POINT('',#124092);
#11058=VERTEX_POINT('',#124093);
#11059=VERTEX_POINT('',#124095);
#11060=VERTEX_POINT('',#124097);
#11061=VERTEX_POINT('',#124101);
#11062=VERTEX_POINT('',#124103);
#11063=VERTEX_POINT('',#124107);
#11064=VERTEX_POINT('',#124109);
#11065=VERTEX_POINT('',#124119);
#11066=VERTEX_POINT('',#124121);
#11067=VERTEX_POINT('',#124124);
#11068=VERTEX_POINT('',#124125);
#11069=VERTEX_POINT('',#124127);
#11070=VERTEX_POINT('',#124129);
#11071=VERTEX_POINT('',#124133);
#11072=VERTEX_POINT('',#124135);
#11073=VERTEX_POINT('',#124139);
#11074=VERTEX_POINT('',#124141);
#11075=VERTEX_POINT('',#124145);
#11076=VERTEX_POINT('',#124147);
#11077=VERTEX_POINT('',#124151);
#11078=VERTEX_POINT('',#124153);
#11079=VERTEX_POINT('',#124157);
#11080=VERTEX_POINT('',#124159);
#11081=VERTEX_POINT('',#124166);
#11082=VERTEX_POINT('',#124168);
#11083=VERTEX_POINT('',#124175);
#11084=VERTEX_POINT('',#124181);
#11085=VERTEX_POINT('',#124186);
#11086=VERTEX_POINT('',#124187);
#11087=VERTEX_POINT('',#124189);
#11088=VERTEX_POINT('',#124191);
#11089=VERTEX_POINT('',#124195);
#11090=VERTEX_POINT('',#124197);
#11091=VERTEX_POINT('',#124201);
#11092=VERTEX_POINT('',#124203);
#11093=VERTEX_POINT('',#124213);
#11094=VERTEX_POINT('',#124215);
#11095=VERTEX_POINT('',#124218);
#11096=VERTEX_POINT('',#124219);
#11097=VERTEX_POINT('',#124221);
#11098=VERTEX_POINT('',#124223);
#11099=VERTEX_POINT('',#124227);
#11100=VERTEX_POINT('',#124229);
#11101=VERTEX_POINT('',#124233);
#11102=VERTEX_POINT('',#124235);
#11103=VERTEX_POINT('',#124239);
#11104=VERTEX_POINT('',#124241);
#11105=VERTEX_POINT('',#124245);
#11106=VERTEX_POINT('',#124247);
#11107=VERTEX_POINT('',#124251);
#11108=VERTEX_POINT('',#124253);
#11109=VERTEX_POINT('',#124260);
#11110=VERTEX_POINT('',#124262);
#11111=VERTEX_POINT('',#124267);
#11112=VERTEX_POINT('',#124268);
#11113=VERTEX_POINT('',#124270);
#11114=VERTEX_POINT('',#124272);
#11115=VERTEX_POINT('',#124276);
#11116=VERTEX_POINT('',#124278);
#11117=VERTEX_POINT('',#124282);
#11118=VERTEX_POINT('',#124284);
#11119=VERTEX_POINT('',#124288);
#11120=VERTEX_POINT('',#124290);
#11121=VERTEX_POINT('',#124294);
#11122=VERTEX_POINT('',#124296);
#11123=VERTEX_POINT('',#124300);
#11124=VERTEX_POINT('',#124302);
#11125=VERTEX_POINT('',#124309);
#11126=VERTEX_POINT('',#124311);
#11127=VERTEX_POINT('',#124318);
#11128=VERTEX_POINT('',#124320);
#11129=VERTEX_POINT('',#124325);
#11130=VERTEX_POINT('',#124330);
#11131=VERTEX_POINT('',#124335);
#11132=VERTEX_POINT('',#124340);
#11133=VERTEX_POINT('',#124345);
#11134=VERTEX_POINT('',#124351);
#11135=VERTEX_POINT('',#124355);
#11136=VERTEX_POINT('',#124359);
#11137=VERTEX_POINT('',#124363);
#11138=VERTEX_POINT('',#124367);
#11139=VERTEX_POINT('',#124371);
#11140=VERTEX_POINT('',#124377);
#11141=VERTEX_POINT('',#124381);
#11142=VERTEX_POINT('',#124385);
#11143=VERTEX_POINT('',#124389);
#11144=VERTEX_POINT('',#124393);
#11145=VERTEX_POINT('',#124397);
#11146=VERTEX_POINT('',#124401);
#11147=VERTEX_POINT('',#124405);
#11148=VERTEX_POINT('',#124409);
#11149=VERTEX_POINT('',#124413);
#11150=VERTEX_POINT('',#124417);
#11151=VERTEX_POINT('',#124421);
#11152=VERTEX_POINT('',#124430);
#11153=VERTEX_POINT('',#124432);
#11154=VERTEX_POINT('',#124437);
#11155=VERTEX_POINT('',#124439);
#11156=VERTEX_POINT('',#124444);
#11157=VERTEX_POINT('',#124445);
#11158=VERTEX_POINT('',#124447);
#11159=VERTEX_POINT('',#124449);
#11160=VERTEX_POINT('',#124453);
#11161=VERTEX_POINT('',#124455);
#11162=VERTEX_POINT('',#124459);
#11163=VERTEX_POINT('',#124460);
#11164=VERTEX_POINT('',#124462);
#11165=VERTEX_POINT('',#124464);
#11166=VERTEX_POINT('',#124468);
#11167=VERTEX_POINT('',#124469);
#11168=VERTEX_POINT('',#124474);
#11169=VERTEX_POINT('',#124475);
#11170=VERTEX_POINT('',#124480);
#11171=VERTEX_POINT('',#124481);
#11172=VERTEX_POINT('',#124486);
#11173=VERTEX_POINT('',#124487);
#11174=VERTEX_POINT('',#124492);
#11175=VERTEX_POINT('',#124493);
#11176=VERTEX_POINT('',#124498);
#11177=VERTEX_POINT('',#124499);
#11178=VERTEX_POINT('',#124512);
#11179=VERTEX_POINT('',#124513);
#11180=VERTEX_POINT('',#124518);
#11181=VERTEX_POINT('',#124520);
#11182=VERTEX_POINT('',#124524);
#11183=VERTEX_POINT('',#124526);
#11184=VERTEX_POINT('',#124530);
#11185=VERTEX_POINT('',#124532);
#11186=VERTEX_POINT('',#124536);
#11187=VERTEX_POINT('',#124537);
#11188=VERTEX_POINT('',#124542);
#11189=VERTEX_POINT('',#124544);
#11190=VERTEX_POINT('',#124551);
#11191=VERTEX_POINT('',#124553);
#11192=VERTEX_POINT('',#124557);
#11193=VERTEX_POINT('',#124558);
#11194=VERTEX_POINT('',#124563);
#11195=VERTEX_POINT('',#124565);
#11196=VERTEX_POINT('',#124569);
#11197=VERTEX_POINT('',#124571);
#11198=VERTEX_POINT('',#124575);
#11199=VERTEX_POINT('',#124577);
#11200=VERTEX_POINT('',#124589);
#11201=VERTEX_POINT('',#124590);
#11202=VERTEX_POINT('',#124595);
#11203=VERTEX_POINT('',#124596);
#11204=VERTEX_POINT('',#124601);
#11205=VERTEX_POINT('',#124602);
#11206=VERTEX_POINT('',#124607);
#11207=VERTEX_POINT('',#124608);
#11208=VERTEX_POINT('',#124613);
#11209=VERTEX_POINT('',#124614);
#11210=VERTEX_POINT('',#124619);
#11211=VERTEX_POINT('',#124620);
#11212=VERTEX_POINT('',#124625);
#11213=VERTEX_POINT('',#124626);
#11214=VERTEX_POINT('',#124631);
#11215=VERTEX_POINT('',#124632);
#11216=VERTEX_POINT('',#124637);
#11217=VERTEX_POINT('',#124638);
#11218=VERTEX_POINT('',#124641);
#11219=VERTEX_POINT('',#124645);
#11220=VERTEX_POINT('',#124647);
#11221=VERTEX_POINT('',#124651);
#11222=VERTEX_POINT('',#124660);
#11223=VERTEX_POINT('',#124662);
#11224=VERTEX_POINT('',#124666);
#11225=VERTEX_POINT('',#124670);
#11226=VERTEX_POINT('',#124674);
#11227=VERTEX_POINT('',#124678);
#11228=VERTEX_POINT('',#124682);
#11229=VERTEX_POINT('',#124686);
#11230=VERTEX_POINT('',#124690);
#11231=VERTEX_POINT('',#124694);
#11232=VERTEX_POINT('',#124698);
#11233=VERTEX_POINT('',#124700);
#11234=VERTEX_POINT('',#124702);
#11235=VERTEX_POINT('',#124706);
#11236=VERTEX_POINT('',#124710);
#11237=VERTEX_POINT('',#124714);
#11238=VERTEX_POINT('',#124716);
#11239=VERTEX_POINT('',#124718);
#11240=VERTEX_POINT('',#124722);
#11241=VERTEX_POINT('',#124726);
#11242=VERTEX_POINT('',#124730);
#11243=VERTEX_POINT('',#124734);
#11244=VERTEX_POINT('',#124739);
#11245=VERTEX_POINT('',#124741);
#11246=VERTEX_POINT('',#124758);
#11247=VERTEX_POINT('',#124760);
#11248=VERTEX_POINT('',#124783);
#11249=VERTEX_POINT('',#124788);
#11250=VERTEX_POINT('',#124792);
#11251=VERTEX_POINT('',#124797);
#11252=VERTEX_POINT('',#124798);
#11253=VERTEX_POINT('',#124800);
#11254=VERTEX_POINT('',#124813);
#11255=VERTEX_POINT('',#124822);
#11256=VERTEX_POINT('',#124840);
#11257=VERTEX_POINT('',#124846);
#11258=VERTEX_POINT('',#124851);
#11259=VERTEX_POINT('',#124853);
#11260=VERTEX_POINT('',#124855);
#11261=VERTEX_POINT('',#124857);
#11262=VERTEX_POINT('',#124859);
#11263=VERTEX_POINT('',#124861);
#11264=VERTEX_POINT('',#124863);
#11265=VERTEX_POINT('',#124865);
#11266=VERTEX_POINT('',#124867);
#11267=VERTEX_POINT('',#124869);
#11268=VERTEX_POINT('',#124871);
#11269=VERTEX_POINT('',#124873);
#11270=VERTEX_POINT('',#124875);
#11271=VERTEX_POINT('',#124877);
#11272=VERTEX_POINT('',#124879);
#11273=VERTEX_POINT('',#124881);
#11274=VERTEX_POINT('',#124883);
#11275=VERTEX_POINT('',#124885);
#11276=VERTEX_POINT('',#124887);
#11277=VERTEX_POINT('',#124891);
#11278=VERTEX_POINT('',#124893);
#11279=VERTEX_POINT('',#124924);
#11280=VERTEX_POINT('',#124925);
#11281=VERTEX_POINT('',#124930);
#11282=VERTEX_POINT('',#124936);
#11283=VERTEX_POINT('',#124937);
#11284=VERTEX_POINT('',#124942);
#11285=VERTEX_POINT('',#124948);
#11286=VERTEX_POINT('',#124952);
#11287=VERTEX_POINT('',#124956);
#11288=VERTEX_POINT('',#124968);
#11289=VERTEX_POINT('',#124998);
#11290=VERTEX_POINT('',#125000);
#11291=VERTEX_POINT('',#125004);
#11292=VERTEX_POINT('',#125011);
#11293=VERTEX_POINT('',#125013);
#11294=VERTEX_POINT('',#125025);
#11295=VERTEX_POINT('',#125027);
#11296=VERTEX_POINT('',#125032);
#11297=VERTEX_POINT('',#125034);
#11298=VERTEX_POINT('',#125039);
#11299=VERTEX_POINT('',#125040);
#11300=VERTEX_POINT('',#125042);
#11301=VERTEX_POINT('',#125044);
#11302=VERTEX_POINT('',#125048);
#11303=VERTEX_POINT('',#125050);
#11304=VERTEX_POINT('',#125054);
#11305=VERTEX_POINT('',#125055);
#11306=VERTEX_POINT('',#125057);
#11307=VERTEX_POINT('',#125059);
#11308=VERTEX_POINT('',#125063);
#11309=VERTEX_POINT('',#125064);
#11310=VERTEX_POINT('',#125069);
#11311=VERTEX_POINT('',#125070);
#11312=VERTEX_POINT('',#125075);
#11313=VERTEX_POINT('',#125076);
#11314=VERTEX_POINT('',#125081);
#11315=VERTEX_POINT('',#125082);
#11316=VERTEX_POINT('',#125087);
#11317=VERTEX_POINT('',#125088);
#11318=VERTEX_POINT('',#125093);
#11319=VERTEX_POINT('',#125094);
#11320=VERTEX_POINT('',#125107);
#11321=VERTEX_POINT('',#125108);
#11322=VERTEX_POINT('',#125113);
#11323=VERTEX_POINT('',#125115);
#11324=VERTEX_POINT('',#125119);
#11325=VERTEX_POINT('',#125121);
#11326=VERTEX_POINT('',#125125);
#11327=VERTEX_POINT('',#125127);
#11328=VERTEX_POINT('',#125131);
#11329=VERTEX_POINT('',#125132);
#11330=VERTEX_POINT('',#125137);
#11331=VERTEX_POINT('',#125139);
#11332=VERTEX_POINT('',#125146);
#11333=VERTEX_POINT('',#125148);
#11334=VERTEX_POINT('',#125152);
#11335=VERTEX_POINT('',#125153);
#11336=VERTEX_POINT('',#125158);
#11337=VERTEX_POINT('',#125160);
#11338=VERTEX_POINT('',#125164);
#11339=VERTEX_POINT('',#125166);
#11340=VERTEX_POINT('',#125170);
#11341=VERTEX_POINT('',#125172);
#11342=VERTEX_POINT('',#125184);
#11343=VERTEX_POINT('',#125185);
#11344=VERTEX_POINT('',#125190);
#11345=VERTEX_POINT('',#125191);
#11346=VERTEX_POINT('',#125196);
#11347=VERTEX_POINT('',#125197);
#11348=VERTEX_POINT('',#125202);
#11349=VERTEX_POINT('',#125203);
#11350=VERTEX_POINT('',#125208);
#11351=VERTEX_POINT('',#125209);
#11352=VERTEX_POINT('',#125214);
#11353=VERTEX_POINT('',#125215);
#11354=VERTEX_POINT('',#125220);
#11355=VERTEX_POINT('',#125221);
#11356=VERTEX_POINT('',#125226);
#11357=VERTEX_POINT('',#125227);
#11358=VERTEX_POINT('',#125232);
#11359=VERTEX_POINT('',#125233);
#11360=VERTEX_POINT('',#125235);
#11361=VERTEX_POINT('',#125240);
#11362=VERTEX_POINT('',#125242);
#11363=VERTEX_POINT('',#125247);
#11364=VERTEX_POINT('',#125255);
#11365=VERTEX_POINT('',#125257);
#11366=VERTEX_POINT('',#125261);
#11367=VERTEX_POINT('',#125265);
#11368=VERTEX_POINT('',#125269);
#11369=VERTEX_POINT('',#125273);
#11370=VERTEX_POINT('',#125277);
#11371=VERTEX_POINT('',#125281);
#11372=VERTEX_POINT('',#125285);
#11373=VERTEX_POINT('',#125289);
#11374=VERTEX_POINT('',#125293);
#11375=VERTEX_POINT('',#125295);
#11376=VERTEX_POINT('',#125297);
#11377=VERTEX_POINT('',#125301);
#11378=VERTEX_POINT('',#125305);
#11379=VERTEX_POINT('',#125309);
#11380=VERTEX_POINT('',#125311);
#11381=VERTEX_POINT('',#125313);
#11382=VERTEX_POINT('',#125317);
#11383=VERTEX_POINT('',#125321);
#11384=VERTEX_POINT('',#125325);
#11385=VERTEX_POINT('',#125329);
#11386=VERTEX_POINT('',#125334);
#11387=VERTEX_POINT('',#125349);
#11388=VERTEX_POINT('',#125353);
#11389=VERTEX_POINT('',#125356);
#11390=VERTEX_POINT('',#125378);
#11391=VERTEX_POINT('',#125383);
#11392=VERTEX_POINT('',#125387);
#11393=VERTEX_POINT('',#125392);
#11394=VERTEX_POINT('',#125393);
#11395=VERTEX_POINT('',#125395);
#11396=VERTEX_POINT('',#125410);
#11397=VERTEX_POINT('',#125412);
#11398=VERTEX_POINT('',#125435);
#11399=VERTEX_POINT('',#125442);
#11400=VERTEX_POINT('',#125446);
#11401=VERTEX_POINT('',#125448);
#11402=VERTEX_POINT('',#125450);
#11403=VERTEX_POINT('',#125452);
#11404=VERTEX_POINT('',#125454);
#11405=VERTEX_POINT('',#125456);
#11406=VERTEX_POINT('',#125458);
#11407=VERTEX_POINT('',#125460);
#11408=VERTEX_POINT('',#125462);
#11409=VERTEX_POINT('',#125464);
#11410=VERTEX_POINT('',#125466);
#11411=VERTEX_POINT('',#125468);
#11412=VERTEX_POINT('',#125470);
#11413=VERTEX_POINT('',#125472);
#11414=VERTEX_POINT('',#125474);
#11415=VERTEX_POINT('',#125476);
#11416=VERTEX_POINT('',#125478);
#11417=VERTEX_POINT('',#125480);
#11418=VERTEX_POINT('',#125482);
#11419=VERTEX_POINT('',#125486);
#11420=VERTEX_POINT('',#125488);
#11421=VERTEX_POINT('',#125519);
#11422=VERTEX_POINT('',#125520);
#11423=VERTEX_POINT('',#125525);
#11424=VERTEX_POINT('',#125531);
#11425=VERTEX_POINT('',#125532);
#11426=VERTEX_POINT('',#125537);
#11427=VERTEX_POINT('',#125543);
#11428=VERTEX_POINT('',#125547);
#11429=VERTEX_POINT('',#125551);
#11430=VERTEX_POINT('',#125563);
#11431=VERTEX_POINT('',#125593);
#11432=VERTEX_POINT('',#125595);
#11433=VERTEX_POINT('',#125599);
#11434=VERTEX_POINT('',#125606);
#11435=VERTEX_POINT('',#125608);
#11436=VERTEX_POINT('',#125619);
#11437=VERTEX_POINT('',#125620);
#11438=VERTEX_POINT('',#125623);
#11439=VERTEX_POINT('',#125628);
#11440=VERTEX_POINT('',#125629);
#11441=VERTEX_POINT('',#125632);
#11442=VERTEX_POINT('',#125638);
#11443=VERTEX_POINT('',#125640);
#11444=VERTEX_POINT('',#125642);
#11445=VERTEX_POINT('',#125644);
#11446=VERTEX_POINT('',#125648);
#11447=VERTEX_POINT('',#125649);
#11448=VERTEX_POINT('',#125653);
#11449=VERTEX_POINT('',#125655);
#11450=VERTEX_POINT('',#125657);
#11451=VERTEX_POINT('',#125662);
#11452=VERTEX_POINT('',#125664);
#11453=VERTEX_POINT('',#125675);
#11454=VERTEX_POINT('',#125677);
#11455=VERTEX_POINT('',#125704);
#11456=VERTEX_POINT('',#125706);
#11457=VERTEX_POINT('',#125717);
#11458=VERTEX_POINT('',#125719);
#11459=VERTEX_POINT('',#125726);
#11460=VERTEX_POINT('',#125728);
#11461=VERTEX_POINT('',#125735);
#11462=VERTEX_POINT('',#125737);
#11463=VERTEX_POINT('',#125744);
#11464=VERTEX_POINT('',#125746);
#11465=VERTEX_POINT('',#125763);
#11466=VERTEX_POINT('',#125765);
#11467=VERTEX_POINT('',#125792);
#11468=VERTEX_POINT('',#125794);
#11469=VERTEX_POINT('',#125811);
#11470=VERTEX_POINT('',#125813);
#11471=VERTEX_POINT('',#125815);
#11472=VERTEX_POINT('',#125817);
#11473=VERTEX_POINT('',#125834);
#11474=VERTEX_POINT('',#125836);
#11475=VERTEX_POINT('',#125863);
#11476=VERTEX_POINT('',#125865);
#11477=VERTEX_POINT('',#125882);
#11478=VERTEX_POINT('',#125884);
#11479=VERTEX_POINT('',#125893);
#11480=VERTEX_POINT('',#125895);
#11481=VERTEX_POINT('',#125902);
#11482=VERTEX_POINT('',#125904);
#11483=VERTEX_POINT('',#125915);
#11484=VERTEX_POINT('',#125917);
#11485=VERTEX_POINT('',#125932);
#11486=VERTEX_POINT('',#125934);
#11487=VERTEX_POINT('',#125966);
#11488=VERTEX_POINT('',#125968);
#11489=VERTEX_POINT('',#125983);
#11490=VERTEX_POINT('',#125985);
#11491=VERTEX_POINT('',#125992);
#11492=VERTEX_POINT('',#125996);
#11493=VERTEX_POINT('',#126005);
#11494=VERTEX_POINT('',#126007);
#11495=VERTEX_POINT('',#126014);
#11496=VERTEX_POINT('',#126016);
#11497=VERTEX_POINT('',#126027);
#11498=VERTEX_POINT('',#126029);
#11499=VERTEX_POINT('',#126036);
#11500=VERTEX_POINT('',#126038);
#11501=VERTEX_POINT('',#126045);
#11502=VERTEX_POINT('',#126054);
#11503=VERTEX_POINT('',#126055);
#11504=VERTEX_POINT('',#126059);
#11505=VERTEX_POINT('',#126061);
#11506=VERTEX_POINT('',#126063);
#11507=VERTEX_POINT('',#126068);
#11508=VERTEX_POINT('',#126070);
#11509=VERTEX_POINT('',#126081);
#11510=VERTEX_POINT('',#126083);
#11511=VERTEX_POINT('',#126110);
#11512=VERTEX_POINT('',#126112);
#11513=VERTEX_POINT('',#126123);
#11514=VERTEX_POINT('',#126125);
#11515=VERTEX_POINT('',#126132);
#11516=VERTEX_POINT('',#126134);
#11517=VERTEX_POINT('',#126141);
#11518=VERTEX_POINT('',#126143);
#11519=VERTEX_POINT('',#126150);
#11520=VERTEX_POINT('',#126152);
#11521=VERTEX_POINT('',#126169);
#11522=VERTEX_POINT('',#126171);
#11523=VERTEX_POINT('',#126198);
#11524=VERTEX_POINT('',#126200);
#11525=VERTEX_POINT('',#126217);
#11526=VERTEX_POINT('',#126219);
#11527=VERTEX_POINT('',#126221);
#11528=VERTEX_POINT('',#126223);
#11529=VERTEX_POINT('',#126240);
#11530=VERTEX_POINT('',#126242);
#11531=VERTEX_POINT('',#126269);
#11532=VERTEX_POINT('',#126271);
#11533=VERTEX_POINT('',#126288);
#11534=VERTEX_POINT('',#126290);
#11535=VERTEX_POINT('',#126299);
#11536=VERTEX_POINT('',#126301);
#11537=VERTEX_POINT('',#126308);
#11538=VERTEX_POINT('',#126310);
#11539=VERTEX_POINT('',#126321);
#11540=VERTEX_POINT('',#126323);
#11541=VERTEX_POINT('',#126338);
#11542=VERTEX_POINT('',#126340);
#11543=VERTEX_POINT('',#126372);
#11544=VERTEX_POINT('',#126374);
#11545=VERTEX_POINT('',#126389);
#11546=VERTEX_POINT('',#126391);
#11547=VERTEX_POINT('',#126398);
#11548=VERTEX_POINT('',#126402);
#11549=VERTEX_POINT('',#126411);
#11550=VERTEX_POINT('',#126413);
#11551=VERTEX_POINT('',#126420);
#11552=VERTEX_POINT('',#126422);
#11553=VERTEX_POINT('',#126433);
#11554=VERTEX_POINT('',#126435);
#11555=VERTEX_POINT('',#126442);
#11556=VERTEX_POINT('',#126444);
#11557=VERTEX_POINT('',#126451);
#11558=VERTEX_POINT('',#126460);
#11559=VERTEX_POINT('',#126461);
#11560=VERTEX_POINT('',#126465);
#11561=VERTEX_POINT('',#126467);
#11562=VERTEX_POINT('',#126469);
#11563=VERTEX_POINT('',#126474);
#11564=VERTEX_POINT('',#126476);
#11565=VERTEX_POINT('',#126489);
#11566=VERTEX_POINT('',#126491);
#11567=VERTEX_POINT('',#126518);
#11568=VERTEX_POINT('',#126520);
#11569=VERTEX_POINT('',#126533);
#11570=VERTEX_POINT('',#126535);
#11571=VERTEX_POINT('',#126542);
#11572=VERTEX_POINT('',#126544);
#11573=VERTEX_POINT('',#126551);
#11574=VERTEX_POINT('',#126553);
#11575=VERTEX_POINT('',#126560);
#11576=VERTEX_POINT('',#126562);
#11577=VERTEX_POINT('',#126579);
#11578=VERTEX_POINT('',#126581);
#11579=VERTEX_POINT('',#126608);
#11580=VERTEX_POINT('',#126610);
#11581=VERTEX_POINT('',#126627);
#11582=VERTEX_POINT('',#126629);
#11583=VERTEX_POINT('',#126631);
#11584=VERTEX_POINT('',#126633);
#11585=VERTEX_POINT('',#126650);
#11586=VERTEX_POINT('',#126652);
#11587=VERTEX_POINT('',#126679);
#11588=VERTEX_POINT('',#126681);
#11589=VERTEX_POINT('',#126698);
#11590=VERTEX_POINT('',#126700);
#11591=VERTEX_POINT('',#126709);
#11592=VERTEX_POINT('',#126711);
#11593=VERTEX_POINT('',#126718);
#11594=VERTEX_POINT('',#126720);
#11595=VERTEX_POINT('',#126731);
#11596=VERTEX_POINT('',#126733);
#11597=VERTEX_POINT('',#126748);
#11598=VERTEX_POINT('',#126750);
#11599=VERTEX_POINT('',#126782);
#11600=VERTEX_POINT('',#126784);
#11601=VERTEX_POINT('',#126799);
#11602=VERTEX_POINT('',#126801);
#11603=VERTEX_POINT('',#126808);
#11604=VERTEX_POINT('',#126812);
#11605=VERTEX_POINT('',#126821);
#11606=VERTEX_POINT('',#126823);
#11607=VERTEX_POINT('',#126830);
#11608=VERTEX_POINT('',#126832);
#11609=VERTEX_POINT('',#126843);
#11610=VERTEX_POINT('',#126845);
#11611=VERTEX_POINT('',#126852);
#11612=VERTEX_POINT('',#126854);
#11613=VERTEX_POINT('',#126861);
#11614=VERTEX_POINT('',#126870);
#11615=VERTEX_POINT('',#126872);
#11616=VERTEX_POINT('',#126874);
#11617=VERTEX_POINT('',#126876);
#11618=VERTEX_POINT('',#126882);
#11619=VERTEX_POINT('',#126886);
#11620=VERTEX_POINT('',#126892);
#11621=VERTEX_POINT('',#126896);
#11622=VERTEX_POINT('',#126902);
#11623=VERTEX_POINT('',#126906);
#11624=VERTEX_POINT('',#126912);
#11625=VERTEX_POINT('',#126916);
#11626=VERTEX_POINT('',#126922);
#11627=VERTEX_POINT('',#126926);
#11628=VERTEX_POINT('',#126932);
#11629=VERTEX_POINT('',#126936);
#11630=VERTEX_POINT('',#126942);
#11631=VERTEX_POINT('',#126946);
#11632=VERTEX_POINT('',#126952);
#11633=VERTEX_POINT('',#126956);
#11634=VERTEX_POINT('',#126962);
#11635=VERTEX_POINT('',#126966);
#11636=VERTEX_POINT('',#126972);
#11637=VERTEX_POINT('',#126976);
#11638=VERTEX_POINT('',#126982);
#11639=VERTEX_POINT('',#126986);
#11640=VERTEX_POINT('',#126994);
#11641=VERTEX_POINT('',#126996);
#11642=VERTEX_POINT('',#126998);
#11643=VERTEX_POINT('',#127000);
#11644=VERTEX_POINT('',#127004);
#11645=VERTEX_POINT('',#127012);
#11646=VERTEX_POINT('',#127020);
#11647=VERTEX_POINT('',#127028);
#11648=VERTEX_POINT('',#127036);
#11649=VERTEX_POINT('',#127044);
#11650=VERTEX_POINT('',#127052);
#11651=VERTEX_POINT('',#127060);
#11652=VERTEX_POINT('',#127068);
#11653=VERTEX_POINT('',#127076);
#11654=VERTEX_POINT('',#127084);
#11655=VERTEX_POINT('',#127092);
#11656=VERTEX_POINT('',#127094);
#11657=VERTEX_POINT('',#127098);
#11658=VERTEX_POINT('',#127100);
#11659=VERTEX_POINT('',#127104);
#11660=VERTEX_POINT('',#127106);
#11661=VERTEX_POINT('',#127110);
#11662=VERTEX_POINT('',#127111);
#11663=VERTEX_POINT('',#127113);
#11664=VERTEX_POINT('',#127115);
#11665=VERTEX_POINT('',#127119);
#11666=VERTEX_POINT('',#127121);
#11667=VERTEX_POINT('',#127125);
#11668=VERTEX_POINT('',#127127);
#11669=VERTEX_POINT('',#127131);
#11670=VERTEX_POINT('',#127133);
#11671=VERTEX_POINT('',#127162);
#11672=VERTEX_POINT('',#127164);
#11673=VERTEX_POINT('',#127168);
#11674=VERTEX_POINT('',#127170);
#11675=VERTEX_POINT('',#127174);
#11676=VERTEX_POINT('',#127176);
#11677=VERTEX_POINT('',#127180);
#11678=VERTEX_POINT('',#127182);
#11679=VERTEX_POINT('',#127186);
#11680=VERTEX_POINT('',#127188);
#11681=VERTEX_POINT('',#127192);
#11682=VERTEX_POINT('',#127194);
#11683=VERTEX_POINT('',#127198);
#11684=VERTEX_POINT('',#127200);
#11685=VERTEX_POINT('',#127204);
#11686=VERTEX_POINT('',#127206);
#11687=VERTEX_POINT('',#127210);
#11688=VERTEX_POINT('',#127212);
#11689=VERTEX_POINT('',#127216);
#11690=VERTEX_POINT('',#127218);
#11691=VERTEX_POINT('',#127222);
#11692=VERTEX_POINT('',#127224);
#11693=VERTEX_POINT('',#127228);
#11694=VERTEX_POINT('',#127230);
#11695=VERTEX_POINT('',#127234);
#11696=VERTEX_POINT('',#127236);
#11697=VERTEX_POINT('',#127240);
#11698=VERTEX_POINT('',#127242);
#11699=VERTEX_POINT('',#127246);
#11700=VERTEX_POINT('',#127248);
#11701=VERTEX_POINT('',#127252);
#11702=VERTEX_POINT('',#127254);
#11703=VERTEX_POINT('',#127258);
#11704=VERTEX_POINT('',#127260);
#11705=VERTEX_POINT('',#127264);
#11706=VERTEX_POINT('',#127266);
#11707=VERTEX_POINT('',#127273);
#11708=VERTEX_POINT('',#127275);
#11709=VERTEX_POINT('',#127279);
#11710=VERTEX_POINT('',#127281);
#11711=VERTEX_POINT('',#127285);
#11712=VERTEX_POINT('',#127287);
#11713=VERTEX_POINT('',#127291);
#11714=VERTEX_POINT('',#127296);
#11715=VERTEX_POINT('',#127300);
#11716=VERTEX_POINT('',#127304);
#11717=VERTEX_POINT('',#127308);
#11718=VERTEX_POINT('',#127312);
#11719=VERTEX_POINT('',#127316);
#11720=VERTEX_POINT('',#127320);
#11721=VERTEX_POINT('',#127324);
#11722=VERTEX_POINT('',#127328);
#11723=VERTEX_POINT('',#127332);
#11724=VERTEX_POINT('',#127338);
#11725=VERTEX_POINT('',#127340);
#11726=VERTEX_POINT('',#127344);
#11727=VERTEX_POINT('',#127346);
#11728=VERTEX_POINT('',#127350);
#11729=VERTEX_POINT('',#127352);
#11730=VERTEX_POINT('',#127356);
#11731=VERTEX_POINT('',#127358);
#11732=VERTEX_POINT('',#127362);
#11733=VERTEX_POINT('',#127364);
#11734=VERTEX_POINT('',#127368);
#11735=VERTEX_POINT('',#127370);
#11736=VERTEX_POINT('',#127374);
#11737=VERTEX_POINT('',#127376);
#11738=VERTEX_POINT('',#127380);
#11739=VERTEX_POINT('',#127382);
#11740=VERTEX_POINT('',#127386);
#11741=VERTEX_POINT('',#127388);
#11742=VERTEX_POINT('',#127392);
#11743=VERTEX_POINT('',#127394);
#11744=VERTEX_POINT('',#127398);
#11745=VERTEX_POINT('',#127400);
#11746=VERTEX_POINT('',#127404);
#11747=VERTEX_POINT('',#127406);
#11748=VERTEX_POINT('',#127410);
#11749=VERTEX_POINT('',#127412);
#11750=VERTEX_POINT('',#127416);
#11751=VERTEX_POINT('',#127418);
#11752=VERTEX_POINT('',#127422);
#11753=VERTEX_POINT('',#127424);
#11754=VERTEX_POINT('',#127428);
#11755=VERTEX_POINT('',#127430);
#11756=VERTEX_POINT('',#127434);
#11757=VERTEX_POINT('',#127436);
#11758=VERTEX_POINT('',#127440);
#11759=VERTEX_POINT('',#127442);
#11760=VERTEX_POINT('',#127454);
#11761=VERTEX_POINT('',#127455);
#11762=VERTEX_POINT('',#127457);
#11763=VERTEX_POINT('',#127461);
#11764=VERTEX_POINT('',#127462);
#11765=VERTEX_POINT('',#127464);
#11766=VERTEX_POINT('',#127468);
#11767=VERTEX_POINT('',#127472);
#11768=VERTEX_POINT('',#127473);
#11769=VERTEX_POINT('',#127475);
#11770=VERTEX_POINT('',#127477);
#11771=VERTEX_POINT('',#127481);
#11772=VERTEX_POINT('',#127482);
#11773=VERTEX_POINT('',#127484);
#11774=VERTEX_POINT('',#127486);
#11775=VERTEX_POINT('',#127488);
#11776=VERTEX_POINT('',#127490);
#11777=VERTEX_POINT('',#127493);
#11778=VERTEX_POINT('',#127495);
#11779=VERTEX_POINT('',#127497);
#11780=VERTEX_POINT('',#127499);
#11781=VERTEX_POINT('',#127501);
#11782=VERTEX_POINT('',#127503);
#11783=VERTEX_POINT('',#127505);
#11784=VERTEX_POINT('',#127507);
#11785=VERTEX_POINT('',#127511);
#11786=VERTEX_POINT('',#127512);
#11787=VERTEX_POINT('',#127517);
#11788=VERTEX_POINT('',#127521);
#11789=VERTEX_POINT('',#127523);
#11790=VERTEX_POINT('',#127525);
#11791=VERTEX_POINT('',#127527);
#11792=VERTEX_POINT('',#127529);
#11793=VERTEX_POINT('',#127531);
#11794=VERTEX_POINT('',#127534);
#11795=VERTEX_POINT('',#127536);
#11796=VERTEX_POINT('',#127538);
#11797=VERTEX_POINT('',#127540);
#11798=VERTEX_POINT('',#127542);
#11799=VERTEX_POINT('',#127544);
#11800=VERTEX_POINT('',#127546);
#11801=VERTEX_POINT('',#127548);
#11802=VERTEX_POINT('',#127550);
#11803=VERTEX_POINT('',#127552);
#11804=VERTEX_POINT('',#127554);
#11805=VERTEX_POINT('',#127564);
#11806=VERTEX_POINT('',#127565);
#11807=VERTEX_POINT('',#127567);
#11808=VERTEX_POINT('',#127569);
#11809=VERTEX_POINT('',#127585);
#11810=VERTEX_POINT('',#127587);
#11811=VERTEX_POINT('',#127591);
#11812=VERTEX_POINT('',#127595);
#11813=VERTEX_POINT('',#127602);
#11814=VERTEX_POINT('',#127603);
#11815=VERTEX_POINT('',#127605);
#11816=VERTEX_POINT('',#127607);
#11817=VERTEX_POINT('',#127609);
#11818=VERTEX_POINT('',#127613);
#11819=VERTEX_POINT('',#127614);
#11820=VERTEX_POINT('',#127616);
#11821=VERTEX_POINT('',#127618);
#11822=VERTEX_POINT('',#127620);
#11823=VERTEX_POINT('',#127640);
#11824=VERTEX_POINT('',#127641);
#11825=VERTEX_POINT('',#127643);
#11826=VERTEX_POINT('',#127647);
#11827=VERTEX_POINT('',#127648);
#11828=VERTEX_POINT('',#127650);
#11829=VERTEX_POINT('',#127654);
#11830=VERTEX_POINT('',#127658);
#11831=VERTEX_POINT('',#127660);
#11832=VERTEX_POINT('',#127665);
#11833=VERTEX_POINT('',#127666);
#11834=VERTEX_POINT('',#127668);
#11835=VERTEX_POINT('',#127670);
#11836=VERTEX_POINT('',#127674);
#11837=VERTEX_POINT('',#127676);
#11838=VERTEX_POINT('',#127678);
#11839=VERTEX_POINT('',#127680);
#11840=VERTEX_POINT('',#127682);
#11841=VERTEX_POINT('',#127684);
#11842=VERTEX_POINT('',#127686);
#11843=VERTEX_POINT('',#127688);
#11844=VERTEX_POINT('',#127690);
#11845=VERTEX_POINT('',#127693);
#11846=VERTEX_POINT('',#127695);
#11847=VERTEX_POINT('',#127697);
#11848=VERTEX_POINT('',#127705);
#11849=VERTEX_POINT('',#127706);
#11850=VERTEX_POINT('',#127711);
#11851=VERTEX_POINT('',#127715);
#11852=VERTEX_POINT('',#127717);
#11853=VERTEX_POINT('',#127719);
#11854=VERTEX_POINT('',#127721);
#11855=VERTEX_POINT('',#127723);
#11856=VERTEX_POINT('',#127725);
#11857=VERTEX_POINT('',#127727);
#11858=VERTEX_POINT('',#127729);
#11859=VERTEX_POINT('',#127731);
#11860=VERTEX_POINT('',#127733);
#11861=VERTEX_POINT('',#127735);
#11862=VERTEX_POINT('',#127738);
#11863=VERTEX_POINT('',#127740);
#11864=VERTEX_POINT('',#127742);
#11865=VERTEX_POINT('',#127744);
#11866=VERTEX_POINT('',#127746);
#11867=VERTEX_POINT('',#127748);
#11868=VERTEX_POINT('',#127752);
#11869=VERTEX_POINT('',#127763);
#11870=VERTEX_POINT('',#127764);
#11871=VERTEX_POINT('',#127766);
#11872=VERTEX_POINT('',#127768);
#11873=VERTEX_POINT('',#127781);
#11874=VERTEX_POINT('',#127783);
#11875=VERTEX_POINT('',#127787);
#11876=VERTEX_POINT('',#127791);
#11877=VERTEX_POINT('',#127799);
#11878=VERTEX_POINT('',#127803);
#11879=VERTEX_POINT('',#127804);
#11880=VERTEX_POINT('',#127809);
#11881=VERTEX_POINT('',#127811);
#11882=VERTEX_POINT('',#127813);
#11883=VERTEX_POINT('',#127817);
#11884=VERTEX_POINT('',#127819);
#11885=VERTEX_POINT('',#127821);
#11886=VERTEX_POINT('',#127843);
#11887=VERTEX_POINT('',#127845);
#11888=VERTEX_POINT('',#127849);
#11889=VERTEX_POINT('',#127850);
#11890=VERTEX_POINT('',#127852);
#11891=VERTEX_POINT('',#127854);
#11892=VERTEX_POINT('',#127858);
#11893=VERTEX_POINT('',#127860);
#11894=VERTEX_POINT('',#127864);
#11895=VERTEX_POINT('',#127866);
#11896=VERTEX_POINT('',#127870);
#11897=VERTEX_POINT('',#127872);
#11898=VERTEX_POINT('',#127876);
#11899=VERTEX_POINT('',#127878);
#11900=VERTEX_POINT('',#127882);
#11901=VERTEX_POINT('',#127884);
#11902=VERTEX_POINT('',#127888);
#11903=VERTEX_POINT('',#127890);
#11904=VERTEX_POINT('',#127894);
#11905=VERTEX_POINT('',#127896);
#11906=VERTEX_POINT('',#127900);
#11907=VERTEX_POINT('',#127902);
#11908=VERTEX_POINT('',#127906);
#11909=VERTEX_POINT('',#127908);
#11910=VERTEX_POINT('',#127912);
#11911=VERTEX_POINT('',#127914);
#11912=VERTEX_POINT('',#127918);
#11913=VERTEX_POINT('',#127920);
#11914=VERTEX_POINT('',#127924);
#11915=VERTEX_POINT('',#127926);
#11916=VERTEX_POINT('',#127930);
#11917=VERTEX_POINT('',#127932);
#11918=VERTEX_POINT('',#127936);
#11919=VERTEX_POINT('',#127938);
#11920=VERTEX_POINT('',#127942);
#11921=VERTEX_POINT('',#127944);
#11922=VERTEX_POINT('',#127948);
#11923=VERTEX_POINT('',#127950);
#11924=VERTEX_POINT('',#127954);
#11925=VERTEX_POINT('',#127956);
#11926=VERTEX_POINT('',#127960);
#11927=VERTEX_POINT('',#127962);
#11928=VERTEX_POINT('',#127966);
#11929=VERTEX_POINT('',#127968);
#11930=VERTEX_POINT('',#127972);
#11931=VERTEX_POINT('',#127974);
#11932=VERTEX_POINT('',#127978);
#11933=VERTEX_POINT('',#127980);
#11934=VERTEX_POINT('',#127984);
#11935=VERTEX_POINT('',#127986);
#11936=VERTEX_POINT('',#127990);
#11937=VERTEX_POINT('',#127992);
#11938=VERTEX_POINT('',#127996);
#11939=VERTEX_POINT('',#127998);
#11940=VERTEX_POINT('',#128002);
#11941=VERTEX_POINT('',#128004);
#11942=VERTEX_POINT('',#128008);
#11943=VERTEX_POINT('',#128010);
#11944=VERTEX_POINT('',#128014);
#11945=VERTEX_POINT('',#128016);
#11946=VERTEX_POINT('',#128020);
#11947=VERTEX_POINT('',#128022);
#11948=VERTEX_POINT('',#128026);
#11949=VERTEX_POINT('',#128028);
#11950=VERTEX_POINT('',#128032);
#11951=VERTEX_POINT('',#128034);
#11952=VERTEX_POINT('',#128038);
#11953=VERTEX_POINT('',#128040);
#11954=VERTEX_POINT('',#128044);
#11955=VERTEX_POINT('',#128046);
#11956=VERTEX_POINT('',#128050);
#11957=VERTEX_POINT('',#128052);
#11958=VERTEX_POINT('',#128056);
#11959=VERTEX_POINT('',#128058);
#11960=VERTEX_POINT('',#128062);
#11961=VERTEX_POINT('',#128064);
#11962=VERTEX_POINT('',#128068);
#11963=VERTEX_POINT('',#128070);
#11964=VERTEX_POINT('',#128074);
#11965=VERTEX_POINT('',#128076);
#11966=VERTEX_POINT('',#128080);
#11967=VERTEX_POINT('',#128082);
#11968=VERTEX_POINT('',#128086);
#11969=VERTEX_POINT('',#128088);
#11970=VERTEX_POINT('',#128092);
#11971=VERTEX_POINT('',#128094);
#11972=VERTEX_POINT('',#128098);
#11973=VERTEX_POINT('',#128100);
#11974=VERTEX_POINT('',#128104);
#11975=VERTEX_POINT('',#128106);
#11976=VERTEX_POINT('',#128110);
#11977=VERTEX_POINT('',#128112);
#11978=VERTEX_POINT('',#128116);
#11979=VERTEX_POINT('',#128118);
#11980=VERTEX_POINT('',#128122);
#11981=VERTEX_POINT('',#128124);
#11982=VERTEX_POINT('',#128128);
#11983=VERTEX_POINT('',#128130);
#11984=VERTEX_POINT('',#128134);
#11985=VERTEX_POINT('',#128136);
#11986=VERTEX_POINT('',#128140);
#11987=VERTEX_POINT('',#128142);
#11988=VERTEX_POINT('',#128146);
#11989=VERTEX_POINT('',#128148);
#11990=VERTEX_POINT('',#128152);
#11991=VERTEX_POINT('',#128154);
#11992=VERTEX_POINT('',#128158);
#11993=VERTEX_POINT('',#128160);
#11994=VERTEX_POINT('',#128164);
#11995=VERTEX_POINT('',#128166);
#11996=VERTEX_POINT('',#128170);
#11997=VERTEX_POINT('',#128172);
#11998=VERTEX_POINT('',#128176);
#11999=VERTEX_POINT('',#128178);
#12000=VERTEX_POINT('',#128182);
#12001=VERTEX_POINT('',#128184);
#12002=VERTEX_POINT('',#128188);
#12003=VERTEX_POINT('',#128190);
#12004=VERTEX_POINT('',#128194);
#12005=VERTEX_POINT('',#128196);
#12006=VERTEX_POINT('',#128200);
#12007=VERTEX_POINT('',#128202);
#12008=VERTEX_POINT('',#128206);
#12009=VERTEX_POINT('',#128208);
#12010=VERTEX_POINT('',#128212);
#12011=VERTEX_POINT('',#128214);
#12012=VERTEX_POINT('',#128218);
#12013=VERTEX_POINT('',#128220);
#12014=VERTEX_POINT('',#128224);
#12015=VERTEX_POINT('',#128226);
#12016=VERTEX_POINT('',#128230);
#12017=VERTEX_POINT('',#128232);
#12018=VERTEX_POINT('',#128236);
#12019=VERTEX_POINT('',#128238);
#12020=VERTEX_POINT('',#128242);
#12021=VERTEX_POINT('',#128244);
#12022=VERTEX_POINT('',#128248);
#12023=VERTEX_POINT('',#128250);
#12024=VERTEX_POINT('',#128254);
#12025=VERTEX_POINT('',#128256);
#12026=VERTEX_POINT('',#128260);
#12027=VERTEX_POINT('',#128262);
#12028=VERTEX_POINT('',#128266);
#12029=VERTEX_POINT('',#128268);
#12030=VERTEX_POINT('',#128272);
#12031=VERTEX_POINT('',#128274);
#12032=VERTEX_POINT('',#128278);
#12033=VERTEX_POINT('',#128280);
#12034=VERTEX_POINT('',#128284);
#12035=VERTEX_POINT('',#128286);
#12036=VERTEX_POINT('',#128290);
#12037=VERTEX_POINT('',#128292);
#12038=VERTEX_POINT('',#128296);
#12039=VERTEX_POINT('',#128298);
#12040=VERTEX_POINT('',#128302);
#12041=VERTEX_POINT('',#128304);
#12042=VERTEX_POINT('',#128308);
#12043=VERTEX_POINT('',#128310);
#12044=VERTEX_POINT('',#128314);
#12045=VERTEX_POINT('',#128316);
#12046=VERTEX_POINT('',#128320);
#12047=VERTEX_POINT('',#128322);
#12048=VERTEX_POINT('',#128326);
#12049=VERTEX_POINT('',#128328);
#12050=VERTEX_POINT('',#128332);
#12051=VERTEX_POINT('',#128334);
#12052=VERTEX_POINT('',#128338);
#12053=VERTEX_POINT('',#128340);
#12054=VERTEX_POINT('',#128344);
#12055=VERTEX_POINT('',#128346);
#12056=VERTEX_POINT('',#128350);
#12057=VERTEX_POINT('',#128352);
#12058=VERTEX_POINT('',#128356);
#12059=VERTEX_POINT('',#128358);
#12060=VERTEX_POINT('',#128362);
#12061=VERTEX_POINT('',#128364);
#12062=VERTEX_POINT('',#128368);
#12063=VERTEX_POINT('',#128370);
#12064=VERTEX_POINT('',#128374);
#12065=VERTEX_POINT('',#128376);
#12066=VERTEX_POINT('',#128380);
#12067=VERTEX_POINT('',#128382);
#12068=VERTEX_POINT('',#128386);
#12069=VERTEX_POINT('',#128388);
#12070=VERTEX_POINT('',#128392);
#12071=VERTEX_POINT('',#128394);
#12072=VERTEX_POINT('',#128404);
#12073=VERTEX_POINT('',#128405);
#12074=VERTEX_POINT('',#128407);
#12075=VERTEX_POINT('',#128436);
#12076=VERTEX_POINT('',#128443);
#12077=VERTEX_POINT('',#128444);
#12078=VERTEX_POINT('',#128446);
#12079=VERTEX_POINT('',#128502);
#12080=VERTEX_POINT('',#128703);
#12081=VERTEX_POINT('',#128704);
#12082=VERTEX_POINT('',#128706);
#12083=VERTEX_POINT('',#128906);
#12084=VERTEX_POINT('',#129147);
#12085=VERTEX_POINT('',#129148);
#12086=VERTEX_POINT('',#129150);
#12087=VERTEX_POINT('',#129387);
#12088=VERTEX_POINT('',#129443);
#12089=VERTEX_POINT('',#129444);
#12090=VERTEX_POINT('',#129446);
#12091=VERTEX_POINT('',#129475);
#12092=VERTEX_POINT('',#129482);
#12093=VERTEX_POINT('',#129483);
#12094=VERTEX_POINT('',#129485);
#12095=VERTEX_POINT('',#129541);
#12096=VERTEX_POINT('',#129742);
#12097=VERTEX_POINT('',#129743);
#12098=VERTEX_POINT('',#129745);
#12099=VERTEX_POINT('',#129945);
#12100=VERTEX_POINT('',#130186);
#12101=VERTEX_POINT('',#130187);
#12102=VERTEX_POINT('',#130189);
#12103=VERTEX_POINT('',#130426);
#12104=VERTEX_POINT('',#130482);
#12105=VERTEX_POINT('',#130483);
#12106=VERTEX_POINT('',#130485);
#12107=VERTEX_POINT('',#130494);
#12108=VERTEX_POINT('',#130553);
#12109=VERTEX_POINT('',#130555);
#12110=VERTEX_POINT('',#130570);
#12111=VERTEX_POINT('',#130571);
#12112=VERTEX_POINT('',#130573);
#12113=VERTEX_POINT('',#130589);
#12114=VERTEX_POINT('',#130721);
#12115=VERTEX_POINT('',#130722);
#12116=VERTEX_POINT('',#130724);
#12117=VERTEX_POINT('',#130855);
#12118=VERTEX_POINT('',#131054);
#12119=VERTEX_POINT('',#131055);
#12120=VERTEX_POINT('',#131057);
#12121=VERTEX_POINT('',#131255);
#12122=VERTEX_POINT('',#131335);
#12123=VERTEX_POINT('',#131336);
#12124=VERTEX_POINT('',#131338);
#12125=VERTEX_POINT('',#131536);
#12126=VERTEX_POINT('',#131671);
#12127=VERTEX_POINT('',#131672);
#12128=VERTEX_POINT('',#131674);
#12129=VERTEX_POINT('',#131753);
#12130=VERTEX_POINT('',#131833);
#12131=VERTEX_POINT('',#131834);
#12132=VERTEX_POINT('',#131836);
#12133=VERTEX_POINT('',#131967);
#12134=VERTEX_POINT('',#132103);
#12135=VERTEX_POINT('',#132104);
#12136=VERTEX_POINT('',#132106);
#12137=VERTEX_POINT('',#132185);
#12138=VERTEX_POINT('',#132378);
#12139=VERTEX_POINT('',#132379);
#12140=VERTEX_POINT('',#132381);
#12141=VERTEX_POINT('',#132516);
#12142=VERTEX_POINT('',#132712);
#12143=VERTEX_POINT('',#132713);
#12144=VERTEX_POINT('',#132715);
#12145=VERTEX_POINT('',#132794);
#12146=VERTEX_POINT('',#132874);
#12147=VERTEX_POINT('',#132875);
#12148=VERTEX_POINT('',#132877);
#12149=VERTEX_POINT('',#133008);
#12150=VERTEX_POINT('',#133141);
#12151=VERTEX_POINT('',#133142);
#12152=VERTEX_POINT('',#133144);
#12153=VERTEX_POINT('',#133223);
#12154=VERTEX_POINT('',#133419);
#12155=VERTEX_POINT('',#133420);
#12156=VERTEX_POINT('',#133422);
#12157=VERTEX_POINT('',#133553);
#12158=VERTEX_POINT('',#133752);
#12159=VERTEX_POINT('',#133753);
#12160=VERTEX_POINT('',#133755);
#12161=VERTEX_POINT('',#133837);
#12162=VERTEX_POINT('',#133917);
#12163=VERTEX_POINT('',#133918);
#12164=VERTEX_POINT('',#133920);
#12165=VERTEX_POINT('',#134051);
#12166=VERTEX_POINT('',#134186);
#12167=VERTEX_POINT('',#134187);
#12168=VERTEX_POINT('',#134189);
#12169=VERTEX_POINT('',#134387);
#12170=VERTEX_POINT('',#134467);
#12171=VERTEX_POINT('',#134468);
#12172=VERTEX_POINT('',#134470);
#12173=VERTEX_POINT('',#134665);
#12174=VERTEX_POINT('',#134800);
#12175=VERTEX_POINT('',#134801);
#12176=VERTEX_POINT('',#134803);
#12177=VERTEX_POINT('',#134882);
#12178=VERTEX_POINT('',#134959);
#12179=VERTEX_POINT('',#134960);
#12180=VERTEX_POINT('',#134962);
#12181=VERTEX_POINT('',#135097);
#12182=VERTEX_POINT('',#135229);
#12183=VERTEX_POINT('',#135230);
#12184=VERTEX_POINT('',#135232);
#12185=VERTEX_POINT('',#135430);
#12186=VERTEX_POINT('',#135510);
#12187=VERTEX_POINT('',#135511);
#12188=VERTEX_POINT('',#135513);
#12189=VERTEX_POINT('',#135708);
#12190=VERTEX_POINT('',#135841);
#12191=VERTEX_POINT('',#135842);
#12192=VERTEX_POINT('',#135844);
#12193=VERTEX_POINT('',#135924);
#12194=VERTEX_POINT('',#136004);
#12195=VERTEX_POINT('',#136005);
#12196=VERTEX_POINT('',#136007);
#12197=VERTEX_POINT('',#136138);
#12198=VERTEX_POINT('',#136270);
#12199=VERTEX_POINT('',#136271);
#12200=VERTEX_POINT('',#136273);
#12201=VERTEX_POINT('',#136352);
#12202=VERTEX_POINT('',#136551);
#12203=VERTEX_POINT('',#136552);
#12204=VERTEX_POINT('',#136554);
#12205=VERTEX_POINT('',#136685);
#12206=VERTEX_POINT('',#136884);
#12207=VERTEX_POINT('',#136885);
#12208=VERTEX_POINT('',#136887);
#12209=VERTEX_POINT('',#137085);
#12210=VERTEX_POINT('',#137165);
#12211=VERTEX_POINT('',#137166);
#12212=VERTEX_POINT('',#137168);
#12213=VERTEX_POINT('',#137247);
#12214=VERTEX_POINT('',#137263);
#12215=VERTEX_POINT('',#137264);
#12216=VERTEX_POINT('',#137266);
#12217=VERTEX_POINT('',#137275);
#12218=VERTEX_POINT('',#137334);
#12219=VERTEX_POINT('',#137336);
#12220=VERTEX_POINT('',#137351);
#12221=VERTEX_POINT('',#137352);
#12222=VERTEX_POINT('',#137354);
#12223=VERTEX_POINT('',#137370);
#12224=VERTEX_POINT('',#137502);
#12225=VERTEX_POINT('',#137503);
#12226=VERTEX_POINT('',#137505);
#12227=VERTEX_POINT('',#137636);
#12228=VERTEX_POINT('',#137835);
#12229=VERTEX_POINT('',#137836);
#12230=VERTEX_POINT('',#137838);
#12231=VERTEX_POINT('',#138036);
#12232=VERTEX_POINT('',#138116);
#12233=VERTEX_POINT('',#138117);
#12234=VERTEX_POINT('',#138119);
#12235=VERTEX_POINT('',#138317);
#12236=VERTEX_POINT('',#138452);
#12237=VERTEX_POINT('',#138453);
#12238=VERTEX_POINT('',#138455);
#12239=VERTEX_POINT('',#138534);
#12240=VERTEX_POINT('',#138614);
#12241=VERTEX_POINT('',#138615);
#12242=VERTEX_POINT('',#138617);
#12243=VERTEX_POINT('',#138748);
#12244=VERTEX_POINT('',#138884);
#12245=VERTEX_POINT('',#138885);
#12246=VERTEX_POINT('',#138887);
#12247=VERTEX_POINT('',#138966);
#12248=VERTEX_POINT('',#139159);
#12249=VERTEX_POINT('',#139160);
#12250=VERTEX_POINT('',#139162);
#12251=VERTEX_POINT('',#139297);
#12252=VERTEX_POINT('',#139493);
#12253=VERTEX_POINT('',#139494);
#12254=VERTEX_POINT('',#139496);
#12255=VERTEX_POINT('',#139575);
#12256=VERTEX_POINT('',#139655);
#12257=VERTEX_POINT('',#139656);
#12258=VERTEX_POINT('',#139658);
#12259=VERTEX_POINT('',#139789);
#12260=VERTEX_POINT('',#139922);
#12261=VERTEX_POINT('',#139923);
#12262=VERTEX_POINT('',#139925);
#12263=VERTEX_POINT('',#140004);
#12264=VERTEX_POINT('',#140200);
#12265=VERTEX_POINT('',#140201);
#12266=VERTEX_POINT('',#140203);
#12267=VERTEX_POINT('',#140334);
#12268=VERTEX_POINT('',#140533);
#12269=VERTEX_POINT('',#140534);
#12270=VERTEX_POINT('',#140536);
#12271=VERTEX_POINT('',#140618);
#12272=VERTEX_POINT('',#140698);
#12273=VERTEX_POINT('',#140699);
#12274=VERTEX_POINT('',#140701);
#12275=VERTEX_POINT('',#140832);
#12276=VERTEX_POINT('',#140967);
#12277=VERTEX_POINT('',#140968);
#12278=VERTEX_POINT('',#140970);
#12279=VERTEX_POINT('',#141168);
#12280=VERTEX_POINT('',#141248);
#12281=VERTEX_POINT('',#141249);
#12282=VERTEX_POINT('',#141251);
#12283=VERTEX_POINT('',#141446);
#12284=VERTEX_POINT('',#141581);
#12285=VERTEX_POINT('',#141582);
#12286=VERTEX_POINT('',#141584);
#12287=VERTEX_POINT('',#141663);
#12288=VERTEX_POINT('',#141740);
#12289=VERTEX_POINT('',#141741);
#12290=VERTEX_POINT('',#141743);
#12291=VERTEX_POINT('',#141878);
#12292=VERTEX_POINT('',#142010);
#12293=VERTEX_POINT('',#142011);
#12294=VERTEX_POINT('',#142013);
#12295=VERTEX_POINT('',#142211);
#12296=VERTEX_POINT('',#142291);
#12297=VERTEX_POINT('',#142292);
#12298=VERTEX_POINT('',#142294);
#12299=VERTEX_POINT('',#142489);
#12300=VERTEX_POINT('',#142622);
#12301=VERTEX_POINT('',#142623);
#12302=VERTEX_POINT('',#142625);
#12303=VERTEX_POINT('',#142705);
#12304=VERTEX_POINT('',#142785);
#12305=VERTEX_POINT('',#142786);
#12306=VERTEX_POINT('',#142788);
#12307=VERTEX_POINT('',#142919);
#12308=VERTEX_POINT('',#143051);
#12309=VERTEX_POINT('',#143052);
#12310=VERTEX_POINT('',#143054);
#12311=VERTEX_POINT('',#143133);
#12312=VERTEX_POINT('',#143332);
#12313=VERTEX_POINT('',#143333);
#12314=VERTEX_POINT('',#143335);
#12315=VERTEX_POINT('',#143466);
#12316=VERTEX_POINT('',#143665);
#12317=VERTEX_POINT('',#143666);
#12318=VERTEX_POINT('',#143668);
#12319=VERTEX_POINT('',#143866);
#12320=VERTEX_POINT('',#143946);
#12321=VERTEX_POINT('',#143947);
#12322=VERTEX_POINT('',#143949);
#12323=VERTEX_POINT('',#144028);
#12324=VERTEX_POINT('',#144044);
#12325=VERTEX_POINT('',#144045);
#12326=VERTEX_POINT('',#144047);
#12327=VERTEX_POINT('',#144056);
#12328=VERTEX_POINT('',#144115);
#12329=VERTEX_POINT('',#144117);
#12330=VERTEX_POINT('',#144132);
#12331=VERTEX_POINT('',#144133);
#12332=VERTEX_POINT('',#144135);
#12333=VERTEX_POINT('',#144151);
#12334=VERTEX_POINT('',#144283);
#12335=VERTEX_POINT('',#144284);
#12336=VERTEX_POINT('',#144286);
#12337=VERTEX_POINT('',#144417);
#12338=VERTEX_POINT('',#144616);
#12339=VERTEX_POINT('',#144617);
#12340=VERTEX_POINT('',#144619);
#12341=VERTEX_POINT('',#144817);
#12342=VERTEX_POINT('',#144897);
#12343=VERTEX_POINT('',#144898);
#12344=VERTEX_POINT('',#144900);
#12345=VERTEX_POINT('',#145098);
#12346=VERTEX_POINT('',#145233);
#12347=VERTEX_POINT('',#145234);
#12348=VERTEX_POINT('',#145236);
#12349=VERTEX_POINT('',#145315);
#12350=VERTEX_POINT('',#145395);
#12351=VERTEX_POINT('',#145396);
#12352=VERTEX_POINT('',#145398);
#12353=VERTEX_POINT('',#145529);
#12354=VERTEX_POINT('',#145665);
#12355=VERTEX_POINT('',#145666);
#12356=VERTEX_POINT('',#145668);
#12357=VERTEX_POINT('',#145747);
#12358=VERTEX_POINT('',#145940);
#12359=VERTEX_POINT('',#145941);
#12360=VERTEX_POINT('',#145943);
#12361=VERTEX_POINT('',#146078);
#12362=VERTEX_POINT('',#146274);
#12363=VERTEX_POINT('',#146275);
#12364=VERTEX_POINT('',#146277);
#12365=VERTEX_POINT('',#146356);
#12366=VERTEX_POINT('',#146436);
#12367=VERTEX_POINT('',#146437);
#12368=VERTEX_POINT('',#146439);
#12369=VERTEX_POINT('',#146570);
#12370=VERTEX_POINT('',#146703);
#12371=VERTEX_POINT('',#146704);
#12372=VERTEX_POINT('',#146706);
#12373=VERTEX_POINT('',#146785);
#12374=VERTEX_POINT('',#146981);
#12375=VERTEX_POINT('',#146982);
#12376=VERTEX_POINT('',#146984);
#12377=VERTEX_POINT('',#147115);
#12378=VERTEX_POINT('',#147314);
#12379=VERTEX_POINT('',#147315);
#12380=VERTEX_POINT('',#147317);
#12381=VERTEX_POINT('',#147399);
#12382=VERTEX_POINT('',#147479);
#12383=VERTEX_POINT('',#147480);
#12384=VERTEX_POINT('',#147482);
#12385=VERTEX_POINT('',#147613);
#12386=VERTEX_POINT('',#147748);
#12387=VERTEX_POINT('',#147749);
#12388=VERTEX_POINT('',#147751);
#12389=VERTEX_POINT('',#147949);
#12390=VERTEX_POINT('',#148029);
#12391=VERTEX_POINT('',#148030);
#12392=VERTEX_POINT('',#148032);
#12393=VERTEX_POINT('',#148227);
#12394=VERTEX_POINT('',#148362);
#12395=VERTEX_POINT('',#148363);
#12396=VERTEX_POINT('',#148365);
#12397=VERTEX_POINT('',#148444);
#12398=VERTEX_POINT('',#148521);
#12399=VERTEX_POINT('',#148522);
#12400=VERTEX_POINT('',#148524);
#12401=VERTEX_POINT('',#148659);
#12402=VERTEX_POINT('',#148791);
#12403=VERTEX_POINT('',#148792);
#12404=VERTEX_POINT('',#148794);
#12405=VERTEX_POINT('',#148992);
#12406=VERTEX_POINT('',#149072);
#12407=VERTEX_POINT('',#149073);
#12408=VERTEX_POINT('',#149075);
#12409=VERTEX_POINT('',#149270);
#12410=VERTEX_POINT('',#149403);
#12411=VERTEX_POINT('',#149404);
#12412=VERTEX_POINT('',#149406);
#12413=VERTEX_POINT('',#149486);
#12414=VERTEX_POINT('',#149566);
#12415=VERTEX_POINT('',#149567);
#12416=VERTEX_POINT('',#149569);
#12417=VERTEX_POINT('',#149700);
#12418=VERTEX_POINT('',#149832);
#12419=VERTEX_POINT('',#149833);
#12420=VERTEX_POINT('',#149835);
#12421=VERTEX_POINT('',#149914);
#12422=VERTEX_POINT('',#150113);
#12423=VERTEX_POINT('',#150114);
#12424=VERTEX_POINT('',#150116);
#12425=VERTEX_POINT('',#150247);
#12426=VERTEX_POINT('',#150446);
#12427=VERTEX_POINT('',#150447);
#12428=VERTEX_POINT('',#150449);
#12429=VERTEX_POINT('',#150647);
#12430=VERTEX_POINT('',#150727);
#12431=VERTEX_POINT('',#150728);
#12432=VERTEX_POINT('',#150730);
#12433=VERTEX_POINT('',#150809);
#12434=VERTEX_POINT('',#150825);
#12435=VERTEX_POINT('',#150826);
#12436=VERTEX_POINT('',#150828);
#12437=VERTEX_POINT('',#150837);
#12438=VERTEX_POINT('',#150896);
#12439=VERTEX_POINT('',#150898);
#12440=VERTEX_POINT('',#150913);
#12441=VERTEX_POINT('',#150914);
#12442=VERTEX_POINT('',#150916);
#12443=VERTEX_POINT('',#150932);
#12444=VERTEX_POINT('',#151064);
#12445=VERTEX_POINT('',#151065);
#12446=VERTEX_POINT('',#151067);
#12447=VERTEX_POINT('',#151198);
#12448=VERTEX_POINT('',#151397);
#12449=VERTEX_POINT('',#151398);
#12450=VERTEX_POINT('',#151400);
#12451=VERTEX_POINT('',#151598);
#12452=VERTEX_POINT('',#151678);
#12453=VERTEX_POINT('',#151679);
#12454=VERTEX_POINT('',#151681);
#12455=VERTEX_POINT('',#151879);
#12456=VERTEX_POINT('',#152014);
#12457=VERTEX_POINT('',#152015);
#12458=VERTEX_POINT('',#152017);
#12459=VERTEX_POINT('',#152096);
#12460=VERTEX_POINT('',#152176);
#12461=VERTEX_POINT('',#152177);
#12462=VERTEX_POINT('',#152179);
#12463=VERTEX_POINT('',#152310);
#12464=VERTEX_POINT('',#152446);
#12465=VERTEX_POINT('',#152447);
#12466=VERTEX_POINT('',#152449);
#12467=VERTEX_POINT('',#152528);
#12468=VERTEX_POINT('',#152721);
#12469=VERTEX_POINT('',#152722);
#12470=VERTEX_POINT('',#152724);
#12471=VERTEX_POINT('',#152859);
#12472=VERTEX_POINT('',#153055);
#12473=VERTEX_POINT('',#153056);
#12474=VERTEX_POINT('',#153058);
#12475=VERTEX_POINT('',#153137);
#12476=VERTEX_POINT('',#153217);
#12477=VERTEX_POINT('',#153218);
#12478=VERTEX_POINT('',#153220);
#12479=VERTEX_POINT('',#153351);
#12480=VERTEX_POINT('',#153484);
#12481=VERTEX_POINT('',#153485);
#12482=VERTEX_POINT('',#153487);
#12483=VERTEX_POINT('',#153566);
#12484=VERTEX_POINT('',#153762);
#12485=VERTEX_POINT('',#153763);
#12486=VERTEX_POINT('',#153765);
#12487=VERTEX_POINT('',#153896);
#12488=VERTEX_POINT('',#154095);
#12489=VERTEX_POINT('',#154096);
#12490=VERTEX_POINT('',#154098);
#12491=VERTEX_POINT('',#154180);
#12492=VERTEX_POINT('',#154260);
#12493=VERTEX_POINT('',#154261);
#12494=VERTEX_POINT('',#154263);
#12495=VERTEX_POINT('',#154394);
#12496=VERTEX_POINT('',#154529);
#12497=VERTEX_POINT('',#154530);
#12498=VERTEX_POINT('',#154532);
#12499=VERTEX_POINT('',#154730);
#12500=VERTEX_POINT('',#154810);
#12501=VERTEX_POINT('',#154811);
#12502=VERTEX_POINT('',#154813);
#12503=VERTEX_POINT('',#155008);
#12504=VERTEX_POINT('',#155143);
#12505=VERTEX_POINT('',#155144);
#12506=VERTEX_POINT('',#155146);
#12507=VERTEX_POINT('',#155225);
#12508=VERTEX_POINT('',#155302);
#12509=VERTEX_POINT('',#155303);
#12510=VERTEX_POINT('',#155305);
#12511=VERTEX_POINT('',#155440);
#12512=VERTEX_POINT('',#155572);
#12513=VERTEX_POINT('',#155573);
#12514=VERTEX_POINT('',#155575);
#12515=VERTEX_POINT('',#155773);
#12516=VERTEX_POINT('',#155853);
#12517=VERTEX_POINT('',#155854);
#12518=VERTEX_POINT('',#155856);
#12519=VERTEX_POINT('',#156051);
#12520=VERTEX_POINT('',#156184);
#12521=VERTEX_POINT('',#156185);
#12522=VERTEX_POINT('',#156187);
#12523=VERTEX_POINT('',#156267);
#12524=VERTEX_POINT('',#156347);
#12525=VERTEX_POINT('',#156348);
#12526=VERTEX_POINT('',#156350);
#12527=VERTEX_POINT('',#156481);
#12528=VERTEX_POINT('',#156613);
#12529=VERTEX_POINT('',#156614);
#12530=VERTEX_POINT('',#156616);
#12531=VERTEX_POINT('',#156695);
#12532=VERTEX_POINT('',#156894);
#12533=VERTEX_POINT('',#156895);
#12534=VERTEX_POINT('',#156897);
#12535=VERTEX_POINT('',#157028);
#12536=VERTEX_POINT('',#157227);
#12537=VERTEX_POINT('',#157228);
#12538=VERTEX_POINT('',#157230);
#12539=VERTEX_POINT('',#157428);
#12540=VERTEX_POINT('',#157508);
#12541=VERTEX_POINT('',#157509);
#12542=VERTEX_POINT('',#157511);
#12543=VERTEX_POINT('',#157590);
#12544=VERTEX_POINT('',#157606);
#12545=VERTEX_POINT('',#157607);
#12546=VERTEX_POINT('',#157609);
#12547=VERTEX_POINT('',#157628);
#12548=VERTEX_POINT('',#157629);
#12549=VERTEX_POINT('',#157685);
#12550=VERTEX_POINT('',#157740);
#12551=VERTEX_POINT('',#157741);
#12552=VERTEX_POINT('',#158028);
#12553=VERTEX_POINT('',#158029);
#12554=VERTEX_POINT('',#158314);
#12555=VERTEX_POINT('',#158315);
#12556=VERTEX_POINT('',#158317);
#12557=VERTEX_POINT('',#158333);
#12558=VERTEX_POINT('',#158370);
#12559=VERTEX_POINT('',#158371);
#12560=VERTEX_POINT('',#158656);
#12561=VERTEX_POINT('',#158657);
#12562=VERTEX_POINT('',#158946);
#12563=VERTEX_POINT('',#158947);
#12564=VERTEX_POINT('',#158949);
#12565=VERTEX_POINT('',#159058);
#12566=VERTEX_POINT('',#159059);
#12567=VERTEX_POINT('',#159061);
#12568=VERTEX_POINT('',#159072);
#12569=VERTEX_POINT('',#159242);
#12570=VERTEX_POINT('',#159244);
#12571=VERTEX_POINT('',#159390);
#12572=VERTEX_POINT('',#159391);
#12573=VERTEX_POINT('',#159393);
#12574=VERTEX_POINT('',#159826);
#12575=VERTEX_POINT('',#159827);
#12576=VERTEX_POINT('',#160069);
#12577=VERTEX_POINT('',#160285);
#12578=VERTEX_POINT('',#160286);
#12579=VERTEX_POINT('',#160288);
#12580=VERTEX_POINT('',#160557);
#12581=VERTEX_POINT('',#160587);
#12582=VERTEX_POINT('',#160588);
#12583=VERTEX_POINT('',#161059);
#12584=VERTEX_POINT('',#161060);
#12585=VERTEX_POINT('',#161062);
#12586=VERTEX_POINT('',#161301);
#12587=VERTEX_POINT('',#161549);
#12588=VERTEX_POINT('',#161550);
#12589=VERTEX_POINT('',#162067);
#12590=VERTEX_POINT('',#162068);
#12591=VERTEX_POINT('',#162070);
#12592=VERTEX_POINT('',#162305);
#12593=VERTEX_POINT('',#162546);
#12594=VERTEX_POINT('',#162547);
#12595=VERTEX_POINT('',#162781);
#12596=VERTEX_POINT('',#162965);
#12597=VERTEX_POINT('',#162966);
#12598=VERTEX_POINT('',#162968);
#12599=VERTEX_POINT('',#163203);
#12600=VERTEX_POINT('',#163233);
#12601=VERTEX_POINT('',#163234);
#12602=VERTEX_POINT('',#163691);
#12603=VERTEX_POINT('',#163692);
#12604=VERTEX_POINT('',#163694);
#12605=VERTEX_POINT('',#163920);
#12606=VERTEX_POINT('',#164154);
#12607=VERTEX_POINT('',#164155);
#12608=VERTEX_POINT('',#164157);
#12609=VERTEX_POINT('',#164454);
#12610=VERTEX_POINT('',#164455);
#12611=VERTEX_POINT('',#164457);
#12612=VERTEX_POINT('',#164665);
#12613=VERTEX_POINT('',#164895);
#12614=VERTEX_POINT('',#164896);
#12615=VERTEX_POINT('',#165130);
#12616=VERTEX_POINT('',#165318);
#12617=VERTEX_POINT('',#165319);
#12618=VERTEX_POINT('',#165321);
#12619=VERTEX_POINT('',#165584);
#12620=VERTEX_POINT('',#165616);
#12621=VERTEX_POINT('',#165617);
#12622=VERTEX_POINT('',#166080);
#12623=VERTEX_POINT('',#166081);
#12624=VERTEX_POINT('',#166083);
#12625=VERTEX_POINT('',#166306);
#12626=VERTEX_POINT('',#166548);
#12627=VERTEX_POINT('',#166549);
#12628=VERTEX_POINT('',#166551);
#12629=VERTEX_POINT('',#166791);
#12630=VERTEX_POINT('',#166792);
#12631=VERTEX_POINT('',#166794);
#12632=VERTEX_POINT('',#166981);
#12633=VERTEX_POINT('',#167223);
#12634=VERTEX_POINT('',#167224);
#12635=VERTEX_POINT('',#167691);
#12636=VERTEX_POINT('',#167692);
#12637=VERTEX_POINT('',#167694);
#12638=VERTEX_POINT('',#167945);
#12639=VERTEX_POINT('',#168201);
#12640=VERTEX_POINT('',#168202);
#12641=VERTEX_POINT('',#168671);
#12642=VERTEX_POINT('',#168672);
#12643=VERTEX_POINT('',#168674);
#12644=VERTEX_POINT('',#168905);
#12645=VERTEX_POINT('',#169137);
#12646=VERTEX_POINT('',#169138);
#12647=VERTEX_POINT('',#169140);
#12648=VERTEX_POINT('',#169436);
#12649=VERTEX_POINT('',#169437);
#12650=VERTEX_POINT('',#169673);
#12651=VERTEX_POINT('',#169914);
#12652=VERTEX_POINT('',#169915);
#12653=VERTEX_POINT('',#169917);
#12654=VERTEX_POINT('',#170153);
#12655=VERTEX_POINT('',#170349);
#12656=VERTEX_POINT('',#170350);
#12657=VERTEX_POINT('',#170352);
#12658=VERTEX_POINT('',#170363);
#12659=VERTEX_POINT('',#170533);
#12660=VERTEX_POINT('',#170535);
#12661=VERTEX_POINT('',#170681);
#12662=VERTEX_POINT('',#170682);
#12663=VERTEX_POINT('',#170684);
#12664=VERTEX_POINT('',#171117);
#12665=VERTEX_POINT('',#171118);
#12666=VERTEX_POINT('',#171356);
#12667=VERTEX_POINT('',#171572);
#12668=VERTEX_POINT('',#171573);
#12669=VERTEX_POINT('',#171575);
#12670=VERTEX_POINT('',#171846);
#12671=VERTEX_POINT('',#171876);
#12672=VERTEX_POINT('',#171877);
#12673=VERTEX_POINT('',#172348);
#12674=VERTEX_POINT('',#172349);
#12675=VERTEX_POINT('',#172351);
#12676=VERTEX_POINT('',#172580);
#12677=VERTEX_POINT('',#172830);
#12678=VERTEX_POINT('',#172831);
#12679=VERTEX_POINT('',#173336);
#12680=VERTEX_POINT('',#173337);
#12681=VERTEX_POINT('',#173339);
#12682=VERTEX_POINT('',#173580);
#12683=VERTEX_POINT('',#173817);
#12684=VERTEX_POINT('',#173818);
#12685=VERTEX_POINT('',#174098);
#12686=VERTEX_POINT('',#174282);
#12687=VERTEX_POINT('',#174283);
#12688=VERTEX_POINT('',#174285);
#12689=VERTEX_POINT('',#174520);
#12690=VERTEX_POINT('',#174550);
#12691=VERTEX_POINT('',#174551);
#12692=VERTEX_POINT('',#175008);
#12693=VERTEX_POINT('',#175009);
#12694=VERTEX_POINT('',#175011);
#12695=VERTEX_POINT('',#175239);
#12696=VERTEX_POINT('',#175471);
#12697=VERTEX_POINT('',#175472);
#12698=VERTEX_POINT('',#175474);
#12699=VERTEX_POINT('',#175771);
#12700=VERTEX_POINT('',#175772);
#12701=VERTEX_POINT('',#175774);
#12702=VERTEX_POINT('',#175982);
#12703=VERTEX_POINT('',#176222);
#12704=VERTEX_POINT('',#176223);
#12705=VERTEX_POINT('',#176459);
#12706=VERTEX_POINT('',#176647);
#12707=VERTEX_POINT('',#176648);
#12708=VERTEX_POINT('',#176650);
#12709=VERTEX_POINT('',#176901);
#12710=VERTEX_POINT('',#176933);
#12711=VERTEX_POINT('',#176934);
#12712=VERTEX_POINT('',#177401);
#12713=VERTEX_POINT('',#177402);
#12714=VERTEX_POINT('',#177404);
#12715=VERTEX_POINT('',#177625);
#12716=VERTEX_POINT('',#177869);
#12717=VERTEX_POINT('',#177870);
#12718=VERTEX_POINT('',#177872);
#12719=VERTEX_POINT('',#178112);
#12720=VERTEX_POINT('',#178113);
#12721=VERTEX_POINT('',#178115);
#12722=VERTEX_POINT('',#178302);
#12723=VERTEX_POINT('',#178544);
#12724=VERTEX_POINT('',#178545);
#12725=VERTEX_POINT('',#179014);
#12726=VERTEX_POINT('',#179015);
#12727=VERTEX_POINT('',#179017);
#12728=VERTEX_POINT('',#179264);
#12729=VERTEX_POINT('',#179544);
#12730=VERTEX_POINT('',#179545);
#12731=VERTEX_POINT('',#180014);
#12732=VERTEX_POINT('',#180015);
#12733=VERTEX_POINT('',#180017);
#12734=VERTEX_POINT('',#180248);
#12735=VERTEX_POINT('',#180478);
#12736=VERTEX_POINT('',#180479);
#12737=VERTEX_POINT('',#180481);
#12738=VERTEX_POINT('',#180747);
#12739=VERTEX_POINT('',#180748);
#12740=VERTEX_POINT('',#180984);
#12741=VERTEX_POINT('',#181225);
#12742=VERTEX_POINT('',#181226);
#12743=VERTEX_POINT('',#181228);
#12744=VERTEX_POINT('',#181464);
#12745=VERTEX_POINT('',#181660);
#12746=VERTEX_POINT('',#181661);
#12747=VERTEX_POINT('',#181663);
#12748=VERTEX_POINT('',#181674);
#12749=VERTEX_POINT('',#181844);
#12750=VERTEX_POINT('',#181846);
#12751=VERTEX_POINT('',#181992);
#12752=VERTEX_POINT('',#181993);
#12753=VERTEX_POINT('',#181995);
#12754=VERTEX_POINT('',#182428);
#12755=VERTEX_POINT('',#182429);
#12756=VERTEX_POINT('',#182671);
#12757=VERTEX_POINT('',#182887);
#12758=VERTEX_POINT('',#182888);
#12759=VERTEX_POINT('',#182890);
#12760=VERTEX_POINT('',#183157);
#12761=VERTEX_POINT('',#183189);
#12762=VERTEX_POINT('',#183190);
#12763=VERTEX_POINT('',#183649);
#12764=VERTEX_POINT('',#183650);
#12765=VERTEX_POINT('',#183652);
#12766=VERTEX_POINT('',#183881);
#12767=VERTEX_POINT('',#184131);
#12768=VERTEX_POINT('',#184132);
#12769=VERTEX_POINT('',#184641);
#12770=VERTEX_POINT('',#184642);
#12771=VERTEX_POINT('',#184644);
#12772=VERTEX_POINT('',#184877);
#12773=VERTEX_POINT('',#185112);
#12774=VERTEX_POINT('',#185113);
#12775=VERTEX_POINT('',#185351);
#12776=VERTEX_POINT('',#185535);
#12777=VERTEX_POINT('',#185536);
#12778=VERTEX_POINT('',#185538);
#12779=VERTEX_POINT('',#185773);
#12780=VERTEX_POINT('',#185803);
#12781=VERTEX_POINT('',#185804);
#12782=VERTEX_POINT('',#186263);
#12783=VERTEX_POINT('',#186264);
#12784=VERTEX_POINT('',#186266);
#12785=VERTEX_POINT('',#186494);
#12786=VERTEX_POINT('',#186726);
#12787=VERTEX_POINT('',#186727);
#12788=VERTEX_POINT('',#186729);
#12789=VERTEX_POINT('',#187050);
#12790=VERTEX_POINT('',#187051);
#12791=VERTEX_POINT('',#187053);
#12792=VERTEX_POINT('',#187261);
#12793=VERTEX_POINT('',#187535);
#12794=VERTEX_POINT('',#187536);
#12795=VERTEX_POINT('',#187808);
#12796=VERTEX_POINT('',#187996);
#12797=VERTEX_POINT('',#187997);
#12798=VERTEX_POINT('',#187999);
#12799=VERTEX_POINT('',#188264);
#12800=VERTEX_POINT('',#188296);
#12801=VERTEX_POINT('',#188297);
#12802=VERTEX_POINT('',#188760);
#12803=VERTEX_POINT('',#188761);
#12804=VERTEX_POINT('',#188763);
#12805=VERTEX_POINT('',#188984);
#12806=VERTEX_POINT('',#189228);
#12807=VERTEX_POINT('',#189229);
#12808=VERTEX_POINT('',#189231);
#12809=VERTEX_POINT('',#189471);
#12810=VERTEX_POINT('',#189472);
#12811=VERTEX_POINT('',#189474);
#12812=VERTEX_POINT('',#189661);
#12813=VERTEX_POINT('',#189903);
#12814=VERTEX_POINT('',#189904);
#12815=VERTEX_POINT('',#190379);
#12816=VERTEX_POINT('',#190380);
#12817=VERTEX_POINT('',#190382);
#12818=VERTEX_POINT('',#190633);
#12819=VERTEX_POINT('',#190889);
#12820=VERTEX_POINT('',#190890);
#12821=VERTEX_POINT('',#191363);
#12822=VERTEX_POINT('',#191364);
#12823=VERTEX_POINT('',#191366);
#12824=VERTEX_POINT('',#191589);
#12825=VERTEX_POINT('',#191821);
#12826=VERTEX_POINT('',#191822);
#12827=VERTEX_POINT('',#191824);
#12828=VERTEX_POINT('',#192076);
#12829=VERTEX_POINT('',#192077);
#12830=VERTEX_POINT('',#192313);
#12831=VERTEX_POINT('',#192556);
#12832=VERTEX_POINT('',#192557);
#12833=VERTEX_POINT('',#192559);
#12834=VERTEX_POINT('',#192795);
#12835=VERTEX_POINT('',#192991);
#12836=VERTEX_POINT('',#192992);
#12837=VERTEX_POINT('',#192994);
#12838=VERTEX_POINT('',#193005);
#12839=VERTEX_POINT('',#193175);
#12840=VERTEX_POINT('',#193177);
#12841=VERTEX_POINT('',#193323);
#12842=VERTEX_POINT('',#193324);
#12843=VERTEX_POINT('',#193326);
#12844=VERTEX_POINT('',#193759);
#12845=VERTEX_POINT('',#193760);
#12846=VERTEX_POINT('',#194000);
#12847=VERTEX_POINT('',#194216);
#12848=VERTEX_POINT('',#194217);
#12849=VERTEX_POINT('',#194219);
#12850=VERTEX_POINT('',#194488);
#12851=VERTEX_POINT('',#194520);
#12852=VERTEX_POINT('',#194521);
#12853=VERTEX_POINT('',#194982);
#12854=VERTEX_POINT('',#194983);
#12855=VERTEX_POINT('',#194985);
#12856=VERTEX_POINT('',#195214);
#12857=VERTEX_POINT('',#195460);
#12858=VERTEX_POINT('',#195461);
#12859=VERTEX_POINT('',#195952);
#12860=VERTEX_POINT('',#195953);
#12861=VERTEX_POINT('',#195955);
#12862=VERTEX_POINT('',#196190);
#12863=VERTEX_POINT('',#196423);
#12864=VERTEX_POINT('',#196424);
#12865=VERTEX_POINT('',#196708);
#12866=VERTEX_POINT('',#196892);
#12867=VERTEX_POINT('',#196893);
#12868=VERTEX_POINT('',#196895);
#12869=VERTEX_POINT('',#197130);
#12870=VERTEX_POINT('',#197160);
#12871=VERTEX_POINT('',#197161);
#12872=VERTEX_POINT('',#197626);
#12873=VERTEX_POINT('',#197627);
#12874=VERTEX_POINT('',#197629);
#12875=VERTEX_POINT('',#197857);
#12876=VERTEX_POINT('',#198091);
#12877=VERTEX_POINT('',#198092);
#12878=VERTEX_POINT('',#198094);
#12879=VERTEX_POINT('',#198389);
#12880=VERTEX_POINT('',#198390);
#12881=VERTEX_POINT('',#198392);
#12882=VERTEX_POINT('',#198600);
#12883=VERTEX_POINT('',#198840);
#12884=VERTEX_POINT('',#198841);
#12885=VERTEX_POINT('',#199077);
#12886=VERTEX_POINT('',#199265);
#12887=VERTEX_POINT('',#199266);
#12888=VERTEX_POINT('',#199268);
#12889=VERTEX_POINT('',#199527);
#12890=VERTEX_POINT('',#199559);
#12891=VERTEX_POINT('',#199560);
#12892=VERTEX_POINT('',#200025);
#12893=VERTEX_POINT('',#200026);
#12894=VERTEX_POINT('',#200028);
#12895=VERTEX_POINT('',#200253);
#12896=VERTEX_POINT('',#200493);
#12897=VERTEX_POINT('',#200494);
#12898=VERTEX_POINT('',#200496);
#12899=VERTEX_POINT('',#200736);
#12900=VERTEX_POINT('',#200737);
#12901=VERTEX_POINT('',#200739);
#12902=VERTEX_POINT('',#200926);
#12903=VERTEX_POINT('',#201214);
#12904=VERTEX_POINT('',#201215);
#12905=VERTEX_POINT('',#201692);
#12906=VERTEX_POINT('',#201693);
#12907=VERTEX_POINT('',#201695);
#12908=VERTEX_POINT('',#201944);
#12909=VERTEX_POINT('',#202220);
#12910=VERTEX_POINT('',#202221);
#12911=VERTEX_POINT('',#202694);
#12912=VERTEX_POINT('',#202695);
#12913=VERTEX_POINT('',#202697);
#12914=VERTEX_POINT('',#202912);
#12915=VERTEX_POINT('',#203140);
#12916=VERTEX_POINT('',#203141);
#12917=VERTEX_POINT('',#203143);
#12918=VERTEX_POINT('',#203437);
#12919=VERTEX_POINT('',#203438);
#12920=VERTEX_POINT('',#203674);
#12921=VERTEX_POINT('',#203913);
#12922=VERTEX_POINT('',#203914);
#12923=VERTEX_POINT('',#203916);
#12924=VERTEX_POINT('',#204152);
#12925=VERTEX_POINT('',#204348);
#12926=VERTEX_POINT('',#204509);
#12927=VERTEX_POINT('',#204618);
#12928=VERTEX_POINT('',#204779);
#12929=VERTEX_POINT('',#204888);
#12930=VERTEX_POINT('',#205049);
#12931=VERTEX_POINT('',#205158);
#12932=VERTEX_POINT('',#205319);
#12933=VERTEX_POINT('',#205428);
#12934=VERTEX_POINT('',#205447);
#12935=VERTEX_POINT('',#205463);
#12936=VERTEX_POINT('',#205500);
#12937=VERTEX_POINT('',#205508);
#12938=VERTEX_POINT('',#205567);
#12939=VERTEX_POINT('',#205569);
#12940=VERTEX_POINT('',#205582);
#12941=VERTEX_POINT('',#205590);
#12942=VERTEX_POINT('',#205649);
#12943=VERTEX_POINT('',#205651);
#12944=VERTEX_POINT('',#205664);
#12945=VERTEX_POINT('',#205672);
#12946=VERTEX_POINT('',#205731);
#12947=VERTEX_POINT('',#205733);
#12948=VERTEX_POINT('',#205746);
#12949=VERTEX_POINT('',#205754);
#12950=VERTEX_POINT('',#205813);
#12951=VERTEX_POINT('',#205815);
#12952=VERTEX_POINT('',#205828);
#12953=VERTEX_POINT('',#205835);
#12954=VERTEX_POINT('',#205990);
#12955=VERTEX_POINT('',#205992);
#12956=VERTEX_POINT('',#206048);
#12957=VERTEX_POINT('',#206055);
#12958=VERTEX_POINT('',#206210);
#12959=VERTEX_POINT('',#206212);
#12960=VERTEX_POINT('',#206268);
#12961=VERTEX_POINT('',#206270);
#12962=VERTEX_POINT('',#206275);
#12963=VERTEX_POINT('',#206276);
#12964=VERTEX_POINT('',#206278);
#12965=VERTEX_POINT('',#206280);
#12966=VERTEX_POINT('',#206284);
#12967=VERTEX_POINT('',#206286);
#12968=VERTEX_POINT('',#206288);
#12969=VERTEX_POINT('',#206292);
#12970=VERTEX_POINT('',#206294);
#12971=VERTEX_POINT('',#206299);
#12972=VERTEX_POINT('',#206300);
#12973=VERTEX_POINT('',#206302);
#12974=VERTEX_POINT('',#206304);
#12975=VERTEX_POINT('',#206308);
#12976=VERTEX_POINT('',#206309);
#12977=VERTEX_POINT('',#206311);
#12978=VERTEX_POINT('',#206316);
#12979=VERTEX_POINT('',#206318);
#12980=VERTEX_POINT('',#206323);
#12981=VERTEX_POINT('',#206325);
#12982=VERTEX_POINT('',#206329);
#12983=VERTEX_POINT('',#206331);
#12984=VERTEX_POINT('',#206333);
#12985=VERTEX_POINT('',#206337);
#12986=VERTEX_POINT('',#206342);
#12987=VERTEX_POINT('',#206344);
#12988=VERTEX_POINT('',#206346);
#12989=VERTEX_POINT('',#206348);
#12990=VERTEX_POINT('',#206350);
#12991=VERTEX_POINT('',#206352);
#12992=VERTEX_POINT('',#206354);
#12993=VERTEX_POINT('',#206356);
#12994=VERTEX_POINT('',#206358);
#12995=VERTEX_POINT('',#206360);
#12996=VERTEX_POINT('',#206362);
#12997=VERTEX_POINT('',#206364);
#12998=VERTEX_POINT('',#206366);
#12999=VERTEX_POINT('',#206368);
#13000=VERTEX_POINT('',#206370);
#13001=VERTEX_POINT('',#206372);
#13002=VERTEX_POINT('',#206374);
#13003=VERTEX_POINT('',#206376);
#13004=VERTEX_POINT('',#206378);
#13005=VERTEX_POINT('',#206380);
#13006=VERTEX_POINT('',#206382);
#13007=VERTEX_POINT('',#206384);
#13008=VERTEX_POINT('',#206386);
#13009=VERTEX_POINT('',#206388);
#13010=VERTEX_POINT('',#206390);
#13011=VERTEX_POINT('',#206392);
#13012=VERTEX_POINT('',#206394);
#13013=VERTEX_POINT('',#206397);
#13014=VERTEX_POINT('',#206399);
#13015=VERTEX_POINT('',#215197);
#13016=VERTEX_POINT('',#215198);
#13017=VERTEX_POINT('',#215200);
#13018=VERTEX_POINT('',#215202);
#13019=VERTEX_POINT('',#215206);
#13020=VERTEX_POINT('',#215208);
#13021=VERTEX_POINT('',#215212);
#13022=VERTEX_POINT('',#215214);
#13023=VERTEX_POINT('',#215218);
#13024=VERTEX_POINT('',#215220);
#13025=VERTEX_POINT('',#215224);
#13026=VERTEX_POINT('',#215226);
#13027=VERTEX_POINT('',#215230);
#13028=VERTEX_POINT('',#215232);
#13029=VERTEX_POINT('',#215239);
#13030=VERTEX_POINT('',#215241);
#13031=VERTEX_POINT('',#215246);
#13032=VERTEX_POINT('',#215247);
#13033=VERTEX_POINT('',#215249);
#13034=VERTEX_POINT('',#215251);
#13035=VERTEX_POINT('',#215255);
#13036=VERTEX_POINT('',#215257);
#13037=VERTEX_POINT('',#215261);
#13038=VERTEX_POINT('',#215263);
#13039=VERTEX_POINT('',#215273);
#13040=VERTEX_POINT('',#215275);
#13041=VERTEX_POINT('',#215278);
#13042=VERTEX_POINT('',#215279);
#13043=VERTEX_POINT('',#215281);
#13044=VERTEX_POINT('',#215283);
#13045=VERTEX_POINT('',#215287);
#13046=VERTEX_POINT('',#215289);
#13047=VERTEX_POINT('',#215293);
#13048=VERTEX_POINT('',#215295);
#13049=VERTEX_POINT('',#215299);
#13050=VERTEX_POINT('',#215301);
#13051=VERTEX_POINT('',#215305);
#13052=VERTEX_POINT('',#215307);
#13053=VERTEX_POINT('',#215311);
#13054=VERTEX_POINT('',#215313);
#13055=VERTEX_POINT('',#215320);
#13056=VERTEX_POINT('',#215322);
#13057=VERTEX_POINT('',#215329);
#13058=VERTEX_POINT('',#215335);
#13059=VERTEX_POINT('',#215340);
#13060=VERTEX_POINT('',#215341);
#13061=VERTEX_POINT('',#215343);
#13062=VERTEX_POINT('',#215345);
#13063=VERTEX_POINT('',#215349);
#13064=VERTEX_POINT('',#215351);
#13065=VERTEX_POINT('',#215355);
#13066=VERTEX_POINT('',#215357);
#13067=VERTEX_POINT('',#215367);
#13068=VERTEX_POINT('',#215369);
#13069=VERTEX_POINT('',#215372);
#13070=VERTEX_POINT('',#215373);
#13071=VERTEX_POINT('',#215375);
#13072=VERTEX_POINT('',#215377);
#13073=VERTEX_POINT('',#215381);
#13074=VERTEX_POINT('',#215383);
#13075=VERTEX_POINT('',#215387);
#13076=VERTEX_POINT('',#215389);
#13077=VERTEX_POINT('',#215393);
#13078=VERTEX_POINT('',#215395);
#13079=VERTEX_POINT('',#215399);
#13080=VERTEX_POINT('',#215401);
#13081=VERTEX_POINT('',#215405);
#13082=VERTEX_POINT('',#215407);
#13083=VERTEX_POINT('',#215414);
#13084=VERTEX_POINT('',#215416);
#13085=VERTEX_POINT('',#215421);
#13086=VERTEX_POINT('',#215422);
#13087=VERTEX_POINT('',#215424);
#13088=VERTEX_POINT('',#215426);
#13089=VERTEX_POINT('',#215430);
#13090=VERTEX_POINT('',#215432);
#13091=VERTEX_POINT('',#215436);
#13092=VERTEX_POINT('',#215438);
#13093=VERTEX_POINT('',#215442);
#13094=VERTEX_POINT('',#215444);
#13095=VERTEX_POINT('',#215448);
#13096=VERTEX_POINT('',#215450);
#13097=VERTEX_POINT('',#215454);
#13098=VERTEX_POINT('',#215456);
#13099=VERTEX_POINT('',#215463);
#13100=VERTEX_POINT('',#215465);
#13101=VERTEX_POINT('',#215472);
#13102=VERTEX_POINT('',#215474);
#13103=VERTEX_POINT('',#215479);
#13104=VERTEX_POINT('',#215484);
#13105=VERTEX_POINT('',#215489);
#13106=VERTEX_POINT('',#215494);
#13107=VERTEX_POINT('',#215499);
#13108=VERTEX_POINT('',#215505);
#13109=VERTEX_POINT('',#215509);
#13110=VERTEX_POINT('',#215513);
#13111=VERTEX_POINT('',#215517);
#13112=VERTEX_POINT('',#215521);
#13113=VERTEX_POINT('',#215525);
#13114=VERTEX_POINT('',#215531);
#13115=VERTEX_POINT('',#215535);
#13116=VERTEX_POINT('',#215539);
#13117=VERTEX_POINT('',#215543);
#13118=VERTEX_POINT('',#215547);
#13119=VERTEX_POINT('',#215551);
#13120=VERTEX_POINT('',#215555);
#13121=VERTEX_POINT('',#215559);
#13122=VERTEX_POINT('',#215563);
#13123=VERTEX_POINT('',#215567);
#13124=VERTEX_POINT('',#215571);
#13125=VERTEX_POINT('',#215575);
#13126=EDGE_CURVE('',#9986,#9987,#6296,.T.);
#13127=EDGE_CURVE('',#9987,#9988,#6297,.T.);
#13128=EDGE_CURVE('',#9988,#9989,#6298,.T.);
#13129=EDGE_CURVE('',#9989,#9990,#5664,.T.);
#13130=EDGE_CURVE('',#9990,#9991,#6299,.T.);
#13131=EDGE_CURVE('',#9991,#9992,#5665,.T.);
#13132=EDGE_CURVE('',#9992,#9993,#6300,.T.);
#13133=EDGE_CURVE('',#9993,#9994,#5666,.T.);
#13134=EDGE_CURVE('',#9994,#9995,#6301,.T.);
#13135=EDGE_CURVE('',#9995,#9996,#5667,.T.);
#13136=EDGE_CURVE('',#9996,#9997,#6302,.T.);
#13137=EDGE_CURVE('',#9997,#9998,#5668,.T.);
#13138=EDGE_CURVE('',#9998,#9999,#6303,.T.);
#13139=EDGE_CURVE('',#9999,#10000,#6304,.T.);
#13140=EDGE_CURVE('',#10000,#10001,#5669,.T.);
#13141=EDGE_CURVE('',#10001,#10002,#6305,.T.);
#13142=EDGE_CURVE('',#10002,#10003,#5670,.T.);
#13143=EDGE_CURVE('',#10003,#10004,#6306,.T.);
#13144=EDGE_CURVE('',#10004,#10005,#5671,.T.);
#13145=EDGE_CURVE('',#10005,#10006,#6307,.T.);
#13146=EDGE_CURVE('',#10006,#10007,#5672,.T.);
#13147=EDGE_CURVE('',#10007,#10008,#6308,.T.);
#13148=EDGE_CURVE('',#10008,#10009,#5673,.T.);
#13149=EDGE_CURVE('',#10009,#10010,#6309,.T.);
#13150=EDGE_CURVE('',#10010,#9986,#6310,.T.);
#13151=EDGE_CURVE('',#10011,#9987,#6311,.T.);
#13152=EDGE_CURVE('',#10012,#10011,#6312,.T.);
#13153=EDGE_CURVE('',#9988,#10012,#6313,.T.);
#13154=EDGE_CURVE('',#10013,#10012,#6314,.T.);
#13155=EDGE_CURVE('',#9989,#10013,#6315,.T.);
#13156=EDGE_CURVE('',#10014,#10013,#5674,.T.);
#13157=EDGE_CURVE('',#9990,#10014,#6316,.T.);
#13158=EDGE_CURVE('',#10015,#10014,#6317,.T.);
#13159=EDGE_CURVE('',#9991,#10015,#6318,.T.);
#13160=EDGE_CURVE('',#10016,#10015,#5675,.T.);
#13161=EDGE_CURVE('',#9992,#10016,#6319,.T.);
#13162=EDGE_CURVE('',#10017,#10016,#6320,.T.);
#13163=EDGE_CURVE('',#9993,#10017,#6321,.T.);
#13164=EDGE_CURVE('',#10018,#10017,#5676,.T.);
#13165=EDGE_CURVE('',#9994,#10018,#6322,.T.);
#13166=EDGE_CURVE('',#10019,#10018,#6323,.T.);
#13167=EDGE_CURVE('',#9995,#10019,#6324,.T.);
#13168=EDGE_CURVE('',#10020,#10019,#5677,.T.);
#13169=EDGE_CURVE('',#9996,#10020,#6325,.T.);
#13170=EDGE_CURVE('',#10021,#10020,#6326,.T.);
#13171=EDGE_CURVE('',#9997,#10021,#6327,.T.);
#13172=EDGE_CURVE('',#10022,#10021,#5678,.T.);
#13173=EDGE_CURVE('',#9998,#10022,#6328,.T.);
#13174=EDGE_CURVE('',#10023,#10022,#6329,.T.);
#13175=EDGE_CURVE('',#9999,#10023,#6330,.T.);
#13176=EDGE_CURVE('',#10024,#10023,#6331,.T.);
#13177=EDGE_CURVE('',#10000,#10024,#6332,.T.);
#13178=EDGE_CURVE('',#10025,#10024,#5679,.T.);
#13179=EDGE_CURVE('',#10001,#10025,#6333,.T.);
#13180=EDGE_CURVE('',#10026,#10025,#6334,.T.);
#13181=EDGE_CURVE('',#10002,#10026,#6335,.T.);
#13182=EDGE_CURVE('',#10027,#10026,#5680,.T.);
#13183=EDGE_CURVE('',#10003,#10027,#6336,.T.);
#13184=EDGE_CURVE('',#10028,#10027,#6337,.T.);
#13185=EDGE_CURVE('',#10004,#10028,#6338,.T.);
#13186=EDGE_CURVE('',#10029,#10028,#5681,.T.);
#13187=EDGE_CURVE('',#10005,#10029,#6339,.T.);
#13188=EDGE_CURVE('',#10030,#10029,#6340,.T.);
#13189=EDGE_CURVE('',#10006,#10030,#6341,.T.);
#13190=EDGE_CURVE('',#10031,#10030,#5682,.T.);
#13191=EDGE_CURVE('',#10007,#10031,#6342,.T.);
#13192=EDGE_CURVE('',#10032,#10031,#6343,.T.);
#13193=EDGE_CURVE('',#10008,#10032,#6344,.T.);
#13194=EDGE_CURVE('',#10033,#10032,#5683,.T.);
#13195=EDGE_CURVE('',#10009,#10033,#6345,.T.);
#13196=EDGE_CURVE('',#10034,#10033,#6346,.T.);
#13197=EDGE_CURVE('',#10010,#10034,#6347,.T.);
#13198=EDGE_CURVE('',#10035,#10034,#6348,.T.);
#13199=EDGE_CURVE('',#9986,#10035,#6349,.T.);
#13200=EDGE_CURVE('',#10011,#10035,#6350,.T.);
#13201=EDGE_CURVE('',#10036,#10037,#6351,.T.);
#13202=EDGE_CURVE('',#10037,#10038,#5684,.T.);
#13203=EDGE_CURVE('',#10038,#10039,#6352,.T.);
#13204=EDGE_CURVE('',#10039,#10040,#5685,.T.);
#13205=EDGE_CURVE('',#10040,#10041,#6353,.T.);
#13206=EDGE_CURVE('',#10041,#10042,#5686,.T.);
#13207=EDGE_CURVE('',#10042,#10043,#6354,.T.);
#13208=EDGE_CURVE('',#10043,#10044,#6355,.T.);
#13209=EDGE_CURVE('',#10044,#10045,#6356,.T.);
#13210=EDGE_CURVE('',#10045,#10046,#6357,.T.);
#13211=EDGE_CURVE('',#10046,#10047,#6358,.T.);
#13212=EDGE_CURVE('',#10047,#10048,#6359,.T.);
#13213=EDGE_CURVE('',#10048,#10049,#5687,.T.);
#13214=EDGE_CURVE('',#10049,#10050,#6360,.T.);
#13215=EDGE_CURVE('',#10050,#10051,#5688,.T.);
#13216=EDGE_CURVE('',#10051,#10052,#6361,.T.);
#13217=EDGE_CURVE('',#10052,#10053,#5689,.T.);
#13218=EDGE_CURVE('',#10053,#10054,#6362,.T.);
#13219=EDGE_CURVE('',#10054,#10055,#5690,.T.);
#13220=EDGE_CURVE('',#10055,#10056,#6363,.T.);
#13221=EDGE_CURVE('',#10056,#10057,#6364,.T.);
#13222=EDGE_CURVE('',#10057,#10058,#6365,.T.);
#13223=EDGE_CURVE('',#10058,#10059,#6366,.T.);
#13224=EDGE_CURVE('',#10059,#10060,#6367,.T.);
#13225=EDGE_CURVE('',#10060,#10061,#6368,.T.);
#13226=EDGE_CURVE('',#10061,#10036,#5691,.T.);
#13227=EDGE_CURVE('',#10062,#10037,#6369,.T.);
#13228=EDGE_CURVE('',#10063,#10062,#5692,.T.);
#13229=EDGE_CURVE('',#10038,#10063,#6370,.T.);
#13230=EDGE_CURVE('',#10064,#10063,#6371,.T.);
#13231=EDGE_CURVE('',#10039,#10064,#6372,.T.);
#13232=EDGE_CURVE('',#10065,#10064,#5693,.T.);
#13233=EDGE_CURVE('',#10040,#10065,#6373,.T.);
#13234=EDGE_CURVE('',#10066,#10065,#6374,.T.);
#13235=EDGE_CURVE('',#10041,#10066,#6375,.T.);
#13236=EDGE_CURVE('',#10067,#10066,#5694,.T.);
#13237=EDGE_CURVE('',#10042,#10067,#6376,.T.);
#13238=EDGE_CURVE('',#10068,#10067,#6377,.T.);
#13239=EDGE_CURVE('',#10043,#10068,#6378,.T.);
#13240=EDGE_CURVE('',#10069,#10068,#6379,.T.);
#13241=EDGE_CURVE('',#10044,#10069,#6380,.T.);
#13242=EDGE_CURVE('',#10070,#10069,#6381,.T.);
#13243=EDGE_CURVE('',#10045,#10070,#6382,.T.);
#13244=EDGE_CURVE('',#10071,#10070,#6383,.T.);
#13245=EDGE_CURVE('',#10046,#10071,#6384,.T.);
#13246=EDGE_CURVE('',#10072,#10071,#6385,.T.);
#13247=EDGE_CURVE('',#10047,#10072,#6386,.T.);
#13248=EDGE_CURVE('',#10073,#10072,#6387,.T.);
#13249=EDGE_CURVE('',#10048,#10073,#6388,.T.);
#13250=EDGE_CURVE('',#10074,#10073,#5695,.T.);
#13251=EDGE_CURVE('',#10049,#10074,#6389,.T.);
#13252=EDGE_CURVE('',#10075,#10074,#6390,.T.);
#13253=EDGE_CURVE('',#10050,#10075,#6391,.T.);
#13254=EDGE_CURVE('',#10076,#10075,#5696,.T.);
#13255=EDGE_CURVE('',#10051,#10076,#6392,.T.);
#13256=EDGE_CURVE('',#10077,#10076,#6393,.T.);
#13257=EDGE_CURVE('',#10052,#10077,#6394,.T.);
#13258=EDGE_CURVE('',#10078,#10077,#5697,.T.);
#13259=EDGE_CURVE('',#10053,#10078,#6395,.T.);
#13260=EDGE_CURVE('',#10079,#10078,#6396,.T.);
#13261=EDGE_CURVE('',#10054,#10079,#6397,.T.);
#13262=EDGE_CURVE('',#10080,#10079,#5698,.T.);
#13263=EDGE_CURVE('',#10055,#10080,#6398,.T.);
#13264=EDGE_CURVE('',#10081,#10080,#6399,.T.);
#13265=EDGE_CURVE('',#10056,#10081,#6400,.T.);
#13266=EDGE_CURVE('',#10082,#10081,#6401,.T.);
#13267=EDGE_CURVE('',#10057,#10082,#6402,.T.);
#13268=EDGE_CURVE('',#10083,#10082,#6403,.T.);
#13269=EDGE_CURVE('',#10058,#10083,#6404,.T.);
#13270=EDGE_CURVE('',#10084,#10083,#6405,.T.);
#13271=EDGE_CURVE('',#10059,#10084,#6406,.T.);
#13272=EDGE_CURVE('',#10085,#10084,#6407,.T.);
#13273=EDGE_CURVE('',#10060,#10085,#6408,.T.);
#13274=EDGE_CURVE('',#10086,#10085,#6409,.T.);
#13275=EDGE_CURVE('',#10061,#10086,#6410,.T.);
#13276=EDGE_CURVE('',#10087,#10086,#5699,.T.);
#13277=EDGE_CURVE('',#10036,#10087,#6411,.T.);
#13278=EDGE_CURVE('',#10062,#10087,#6412,.T.);
#13279=EDGE_CURVE('',#10088,#10089,#6413,.T.);
#13280=EDGE_CURVE('',#10089,#10090,#247,.T.);
#13281=EDGE_CURVE('',#10091,#10090,#5700,.T.);
#13282=EDGE_CURVE('',#10088,#10091,#248,.T.);
#13283=EDGE_CURVE('',#10092,#10093,#6414,.T.);
#13284=EDGE_CURVE('',#10093,#10094,#249,.T.);
#13285=EDGE_CURVE('',#10094,#10089,#250,.T.);
#13286=EDGE_CURVE('',#10095,#10088,#251,.T.);
#13287=EDGE_CURVE('',#10092,#10095,#252,.T.);
#13288=EDGE_CURVE('',#10096,#10097,#6415,.T.);
#13289=EDGE_CURVE('',#10097,#10098,#253,.T.);
#13290=EDGE_CURVE('',#10098,#10093,#254,.T.);
#13291=EDGE_CURVE('',#10099,#10092,#255,.T.);
#13292=EDGE_CURVE('',#10096,#10099,#256,.T.);
#13293=EDGE_CURVE('',#10100,#10101,#6416,.T.);
#13294=EDGE_CURVE('',#10102,#10100,#257,.T.);
#13295=EDGE_CURVE('',#10103,#10102,#258,.T.);
#13296=EDGE_CURVE('',#10104,#10103,#5701,.T.);
#13297=EDGE_CURVE('',#10104,#10105,#259,.T.);
#13298=EDGE_CURVE('',#10105,#10101,#260,.T.);
#13299=EDGE_CURVE('',#10106,#10107,#6417,.T.);
#13300=EDGE_CURVE('',#10107,#10108,#261,.T.);
#13301=EDGE_CURVE('',#10109,#10108,#5702,.T.);
#13302=EDGE_CURVE('',#10106,#10109,#262,.T.);
#13303=EDGE_CURVE('',#10110,#10111,#6418,.T.);
#13304=EDGE_CURVE('',#10111,#10112,#263,.T.);
#13305=EDGE_CURVE('',#10112,#10107,#264,.T.);
#13306=EDGE_CURVE('',#10113,#10106,#265,.T.);
#13307=EDGE_CURVE('',#10110,#10113,#266,.T.);
#13308=EDGE_CURVE('',#10114,#10115,#6419,.T.);
#13309=EDGE_CURVE('',#10115,#10116,#267,.T.);
#13310=EDGE_CURVE('',#10116,#10111,#268,.T.);
#13311=EDGE_CURVE('',#10117,#10110,#269,.T.);
#13312=EDGE_CURVE('',#10114,#10117,#270,.T.);
#13313=EDGE_CURVE('',#10118,#10119,#6420,.T.);
#13314=EDGE_CURVE('',#10120,#10118,#271,.T.);
#13315=EDGE_CURVE('',#10121,#10120,#272,.T.);
#13316=EDGE_CURVE('',#10122,#10121,#5703,.T.);
#13317=EDGE_CURVE('',#10122,#10123,#273,.T.);
#13318=EDGE_CURVE('',#10123,#10119,#274,.T.);
#13319=EDGE_CURVE('',#10124,#10125,#6421,.T.);
#13320=EDGE_CURVE('',#10125,#10126,#275,.T.);
#13321=EDGE_CURVE('',#10126,#10127,#276,.T.);
#13322=EDGE_CURVE('',#10128,#10127,#5704,.T.);
#13323=EDGE_CURVE('',#10129,#10128,#277,.T.);
#13324=EDGE_CURVE('',#10124,#10129,#278,.T.);
#13325=EDGE_CURVE('',#10130,#10131,#6422,.T.);
#13326=EDGE_CURVE('',#10131,#10132,#279,.T.);
#13327=EDGE_CURVE('',#10132,#10125,#280,.T.);
#13328=EDGE_CURVE('',#10133,#10124,#281,.T.);
#13329=EDGE_CURVE('',#10130,#10133,#282,.T.);
#13330=EDGE_CURVE('',#10134,#10135,#6423,.T.);
#13331=EDGE_CURVE('',#10135,#10136,#283,.T.);
#13332=EDGE_CURVE('',#10136,#10131,#284,.T.);
#13333=EDGE_CURVE('',#10137,#10130,#285,.T.);
#13334=EDGE_CURVE('',#10134,#10137,#286,.T.);
#13335=EDGE_CURVE('',#10138,#10139,#6424,.T.);
#13336=EDGE_CURVE('',#10139,#10140,#287,.T.);
#13337=EDGE_CURVE('',#10140,#10135,#288,.T.);
#13338=EDGE_CURVE('',#10141,#10134,#289,.T.);
#13339=EDGE_CURVE('',#10138,#10141,#290,.T.);
#13340=EDGE_CURVE('',#10142,#10143,#6425,.T.);
#13341=EDGE_CURVE('',#10143,#10144,#291,.T.);
#13342=EDGE_CURVE('',#10144,#10139,#292,.T.);
#13343=EDGE_CURVE('',#10145,#10138,#293,.T.);
#13344=EDGE_CURVE('',#10142,#10145,#294,.T.);
#13345=EDGE_CURVE('',#10146,#10147,#6426,.T.);
#13346=EDGE_CURVE('',#10147,#10148,#295,.T.);
#13347=EDGE_CURVE('',#10148,#10143,#296,.T.);
#13348=EDGE_CURVE('',#10149,#10142,#297,.T.);
#13349=EDGE_CURVE('',#10146,#10149,#298,.T.);
#13350=EDGE_CURVE('',#10150,#10151,#6427,.T.);
#13351=EDGE_CURVE('',#10151,#10152,#299,.T.);
#13352=EDGE_CURVE('',#10152,#10147,#300,.T.);
#13353=EDGE_CURVE('',#10153,#10146,#301,.T.);
#13354=EDGE_CURVE('',#10150,#10153,#302,.T.);
#13355=EDGE_CURVE('',#10154,#10155,#6428,.T.);
#13356=EDGE_CURVE('',#10155,#10156,#303,.T.);
#13357=EDGE_CURVE('',#10156,#10151,#304,.T.);
#13358=EDGE_CURVE('',#10157,#10150,#305,.T.);
#13359=EDGE_CURVE('',#10154,#10157,#306,.T.);
#13360=EDGE_CURVE('',#10158,#10159,#6429,.T.);
#13361=EDGE_CURVE('',#10159,#10160,#307,.T.);
#13362=EDGE_CURVE('',#10160,#10155,#308,.T.);
#13363=EDGE_CURVE('',#10161,#10154,#309,.T.);
#13364=EDGE_CURVE('',#10158,#10161,#310,.T.);
#13365=EDGE_CURVE('',#10162,#10163,#6430,.T.);
#13366=EDGE_CURVE('',#10163,#10164,#311,.T.);
#13367=EDGE_CURVE('',#10164,#10159,#312,.T.);
#13368=EDGE_CURVE('',#10165,#10158,#313,.T.);
#13369=EDGE_CURVE('',#10162,#10165,#314,.T.);
#13370=EDGE_CURVE('',#10166,#10167,#6431,.T.);
#13371=EDGE_CURVE('',#10167,#10168,#315,.T.);
#13372=EDGE_CURVE('',#10168,#10163,#316,.T.);
#13373=EDGE_CURVE('',#10169,#10162,#317,.T.);
#13374=EDGE_CURVE('',#10166,#10169,#318,.T.);
#13375=EDGE_CURVE('',#10170,#10171,#6432,.T.);
#13376=EDGE_CURVE('',#10171,#10172,#319,.T.);
#13377=EDGE_CURVE('',#10172,#10167,#320,.T.);
#13378=EDGE_CURVE('',#10173,#10166,#321,.T.);
#13379=EDGE_CURVE('',#10170,#10173,#322,.T.);
#13380=EDGE_CURVE('',#10174,#10175,#6433,.T.);
#13381=EDGE_CURVE('',#10175,#10176,#323,.T.);
#13382=EDGE_CURVE('',#10176,#10171,#324,.T.);
#13383=EDGE_CURVE('',#10177,#10170,#325,.T.);
#13384=EDGE_CURVE('',#10174,#10177,#326,.T.);
#13385=EDGE_CURVE('',#10178,#10179,#6434,.T.);
#13386=EDGE_CURVE('',#10179,#10180,#327,.T.);
#13387=EDGE_CURVE('',#10180,#10175,#328,.T.);
#13388=EDGE_CURVE('',#10181,#10174,#329,.T.);
#13389=EDGE_CURVE('',#10178,#10181,#330,.T.);
#13390=EDGE_CURVE('',#10182,#10183,#6435,.T.);
#13391=EDGE_CURVE('',#10183,#10184,#331,.T.);
#13392=EDGE_CURVE('',#10184,#10179,#332,.T.);
#13393=EDGE_CURVE('',#10185,#10178,#333,.T.);
#13394=EDGE_CURVE('',#10182,#10185,#334,.T.);
#13395=EDGE_CURVE('',#10186,#10187,#6436,.T.);
#13396=EDGE_CURVE('',#10187,#10188,#335,.T.);
#13397=EDGE_CURVE('',#10188,#10183,#336,.T.);
#13398=EDGE_CURVE('',#10189,#10182,#337,.T.);
#13399=EDGE_CURVE('',#10186,#10189,#338,.T.);
#13400=EDGE_CURVE('',#10190,#10191,#6437,.T.);
#13401=EDGE_CURVE('',#10191,#10192,#339,.T.);
#13402=EDGE_CURVE('',#10192,#10187,#340,.T.);
#13403=EDGE_CURVE('',#10193,#10186,#341,.T.);
#13404=EDGE_CURVE('',#10190,#10193,#342,.T.);
#13405=EDGE_CURVE('',#10194,#10195,#6438,.T.);
#13406=EDGE_CURVE('',#10195,#10196,#343,.T.);
#13407=EDGE_CURVE('',#10196,#10191,#344,.T.);
#13408=EDGE_CURVE('',#10197,#10190,#345,.T.);
#13409=EDGE_CURVE('',#10194,#10197,#346,.T.);
#13410=EDGE_CURVE('',#10198,#10199,#6439,.T.);
#13411=EDGE_CURVE('',#10199,#10200,#347,.T.);
#13412=EDGE_CURVE('',#10200,#10195,#348,.T.);
#13413=EDGE_CURVE('',#10201,#10194,#349,.T.);
#13414=EDGE_CURVE('',#10198,#10201,#350,.T.);
#13415=EDGE_CURVE('',#10202,#10203,#6440,.T.);
#13416=EDGE_CURVE('',#10203,#10204,#351,.T.);
#13417=EDGE_CURVE('',#10204,#10199,#352,.T.);
#13418=EDGE_CURVE('',#10205,#10198,#353,.T.);
#13419=EDGE_CURVE('',#10202,#10205,#354,.T.);
#13420=EDGE_CURVE('',#10206,#10207,#6441,.T.);
#13421=EDGE_CURVE('',#10207,#10208,#355,.T.);
#13422=EDGE_CURVE('',#10208,#10203,#356,.T.);
#13423=EDGE_CURVE('',#10209,#10202,#357,.T.);
#13424=EDGE_CURVE('',#10206,#10209,#358,.T.);
#13425=EDGE_CURVE('',#10210,#10211,#6442,.T.);
#13426=EDGE_CURVE('',#10211,#10212,#359,.T.);
#13427=EDGE_CURVE('',#10212,#10207,#360,.T.);
#13428=EDGE_CURVE('',#10213,#10206,#361,.T.);
#13429=EDGE_CURVE('',#10210,#10213,#362,.T.);
#13430=EDGE_CURVE('',#10214,#10215,#6443,.T.);
#13431=EDGE_CURVE('',#10215,#10216,#363,.T.);
#13432=EDGE_CURVE('',#10216,#10211,#364,.T.);
#13433=EDGE_CURVE('',#10217,#10210,#365,.T.);
#13434=EDGE_CURVE('',#10214,#10217,#366,.T.);
#13435=EDGE_CURVE('',#10218,#10219,#6444,.T.);
#13436=EDGE_CURVE('',#10219,#10220,#367,.T.);
#13437=EDGE_CURVE('',#10220,#10215,#368,.T.);
#13438=EDGE_CURVE('',#10221,#10214,#369,.T.);
#13439=EDGE_CURVE('',#10218,#10221,#370,.T.);
#13440=EDGE_CURVE('',#10222,#10223,#6445,.T.);
#13441=EDGE_CURVE('',#10223,#10224,#371,.T.);
#13442=EDGE_CURVE('',#10224,#10219,#372,.T.);
#13443=EDGE_CURVE('',#10225,#10218,#373,.T.);
#13444=EDGE_CURVE('',#10222,#10225,#374,.T.);
#13445=EDGE_CURVE('',#10226,#10227,#6446,.T.);
#13446=EDGE_CURVE('',#10227,#10228,#375,.T.);
#13447=EDGE_CURVE('',#10228,#10223,#376,.T.);
#13448=EDGE_CURVE('',#10229,#10222,#377,.T.);
#13449=EDGE_CURVE('',#10226,#10229,#378,.T.);
#13450=EDGE_CURVE('',#10230,#10231,#6447,.T.);
#13451=EDGE_CURVE('',#10232,#10230,#379,.T.);
#13452=EDGE_CURVE('',#10233,#10232,#380,.T.);
#13453=EDGE_CURVE('',#10234,#10233,#5705,.T.);
#13454=EDGE_CURVE('',#10234,#10235,#381,.T.);
#13455=EDGE_CURVE('',#10235,#10231,#382,.T.);
#13456=EDGE_CURVE('',#10236,#10237,#6448,.T.);
#13457=EDGE_CURVE('',#10237,#10238,#383,.T.);
#13458=EDGE_CURVE('',#10238,#10239,#384,.T.);
#13459=EDGE_CURVE('',#10240,#10239,#5706,.T.);
#13460=EDGE_CURVE('',#10241,#10240,#385,.T.);
#13461=EDGE_CURVE('',#10236,#10241,#386,.T.);
#13462=EDGE_CURVE('',#10242,#10243,#6449,.T.);
#13463=EDGE_CURVE('',#10243,#10244,#387,.T.);
#13464=EDGE_CURVE('',#10244,#10237,#388,.T.);
#13465=EDGE_CURVE('',#10245,#10236,#389,.T.);
#13466=EDGE_CURVE('',#10242,#10245,#390,.T.);
#13467=EDGE_CURVE('',#10246,#10247,#6450,.T.);
#13468=EDGE_CURVE('',#10247,#10248,#391,.T.);
#13469=EDGE_CURVE('',#10248,#10243,#392,.T.);
#13470=EDGE_CURVE('',#10249,#10242,#393,.T.);
#13471=EDGE_CURVE('',#10246,#10249,#394,.T.);
#13472=EDGE_CURVE('',#10250,#10251,#6451,.T.);
#13473=EDGE_CURVE('',#10251,#10252,#395,.T.);
#13474=EDGE_CURVE('',#10252,#10247,#396,.T.);
#13475=EDGE_CURVE('',#10253,#10246,#397,.T.);
#13476=EDGE_CURVE('',#10250,#10253,#398,.T.);
#13477=EDGE_CURVE('',#10254,#10255,#6452,.T.);
#13478=EDGE_CURVE('',#10255,#10256,#399,.T.);
#13479=EDGE_CURVE('',#10256,#10251,#400,.T.);
#13480=EDGE_CURVE('',#10257,#10250,#401,.T.);
#13481=EDGE_CURVE('',#10254,#10257,#402,.T.);
#13482=EDGE_CURVE('',#10258,#10259,#6453,.T.);
#13483=EDGE_CURVE('',#10259,#10260,#403,.T.);
#13484=EDGE_CURVE('',#10260,#10255,#404,.T.);
#13485=EDGE_CURVE('',#10261,#10254,#405,.T.);
#13486=EDGE_CURVE('',#10258,#10261,#406,.T.);
#13487=EDGE_CURVE('',#10262,#10263,#6454,.T.);
#13488=EDGE_CURVE('',#10263,#10264,#407,.T.);
#13489=EDGE_CURVE('',#10264,#10259,#408,.T.);
#13490=EDGE_CURVE('',#10265,#10258,#409,.T.);
#13491=EDGE_CURVE('',#10262,#10265,#410,.T.);
#13492=EDGE_CURVE('',#10266,#10267,#6455,.T.);
#13493=EDGE_CURVE('',#10267,#10268,#411,.T.);
#13494=EDGE_CURVE('',#10268,#10263,#412,.T.);
#13495=EDGE_CURVE('',#10269,#10262,#413,.T.);
#13496=EDGE_CURVE('',#10266,#10269,#414,.T.);
#13497=EDGE_CURVE('',#10270,#10271,#6456,.T.);
#13498=EDGE_CURVE('',#10271,#10272,#415,.T.);
#13499=EDGE_CURVE('',#10272,#10267,#416,.T.);
#13500=EDGE_CURVE('',#10273,#10266,#417,.T.);
#13501=EDGE_CURVE('',#10270,#10273,#418,.T.);
#13502=EDGE_CURVE('',#10274,#10275,#6457,.T.);
#13503=EDGE_CURVE('',#10275,#10276,#419,.T.);
#13504=EDGE_CURVE('',#10276,#10271,#420,.T.);
#13505=EDGE_CURVE('',#10277,#10270,#421,.T.);
#13506=EDGE_CURVE('',#10274,#10277,#422,.T.);
#13507=EDGE_CURVE('',#10278,#10279,#6458,.T.);
#13508=EDGE_CURVE('',#10279,#10280,#423,.T.);
#13509=EDGE_CURVE('',#10280,#10275,#424,.T.);
#13510=EDGE_CURVE('',#10281,#10274,#425,.T.);
#13511=EDGE_CURVE('',#10278,#10281,#426,.T.);
#13512=EDGE_CURVE('',#10282,#10283,#6459,.T.);
#13513=EDGE_CURVE('',#10283,#10284,#427,.T.);
#13514=EDGE_CURVE('',#10284,#10279,#428,.T.);
#13515=EDGE_CURVE('',#10285,#10278,#429,.T.);
#13516=EDGE_CURVE('',#10282,#10285,#430,.T.);
#13517=EDGE_CURVE('',#10286,#10287,#6460,.T.);
#13518=EDGE_CURVE('',#10287,#10288,#431,.T.);
#13519=EDGE_CURVE('',#10288,#10283,#432,.T.);
#13520=EDGE_CURVE('',#10289,#10282,#433,.T.);
#13521=EDGE_CURVE('',#10286,#10289,#434,.T.);
#13522=EDGE_CURVE('',#10290,#10291,#6461,.T.);
#13523=EDGE_CURVE('',#10291,#10292,#435,.T.);
#13524=EDGE_CURVE('',#10292,#10287,#436,.T.);
#13525=EDGE_CURVE('',#10293,#10286,#437,.T.);
#13526=EDGE_CURVE('',#10290,#10293,#438,.T.);
#13527=EDGE_CURVE('',#10294,#10295,#6462,.T.);
#13528=EDGE_CURVE('',#10295,#10296,#439,.T.);
#13529=EDGE_CURVE('',#10296,#10291,#440,.T.);
#13530=EDGE_CURVE('',#10297,#10290,#441,.T.);
#13531=EDGE_CURVE('',#10294,#10297,#442,.T.);
#13532=EDGE_CURVE('',#10298,#10299,#6463,.T.);
#13533=EDGE_CURVE('',#10299,#10300,#443,.T.);
#13534=EDGE_CURVE('',#10300,#10295,#444,.T.);
#13535=EDGE_CURVE('',#10301,#10294,#445,.T.);
#13536=EDGE_CURVE('',#10298,#10301,#446,.T.);
#13537=EDGE_CURVE('',#10302,#10303,#6464,.T.);
#13538=EDGE_CURVE('',#10303,#10304,#447,.T.);
#13539=EDGE_CURVE('',#10304,#10299,#448,.T.);
#13540=EDGE_CURVE('',#10305,#10298,#449,.T.);
#13541=EDGE_CURVE('',#10302,#10305,#450,.T.);
#13542=EDGE_CURVE('',#10306,#10307,#6465,.T.);
#13543=EDGE_CURVE('',#10307,#10308,#451,.T.);
#13544=EDGE_CURVE('',#10308,#10303,#452,.T.);
#13545=EDGE_CURVE('',#10309,#10302,#453,.T.);
#13546=EDGE_CURVE('',#10306,#10309,#454,.T.);
#13547=EDGE_CURVE('',#10310,#10311,#6466,.T.);
#13548=EDGE_CURVE('',#10311,#10312,#455,.T.);
#13549=EDGE_CURVE('',#10312,#10307,#456,.T.);
#13550=EDGE_CURVE('',#10313,#10306,#457,.T.);
#13551=EDGE_CURVE('',#10310,#10313,#458,.T.);
#13552=EDGE_CURVE('',#10314,#10315,#6467,.T.);
#13553=EDGE_CURVE('',#10315,#10316,#459,.T.);
#13554=EDGE_CURVE('',#10316,#10311,#460,.T.);
#13555=EDGE_CURVE('',#10317,#10310,#461,.T.);
#13556=EDGE_CURVE('',#10314,#10317,#462,.T.);
#13557=EDGE_CURVE('',#10318,#10319,#6468,.T.);
#13558=EDGE_CURVE('',#10319,#10320,#463,.T.);
#13559=EDGE_CURVE('',#10320,#10315,#464,.T.);
#13560=EDGE_CURVE('',#10321,#10314,#465,.T.);
#13561=EDGE_CURVE('',#10318,#10321,#466,.T.);
#13562=EDGE_CURVE('',#10322,#10323,#6469,.T.);
#13563=EDGE_CURVE('',#10323,#10324,#467,.T.);
#13564=EDGE_CURVE('',#10324,#10319,#468,.T.);
#13565=EDGE_CURVE('',#10325,#10318,#469,.T.);
#13566=EDGE_CURVE('',#10322,#10325,#470,.T.);
#13567=EDGE_CURVE('',#10326,#10327,#6470,.T.);
#13568=EDGE_CURVE('',#10327,#10328,#471,.T.);
#13569=EDGE_CURVE('',#10328,#10323,#472,.T.);
#13570=EDGE_CURVE('',#10329,#10322,#473,.T.);
#13571=EDGE_CURVE('',#10326,#10329,#474,.T.);
#13572=EDGE_CURVE('',#10330,#10331,#6471,.T.);
#13573=EDGE_CURVE('',#10331,#10332,#475,.T.);
#13574=EDGE_CURVE('',#10332,#10327,#476,.T.);
#13575=EDGE_CURVE('',#10333,#10326,#477,.T.);
#13576=EDGE_CURVE('',#10330,#10333,#478,.T.);
#13577=EDGE_CURVE('',#10334,#10335,#6472,.T.);
#13578=EDGE_CURVE('',#10335,#10336,#479,.T.);
#13579=EDGE_CURVE('',#10336,#10331,#480,.T.);
#13580=EDGE_CURVE('',#10337,#10330,#481,.T.);
#13581=EDGE_CURVE('',#10334,#10337,#482,.T.);
#13582=EDGE_CURVE('',#10338,#10339,#6473,.T.);
#13583=EDGE_CURVE('',#10339,#10340,#483,.T.);
#13584=EDGE_CURVE('',#10340,#10335,#484,.T.);
#13585=EDGE_CURVE('',#10341,#10334,#485,.T.);
#13586=EDGE_CURVE('',#10338,#10341,#486,.T.);
#13587=EDGE_CURVE('',#10342,#10343,#6474,.T.);
#13588=EDGE_CURVE('',#10344,#10342,#487,.T.);
#13589=EDGE_CURVE('',#10345,#10344,#488,.T.);
#13590=EDGE_CURVE('',#10346,#10345,#5707,.T.);
#13591=EDGE_CURVE('',#10346,#10347,#489,.T.);
#13592=EDGE_CURVE('',#10347,#10343,#490,.T.);
#13593=EDGE_CURVE('',#10348,#10349,#6475,.T.);
#13594=EDGE_CURVE('',#10349,#10350,#491,.T.);
#13595=EDGE_CURVE('',#10350,#10351,#492,.T.);
#13596=EDGE_CURVE('',#10352,#10351,#5708,.T.);
#13597=EDGE_CURVE('',#10353,#10352,#493,.T.);
#13598=EDGE_CURVE('',#10348,#10353,#494,.T.);
#13599=EDGE_CURVE('',#10354,#10355,#6476,.T.);
#13600=EDGE_CURVE('',#10355,#10356,#495,.T.);
#13601=EDGE_CURVE('',#10356,#10349,#496,.T.);
#13602=EDGE_CURVE('',#10357,#10348,#497,.T.);
#13603=EDGE_CURVE('',#10354,#10357,#498,.T.);
#13604=EDGE_CURVE('',#10358,#10359,#6477,.T.);
#13605=EDGE_CURVE('',#10359,#10360,#499,.T.);
#13606=EDGE_CURVE('',#10360,#10355,#500,.T.);
#13607=EDGE_CURVE('',#10361,#10354,#501,.T.);
#13608=EDGE_CURVE('',#10358,#10361,#502,.T.);
#13609=EDGE_CURVE('',#10362,#10363,#6478,.T.);
#13610=EDGE_CURVE('',#10363,#10364,#503,.T.);
#13611=EDGE_CURVE('',#10364,#10359,#504,.T.);
#13612=EDGE_CURVE('',#10365,#10358,#505,.T.);
#13613=EDGE_CURVE('',#10362,#10365,#506,.T.);
#13614=EDGE_CURVE('',#10366,#10367,#6479,.T.);
#13615=EDGE_CURVE('',#10367,#10368,#507,.T.);
#13616=EDGE_CURVE('',#10368,#10363,#508,.T.);
#13617=EDGE_CURVE('',#10369,#10362,#509,.T.);
#13618=EDGE_CURVE('',#10366,#10369,#510,.T.);
#13619=EDGE_CURVE('',#10370,#10371,#6480,.T.);
#13620=EDGE_CURVE('',#10371,#10372,#511,.T.);
#13621=EDGE_CURVE('',#10372,#10367,#512,.T.);
#13622=EDGE_CURVE('',#10373,#10366,#513,.T.);
#13623=EDGE_CURVE('',#10370,#10373,#514,.T.);
#13624=EDGE_CURVE('',#10374,#10375,#6481,.T.);
#13625=EDGE_CURVE('',#10375,#10376,#515,.T.);
#13626=EDGE_CURVE('',#10376,#10371,#516,.T.);
#13627=EDGE_CURVE('',#10377,#10370,#517,.T.);
#13628=EDGE_CURVE('',#10374,#10377,#518,.T.);
#13629=EDGE_CURVE('',#10378,#10379,#6482,.T.);
#13630=EDGE_CURVE('',#10379,#10380,#519,.T.);
#13631=EDGE_CURVE('',#10380,#10375,#520,.T.);
#13632=EDGE_CURVE('',#10381,#10374,#521,.T.);
#13633=EDGE_CURVE('',#10378,#10381,#522,.T.);
#13634=EDGE_CURVE('',#10382,#10383,#6483,.T.);
#13635=EDGE_CURVE('',#10383,#10384,#523,.T.);
#13636=EDGE_CURVE('',#10384,#10379,#524,.T.);
#13637=EDGE_CURVE('',#10385,#10378,#525,.T.);
#13638=EDGE_CURVE('',#10382,#10385,#526,.T.);
#13639=EDGE_CURVE('',#10386,#10387,#6484,.T.);
#13640=EDGE_CURVE('',#10387,#10388,#527,.T.);
#13641=EDGE_CURVE('',#10388,#10383,#528,.T.);
#13642=EDGE_CURVE('',#10389,#10382,#529,.T.);
#13643=EDGE_CURVE('',#10386,#10389,#530,.T.);
#13644=EDGE_CURVE('',#10390,#10391,#6485,.T.);
#13645=EDGE_CURVE('',#10391,#10392,#531,.T.);
#13646=EDGE_CURVE('',#10392,#10387,#532,.T.);
#13647=EDGE_CURVE('',#10393,#10386,#533,.T.);
#13648=EDGE_CURVE('',#10390,#10393,#534,.T.);
#13649=EDGE_CURVE('',#10394,#10395,#6486,.T.);
#13650=EDGE_CURVE('',#10395,#10396,#535,.T.);
#13651=EDGE_CURVE('',#10396,#10391,#536,.T.);
#13652=EDGE_CURVE('',#10397,#10390,#537,.T.);
#13653=EDGE_CURVE('',#10394,#10397,#538,.T.);
#13654=EDGE_CURVE('',#10398,#10399,#6487,.T.);
#13655=EDGE_CURVE('',#10399,#10400,#539,.T.);
#13656=EDGE_CURVE('',#10400,#10395,#540,.T.);
#13657=EDGE_CURVE('',#10401,#10394,#541,.T.);
#13658=EDGE_CURVE('',#10398,#10401,#542,.T.);
#13659=EDGE_CURVE('',#10402,#10403,#6488,.T.);
#13660=EDGE_CURVE('',#10403,#10404,#543,.T.);
#13661=EDGE_CURVE('',#10404,#10399,#544,.T.);
#13662=EDGE_CURVE('',#10405,#10398,#545,.T.);
#13663=EDGE_CURVE('',#10402,#10405,#546,.T.);
#13664=EDGE_CURVE('',#10406,#10407,#6489,.T.);
#13665=EDGE_CURVE('',#10407,#10408,#547,.T.);
#13666=EDGE_CURVE('',#10408,#10403,#548,.T.);
#13667=EDGE_CURVE('',#10409,#10402,#549,.T.);
#13668=EDGE_CURVE('',#10406,#10409,#550,.T.);
#13669=EDGE_CURVE('',#10410,#10411,#6490,.T.);
#13670=EDGE_CURVE('',#10411,#10412,#551,.T.);
#13671=EDGE_CURVE('',#10412,#10407,#552,.T.);
#13672=EDGE_CURVE('',#10413,#10406,#553,.T.);
#13673=EDGE_CURVE('',#10410,#10413,#554,.T.);
#13674=EDGE_CURVE('',#10414,#10415,#6491,.T.);
#13675=EDGE_CURVE('',#10415,#10416,#555,.T.);
#13676=EDGE_CURVE('',#10416,#10411,#556,.T.);
#13677=EDGE_CURVE('',#10417,#10410,#557,.T.);
#13678=EDGE_CURVE('',#10414,#10417,#558,.T.);
#13679=EDGE_CURVE('',#10418,#10419,#6492,.T.);
#13680=EDGE_CURVE('',#10419,#10420,#559,.T.);
#13681=EDGE_CURVE('',#10420,#10415,#560,.T.);
#13682=EDGE_CURVE('',#10421,#10414,#561,.T.);
#13683=EDGE_CURVE('',#10418,#10421,#562,.T.);
#13684=EDGE_CURVE('',#10422,#10423,#6493,.T.);
#13685=EDGE_CURVE('',#10423,#10424,#563,.T.);
#13686=EDGE_CURVE('',#10424,#10419,#564,.T.);
#13687=EDGE_CURVE('',#10425,#10418,#565,.T.);
#13688=EDGE_CURVE('',#10422,#10425,#566,.T.);
#13689=EDGE_CURVE('',#10426,#10427,#6494,.T.);
#13690=EDGE_CURVE('',#10427,#10428,#567,.T.);
#13691=EDGE_CURVE('',#10428,#10423,#568,.T.);
#13692=EDGE_CURVE('',#10429,#10422,#569,.T.);
#13693=EDGE_CURVE('',#10426,#10429,#570,.T.);
#13694=EDGE_CURVE('',#10430,#10431,#6495,.T.);
#13695=EDGE_CURVE('',#10431,#10432,#571,.T.);
#13696=EDGE_CURVE('',#10432,#10427,#572,.T.);
#13697=EDGE_CURVE('',#10433,#10426,#573,.T.);
#13698=EDGE_CURVE('',#10430,#10433,#574,.T.);
#13699=EDGE_CURVE('',#10434,#10435,#6496,.T.);
#13700=EDGE_CURVE('',#10435,#10436,#575,.T.);
#13701=EDGE_CURVE('',#10436,#10431,#576,.T.);
#13702=EDGE_CURVE('',#10437,#10430,#577,.T.);
#13703=EDGE_CURVE('',#10434,#10437,#578,.T.);
#13704=EDGE_CURVE('',#10438,#10439,#6497,.T.);
#13705=EDGE_CURVE('',#10439,#10440,#579,.T.);
#13706=EDGE_CURVE('',#10440,#10435,#580,.T.);
#13707=EDGE_CURVE('',#10441,#10434,#581,.T.);
#13708=EDGE_CURVE('',#10438,#10441,#582,.T.);
#13709=EDGE_CURVE('',#10442,#10443,#6498,.T.);
#13710=EDGE_CURVE('',#10443,#10444,#583,.T.);
#13711=EDGE_CURVE('',#10444,#10439,#584,.T.);
#13712=EDGE_CURVE('',#10445,#10438,#585,.T.);
#13713=EDGE_CURVE('',#10442,#10445,#586,.T.);
#13714=EDGE_CURVE('',#10446,#10447,#6499,.T.);
#13715=EDGE_CURVE('',#10447,#10448,#587,.T.);
#13716=EDGE_CURVE('',#10448,#10443,#588,.T.);
#13717=EDGE_CURVE('',#10449,#10442,#589,.T.);
#13718=EDGE_CURVE('',#10446,#10449,#590,.T.);
#13719=EDGE_CURVE('',#10450,#10451,#6500,.T.);
#13720=EDGE_CURVE('',#10451,#10452,#591,.T.);
#13721=EDGE_CURVE('',#10452,#10447,#592,.T.);
#13722=EDGE_CURVE('',#10453,#10446,#593,.T.);
#13723=EDGE_CURVE('',#10450,#10453,#594,.T.);
#13724=EDGE_CURVE('',#10454,#10455,#6501,.T.);
#13725=EDGE_CURVE('',#10456,#10454,#595,.T.);
#13726=EDGE_CURVE('',#10457,#10456,#596,.T.);
#13727=EDGE_CURVE('',#10458,#10457,#5709,.T.);
#13728=EDGE_CURVE('',#10458,#10459,#597,.T.);
#13729=EDGE_CURVE('',#10459,#10455,#598,.T.);
#13730=EDGE_CURVE('',#10460,#10461,#6502,.T.);
#13731=EDGE_CURVE('',#10461,#10462,#599,.T.);
#13732=EDGE_CURVE('',#10462,#10463,#600,.T.);
#13733=EDGE_CURVE('',#10464,#10463,#5710,.T.);
#13734=EDGE_CURVE('',#10465,#10464,#601,.T.);
#13735=EDGE_CURVE('',#10460,#10465,#602,.T.);
#13736=EDGE_CURVE('',#10466,#10467,#6503,.T.);
#13737=EDGE_CURVE('',#10467,#10468,#603,.T.);
#13738=EDGE_CURVE('',#10468,#10461,#604,.T.);
#13739=EDGE_CURVE('',#10469,#10460,#605,.T.);
#13740=EDGE_CURVE('',#10466,#10469,#606,.T.);
#13741=EDGE_CURVE('',#10470,#10471,#6504,.T.);
#13742=EDGE_CURVE('',#10471,#10472,#607,.T.);
#13743=EDGE_CURVE('',#10472,#10467,#608,.T.);
#13744=EDGE_CURVE('',#10473,#10466,#609,.T.);
#13745=EDGE_CURVE('',#10470,#10473,#610,.T.);
#13746=EDGE_CURVE('',#10474,#10475,#6505,.T.);
#13747=EDGE_CURVE('',#10475,#10476,#611,.T.);
#13748=EDGE_CURVE('',#10476,#10471,#612,.T.);
#13749=EDGE_CURVE('',#10477,#10470,#613,.T.);
#13750=EDGE_CURVE('',#10474,#10477,#614,.T.);
#13751=EDGE_CURVE('',#10478,#10479,#6506,.T.);
#13752=EDGE_CURVE('',#10479,#10480,#615,.T.);
#13753=EDGE_CURVE('',#10480,#10475,#616,.T.);
#13754=EDGE_CURVE('',#10481,#10474,#617,.T.);
#13755=EDGE_CURVE('',#10478,#10481,#618,.T.);
#13756=EDGE_CURVE('',#10482,#10483,#6507,.T.);
#13757=EDGE_CURVE('',#10483,#10484,#619,.T.);
#13758=EDGE_CURVE('',#10484,#10479,#620,.T.);
#13759=EDGE_CURVE('',#10485,#10478,#621,.T.);
#13760=EDGE_CURVE('',#10482,#10485,#622,.T.);
#13761=EDGE_CURVE('',#10486,#10487,#6508,.T.);
#13762=EDGE_CURVE('',#10487,#10488,#623,.T.);
#13763=EDGE_CURVE('',#10488,#10483,#624,.T.);
#13764=EDGE_CURVE('',#10489,#10482,#625,.T.);
#13765=EDGE_CURVE('',#10486,#10489,#626,.T.);
#13766=EDGE_CURVE('',#10490,#10491,#6509,.T.);
#13767=EDGE_CURVE('',#10491,#10492,#627,.T.);
#13768=EDGE_CURVE('',#10492,#10487,#628,.T.);
#13769=EDGE_CURVE('',#10493,#10486,#629,.T.);
#13770=EDGE_CURVE('',#10490,#10493,#630,.T.);
#13771=EDGE_CURVE('',#10494,#10495,#6510,.T.);
#13772=EDGE_CURVE('',#10495,#10496,#631,.T.);
#13773=EDGE_CURVE('',#10496,#10491,#632,.T.);
#13774=EDGE_CURVE('',#10497,#10490,#633,.T.);
#13775=EDGE_CURVE('',#10494,#10497,#634,.T.);
#13776=EDGE_CURVE('',#10498,#10499,#6511,.T.);
#13777=EDGE_CURVE('',#10499,#10500,#635,.T.);
#13778=EDGE_CURVE('',#10500,#10495,#636,.T.);
#13779=EDGE_CURVE('',#10501,#10494,#637,.T.);
#13780=EDGE_CURVE('',#10498,#10501,#638,.T.);
#13781=EDGE_CURVE('',#10502,#10503,#6512,.T.);
#13782=EDGE_CURVE('',#10503,#10504,#639,.T.);
#13783=EDGE_CURVE('',#10504,#10499,#640,.T.);
#13784=EDGE_CURVE('',#10505,#10498,#641,.T.);
#13785=EDGE_CURVE('',#10502,#10505,#642,.T.);
#13786=EDGE_CURVE('',#10506,#10507,#6513,.T.);
#13787=EDGE_CURVE('',#10507,#10508,#643,.T.);
#13788=EDGE_CURVE('',#10508,#10503,#644,.T.);
#13789=EDGE_CURVE('',#10509,#10502,#645,.T.);
#13790=EDGE_CURVE('',#10506,#10509,#646,.T.);
#13791=EDGE_CURVE('',#10510,#10511,#6514,.T.);
#13792=EDGE_CURVE('',#10511,#10512,#647,.T.);
#13793=EDGE_CURVE('',#10512,#10507,#648,.T.);
#13794=EDGE_CURVE('',#10513,#10506,#649,.T.);
#13795=EDGE_CURVE('',#10510,#10513,#650,.T.);
#13796=EDGE_CURVE('',#10514,#10515,#6515,.T.);
#13797=EDGE_CURVE('',#10515,#10516,#651,.T.);
#13798=EDGE_CURVE('',#10516,#10511,#652,.T.);
#13799=EDGE_CURVE('',#10517,#10510,#653,.T.);
#13800=EDGE_CURVE('',#10514,#10517,#654,.T.);
#13801=EDGE_CURVE('',#10518,#10519,#6516,.T.);
#13802=EDGE_CURVE('',#10519,#10520,#655,.T.);
#13803=EDGE_CURVE('',#10520,#10515,#656,.T.);
#13804=EDGE_CURVE('',#10521,#10514,#657,.T.);
#13805=EDGE_CURVE('',#10518,#10521,#658,.T.);
#13806=EDGE_CURVE('',#10522,#10523,#6517,.T.);
#13807=EDGE_CURVE('',#10523,#10524,#659,.T.);
#13808=EDGE_CURVE('',#10524,#10519,#660,.T.);
#13809=EDGE_CURVE('',#10525,#10518,#661,.T.);
#13810=EDGE_CURVE('',#10522,#10525,#662,.T.);
#13811=EDGE_CURVE('',#10526,#10527,#6518,.T.);
#13812=EDGE_CURVE('',#10527,#10528,#663,.T.);
#13813=EDGE_CURVE('',#10528,#10523,#664,.T.);
#13814=EDGE_CURVE('',#10529,#10522,#665,.T.);
#13815=EDGE_CURVE('',#10526,#10529,#666,.T.);
#13816=EDGE_CURVE('',#10530,#10531,#6519,.T.);
#13817=EDGE_CURVE('',#10531,#10532,#667,.T.);
#13818=EDGE_CURVE('',#10532,#10527,#668,.T.);
#13819=EDGE_CURVE('',#10533,#10526,#669,.T.);
#13820=EDGE_CURVE('',#10530,#10533,#670,.T.);
#13821=EDGE_CURVE('',#10534,#10535,#6520,.T.);
#13822=EDGE_CURVE('',#10535,#10536,#671,.T.);
#13823=EDGE_CURVE('',#10536,#10531,#672,.T.);
#13824=EDGE_CURVE('',#10537,#10530,#673,.T.);
#13825=EDGE_CURVE('',#10534,#10537,#674,.T.);
#13826=EDGE_CURVE('',#10538,#10539,#6521,.T.);
#13827=EDGE_CURVE('',#10539,#10540,#675,.T.);
#13828=EDGE_CURVE('',#10540,#10535,#676,.T.);
#13829=EDGE_CURVE('',#10541,#10534,#677,.T.);
#13830=EDGE_CURVE('',#10538,#10541,#678,.T.);
#13831=EDGE_CURVE('',#10542,#10543,#6522,.T.);
#13832=EDGE_CURVE('',#10543,#10544,#679,.T.);
#13833=EDGE_CURVE('',#10544,#10539,#680,.T.);
#13834=EDGE_CURVE('',#10545,#10538,#681,.T.);
#13835=EDGE_CURVE('',#10542,#10545,#682,.T.);
#13836=EDGE_CURVE('',#10546,#10547,#6523,.T.);
#13837=EDGE_CURVE('',#10547,#10548,#683,.T.);
#13838=EDGE_CURVE('',#10548,#10543,#684,.T.);
#13839=EDGE_CURVE('',#10549,#10542,#685,.T.);
#13840=EDGE_CURVE('',#10546,#10549,#686,.T.);
#13841=EDGE_CURVE('',#10550,#10551,#6524,.T.);
#13842=EDGE_CURVE('',#10551,#10552,#687,.T.);
#13843=EDGE_CURVE('',#10552,#10547,#688,.T.);
#13844=EDGE_CURVE('',#10553,#10546,#689,.T.);
#13845=EDGE_CURVE('',#10550,#10553,#690,.T.);
#13846=EDGE_CURVE('',#10554,#10555,#6525,.T.);
#13847=EDGE_CURVE('',#10555,#10556,#691,.T.);
#13848=EDGE_CURVE('',#10556,#10551,#692,.T.);
#13849=EDGE_CURVE('',#10557,#10550,#693,.T.);
#13850=EDGE_CURVE('',#10554,#10557,#694,.T.);
#13851=EDGE_CURVE('',#10558,#10559,#6526,.T.);
#13852=EDGE_CURVE('',#10559,#10560,#695,.T.);
#13853=EDGE_CURVE('',#10560,#10555,#696,.T.);
#13854=EDGE_CURVE('',#10561,#10554,#697,.T.);
#13855=EDGE_CURVE('',#10558,#10561,#698,.T.);
#13856=EDGE_CURVE('',#10562,#10563,#6527,.T.);
#13857=EDGE_CURVE('',#10563,#10564,#699,.T.);
#13858=EDGE_CURVE('',#10564,#10559,#700,.T.);
#13859=EDGE_CURVE('',#10565,#10558,#701,.T.);
#13860=EDGE_CURVE('',#10562,#10565,#702,.T.);
#13861=EDGE_CURVE('',#10566,#10567,#6528,.T.);
#13862=EDGE_CURVE('',#10568,#10566,#703,.T.);
#13863=EDGE_CURVE('',#10569,#10568,#704,.T.);
#13864=EDGE_CURVE('',#10570,#10569,#5711,.T.);
#13865=EDGE_CURVE('',#10570,#10571,#705,.T.);
#13866=EDGE_CURVE('',#10571,#10567,#706,.T.);
#13867=EDGE_CURVE('',#10572,#10573,#6529,.T.);
#13868=EDGE_CURVE('',#10573,#10574,#707,.F.);
#13869=EDGE_CURVE('',#10574,#10575,#5712,.F.);
#13870=EDGE_CURVE('',#10575,#10576,#708,.T.);
#13871=EDGE_CURVE('',#10576,#10572,#709,.T.);
#13872=EDGE_CURVE('',#10577,#10578,#6530,.T.);
#13873=EDGE_CURVE('',#10578,#10579,#710,.T.);
#13874=EDGE_CURVE('',#10579,#10573,#711,.F.);
#13875=EDGE_CURVE('',#10572,#10580,#712,.T.);
#13876=EDGE_CURVE('',#10580,#10577,#713,.T.);
#13877=EDGE_CURVE('',#10581,#10582,#6531,.T.);
#13878=EDGE_CURVE('',#10582,#10583,#714,.T.);
#13879=EDGE_CURVE('',#10583,#10578,#715,.T.);
#13880=EDGE_CURVE('',#10577,#10584,#716,.T.);
#13881=EDGE_CURVE('',#10584,#10581,#717,.T.);
#13882=EDGE_CURVE('',#10585,#10586,#6532,.T.);
#13883=EDGE_CURVE('',#10587,#10585,#5713,.F.);
#13884=EDGE_CURVE('',#10587,#10586,#718,.T.);
#13885=EDGE_CURVE('',#10588,#10589,#6533,.T.);
#13886=EDGE_CURVE('',#10589,#10590,#5714,.T.);
#13887=EDGE_CURVE('',#10590,#10588,#719,.T.);
#13888=EDGE_CURVE('',#10591,#10592,#6534,.T.);
#13889=EDGE_CURVE('',#10592,#10593,#720,.T.);
#13890=EDGE_CURVE('',#10593,#10589,#5715,.T.);
#13891=EDGE_CURVE('',#10588,#10591,#721,.T.);
#13892=EDGE_CURVE('',#10594,#10595,#6535,.T.);
#13893=EDGE_CURVE('',#10595,#10596,#722,.T.);
#13894=EDGE_CURVE('',#10596,#10592,#723,.T.);
#13895=EDGE_CURVE('',#10591,#10597,#724,.T.);
#13896=EDGE_CURVE('',#10597,#10594,#725,.T.);
#13897=EDGE_CURVE('',#10598,#10599,#6536,.T.);
#13898=EDGE_CURVE('',#10598,#10600,#726,.F.);
#13899=EDGE_CURVE('',#10600,#10601,#5716,.F.);
#13900=EDGE_CURVE('',#10601,#10602,#727,.T.);
#13901=EDGE_CURVE('',#10602,#10599,#728,.T.);
#13902=EDGE_CURVE('',#10603,#10604,#6537,.T.);
#13903=EDGE_CURVE('',#10604,#10605,#729,.T.);
#13904=EDGE_CURVE('',#10605,#10606,#730,.T.);
#13905=EDGE_CURVE('',#10607,#10606,#5717,.T.);
#13906=EDGE_CURVE('',#10607,#10608,#731,.T.);
#13907=EDGE_CURVE('',#10608,#10603,#732,.T.);
#13908=EDGE_CURVE('',#10609,#10610,#6538,.T.);
#13909=EDGE_CURVE('',#10610,#10604,#733,.T.);
#13910=EDGE_CURVE('',#10603,#10609,#734,.T.);
#13911=EDGE_CURVE('',#10611,#10612,#6539,.T.);
#13912=EDGE_CURVE('',#10612,#10613,#735,.T.);
#13913=EDGE_CURVE('',#10613,#10610,#736,.T.);
#13914=EDGE_CURVE('',#10609,#10614,#737,.T.);
#13915=EDGE_CURVE('',#10614,#10611,#738,.T.);
#13916=EDGE_CURVE('',#10615,#10616,#6540,.T.);
#13917=EDGE_CURVE('',#10616,#10617,#739,.T.);
#13918=EDGE_CURVE('',#10617,#10612,#740,.T.);
#13919=EDGE_CURVE('',#10611,#10615,#741,.T.);
#13920=EDGE_CURVE('',#10618,#10619,#6541,.T.);
#13921=EDGE_CURVE('',#10619,#10620,#742,.T.);
#13922=EDGE_CURVE('',#10620,#10616,#743,.T.);
#13923=EDGE_CURVE('',#10615,#10621,#744,.T.);
#13924=EDGE_CURVE('',#10621,#10618,#745,.T.);
#13925=EDGE_CURVE('',#10622,#10623,#6542,.T.);
#13926=EDGE_CURVE('',#10623,#10619,#746,.T.);
#13927=EDGE_CURVE('',#10618,#10622,#747,.T.);
#13928=EDGE_CURVE('',#10624,#10625,#6543,.T.);
#13929=EDGE_CURVE('',#10625,#10626,#748,.T.);
#13930=EDGE_CURVE('',#10626,#10623,#749,.T.);
#13931=EDGE_CURVE('',#10622,#10627,#750,.T.);
#13932=EDGE_CURVE('',#10627,#10624,#751,.T.);
#13933=EDGE_CURVE('',#10628,#10629,#6544,.T.);
#13934=EDGE_CURVE('',#10629,#10625,#752,.T.);
#13935=EDGE_CURVE('',#10624,#10628,#753,.T.);
#13936=EDGE_CURVE('',#10630,#10631,#6545,.T.);
#13937=EDGE_CURVE('',#10631,#10632,#754,.T.);
#13938=EDGE_CURVE('',#10632,#10629,#755,.T.);
#13939=EDGE_CURVE('',#10628,#10633,#756,.T.);
#13940=EDGE_CURVE('',#10633,#10630,#757,.T.);
#13941=EDGE_CURVE('',#10634,#10635,#6546,.T.);
#13942=EDGE_CURVE('',#10635,#10636,#758,.T.);
#13943=EDGE_CURVE('',#10636,#10631,#759,.T.);
#13944=EDGE_CURVE('',#10630,#10634,#760,.T.);
#13945=EDGE_CURVE('',#10637,#10638,#6547,.T.);
#13946=EDGE_CURVE('',#10638,#10639,#761,.T.);
#13947=EDGE_CURVE('',#10639,#10635,#762,.T.);
#13948=EDGE_CURVE('',#10634,#10640,#763,.T.);
#13949=EDGE_CURVE('',#10640,#10637,#764,.T.);
#13950=EDGE_CURVE('',#10641,#10642,#6548,.T.);
#13951=EDGE_CURVE('',#10642,#10638,#765,.T.);
#13952=EDGE_CURVE('',#10637,#10643,#766,.T.);
#13953=EDGE_CURVE('',#10643,#10641,#767,.T.);
#13954=EDGE_CURVE('',#10644,#10645,#6549,.T.);
#13955=EDGE_CURVE('',#10645,#10646,#768,.T.);
#13956=EDGE_CURVE('',#10646,#10642,#769,.T.);
#13957=EDGE_CURVE('',#10641,#10647,#770,.T.);
#13958=EDGE_CURVE('',#10647,#10644,#771,.T.);
#13959=EDGE_CURVE('',#10648,#10649,#6550,.T.);
#13960=EDGE_CURVE('',#10649,#10645,#772,.T.);
#13961=EDGE_CURVE('',#10644,#10648,#773,.T.);
#13962=EDGE_CURVE('',#10650,#10651,#6551,.T.);
#13963=EDGE_CURVE('',#10651,#10652,#774,.T.);
#13964=EDGE_CURVE('',#10652,#10649,#775,.T.);
#13965=EDGE_CURVE('',#10648,#10653,#776,.T.);
#13966=EDGE_CURVE('',#10653,#10650,#777,.T.);
#13967=EDGE_CURVE('',#10654,#10655,#6552,.T.);
#13968=EDGE_CURVE('',#10655,#10656,#778,.T.);
#13969=EDGE_CURVE('',#10656,#10651,#779,.T.);
#13970=EDGE_CURVE('',#10650,#10654,#780,.T.);
#13971=EDGE_CURVE('',#10657,#10658,#6553,.T.);
#13972=EDGE_CURVE('',#10658,#10659,#781,.T.);
#13973=EDGE_CURVE('',#10659,#10655,#782,.T.);
#13974=EDGE_CURVE('',#10654,#10660,#783,.T.);
#13975=EDGE_CURVE('',#10660,#10657,#784,.T.);
#13976=EDGE_CURVE('',#10661,#10662,#6554,.T.);
#13977=EDGE_CURVE('',#10662,#10658,#785,.T.);
#13978=EDGE_CURVE('',#10657,#10663,#786,.T.);
#13979=EDGE_CURVE('',#10663,#10661,#787,.T.);
#13980=EDGE_CURVE('',#10664,#10665,#6555,.T.);
#13981=EDGE_CURVE('',#10665,#10666,#788,.T.);
#13982=EDGE_CURVE('',#10666,#10662,#789,.T.);
#13983=EDGE_CURVE('',#10661,#10667,#790,.T.);
#13984=EDGE_CURVE('',#10667,#10664,#791,.T.);
#13985=EDGE_CURVE('',#10668,#10669,#6556,.T.);
#13986=EDGE_CURVE('',#10669,#10665,#792,.T.);
#13987=EDGE_CURVE('',#10664,#10668,#793,.T.);
#13988=EDGE_CURVE('',#10670,#10671,#6557,.T.);
#13989=EDGE_CURVE('',#10671,#10672,#794,.T.);
#13990=EDGE_CURVE('',#10672,#10669,#795,.T.);
#13991=EDGE_CURVE('',#10668,#10673,#796,.T.);
#13992=EDGE_CURVE('',#10673,#10670,#797,.T.);
#13993=EDGE_CURVE('',#10674,#10675,#6558,.T.);
#13994=EDGE_CURVE('',#10675,#10671,#798,.T.);
#13995=EDGE_CURVE('',#10670,#10674,#799,.T.);
#13996=EDGE_CURVE('',#10676,#10677,#6559,.T.);
#13997=EDGE_CURVE('',#10677,#10678,#800,.T.);
#13998=EDGE_CURVE('',#10678,#10675,#801,.T.);
#13999=EDGE_CURVE('',#10674,#10679,#802,.T.);
#14000=EDGE_CURVE('',#10679,#10676,#803,.T.);
#14001=EDGE_CURVE('',#10680,#10681,#6560,.T.);
#14002=EDGE_CURVE('',#10681,#10677,#804,.T.);
#14003=EDGE_CURVE('',#10676,#10682,#805,.T.);
#14004=EDGE_CURVE('',#10682,#10680,#806,.T.);
#14005=EDGE_CURVE('',#10683,#10684,#6561,.T.);
#14006=EDGE_CURVE('',#10684,#10685,#807,.T.);
#14007=EDGE_CURVE('',#10685,#10681,#808,.T.);
#14008=EDGE_CURVE('',#10680,#10686,#809,.T.);
#14009=EDGE_CURVE('',#10686,#10683,#810,.T.);
#14010=EDGE_CURVE('',#10687,#10688,#6562,.T.);
#14011=EDGE_CURVE('',#10688,#10684,#811,.T.);
#14012=EDGE_CURVE('',#10683,#10687,#812,.T.);
#14013=EDGE_CURVE('',#10689,#10690,#6563,.T.);
#14014=EDGE_CURVE('',#10689,#10691,#813,.T.);
#14015=EDGE_CURVE('',#10692,#10691,#5718,.F.);
#14016=EDGE_CURVE('',#10692,#10690,#814,.T.);
#14017=EDGE_CURVE('',#10693,#10694,#6564,.T.);
#14018=EDGE_CURVE('',#10694,#10695,#815,.T.);
#14019=EDGE_CURVE('',#10695,#10696,#816,.T.);
#14020=EDGE_CURVE('',#10697,#10696,#5719,.T.);
#14021=EDGE_CURVE('',#10697,#10698,#817,.T.);
#14022=EDGE_CURVE('',#10698,#10693,#818,.T.);
#14023=EDGE_CURVE('',#10699,#10700,#6565,.T.);
#14024=EDGE_CURVE('',#10700,#10694,#819,.T.);
#14025=EDGE_CURVE('',#10693,#10699,#820,.T.);
#14026=EDGE_CURVE('',#10701,#10702,#6566,.T.);
#14027=EDGE_CURVE('',#10702,#10703,#821,.T.);
#14028=EDGE_CURVE('',#10703,#10700,#822,.T.);
#14029=EDGE_CURVE('',#10699,#10704,#823,.T.);
#14030=EDGE_CURVE('',#10704,#10701,#824,.T.);
#14031=EDGE_CURVE('',#10705,#10706,#6567,.T.);
#14032=EDGE_CURVE('',#10706,#10707,#825,.T.);
#14033=EDGE_CURVE('',#10707,#10702,#826,.T.);
#14034=EDGE_CURVE('',#10701,#10705,#827,.T.);
#14035=EDGE_CURVE('',#10708,#10709,#6568,.T.);
#14036=EDGE_CURVE('',#10709,#10710,#828,.T.);
#14037=EDGE_CURVE('',#10710,#10706,#829,.T.);
#14038=EDGE_CURVE('',#10705,#10711,#830,.T.);
#14039=EDGE_CURVE('',#10711,#10708,#831,.T.);
#14040=EDGE_CURVE('',#10712,#10713,#6569,.T.);
#14041=EDGE_CURVE('',#10713,#10709,#832,.T.);
#14042=EDGE_CURVE('',#10708,#10712,#833,.T.);
#14043=EDGE_CURVE('',#10714,#10715,#6570,.T.);
#14044=EDGE_CURVE('',#10715,#10716,#834,.T.);
#14045=EDGE_CURVE('',#10716,#10713,#835,.T.);
#14046=EDGE_CURVE('',#10712,#10717,#836,.T.);
#14047=EDGE_CURVE('',#10717,#10714,#837,.T.);
#14048=EDGE_CURVE('',#10718,#10719,#6571,.T.);
#14049=EDGE_CURVE('',#10719,#10715,#838,.T.);
#14050=EDGE_CURVE('',#10714,#10718,#839,.T.);
#14051=EDGE_CURVE('',#10720,#10721,#6572,.T.);
#14052=EDGE_CURVE('',#10721,#10722,#840,.T.);
#14053=EDGE_CURVE('',#10722,#10719,#841,.T.);
#14054=EDGE_CURVE('',#10718,#10723,#842,.T.);
#14055=EDGE_CURVE('',#10723,#10720,#843,.T.);
#14056=EDGE_CURVE('',#10724,#10725,#6573,.T.);
#14057=EDGE_CURVE('',#10725,#10726,#844,.T.);
#14058=EDGE_CURVE('',#10726,#10721,#845,.T.);
#14059=EDGE_CURVE('',#10720,#10724,#846,.T.);
#14060=EDGE_CURVE('',#10727,#10728,#6574,.T.);
#14061=EDGE_CURVE('',#10728,#10729,#847,.T.);
#14062=EDGE_CURVE('',#10729,#10725,#848,.T.);
#14063=EDGE_CURVE('',#10724,#10730,#849,.T.);
#14064=EDGE_CURVE('',#10730,#10727,#850,.T.);
#14065=EDGE_CURVE('',#10731,#10732,#6575,.T.);
#14066=EDGE_CURVE('',#10732,#10728,#851,.T.);
#14067=EDGE_CURVE('',#10727,#10733,#852,.T.);
#14068=EDGE_CURVE('',#10733,#10731,#853,.T.);
#14069=EDGE_CURVE('',#10734,#10735,#6576,.T.);
#14070=EDGE_CURVE('',#10735,#10736,#854,.T.);
#14071=EDGE_CURVE('',#10736,#10732,#855,.T.);
#14072=EDGE_CURVE('',#10731,#10737,#856,.T.);
#14073=EDGE_CURVE('',#10737,#10734,#857,.T.);
#14074=EDGE_CURVE('',#10738,#10739,#6577,.T.);
#14075=EDGE_CURVE('',#10739,#10735,#858,.T.);
#14076=EDGE_CURVE('',#10734,#10738,#859,.T.);
#14077=EDGE_CURVE('',#10740,#10741,#6578,.T.);
#14078=EDGE_CURVE('',#10741,#10742,#860,.T.);
#14079=EDGE_CURVE('',#10742,#10739,#861,.T.);
#14080=EDGE_CURVE('',#10738,#10743,#862,.T.);
#14081=EDGE_CURVE('',#10743,#10740,#863,.T.);
#14082=EDGE_CURVE('',#10744,#10745,#6579,.T.);
#14083=EDGE_CURVE('',#10745,#10746,#864,.T.);
#14084=EDGE_CURVE('',#10746,#10741,#865,.T.);
#14085=EDGE_CURVE('',#10740,#10744,#866,.T.);
#14086=EDGE_CURVE('',#10747,#10748,#6580,.T.);
#14087=EDGE_CURVE('',#10748,#10749,#867,.T.);
#14088=EDGE_CURVE('',#10749,#10745,#868,.T.);
#14089=EDGE_CURVE('',#10744,#10750,#869,.T.);
#14090=EDGE_CURVE('',#10750,#10747,#870,.T.);
#14091=EDGE_CURVE('',#10751,#10752,#6581,.T.);
#14092=EDGE_CURVE('',#10752,#10748,#871,.T.);
#14093=EDGE_CURVE('',#10747,#10753,#872,.T.);
#14094=EDGE_CURVE('',#10753,#10751,#873,.T.);
#14095=EDGE_CURVE('',#10754,#10755,#6582,.T.);
#14096=EDGE_CURVE('',#10755,#10756,#874,.T.);
#14097=EDGE_CURVE('',#10756,#10752,#875,.T.);
#14098=EDGE_CURVE('',#10751,#10757,#876,.T.);
#14099=EDGE_CURVE('',#10757,#10754,#877,.T.);
#14100=EDGE_CURVE('',#10758,#10759,#6583,.T.);
#14101=EDGE_CURVE('',#10759,#10755,#878,.T.);
#14102=EDGE_CURVE('',#10754,#10758,#879,.T.);
#14103=EDGE_CURVE('',#10760,#10761,#6584,.T.);
#14104=EDGE_CURVE('',#10761,#10762,#880,.T.);
#14105=EDGE_CURVE('',#10762,#10759,#881,.T.);
#14106=EDGE_CURVE('',#10758,#10763,#882,.T.);
#14107=EDGE_CURVE('',#10763,#10760,#883,.T.);
#14108=EDGE_CURVE('',#10764,#10765,#6585,.T.);
#14109=EDGE_CURVE('',#10765,#10761,#884,.T.);
#14110=EDGE_CURVE('',#10760,#10764,#885,.T.);
#14111=EDGE_CURVE('',#10766,#10767,#6586,.T.);
#14112=EDGE_CURVE('',#10767,#10768,#886,.T.);
#14113=EDGE_CURVE('',#10768,#10765,#887,.T.);
#14114=EDGE_CURVE('',#10764,#10769,#888,.T.);
#14115=EDGE_CURVE('',#10769,#10766,#889,.T.);
#14116=EDGE_CURVE('',#10770,#10771,#6587,.T.);
#14117=EDGE_CURVE('',#10771,#10767,#890,.T.);
#14118=EDGE_CURVE('',#10766,#10772,#891,.T.);
#14119=EDGE_CURVE('',#10772,#10770,#892,.T.);
#14120=EDGE_CURVE('',#10773,#10774,#6588,.T.);
#14121=EDGE_CURVE('',#10774,#10775,#893,.T.);
#14122=EDGE_CURVE('',#10775,#10771,#894,.T.);
#14123=EDGE_CURVE('',#10770,#10776,#895,.T.);
#14124=EDGE_CURVE('',#10776,#10773,#896,.T.);
#14125=EDGE_CURVE('',#10777,#10778,#6589,.T.);
#14126=EDGE_CURVE('',#10778,#10774,#897,.T.);
#14127=EDGE_CURVE('',#10773,#10777,#898,.T.);
#14128=EDGE_CURVE('',#10779,#10780,#6590,.T.);
#14129=EDGE_CURVE('',#10779,#10781,#899,.T.);
#14130=EDGE_CURVE('',#10782,#10781,#5720,.F.);
#14131=EDGE_CURVE('',#10782,#10780,#900,.T.);
#14132=EDGE_CURVE('',#10783,#10784,#6591,.T.);
#14133=EDGE_CURVE('',#10784,#10785,#901,.T.);
#14134=EDGE_CURVE('',#10785,#10786,#902,.T.);
#14135=EDGE_CURVE('',#10787,#10786,#5721,.T.);
#14136=EDGE_CURVE('',#10787,#10788,#903,.T.);
#14137=EDGE_CURVE('',#10788,#10783,#904,.T.);
#14138=EDGE_CURVE('',#10789,#10790,#6592,.T.);
#14139=EDGE_CURVE('',#10790,#10784,#905,.T.);
#14140=EDGE_CURVE('',#10783,#10789,#906,.T.);
#14141=EDGE_CURVE('',#10791,#10792,#6593,.T.);
#14142=EDGE_CURVE('',#10792,#10793,#907,.T.);
#14143=EDGE_CURVE('',#10793,#10790,#908,.T.);
#14144=EDGE_CURVE('',#10789,#10794,#909,.T.);
#14145=EDGE_CURVE('',#10794,#10791,#910,.T.);
#14146=EDGE_CURVE('',#10795,#10796,#6594,.T.);
#14147=EDGE_CURVE('',#10796,#10797,#911,.T.);
#14148=EDGE_CURVE('',#10797,#10792,#912,.T.);
#14149=EDGE_CURVE('',#10791,#10795,#913,.T.);
#14150=EDGE_CURVE('',#10798,#10799,#6595,.T.);
#14151=EDGE_CURVE('',#10799,#10800,#914,.T.);
#14152=EDGE_CURVE('',#10800,#10796,#915,.T.);
#14153=EDGE_CURVE('',#10795,#10801,#916,.T.);
#14154=EDGE_CURVE('',#10801,#10798,#917,.T.);
#14155=EDGE_CURVE('',#10802,#10803,#6596,.T.);
#14156=EDGE_CURVE('',#10803,#10799,#918,.T.);
#14157=EDGE_CURVE('',#10798,#10802,#919,.T.);
#14158=EDGE_CURVE('',#10804,#10805,#6597,.T.);
#14159=EDGE_CURVE('',#10805,#10806,#920,.T.);
#14160=EDGE_CURVE('',#10806,#10803,#921,.T.);
#14161=EDGE_CURVE('',#10802,#10807,#922,.T.);
#14162=EDGE_CURVE('',#10807,#10804,#923,.T.);
#14163=EDGE_CURVE('',#10808,#10809,#6598,.T.);
#14164=EDGE_CURVE('',#10809,#10805,#924,.T.);
#14165=EDGE_CURVE('',#10804,#10808,#925,.T.);
#14166=EDGE_CURVE('',#10810,#10811,#6599,.T.);
#14167=EDGE_CURVE('',#10811,#10812,#926,.T.);
#14168=EDGE_CURVE('',#10812,#10809,#927,.T.);
#14169=EDGE_CURVE('',#10808,#10813,#928,.T.);
#14170=EDGE_CURVE('',#10813,#10810,#929,.T.);
#14171=EDGE_CURVE('',#10814,#10815,#6600,.T.);
#14172=EDGE_CURVE('',#10815,#10816,#930,.T.);
#14173=EDGE_CURVE('',#10816,#10811,#931,.T.);
#14174=EDGE_CURVE('',#10810,#10814,#932,.T.);
#14175=EDGE_CURVE('',#10817,#10818,#6601,.T.);
#14176=EDGE_CURVE('',#10818,#10819,#933,.T.);
#14177=EDGE_CURVE('',#10819,#10815,#934,.T.);
#14178=EDGE_CURVE('',#10814,#10820,#935,.T.);
#14179=EDGE_CURVE('',#10820,#10817,#936,.T.);
#14180=EDGE_CURVE('',#10821,#10822,#6602,.T.);
#14181=EDGE_CURVE('',#10822,#10818,#937,.T.);
#14182=EDGE_CURVE('',#10817,#10823,#938,.T.);
#14183=EDGE_CURVE('',#10823,#10821,#939,.T.);
#14184=EDGE_CURVE('',#10824,#10825,#6603,.T.);
#14185=EDGE_CURVE('',#10825,#10826,#940,.T.);
#14186=EDGE_CURVE('',#10826,#10822,#941,.T.);
#14187=EDGE_CURVE('',#10821,#10827,#942,.T.);
#14188=EDGE_CURVE('',#10827,#10824,#943,.T.);
#14189=EDGE_CURVE('',#10828,#10829,#6604,.T.);
#14190=EDGE_CURVE('',#10829,#10825,#944,.T.);
#14191=EDGE_CURVE('',#10824,#10828,#945,.T.);
#14192=EDGE_CURVE('',#10830,#10831,#6605,.T.);
#14193=EDGE_CURVE('',#10831,#10832,#946,.T.);
#14194=EDGE_CURVE('',#10832,#10829,#947,.T.);
#14195=EDGE_CURVE('',#10828,#10833,#948,.T.);
#14196=EDGE_CURVE('',#10833,#10830,#949,.T.);
#14197=EDGE_CURVE('',#10834,#10835,#6606,.T.);
#14198=EDGE_CURVE('',#10835,#10836,#950,.T.);
#14199=EDGE_CURVE('',#10836,#10831,#951,.T.);
#14200=EDGE_CURVE('',#10830,#10834,#952,.T.);
#14201=EDGE_CURVE('',#10837,#10838,#6607,.T.);
#14202=EDGE_CURVE('',#10838,#10839,#953,.T.);
#14203=EDGE_CURVE('',#10839,#10835,#954,.T.);
#14204=EDGE_CURVE('',#10834,#10840,#955,.T.);
#14205=EDGE_CURVE('',#10840,#10837,#956,.T.);
#14206=EDGE_CURVE('',#10841,#10842,#6608,.T.);
#14207=EDGE_CURVE('',#10842,#10838,#957,.T.);
#14208=EDGE_CURVE('',#10837,#10843,#958,.T.);
#14209=EDGE_CURVE('',#10843,#10841,#959,.T.);
#14210=EDGE_CURVE('',#10844,#10845,#6609,.T.);
#14211=EDGE_CURVE('',#10845,#10846,#960,.T.);
#14212=EDGE_CURVE('',#10846,#10842,#961,.T.);
#14213=EDGE_CURVE('',#10841,#10847,#962,.T.);
#14214=EDGE_CURVE('',#10847,#10844,#963,.T.);
#14215=EDGE_CURVE('',#10848,#10849,#6610,.T.);
#14216=EDGE_CURVE('',#10849,#10845,#964,.T.);
#14217=EDGE_CURVE('',#10844,#10848,#965,.T.);
#14218=EDGE_CURVE('',#10850,#10851,#6611,.T.);
#14219=EDGE_CURVE('',#10851,#10852,#966,.T.);
#14220=EDGE_CURVE('',#10852,#10849,#967,.T.);
#14221=EDGE_CURVE('',#10848,#10853,#968,.T.);
#14222=EDGE_CURVE('',#10853,#10850,#969,.T.);
#14223=EDGE_CURVE('',#10854,#10855,#6612,.T.);
#14224=EDGE_CURVE('',#10855,#10851,#970,.T.);
#14225=EDGE_CURVE('',#10850,#10854,#971,.T.);
#14226=EDGE_CURVE('',#10856,#10857,#6613,.T.);
#14227=EDGE_CURVE('',#10857,#10858,#972,.T.);
#14228=EDGE_CURVE('',#10858,#10855,#973,.T.);
#14229=EDGE_CURVE('',#10854,#10859,#974,.T.);
#14230=EDGE_CURVE('',#10859,#10856,#975,.T.);
#14231=EDGE_CURVE('',#10860,#10861,#6614,.T.);
#14232=EDGE_CURVE('',#10861,#10857,#976,.T.);
#14233=EDGE_CURVE('',#10856,#10862,#977,.T.);
#14234=EDGE_CURVE('',#10862,#10860,#978,.T.);
#14235=EDGE_CURVE('',#10863,#10864,#6615,.T.);
#14236=EDGE_CURVE('',#10864,#10865,#979,.T.);
#14237=EDGE_CURVE('',#10865,#10861,#980,.T.);
#14238=EDGE_CURVE('',#10860,#10866,#981,.T.);
#14239=EDGE_CURVE('',#10866,#10863,#982,.T.);
#14240=EDGE_CURVE('',#10867,#10868,#6616,.T.);
#14241=EDGE_CURVE('',#10868,#10864,#983,.T.);
#14242=EDGE_CURVE('',#10863,#10867,#984,.T.);
#14243=EDGE_CURVE('',#10869,#10870,#6617,.T.);
#14244=EDGE_CURVE('',#10869,#10871,#985,.T.);
#14245=EDGE_CURVE('',#10872,#10871,#5722,.F.);
#14246=EDGE_CURVE('',#10872,#10870,#986,.T.);
#14247=EDGE_CURVE('',#10873,#10874,#6618,.T.);
#14248=EDGE_CURVE('',#10874,#10875,#987,.T.);
#14249=EDGE_CURVE('',#10875,#10876,#988,.T.);
#14250=EDGE_CURVE('',#10877,#10876,#5723,.T.);
#14251=EDGE_CURVE('',#10877,#10878,#989,.T.);
#14252=EDGE_CURVE('',#10878,#10873,#990,.T.);
#14253=EDGE_CURVE('',#10879,#10880,#6619,.T.);
#14254=EDGE_CURVE('',#10880,#10874,#991,.T.);
#14255=EDGE_CURVE('',#10873,#10879,#992,.T.);
#14256=EDGE_CURVE('',#10881,#10882,#6620,.T.);
#14257=EDGE_CURVE('',#10882,#10883,#993,.T.);
#14258=EDGE_CURVE('',#10883,#10880,#994,.T.);
#14259=EDGE_CURVE('',#10879,#10884,#995,.T.);
#14260=EDGE_CURVE('',#10884,#10881,#996,.T.);
#14261=EDGE_CURVE('',#10885,#10886,#6621,.T.);
#14262=EDGE_CURVE('',#10886,#10887,#997,.T.);
#14263=EDGE_CURVE('',#10887,#10882,#998,.T.);
#14264=EDGE_CURVE('',#10881,#10885,#999,.T.);
#14265=EDGE_CURVE('',#10888,#10889,#6622,.T.);
#14266=EDGE_CURVE('',#10889,#10890,#1000,.T.);
#14267=EDGE_CURVE('',#10890,#10886,#1001,.T.);
#14268=EDGE_CURVE('',#10885,#10891,#1002,.T.);
#14269=EDGE_CURVE('',#10891,#10888,#1003,.T.);
#14270=EDGE_CURVE('',#10892,#10893,#6623,.T.);
#14271=EDGE_CURVE('',#10893,#10889,#1004,.T.);
#14272=EDGE_CURVE('',#10888,#10892,#1005,.T.);
#14273=EDGE_CURVE('',#10894,#10895,#6624,.T.);
#14274=EDGE_CURVE('',#10895,#10896,#1006,.T.);
#14275=EDGE_CURVE('',#10896,#10893,#1007,.T.);
#14276=EDGE_CURVE('',#10892,#10897,#1008,.T.);
#14277=EDGE_CURVE('',#10897,#10894,#1009,.T.);
#14278=EDGE_CURVE('',#10898,#10899,#6625,.T.);
#14279=EDGE_CURVE('',#10899,#10895,#1010,.T.);
#14280=EDGE_CURVE('',#10894,#10898,#1011,.T.);
#14281=EDGE_CURVE('',#10900,#10901,#6626,.T.);
#14282=EDGE_CURVE('',#10901,#10902,#1012,.T.);
#14283=EDGE_CURVE('',#10902,#10899,#1013,.T.);
#14284=EDGE_CURVE('',#10898,#10903,#1014,.T.);
#14285=EDGE_CURVE('',#10903,#10900,#1015,.T.);
#14286=EDGE_CURVE('',#10904,#10905,#6627,.T.);
#14287=EDGE_CURVE('',#10905,#10906,#1016,.T.);
#14288=EDGE_CURVE('',#10906,#10901,#1017,.T.);
#14289=EDGE_CURVE('',#10900,#10904,#1018,.T.);
#14290=EDGE_CURVE('',#10907,#10908,#6628,.T.);
#14291=EDGE_CURVE('',#10908,#10909,#1019,.T.);
#14292=EDGE_CURVE('',#10909,#10905,#1020,.T.);
#14293=EDGE_CURVE('',#10904,#10910,#1021,.T.);
#14294=EDGE_CURVE('',#10910,#10907,#1022,.T.);
#14295=EDGE_CURVE('',#10911,#10912,#6629,.T.);
#14296=EDGE_CURVE('',#10912,#10908,#1023,.T.);
#14297=EDGE_CURVE('',#10907,#10913,#1024,.T.);
#14298=EDGE_CURVE('',#10913,#10911,#1025,.T.);
#14299=EDGE_CURVE('',#10914,#10915,#6630,.T.);
#14300=EDGE_CURVE('',#10915,#10916,#1026,.T.);
#14301=EDGE_CURVE('',#10916,#10912,#1027,.T.);
#14302=EDGE_CURVE('',#10911,#10917,#1028,.T.);
#14303=EDGE_CURVE('',#10917,#10914,#1029,.T.);
#14304=EDGE_CURVE('',#10918,#10919,#6631,.T.);
#14305=EDGE_CURVE('',#10919,#10915,#1030,.T.);
#14306=EDGE_CURVE('',#10914,#10918,#1031,.T.);
#14307=EDGE_CURVE('',#10920,#10921,#6632,.T.);
#14308=EDGE_CURVE('',#10921,#10922,#1032,.T.);
#14309=EDGE_CURVE('',#10922,#10919,#1033,.T.);
#14310=EDGE_CURVE('',#10918,#10923,#1034,.T.);
#14311=EDGE_CURVE('',#10923,#10920,#1035,.T.);
#14312=EDGE_CURVE('',#10924,#10925,#6633,.T.);
#14313=EDGE_CURVE('',#10925,#10926,#1036,.T.);
#14314=EDGE_CURVE('',#10926,#10921,#1037,.T.);
#14315=EDGE_CURVE('',#10920,#10924,#1038,.T.);
#14316=EDGE_CURVE('',#10927,#10928,#6634,.T.);
#14317=EDGE_CURVE('',#10928,#10929,#1039,.T.);
#14318=EDGE_CURVE('',#10929,#10925,#1040,.T.);
#14319=EDGE_CURVE('',#10924,#10930,#1041,.T.);
#14320=EDGE_CURVE('',#10930,#10927,#1042,.T.);
#14321=EDGE_CURVE('',#10931,#10932,#6635,.T.);
#14322=EDGE_CURVE('',#10932,#10928,#1043,.T.);
#14323=EDGE_CURVE('',#10927,#10933,#1044,.T.);
#14324=EDGE_CURVE('',#10933,#10931,#1045,.T.);
#14325=EDGE_CURVE('',#10934,#10935,#6636,.T.);
#14326=EDGE_CURVE('',#10935,#10936,#1046,.T.);
#14327=EDGE_CURVE('',#10936,#10932,#1047,.T.);
#14328=EDGE_CURVE('',#10931,#10937,#1048,.T.);
#14329=EDGE_CURVE('',#10937,#10934,#1049,.T.);
#14330=EDGE_CURVE('',#10938,#10939,#6637,.T.);
#14331=EDGE_CURVE('',#10939,#10935,#1050,.T.);
#14332=EDGE_CURVE('',#10934,#10938,#1051,.T.);
#14333=EDGE_CURVE('',#10940,#10941,#6638,.T.);
#14334=EDGE_CURVE('',#10941,#10942,#1052,.T.);
#14335=EDGE_CURVE('',#10942,#10939,#1053,.T.);
#14336=EDGE_CURVE('',#10938,#10943,#1054,.T.);
#14337=EDGE_CURVE('',#10943,#10940,#1055,.T.);
#14338=EDGE_CURVE('',#10944,#10945,#6639,.T.);
#14339=EDGE_CURVE('',#10945,#10941,#1056,.T.);
#14340=EDGE_CURVE('',#10940,#10944,#1057,.T.);
#14341=EDGE_CURVE('',#10946,#10947,#6640,.T.);
#14342=EDGE_CURVE('',#10947,#10948,#1058,.T.);
#14343=EDGE_CURVE('',#10948,#10945,#1059,.T.);
#14344=EDGE_CURVE('',#10944,#10949,#1060,.T.);
#14345=EDGE_CURVE('',#10949,#10946,#1061,.T.);
#14346=EDGE_CURVE('',#10950,#10951,#6641,.T.);
#14347=EDGE_CURVE('',#10951,#10947,#1062,.T.);
#14348=EDGE_CURVE('',#10946,#10952,#1063,.T.);
#14349=EDGE_CURVE('',#10952,#10950,#1064,.T.);
#14350=EDGE_CURVE('',#10953,#10954,#6642,.T.);
#14351=EDGE_CURVE('',#10954,#10955,#1065,.T.);
#14352=EDGE_CURVE('',#10955,#10951,#1066,.T.);
#14353=EDGE_CURVE('',#10950,#10956,#1067,.T.);
#14354=EDGE_CURVE('',#10956,#10953,#1068,.T.);
#14355=EDGE_CURVE('',#10957,#10958,#6643,.T.);
#14356=EDGE_CURVE('',#10958,#10954,#1069,.T.);
#14357=EDGE_CURVE('',#10953,#10957,#1070,.T.);
#14358=EDGE_CURVE('',#10959,#10960,#6644,.T.);
#14359=EDGE_CURVE('',#10959,#10961,#1071,.T.);
#14360=EDGE_CURVE('',#10962,#10961,#5724,.F.);
#14361=EDGE_CURVE('',#10962,#10960,#1072,.T.);
#14362=EDGE_CURVE('',#10960,#10963,#1073,.T.);
#14363=EDGE_CURVE('',#10963,#10958,#1074,.T.);
#14364=EDGE_CURVE('',#10957,#10964,#1075,.T.);
#14365=EDGE_CURVE('',#10964,#10959,#1076,.T.);
#14366=EDGE_CURVE('',#10870,#10965,#1077,.T.);
#14367=EDGE_CURVE('',#10965,#10868,#1078,.T.);
#14368=EDGE_CURVE('',#10867,#10966,#1079,.T.);
#14369=EDGE_CURVE('',#10966,#10869,#1080,.T.);
#14370=EDGE_CURVE('',#10780,#10967,#1081,.T.);
#14371=EDGE_CURVE('',#10967,#10778,#1082,.T.);
#14372=EDGE_CURVE('',#10777,#10968,#1083,.T.);
#14373=EDGE_CURVE('',#10968,#10779,#1084,.T.);
#14374=EDGE_CURVE('',#10690,#10969,#1085,.T.);
#14375=EDGE_CURVE('',#10969,#10688,#1086,.T.);
#14376=EDGE_CURVE('',#10687,#10970,#1087,.T.);
#14377=EDGE_CURVE('',#10970,#10689,#1088,.T.);
#14378=EDGE_CURVE('',#10599,#10971,#1089,.T.);
#14379=EDGE_CURVE('',#10971,#10595,#1090,.T.);
#14380=EDGE_CURVE('',#10594,#10972,#1091,.T.);
#14381=EDGE_CURVE('',#10972,#10598,#1092,.F.);
#14382=EDGE_CURVE('',#10586,#10582,#1093,.T.);
#14383=EDGE_CURVE('',#10581,#10973,#1094,.T.);
#14384=EDGE_CURVE('',#10585,#10973,#5725,.F.);
#14385=EDGE_CURVE('',#10567,#10974,#1095,.T.);
#14386=EDGE_CURVE('',#10974,#10563,#1096,.T.);
#14387=EDGE_CURVE('',#10975,#10562,#1097,.T.);
#14388=EDGE_CURVE('',#10566,#10975,#1098,.T.);
#14389=EDGE_CURVE('',#10455,#10976,#1099,.T.);
#14390=EDGE_CURVE('',#10976,#10451,#1100,.T.);
#14391=EDGE_CURVE('',#10977,#10450,#1101,.T.);
#14392=EDGE_CURVE('',#10454,#10977,#1102,.T.);
#14393=EDGE_CURVE('',#10343,#10978,#1103,.T.);
#14394=EDGE_CURVE('',#10978,#10339,#1104,.T.);
#14395=EDGE_CURVE('',#10979,#10338,#1105,.T.);
#14396=EDGE_CURVE('',#10342,#10979,#1106,.T.);
#14397=EDGE_CURVE('',#10231,#10980,#1107,.T.);
#14398=EDGE_CURVE('',#10980,#10227,#1108,.T.);
#14399=EDGE_CURVE('',#10981,#10226,#1109,.T.);
#14400=EDGE_CURVE('',#10230,#10981,#1110,.T.);
#14401=EDGE_CURVE('',#10119,#10982,#1111,.T.);
#14402=EDGE_CURVE('',#10982,#10115,#1112,.T.);
#14403=EDGE_CURVE('',#10983,#10114,#1113,.T.);
#14404=EDGE_CURVE('',#10118,#10983,#1114,.T.);
#14405=EDGE_CURVE('',#10101,#10984,#1115,.T.);
#14406=EDGE_CURVE('',#10984,#10097,#1116,.T.);
#14407=EDGE_CURVE('',#10985,#10096,#1117,.T.);
#14408=EDGE_CURVE('',#10100,#10985,#1118,.T.);
#14409=EDGE_CURVE('',#10986,#10986,#5726,.T.);
#14410=EDGE_CURVE('',#10986,#10987,#6645,.T.);
#14411=EDGE_CURVE('',#10987,#10987,#5727,.T.);
#14412=EDGE_CURVE('',#10988,#10989,#5728,.T.);
#14413=EDGE_CURVE('',#10990,#10988,#6646,.T.);
#14414=EDGE_CURVE('',#10990,#10991,#5729,.T.);
#14415=EDGE_CURVE('',#10989,#10991,#6647,.T.);
#14416=EDGE_CURVE('',#10991,#10992,#6648,.T.);
#14417=EDGE_CURVE('',#10993,#10990,#6649,.T.);
#14418=EDGE_CURVE('',#10994,#10993,#6650,.T.);
#14419=EDGE_CURVE('',#10992,#10994,#5730,.T.);
#14420=EDGE_CURVE('',#10995,#10995,#5731,.T.);
#14421=EDGE_CURVE('',#10995,#10996,#6651,.T.);
#14422=EDGE_CURVE('',#10996,#10996,#5732,.T.);
#14423=EDGE_CURVE('',#10997,#10998,#5733,.T.);
#14424=EDGE_CURVE('',#10999,#10997,#6652,.T.);
#14425=EDGE_CURVE('',#10999,#11000,#5734,.T.);
#14426=EDGE_CURVE('',#10998,#11000,#6653,.T.);
#14427=EDGE_CURVE('',#11001,#11002,#6654,.T.);
#14428=EDGE_CURVE('',#11000,#11001,#6655,.T.);
#14429=EDGE_CURVE('',#11003,#10999,#6656,.T.);
#14430=EDGE_CURVE('',#11002,#11003,#5735,.T.);
#14431=EDGE_CURVE('',#11004,#11004,#5736,.T.);
#14432=EDGE_CURVE('',#11004,#11005,#6657,.T.);
#14433=EDGE_CURVE('',#11005,#11005,#5737,.T.);
#14434=EDGE_CURVE('',#11006,#10993,#6658,.T.);
#14435=EDGE_CURVE('',#11006,#11007,#6659,.T.);
#14436=EDGE_CURVE('',#11007,#10994,#6660,.T.);
#14437=EDGE_CURVE('',#11008,#10997,#6661,.T.);
#14438=EDGE_CURVE('',#11009,#11008,#6662,.T.);
#14439=EDGE_CURVE('',#11010,#11009,#6663,.T.);
#14440=EDGE_CURVE('',#11010,#11003,#6664,.T.);
#14441=EDGE_CURVE('',#10998,#10988,#6665,.T.);
#14442=EDGE_CURVE('',#11011,#11001,#6666,.T.);
#14443=EDGE_CURVE('',#11006,#11011,#6667,.T.);
#14444=EDGE_CURVE('',#10989,#11012,#6668,.T.);
#14445=EDGE_CURVE('',#11012,#11013,#5738,.T.);
#14446=EDGE_CURVE('',#11013,#11014,#6669,.T.);
#14447=EDGE_CURVE('',#11014,#11015,#5739,.T.);
#14448=EDGE_CURVE('',#11015,#11016,#6670,.T.);
#14449=EDGE_CURVE('',#11016,#11017,#5740,.T.);
#14450=EDGE_CURVE('',#11017,#11018,#6671,.T.);
#14451=EDGE_CURVE('',#11018,#11019,#5741,.T.);
#14452=EDGE_CURVE('',#11019,#11020,#6672,.T.);
#14453=EDGE_CURVE('',#11020,#11021,#6673,.T.);
#14454=EDGE_CURVE('',#11021,#11022,#6674,.T.);
#14455=EDGE_CURVE('',#11022,#11023,#6675,.T.);
#14456=EDGE_CURVE('',#11023,#11024,#6676,.T.);
#14457=EDGE_CURVE('',#11024,#11025,#5742,.T.);
#14458=EDGE_CURVE('',#11025,#11026,#6677,.T.);
#14459=EDGE_CURVE('',#11026,#11027,#5743,.T.);
#14460=EDGE_CURVE('',#11027,#11028,#6678,.T.);
#14461=EDGE_CURVE('',#11028,#11029,#6679,.T.);
#14462=EDGE_CURVE('',#11029,#11030,#6680,.T.);
#14463=EDGE_CURVE('',#11030,#11031,#6681,.T.);
#14464=EDGE_CURVE('',#11031,#11032,#6682,.T.);
#14465=EDGE_CURVE('',#11032,#11033,#5744,.T.);
#14466=EDGE_CURVE('',#11033,#11034,#6683,.T.);
#14467=EDGE_CURVE('',#11034,#11035,#5745,.T.);
#14468=EDGE_CURVE('',#11035,#11036,#6684,.T.);
#14469=EDGE_CURVE('',#11036,#11037,#5746,.T.);
#14470=EDGE_CURVE('',#11037,#11038,#6685,.T.);
#14471=EDGE_CURVE('',#11038,#11008,#5747,.T.);
#14472=EDGE_CURVE('',#11039,#11039,#5748,.T.);
#14473=EDGE_CURVE('',#11040,#11040,#5749,.T.);
#14474=EDGE_CURVE('',#10876,#10128,#1119,.T.);
#14475=EDGE_CURVE('',#10127,#10877,#1120,.T.);
#14476=EDGE_CURVE('',#10786,#10240,#1121,.T.);
#14477=EDGE_CURVE('',#10239,#10787,#1122,.T.);
#14478=EDGE_CURVE('',#10696,#10352,#1123,.T.);
#14479=EDGE_CURVE('',#10351,#10697,#1124,.T.);
#14480=EDGE_CURVE('',#10606,#10464,#1125,.T.);
#14481=EDGE_CURVE('',#10463,#10607,#1126,.T.);
#14482=EDGE_CURVE('',#10090,#10590,#1127,.T.);
#14483=EDGE_CURVE('',#10600,#10104,#1128,.T.);
#14484=EDGE_CURVE('',#10593,#10091,#1129,.T.);
#14485=EDGE_CURVE('',#10103,#10601,#1130,.T.);
#14486=EDGE_CURVE('',#10108,#10587,#1131,.T.);
#14487=EDGE_CURVE('',#10574,#10122,#1132,.T.);
#14488=EDGE_CURVE('',#10973,#10109,#1133,.T.);
#14489=EDGE_CURVE('',#10121,#10575,#1134,.T.);
#14490=EDGE_CURVE('',#10961,#10234,#1135,.T.);
#14491=EDGE_CURVE('',#10233,#10962,#1136,.T.);
#14492=EDGE_CURVE('',#10871,#10346,#1137,.T.);
#14493=EDGE_CURVE('',#10345,#10872,#1138,.T.);
#14494=EDGE_CURVE('',#10781,#10458,#1139,.T.);
#14495=EDGE_CURVE('',#10457,#10782,#1140,.T.);
#14496=EDGE_CURVE('',#10691,#10570,#1141,.T.);
#14497=EDGE_CURVE('',#10569,#10692,#1142,.T.);
#14498=EDGE_CURVE('',#11041,#11042,#6686,.T.);
#14499=EDGE_CURVE('',#11041,#11043,#6687,.T.);
#14500=EDGE_CURVE('',#11044,#11043,#6688,.T.);
#14501=EDGE_CURVE('',#11042,#11044,#6689,.T.);
#14502=EDGE_CURVE('',#11042,#11045,#6690,.T.);
#14503=EDGE_CURVE('',#11046,#11044,#6691,.T.);
#14504=EDGE_CURVE('',#11045,#11046,#6692,.T.);
#14505=EDGE_CURVE('',#11045,#11047,#6693,.T.);
#14506=EDGE_CURVE('',#11048,#11046,#6694,.T.);
#14507=EDGE_CURVE('',#11047,#11048,#6695,.T.);
#14508=EDGE_CURVE('',#11047,#11049,#6696,.T.);
#14509=EDGE_CURVE('',#11050,#11048,#6697,.T.);
#14510=EDGE_CURVE('',#11049,#11050,#6698,.T.);
#14511=EDGE_CURVE('',#11049,#11051,#6699,.T.);
#14512=EDGE_CURVE('',#11052,#11050,#6700,.T.);
#14513=EDGE_CURVE('',#11051,#11052,#6701,.T.);
#14514=EDGE_CURVE('',#11051,#11053,#6702,.T.);
#14515=EDGE_CURVE('',#11054,#11052,#6703,.T.);
#14516=EDGE_CURVE('',#11053,#11054,#6704,.T.);
#14517=EDGE_CURVE('',#11053,#11041,#6705,.T.);
#14518=EDGE_CURVE('',#11043,#11054,#6706,.T.);
#14519=EDGE_CURVE('',#11055,#11055,#5750,.T.);
#14520=EDGE_CURVE('',#11055,#11056,#6707,.T.);
#14521=EDGE_CURVE('',#11056,#11056,#5751,.T.);
#14522=EDGE_CURVE('',#11057,#11058,#5752,.T.);
#14523=EDGE_CURVE('',#11057,#11059,#6708,.T.);
#14524=EDGE_CURVE('',#11060,#11059,#5753,.T.);
#14525=EDGE_CURVE('',#11058,#11060,#6709,.T.);
#14526=EDGE_CURVE('',#11058,#11061,#6710,.T.);
#14527=EDGE_CURVE('',#11062,#11060,#6711,.T.);
#14528=EDGE_CURVE('',#11061,#11062,#6712,.T.);
#14529=EDGE_CURVE('',#11061,#11063,#5754,.T.);
#14530=EDGE_CURVE('',#11064,#11062,#5755,.T.);
#14531=EDGE_CURVE('',#11063,#11064,#6713,.T.);
#14532=EDGE_CURVE('',#11063,#11020,#6714,.T.);
#14533=EDGE_CURVE('',#11021,#11064,#6715,.T.);
#14534=EDGE_CURVE('',#11023,#11057,#6716,.T.);
#14535=EDGE_CURVE('',#11059,#11022,#6717,.T.);
#14536=EDGE_CURVE('',#11065,#11065,#5756,.T.);
#14537=EDGE_CURVE('',#11066,#11066,#5757,.T.);
#14538=EDGE_CURVE('',#11067,#11068,#6718,.T.);
#14539=EDGE_CURVE('',#11067,#11069,#6719,.T.);
#14540=EDGE_CURVE('',#11070,#11069,#6720,.T.);
#14541=EDGE_CURVE('',#11068,#11070,#6721,.T.);
#14542=EDGE_CURVE('',#11068,#11071,#6722,.T.);
#14543=EDGE_CURVE('',#11072,#11070,#6723,.T.);
#14544=EDGE_CURVE('',#11071,#11072,#6724,.T.);
#14545=EDGE_CURVE('',#11071,#11073,#6725,.T.);
#14546=EDGE_CURVE('',#11074,#11072,#6726,.T.);
#14547=EDGE_CURVE('',#11073,#11074,#6727,.T.);
#14548=EDGE_CURVE('',#11073,#11075,#6728,.T.);
#14549=EDGE_CURVE('',#11076,#11074,#6729,.T.);
#14550=EDGE_CURVE('',#11075,#11076,#6730,.T.);
#14551=EDGE_CURVE('',#11075,#11077,#6731,.T.);
#14552=EDGE_CURVE('',#11078,#11076,#6732,.T.);
#14553=EDGE_CURVE('',#11077,#11078,#6733,.T.);
#14554=EDGE_CURVE('',#11077,#11079,#6734,.T.);
#14555=EDGE_CURVE('',#11080,#11078,#6735,.T.);
#14556=EDGE_CURVE('',#11079,#11080,#6736,.T.);
#14557=EDGE_CURVE('',#11079,#11067,#6737,.T.);
#14558=EDGE_CURVE('',#11069,#11080,#6738,.T.);
#14559=EDGE_CURVE('',#11081,#11081,#5758,.T.);
#14560=EDGE_CURVE('',#11081,#11082,#6739,.T.);
#14561=EDGE_CURVE('',#11082,#11082,#5759,.T.);
#14562=EDGE_CURVE('',#11083,#11083,#5760,.T.);
#14563=EDGE_CURVE('',#11083,#11065,#6740,.T.);
#14564=EDGE_CURVE('',#11084,#11084,#5761,.T.);
#14565=EDGE_CURVE('',#11084,#11066,#6741,.T.);
#14566=EDGE_CURVE('',#11085,#11086,#5762,.T.);
#14567=EDGE_CURVE('',#11085,#11087,#6742,.T.);
#14568=EDGE_CURVE('',#11087,#11088,#5763,.T.);
#14569=EDGE_CURVE('',#11086,#11088,#6743,.T.);
#14570=EDGE_CURVE('',#11089,#11085,#6744,.T.);
#14571=EDGE_CURVE('',#11089,#11090,#6745,.T.);
#14572=EDGE_CURVE('',#11090,#11087,#6746,.T.);
#14573=EDGE_CURVE('',#11091,#11089,#5764,.T.);
#14574=EDGE_CURVE('',#11091,#11092,#6747,.T.);
#14575=EDGE_CURVE('',#11092,#11090,#5765,.T.);
#14576=EDGE_CURVE('',#11031,#11091,#6748,.T.);
#14577=EDGE_CURVE('',#11030,#11092,#6749,.T.);
#14578=EDGE_CURVE('',#11086,#11028,#6750,.T.);
#14579=EDGE_CURVE('',#11088,#11029,#6751,.T.);
#14580=EDGE_CURVE('',#11093,#11093,#5766,.T.);
#14581=EDGE_CURVE('',#11094,#11094,#5767,.T.);
#14582=EDGE_CURVE('',#11095,#11096,#6752,.T.);
#14583=EDGE_CURVE('',#11095,#11097,#6753,.T.);
#14584=EDGE_CURVE('',#11097,#11098,#6754,.T.);
#14585=EDGE_CURVE('',#11096,#11098,#6755,.T.);
#14586=EDGE_CURVE('',#11099,#11095,#6756,.T.);
#14587=EDGE_CURVE('',#11099,#11100,#6757,.T.);
#14588=EDGE_CURVE('',#11100,#11097,#6758,.T.);
#14589=EDGE_CURVE('',#11101,#11099,#6759,.T.);
#14590=EDGE_CURVE('',#11101,#11102,#6760,.T.);
#14591=EDGE_CURVE('',#11102,#11100,#6761,.T.);
#14592=EDGE_CURVE('',#11103,#11101,#6762,.T.);
#14593=EDGE_CURVE('',#11103,#11104,#6763,.T.);
#14594=EDGE_CURVE('',#11104,#11102,#6764,.T.);
#14595=EDGE_CURVE('',#11105,#11103,#6765,.T.);
#14596=EDGE_CURVE('',#11105,#11106,#6766,.T.);
#14597=EDGE_CURVE('',#11106,#11104,#6767,.T.);
#14598=EDGE_CURVE('',#11107,#11105,#6768,.T.);
#14599=EDGE_CURVE('',#11107,#11108,#6769,.T.);
#14600=EDGE_CURVE('',#11108,#11106,#6770,.T.);
#14601=EDGE_CURVE('',#11096,#11107,#6771,.T.);
#14602=EDGE_CURVE('',#11098,#11108,#6772,.T.);
#14603=EDGE_CURVE('',#11109,#11109,#5768,.T.);
#14604=EDGE_CURVE('',#11109,#11110,#6773,.T.);
#14605=EDGE_CURVE('',#11110,#11110,#5769,.T.);
#14606=EDGE_CURVE('',#11111,#11112,#6774,.T.);
#14607=EDGE_CURVE('',#11111,#11113,#6775,.T.);
#14608=EDGE_CURVE('',#11113,#11114,#6776,.T.);
#14609=EDGE_CURVE('',#11112,#11114,#6777,.T.);
#14610=EDGE_CURVE('',#11115,#11111,#6778,.T.);
#14611=EDGE_CURVE('',#11115,#11116,#6779,.T.);
#14612=EDGE_CURVE('',#11116,#11113,#6780,.T.);
#14613=EDGE_CURVE('',#11117,#11115,#6781,.T.);
#14614=EDGE_CURVE('',#11117,#11118,#6782,.T.);
#14615=EDGE_CURVE('',#11118,#11116,#6783,.T.);
#14616=EDGE_CURVE('',#11119,#11117,#6784,.T.);
#14617=EDGE_CURVE('',#11119,#11120,#6785,.T.);
#14618=EDGE_CURVE('',#11120,#11118,#6786,.T.);
#14619=EDGE_CURVE('',#11121,#11119,#6787,.T.);
#14620=EDGE_CURVE('',#11121,#11122,#6788,.T.);
#14621=EDGE_CURVE('',#11122,#11120,#6789,.T.);
#14622=EDGE_CURVE('',#11123,#11121,#6790,.T.);
#14623=EDGE_CURVE('',#11123,#11124,#6791,.T.);
#14624=EDGE_CURVE('',#11124,#11122,#6792,.T.);
#14625=EDGE_CURVE('',#11112,#11123,#6793,.T.);
#14626=EDGE_CURVE('',#11114,#11124,#6794,.T.);
#14627=EDGE_CURVE('',#11125,#11125,#5770,.T.);
#14628=EDGE_CURVE('',#11125,#11126,#6795,.T.);
#14629=EDGE_CURVE('',#11126,#11126,#5771,.T.);
#14630=EDGE_CURVE('',#11127,#11027,#6796,.T.);
#14631=EDGE_CURVE('',#11128,#11127,#6797,.T.);
#14632=EDGE_CURVE('',#11128,#11032,#6798,.T.);
#14633=EDGE_CURVE('',#11094,#11129,#6799,.T.);
#14634=EDGE_CURVE('',#11129,#11129,#5772,.T.);
#14635=EDGE_CURVE('',#11093,#11130,#6800,.T.);
#14636=EDGE_CURVE('',#11130,#11130,#5773,.T.);
#14637=EDGE_CURVE('',#11039,#11131,#6801,.T.);
#14638=EDGE_CURVE('',#11131,#11131,#5774,.T.);
#14639=EDGE_CURVE('',#11040,#11132,#6802,.T.);
#14640=EDGE_CURVE('',#11132,#11132,#5775,.T.);
#14641=EDGE_CURVE('',#11133,#11002,#6803,.T.);
#14642=EDGE_CURVE('',#11011,#11133,#6804,.T.);
#14643=EDGE_CURVE('',#11133,#11010,#5776,.T.);
#14644=EDGE_CURVE('',#11134,#11009,#5777,.T.);
#14645=EDGE_CURVE('',#11134,#11038,#6805,.T.);
#14646=EDGE_CURVE('',#11134,#11135,#6806,.T.);
#14647=EDGE_CURVE('',#11135,#11037,#6807,.T.);
#14648=EDGE_CURVE('',#11135,#11136,#5778,.T.);
#14649=EDGE_CURVE('',#11136,#11036,#6808,.T.);
#14650=EDGE_CURVE('',#11136,#11137,#6809,.T.);
#14651=EDGE_CURVE('',#11137,#11035,#6810,.T.);
#14652=EDGE_CURVE('',#11137,#11138,#5779,.T.);
#14653=EDGE_CURVE('',#11138,#11034,#6811,.T.);
#14654=EDGE_CURVE('',#11138,#11139,#6812,.T.);
#14655=EDGE_CURVE('',#11139,#11033,#6813,.T.);
#14656=EDGE_CURVE('',#11139,#11128,#5780,.T.);
#14657=EDGE_CURVE('',#11127,#11140,#5781,.T.);
#14658=EDGE_CURVE('',#11140,#11026,#6814,.T.);
#14659=EDGE_CURVE('',#11140,#11141,#6815,.T.);
#14660=EDGE_CURVE('',#11141,#11025,#6816,.T.);
#14661=EDGE_CURVE('',#11141,#11142,#5782,.T.);
#14662=EDGE_CURVE('',#11142,#11024,#6817,.T.);
#14663=EDGE_CURVE('',#11143,#11019,#6818,.T.);
#14664=EDGE_CURVE('',#11143,#11142,#6819,.T.);
#14665=EDGE_CURVE('',#11143,#11144,#5783,.T.);
#14666=EDGE_CURVE('',#11144,#11018,#6820,.T.);
#14667=EDGE_CURVE('',#11145,#11144,#6821,.T.);
#14668=EDGE_CURVE('',#11145,#11017,#6822,.T.);
#14669=EDGE_CURVE('',#11145,#11146,#5784,.T.);
#14670=EDGE_CURVE('',#11146,#11016,#6823,.T.);
#14671=EDGE_CURVE('',#11147,#11146,#6824,.T.);
#14672=EDGE_CURVE('',#11147,#11015,#6825,.T.);
#14673=EDGE_CURVE('',#11147,#11148,#5785,.T.);
#14674=EDGE_CURVE('',#11148,#11014,#6826,.T.);
#14675=EDGE_CURVE('',#11149,#11148,#6827,.T.);
#14676=EDGE_CURVE('',#11149,#11013,#6828,.T.);
#14677=EDGE_CURVE('',#11150,#11149,#5786,.T.);
#14678=EDGE_CURVE('',#11150,#11012,#6829,.T.);
#14679=EDGE_CURVE('',#11151,#10992,#6830,.T.);
#14680=EDGE_CURVE('',#11151,#11150,#6831,.T.);
#14681=EDGE_CURVE('',#11151,#11007,#5787,.T.);
#14682=EDGE_CURVE('',#11152,#11152,#5788,.T.);
#14683=EDGE_CURVE('',#11152,#11153,#6832,.T.);
#14684=EDGE_CURVE('',#11153,#11153,#5789,.T.);
#14685=EDGE_CURVE('',#11154,#11154,#5790,.T.);
#14686=EDGE_CURVE('',#11154,#11155,#6833,.T.);
#14687=EDGE_CURVE('',#11155,#11155,#5791,.T.);
#14688=EDGE_CURVE('',#11156,#11157,#6834,.T.);
#14689=EDGE_CURVE('',#11157,#11158,#5792,.T.);
#14690=EDGE_CURVE('',#11158,#11159,#6835,.T.);
#14691=EDGE_CURVE('',#11159,#11156,#95,.T.);
#14692=EDGE_CURVE('',#11157,#11160,#6836,.T.);
#14693=EDGE_CURVE('',#11160,#11161,#5793,.T.);
#14694=EDGE_CURVE('',#11161,#11158,#6837,.T.);
#14695=EDGE_CURVE('',#11162,#11163,#5794,.T.);
#14696=EDGE_CURVE('',#11163,#11164,#6838,.T.);
#14697=EDGE_CURVE('',#11164,#11165,#5795,.T.);
#14698=EDGE_CURVE('',#11165,#11162,#6839,.T.);
#14699=EDGE_CURVE('',#11166,#11167,#5796,.T.);
#14700=EDGE_CURVE('',#11167,#11165,#5797,.T.);
#14701=EDGE_CURVE('',#11164,#11166,#5798,.T.);
#14702=EDGE_CURVE('',#11168,#11169,#5799,.T.);
#14703=EDGE_CURVE('',#11169,#11167,#6840,.T.);
#14704=EDGE_CURVE('',#11166,#11168,#6841,.T.);
#14705=EDGE_CURVE('',#11170,#11171,#5800,.T.);
#14706=EDGE_CURVE('',#11171,#11169,#5801,.T.);
#14707=EDGE_CURVE('',#11168,#11170,#5802,.T.);
#14708=EDGE_CURVE('',#11172,#11173,#5803,.T.);
#14709=EDGE_CURVE('',#11173,#11171,#6842,.T.);
#14710=EDGE_CURVE('',#11170,#11172,#6843,.T.);
#14711=EDGE_CURVE('',#11174,#11175,#5804,.T.);
#14712=EDGE_CURVE('',#11175,#11173,#5805,.T.);
#14713=EDGE_CURVE('',#11172,#11174,#5806,.T.);
#14714=EDGE_CURVE('',#11176,#11177,#5807,.T.);
#14715=EDGE_CURVE('',#11177,#11175,#6844,.T.);
#14716=EDGE_CURVE('',#11174,#11176,#6845,.T.);
#14717=EDGE_CURVE('',#11178,#11179,#5808,.T.);
#14718=EDGE_CURVE('',#11179,#11177,#5809,.T.);
#14719=EDGE_CURVE('',#11176,#11178,#5810,.T.);
#14720=EDGE_CURVE('',#11180,#11179,#6846,.T.);
#14721=EDGE_CURVE('',#11178,#11181,#6847,.T.);
#14722=EDGE_CURVE('',#11181,#11180,#96,.T.);
#14723=EDGE_CURVE('',#11182,#11180,#6848,.T.);
#14724=EDGE_CURVE('',#11181,#11183,#6849,.T.);
#14725=EDGE_CURVE('',#11183,#11182,#97,.T.);
#14726=EDGE_CURVE('',#11183,#11184,#6850,.T.);
#14727=EDGE_CURVE('',#11184,#11185,#5811,.T.);
#14728=EDGE_CURVE('',#11185,#11182,#6851,.T.);
#14729=EDGE_CURVE('',#11186,#11187,#5812,.T.);
#14730=EDGE_CURVE('',#11187,#11185,#5813,.T.);
#14731=EDGE_CURVE('',#11184,#11186,#5814,.T.);
#14732=EDGE_CURVE('',#11188,#11187,#6852,.T.);
#14733=EDGE_CURVE('',#11186,#11189,#6853,.T.);
#14734=EDGE_CURVE('',#11189,#11188,#98,.T.);
#14735=EDGE_CURVE('',#11160,#11188,#6854,.T.);
#14736=EDGE_CURVE('',#11189,#11161,#6855,.T.);
#14737=EDGE_CURVE('',#11159,#11190,#6856,.T.);
#14738=EDGE_CURVE('',#11190,#11191,#5815,.T.);
#14739=EDGE_CURVE('',#11191,#11156,#6857,.T.);
#14740=EDGE_CURVE('',#11192,#11193,#5816,.T.);
#14741=EDGE_CURVE('',#11193,#11191,#5817,.T.);
#14742=EDGE_CURVE('',#11190,#11192,#5818,.T.);
#14743=EDGE_CURVE('',#11194,#11193,#6858,.T.);
#14744=EDGE_CURVE('',#11192,#11195,#6859,.T.);
#14745=EDGE_CURVE('',#11195,#11194,#99,.T.);
#14746=EDGE_CURVE('',#11195,#11196,#6860,.T.);
#14747=EDGE_CURVE('',#11196,#11197,#100,.T.);
#14748=EDGE_CURVE('',#11197,#11194,#6861,.T.);
#14749=EDGE_CURVE('',#11196,#11198,#6862,.T.);
#14750=EDGE_CURVE('',#11198,#11199,#5819,.T.);
#14751=EDGE_CURVE('',#11199,#11197,#6863,.T.);
#14752=EDGE_CURVE('',#11200,#11201,#5820,.T.);
#14753=EDGE_CURVE('',#11201,#11199,#5821,.T.);
#14754=EDGE_CURVE('',#11198,#11200,#5822,.T.);
#14755=EDGE_CURVE('',#11202,#11203,#5823,.T.);
#14756=EDGE_CURVE('',#11203,#11201,#6864,.T.);
#14757=EDGE_CURVE('',#11200,#11202,#6865,.T.);
#14758=EDGE_CURVE('',#11204,#11205,#5824,.T.);
#14759=EDGE_CURVE('',#11205,#11203,#5825,.T.);
#14760=EDGE_CURVE('',#11202,#11204,#5826,.T.);
#14761=EDGE_CURVE('',#11206,#11207,#5827,.T.);
#14762=EDGE_CURVE('',#11207,#11205,#6866,.T.);
#14763=EDGE_CURVE('',#11204,#11206,#6867,.T.);
#14764=EDGE_CURVE('',#11208,#11209,#5828,.T.);
#14765=EDGE_CURVE('',#11209,#11207,#5829,.T.);
#14766=EDGE_CURVE('',#11206,#11208,#5830,.T.);
#14767=EDGE_CURVE('',#11210,#11211,#5831,.T.);
#14768=EDGE_CURVE('',#11211,#11209,#6868,.T.);
#14769=EDGE_CURVE('',#11208,#11210,#6869,.T.);
#14770=EDGE_CURVE('',#11212,#11213,#5832,.T.);
#14771=EDGE_CURVE('',#11213,#11211,#5833,.T.);
#14772=EDGE_CURVE('',#11210,#11212,#5834,.T.);
#14773=EDGE_CURVE('',#11214,#11215,#5835,.T.);
#14774=EDGE_CURVE('',#11215,#11213,#6870,.T.);
#14775=EDGE_CURVE('',#11212,#11214,#6871,.T.);
#14776=EDGE_CURVE('',#11216,#11217,#5836,.T.);
#14777=EDGE_CURVE('',#11217,#11163,#6872,.T.);
#14778=EDGE_CURVE('',#11163,#11218,#5837,.T.);
#14779=EDGE_CURVE('',#11218,#11216,#6873,.T.);
#14780=EDGE_CURVE('',#11216,#11219,#6874,.T.);
#14781=EDGE_CURVE('',#11219,#11220,#5838,.T.);
#14782=EDGE_CURVE('',#11220,#11217,#6875,.T.);
#14783=EDGE_CURVE('',#11219,#11221,#6876,.T.);
#14784=EDGE_CURVE('',#11221,#11214,#5839,.T.);
#14785=EDGE_CURVE('',#11214,#11220,#6877,.T.);
#14786=EDGE_CURVE('',#11221,#11215,#5840,.T.);
#14787=EDGE_CURVE('',#11162,#11218,#5841,.T.);
#14788=EDGE_CURVE('',#11191,#11222,#6878,.T.);
#14789=EDGE_CURVE('',#11223,#11222,#6879,.T.);
#14790=EDGE_CURVE('',#11156,#11223,#6880,.T.);
#14791=EDGE_CURVE('',#11193,#11224,#6881,.T.);
#14792=EDGE_CURVE('',#11222,#11224,#5842,.T.);
#14793=EDGE_CURVE('',#11194,#11225,#6882,.T.);
#14794=EDGE_CURVE('',#11224,#11225,#6883,.T.);
#14795=EDGE_CURVE('',#11197,#11226,#6884,.T.);
#14796=EDGE_CURVE('',#11225,#11226,#6885,.T.);
#14797=EDGE_CURVE('',#11199,#11227,#6886,.T.);
#14798=EDGE_CURVE('',#11226,#11227,#6887,.T.);
#14799=EDGE_CURVE('',#11201,#11228,#6888,.T.);
#14800=EDGE_CURVE('',#11227,#11228,#5843,.T.);
#14801=EDGE_CURVE('',#11203,#11229,#6889,.T.);
#14802=EDGE_CURVE('',#11228,#11229,#6890,.T.);
#14803=EDGE_CURVE('',#11205,#11230,#6891,.T.);
#14804=EDGE_CURVE('',#11229,#11230,#5844,.T.);
#14805=EDGE_CURVE('',#11207,#11231,#6892,.T.);
#14806=EDGE_CURVE('',#11230,#11231,#6893,.T.);
#14807=EDGE_CURVE('',#11209,#11232,#6894,.T.);
#14808=EDGE_CURVE('',#11232,#11233,#5845,.T.);
#14809=EDGE_CURVE('',#11233,#11234,#6895,.T.);
#14810=EDGE_CURVE('',#11231,#11234,#5846,.T.);
#14811=EDGE_CURVE('',#11211,#11235,#6896,.T.);
#14812=EDGE_CURVE('',#11235,#11232,#6897,.T.);
#14813=EDGE_CURVE('',#11213,#11236,#6898,.T.);
#14814=EDGE_CURVE('',#11236,#11235,#5847,.T.);
#14815=EDGE_CURVE('',#11215,#11237,#6899,.T.);
#14816=EDGE_CURVE('',#11238,#11237,#6900,.T.);
#14817=EDGE_CURVE('',#11238,#11239,#6901,.T.);
#14818=EDGE_CURVE('',#11239,#11236,#6902,.T.);
#14819=EDGE_CURVE('',#11221,#11240,#6903,.T.);
#14820=EDGE_CURVE('',#11237,#11240,#5848,.T.);
#14821=EDGE_CURVE('',#11219,#11241,#6904,.T.);
#14822=EDGE_CURVE('',#11240,#11241,#6905,.T.);
#14823=EDGE_CURVE('',#11216,#11242,#6906,.T.);
#14824=EDGE_CURVE('',#11241,#11242,#6907,.T.);
#14825=EDGE_CURVE('',#11218,#11243,#6908,.T.);
#14826=EDGE_CURVE('',#11242,#11243,#6909,.T.);
#14827=EDGE_CURVE('',#11237,#11244,#5849,.T.);
#14828=EDGE_CURVE('',#11244,#11245,#6910,.T.);
#14829=EDGE_CURVE('',#11245,#11238,#1143,.T.);
#14830=EDGE_CURVE('',#11245,#11246,#5850,.T.);
#14831=EDGE_CURVE('',#11246,#11247,#1144,.T.);
#14832=EDGE_CURVE('',#11247,#11234,#1145,.T.);
#14833=EDGE_CURVE('',#11234,#11238,#5851,.T.);
#14834=EDGE_CURVE('',#11241,#11248,#5852,.T.);
#14835=EDGE_CURVE('',#11248,#11244,#6911,.T.);
#14836=EDGE_CURVE('',#11244,#11240,#5853,.T.);
#14837=EDGE_CURVE('',#11242,#11249,#5854,.T.);
#14838=EDGE_CURVE('',#11249,#11248,#6912,.T.);
#14839=EDGE_CURVE('',#11243,#11250,#5855,.T.);
#14840=EDGE_CURVE('',#11250,#11249,#6913,.T.);
#14841=EDGE_CURVE('',#11251,#11252,#5856,.T.);
#14842=EDGE_CURVE('',#11252,#11253,#1146,.T.);
#14843=EDGE_CURVE('',#11253,#11254,#1147,.T.);
#14844=EDGE_CURVE('',#11254,#11255,#5857,.T.);
#14845=EDGE_CURVE('',#11255,#11251,#1148,.T.);
#14846=EDGE_CURVE('',#11255,#11250,#6914,.T.);
#14847=EDGE_CURVE('',#11250,#11256,#5858,.T.);
#14848=EDGE_CURVE('',#11256,#11251,#6915,.T.);
#14849=EDGE_CURVE('',#11243,#11256,#5859,.T.);
#14850=EDGE_CURVE('',#11246,#11257,#6916,.T.);
#14851=EDGE_CURVE('',#11230,#11257,#5860,.T.);
#14852=EDGE_CURVE('',#11231,#11247,#5861,.T.);
#14853=EDGE_CURVE('',#11258,#11254,#6917,.T.);
#14854=EDGE_CURVE('',#11259,#11258,#5862,.T.);
#14855=EDGE_CURVE('',#11260,#11259,#6918,.T.);
#14856=EDGE_CURVE('',#11261,#11260,#5863,.T.);
#14857=EDGE_CURVE('',#11262,#11261,#6919,.T.);
#14858=EDGE_CURVE('',#11263,#11262,#6920,.T.);
#14859=EDGE_CURVE('',#11264,#11263,#6921,.T.);
#14860=EDGE_CURVE('',#11265,#11264,#5864,.T.);
#14861=EDGE_CURVE('',#11266,#11265,#6922,.T.);
#14862=EDGE_CURVE('',#11267,#11266,#6923,.T.);
#14863=EDGE_CURVE('',#11268,#11267,#6924,.T.);
#14864=EDGE_CURVE('',#11269,#11268,#6925,.T.);
#14865=EDGE_CURVE('',#11270,#11269,#6926,.T.);
#14866=EDGE_CURVE('',#11271,#11270,#5865,.T.);
#14867=EDGE_CURVE('',#11272,#11271,#6927,.T.);
#14868=EDGE_CURVE('',#11273,#11272,#6928,.T.);
#14869=EDGE_CURVE('',#11274,#11273,#6929,.T.);
#14870=EDGE_CURVE('',#11275,#11274,#5866,.T.);
#14871=EDGE_CURVE('',#11276,#11275,#6930,.T.);
#14872=EDGE_CURVE('',#11257,#11276,#5867,.T.);
#14873=EDGE_CURVE('',#11277,#11253,#5868,.T.);
#14874=EDGE_CURVE('',#11277,#11278,#6931,.T.);
#14875=EDGE_CURVE('',#11278,#11258,#5869,.T.);
#14876=EDGE_CURVE('',#11252,#11277,#5870,.T.);
#14877=EDGE_CURVE('',#11227,#11274,#5871,.T.);
#14878=EDGE_CURVE('',#11273,#11226,#101,.T.);
#14879=EDGE_CURVE('',#11228,#11275,#5872,.T.);
#14880=EDGE_CURVE('',#11229,#11276,#5873,.T.);
#14881=EDGE_CURVE('',#11272,#11225,#102,.T.);
#14882=EDGE_CURVE('',#11222,#11270,#5874,.T.);
#14883=EDGE_CURVE('',#11269,#11223,#103,.T.);
#14884=EDGE_CURVE('',#11224,#11271,#5875,.T.);
#14885=EDGE_CURVE('',#11279,#11280,#6932,.T.);
#14886=EDGE_CURVE('',#11280,#11267,#5876,.T.);
#14887=EDGE_CURVE('',#11266,#11279,#104,.T.);
#14888=EDGE_CURVE('',#11281,#11268,#5877,.T.);
#14889=EDGE_CURVE('',#11280,#11281,#6933,.T.);
#14890=EDGE_CURVE('',#11281,#11223,#6934,.T.);
#14891=EDGE_CURVE('',#11282,#11283,#6935,.T.);
#14892=EDGE_CURVE('',#11283,#11264,#5878,.T.);
#14893=EDGE_CURVE('',#11263,#11282,#105,.T.);
#14894=EDGE_CURVE('',#11284,#11265,#5879,.T.);
#14895=EDGE_CURVE('',#11283,#11284,#5880,.T.);
#14896=EDGE_CURVE('',#11284,#11279,#6936,.T.);
#14897=EDGE_CURVE('',#11285,#11282,#6937,.T.);
#14898=EDGE_CURVE('',#11262,#11285,#106,.T.);
#14899=EDGE_CURVE('',#11286,#11259,#5881,.T.);
#14900=EDGE_CURVE('',#11278,#11286,#5882,.T.);
#14901=EDGE_CURVE('',#11287,#11260,#5883,.T.);
#14902=EDGE_CURVE('',#11286,#11287,#6938,.T.);
#14903=EDGE_CURVE('',#11288,#11261,#5884,.T.);
#14904=EDGE_CURVE('',#11287,#11288,#5885,.T.);
#14905=EDGE_CURVE('',#11288,#11285,#6939,.T.);
#14906=EDGE_CURVE('',#11157,#11281,#6940,.T.);
#14907=EDGE_CURVE('',#11160,#11280,#6941,.T.);
#14908=EDGE_CURVE('',#11188,#11279,#6942,.T.);
#14909=EDGE_CURVE('',#11187,#11284,#6943,.T.);
#14910=EDGE_CURVE('',#11185,#11283,#6944,.T.);
#14911=EDGE_CURVE('',#11182,#11282,#6945,.T.);
#14912=EDGE_CURVE('',#11180,#11285,#6946,.T.);
#14913=EDGE_CURVE('',#11179,#11288,#6947,.T.);
#14914=EDGE_CURVE('',#11177,#11287,#6948,.T.);
#14915=EDGE_CURVE('',#11175,#11286,#6949,.T.);
#14916=EDGE_CURVE('',#11173,#11278,#6950,.T.);
#14917=EDGE_CURVE('',#11171,#11277,#6951,.T.);
#14918=EDGE_CURVE('',#11252,#11289,#6952,.T.);
#14919=EDGE_CURVE('',#11289,#11290,#5886,.T.);
#14920=EDGE_CURVE('',#11169,#11290,#6953,.T.);
#14921=EDGE_CURVE('',#11291,#11251,#6954,.T.);
#14922=EDGE_CURVE('',#11291,#11289,#5887,.T.);
#14923=EDGE_CURVE('',#11233,#11239,#5888,.T.);
#14924=EDGE_CURVE('',#11290,#11292,#6955,.T.);
#14925=EDGE_CURVE('',#11293,#11291,#6956,.T.);
#14926=EDGE_CURVE('',#11292,#11293,#5889,.T.);
#14927=EDGE_CURVE('',#11167,#11292,#6957,.T.);
#14928=EDGE_CURVE('',#11165,#11293,#6958,.T.);
#14929=EDGE_CURVE('',#11162,#11256,#6959,.T.);
#14930=EDGE_CURVE('',#11294,#11294,#5890,.T.);
#14931=EDGE_CURVE('',#11294,#11295,#6960,.T.);
#14932=EDGE_CURVE('',#11295,#11295,#5891,.T.);
#14933=EDGE_CURVE('',#11296,#11296,#5892,.T.);
#14934=EDGE_CURVE('',#11296,#11297,#6961,.T.);
#14935=EDGE_CURVE('',#11297,#11297,#5893,.T.);
#14936=EDGE_CURVE('',#11298,#11299,#6962,.T.);
#14937=EDGE_CURVE('',#11300,#11298,#107,.T.);
#14938=EDGE_CURVE('',#11301,#11300,#6963,.T.);
#14939=EDGE_CURVE('',#11299,#11301,#5894,.T.);
#14940=EDGE_CURVE('',#11302,#11301,#6964,.T.);
#14941=EDGE_CURVE('',#11303,#11302,#5895,.T.);
#14942=EDGE_CURVE('',#11299,#11303,#6965,.T.);
#14943=EDGE_CURVE('',#11304,#11305,#5896,.T.);
#14944=EDGE_CURVE('',#11306,#11304,#6966,.T.);
#14945=EDGE_CURVE('',#11307,#11306,#5897,.T.);
#14946=EDGE_CURVE('',#11305,#11307,#6967,.T.);
#14947=EDGE_CURVE('',#11308,#11309,#5898,.T.);
#14948=EDGE_CURVE('',#11307,#11308,#5899,.T.);
#14949=EDGE_CURVE('',#11309,#11306,#5900,.T.);
#14950=EDGE_CURVE('',#11310,#11311,#5901,.T.);
#14951=EDGE_CURVE('',#11308,#11310,#6968,.T.);
#14952=EDGE_CURVE('',#11311,#11309,#6969,.T.);
#14953=EDGE_CURVE('',#11312,#11313,#5902,.T.);
#14954=EDGE_CURVE('',#11310,#11312,#5903,.T.);
#14955=EDGE_CURVE('',#11313,#11311,#5904,.T.);
#14956=EDGE_CURVE('',#11314,#11315,#5905,.T.);
#14957=EDGE_CURVE('',#11312,#11314,#6970,.T.);
#14958=EDGE_CURVE('',#11315,#11313,#6971,.T.);
#14959=EDGE_CURVE('',#11316,#11317,#5906,.T.);
#14960=EDGE_CURVE('',#11314,#11316,#5907,.T.);
#14961=EDGE_CURVE('',#11317,#11315,#5908,.T.);
#14962=EDGE_CURVE('',#11318,#11319,#5909,.T.);
#14963=EDGE_CURVE('',#11316,#11318,#6972,.T.);
#14964=EDGE_CURVE('',#11319,#11317,#6973,.T.);
#14965=EDGE_CURVE('',#11320,#11321,#5910,.T.);
#14966=EDGE_CURVE('',#11318,#11320,#5911,.T.);
#14967=EDGE_CURVE('',#11321,#11319,#5912,.T.);
#14968=EDGE_CURVE('',#11322,#11321,#6974,.T.);
#14969=EDGE_CURVE('',#11323,#11322,#108,.T.);
#14970=EDGE_CURVE('',#11320,#11323,#6975,.T.);
#14971=EDGE_CURVE('',#11324,#11322,#6976,.T.);
#14972=EDGE_CURVE('',#11325,#11324,#109,.T.);
#14973=EDGE_CURVE('',#11323,#11325,#6977,.T.);
#14974=EDGE_CURVE('',#11325,#11326,#6978,.T.);
#14975=EDGE_CURVE('',#11327,#11324,#6979,.T.);
#14976=EDGE_CURVE('',#11326,#11327,#5913,.T.);
#14977=EDGE_CURVE('',#11328,#11329,#5914,.T.);
#14978=EDGE_CURVE('',#11326,#11328,#5915,.T.);
#14979=EDGE_CURVE('',#11329,#11327,#5916,.T.);
#14980=EDGE_CURVE('',#11330,#11329,#6980,.T.);
#14981=EDGE_CURVE('',#11331,#11330,#110,.T.);
#14982=EDGE_CURVE('',#11328,#11331,#6981,.T.);
#14983=EDGE_CURVE('',#11331,#11302,#6982,.T.);
#14984=EDGE_CURVE('',#11303,#11330,#6983,.T.);
#14985=EDGE_CURVE('',#11300,#11332,#6984,.T.);
#14986=EDGE_CURVE('',#11333,#11298,#6985,.T.);
#14987=EDGE_CURVE('',#11332,#11333,#5917,.T.);
#14988=EDGE_CURVE('',#11334,#11335,#5918,.T.);
#14989=EDGE_CURVE('',#11332,#11334,#5919,.T.);
#14990=EDGE_CURVE('',#11335,#11333,#5920,.T.);
#14991=EDGE_CURVE('',#11336,#11335,#6986,.T.);
#14992=EDGE_CURVE('',#11337,#11336,#111,.T.);
#14993=EDGE_CURVE('',#11334,#11337,#6987,.T.);
#14994=EDGE_CURVE('',#11337,#11338,#6988,.T.);
#14995=EDGE_CURVE('',#11339,#11336,#6989,.T.);
#14996=EDGE_CURVE('',#11338,#11339,#112,.T.);
#14997=EDGE_CURVE('',#11338,#11340,#6990,.T.);
#14998=EDGE_CURVE('',#11341,#11339,#6991,.T.);
#14999=EDGE_CURVE('',#11340,#11341,#5921,.T.);
#15000=EDGE_CURVE('',#11342,#11343,#5922,.T.);
#15001=EDGE_CURVE('',#11340,#11342,#5923,.T.);
#15002=EDGE_CURVE('',#11343,#11341,#5924,.T.);
#15003=EDGE_CURVE('',#11344,#11345,#5925,.T.);
#15004=EDGE_CURVE('',#11342,#11344,#6992,.T.);
#15005=EDGE_CURVE('',#11345,#11343,#6993,.T.);
#15006=EDGE_CURVE('',#11346,#11347,#5926,.T.);
#15007=EDGE_CURVE('',#11344,#11346,#5927,.T.);
#15008=EDGE_CURVE('',#11347,#11345,#5928,.T.);
#15009=EDGE_CURVE('',#11348,#11349,#5929,.T.);
#15010=EDGE_CURVE('',#11346,#11348,#6994,.T.);
#15011=EDGE_CURVE('',#11349,#11347,#6995,.T.);
#15012=EDGE_CURVE('',#11350,#11351,#5930,.T.);
#15013=EDGE_CURVE('',#11348,#11350,#5931,.T.);
#15014=EDGE_CURVE('',#11351,#11349,#5932,.T.);
#15015=EDGE_CURVE('',#11352,#11353,#5933,.T.);
#15016=EDGE_CURVE('',#11350,#11352,#6996,.T.);
#15017=EDGE_CURVE('',#11353,#11351,#6997,.T.);
#15018=EDGE_CURVE('',#11354,#11355,#5934,.T.);
#15019=EDGE_CURVE('',#11352,#11354,#5935,.T.);
#15020=EDGE_CURVE('',#11355,#11353,#5936,.T.);
#15021=EDGE_CURVE('',#11356,#11357,#5937,.T.);
#15022=EDGE_CURVE('',#11354,#11356,#6998,.T.);
#15023=EDGE_CURVE('',#11357,#11355,#6999,.T.);
#15024=EDGE_CURVE('',#11358,#11359,#5938,.T.);
#15025=EDGE_CURVE('',#11360,#11358,#7000,.T.);
#15026=EDGE_CURVE('',#11305,#11360,#5939,.T.);
#15027=EDGE_CURVE('',#11359,#11305,#7001,.T.);
#15028=EDGE_CURVE('',#11361,#11359,#7002,.T.);
#15029=EDGE_CURVE('',#11362,#11361,#5940,.T.);
#15030=EDGE_CURVE('',#11358,#11362,#7003,.T.);
#15031=EDGE_CURVE('',#11356,#11361,#7004,.T.);
#15032=EDGE_CURVE('',#11363,#11356,#5941,.T.);
#15033=EDGE_CURVE('',#11362,#11363,#7005,.T.);
#15034=EDGE_CURVE('',#11363,#11357,#5942,.T.);
#15035=EDGE_CURVE('',#11304,#11360,#5943,.T.);
#15036=EDGE_CURVE('',#11298,#11364,#7006,.T.);
#15037=EDGE_CURVE('',#11364,#11365,#7007,.T.);
#15038=EDGE_CURVE('',#11333,#11365,#7008,.T.);
#15039=EDGE_CURVE('',#11365,#11366,#5944,.T.);
#15040=EDGE_CURVE('',#11335,#11366,#7009,.T.);
#15041=EDGE_CURVE('',#11366,#11367,#7010,.T.);
#15042=EDGE_CURVE('',#11336,#11367,#7011,.T.);
#15043=EDGE_CURVE('',#11367,#11368,#7012,.T.);
#15044=EDGE_CURVE('',#11339,#11368,#7013,.T.);
#15045=EDGE_CURVE('',#11368,#11369,#7014,.T.);
#15046=EDGE_CURVE('',#11341,#11369,#7015,.T.);
#15047=EDGE_CURVE('',#11369,#11370,#5945,.T.);
#15048=EDGE_CURVE('',#11343,#11370,#7016,.T.);
#15049=EDGE_CURVE('',#11370,#11371,#7017,.T.);
#15050=EDGE_CURVE('',#11345,#11371,#7018,.T.);
#15051=EDGE_CURVE('',#11371,#11372,#5946,.T.);
#15052=EDGE_CURVE('',#11347,#11372,#7019,.T.);
#15053=EDGE_CURVE('',#11372,#11373,#7020,.T.);
#15054=EDGE_CURVE('',#11349,#11373,#7021,.T.);
#15055=EDGE_CURVE('',#11373,#11374,#5947,.T.);
#15056=EDGE_CURVE('',#11375,#11374,#7022,.T.);
#15057=EDGE_CURVE('',#11376,#11375,#5948,.T.);
#15058=EDGE_CURVE('',#11351,#11376,#7023,.T.);
#15059=EDGE_CURVE('',#11377,#11376,#7024,.T.);
#15060=EDGE_CURVE('',#11353,#11377,#7025,.T.);
#15061=EDGE_CURVE('',#11378,#11377,#5949,.T.);
#15062=EDGE_CURVE('',#11355,#11378,#7026,.T.);
#15063=EDGE_CURVE('',#11379,#11378,#7027,.T.);
#15064=EDGE_CURVE('',#11380,#11379,#7028,.T.);
#15065=EDGE_CURVE('',#11380,#11381,#7029,.T.);
#15066=EDGE_CURVE('',#11357,#11381,#7030,.T.);
#15067=EDGE_CURVE('',#11381,#11382,#5950,.T.);
#15068=EDGE_CURVE('',#11363,#11382,#7031,.T.);
#15069=EDGE_CURVE('',#11382,#11383,#7032,.T.);
#15070=EDGE_CURVE('',#11362,#11383,#7033,.T.);
#15071=EDGE_CURVE('',#11383,#11384,#7034,.T.);
#15072=EDGE_CURVE('',#11358,#11384,#7035,.T.);
#15073=EDGE_CURVE('',#11384,#11385,#7036,.T.);
#15074=EDGE_CURVE('',#11360,#11385,#7037,.T.);
#15075=EDGE_CURVE('',#11386,#11380,#1149,.T.);
#15076=EDGE_CURVE('',#11387,#11386,#7038,.T.);
#15077=EDGE_CURVE('',#11381,#11387,#5951,.T.);
#15078=EDGE_CURVE('',#11386,#11388,#5952,.T.);
#15079=EDGE_CURVE('',#11374,#11380,#5953,.T.);
#15080=EDGE_CURVE('',#11389,#11374,#1150,.T.);
#15081=EDGE_CURVE('',#11388,#11389,#1151,.T.);
#15082=EDGE_CURVE('',#11383,#11390,#5954,.T.);
#15083=EDGE_CURVE('',#11387,#11382,#5955,.T.);
#15084=EDGE_CURVE('',#11390,#11387,#7039,.T.);
#15085=EDGE_CURVE('',#11384,#11391,#5956,.T.);
#15086=EDGE_CURVE('',#11391,#11390,#7040,.T.);
#15087=EDGE_CURVE('',#11392,#11391,#7041,.T.);
#15088=EDGE_CURVE('',#11385,#11392,#5957,.T.);
#15089=EDGE_CURVE('',#11393,#11394,#5958,.T.);
#15090=EDGE_CURVE('',#11395,#11393,#1152,.T.);
#15091=EDGE_CURVE('',#11396,#11395,#5959,.T.);
#15092=EDGE_CURVE('',#11397,#11396,#1153,.T.);
#15093=EDGE_CURVE('',#11394,#11397,#1154,.T.);
#15094=EDGE_CURVE('',#11395,#11392,#7042,.T.);
#15095=EDGE_CURVE('',#11398,#11393,#7043,.T.);
#15096=EDGE_CURVE('',#11392,#11398,#5960,.T.);
#15097=EDGE_CURVE('',#11385,#11398,#5961,.T.);
#15098=EDGE_CURVE('',#11373,#11389,#5962,.T.);
#15099=EDGE_CURVE('',#11372,#11399,#5963,.T.);
#15100=EDGE_CURVE('',#11388,#11399,#7044,.T.);
#15101=EDGE_CURVE('',#11399,#11400,#5964,.T.);
#15102=EDGE_CURVE('',#11400,#11401,#7045,.T.);
#15103=EDGE_CURVE('',#11401,#11402,#5965,.T.);
#15104=EDGE_CURVE('',#11402,#11403,#7046,.T.);
#15105=EDGE_CURVE('',#11403,#11404,#7047,.T.);
#15106=EDGE_CURVE('',#11404,#11405,#7048,.T.);
#15107=EDGE_CURVE('',#11405,#11406,#5966,.T.);
#15108=EDGE_CURVE('',#11406,#11407,#7049,.T.);
#15109=EDGE_CURVE('',#11407,#11408,#7050,.T.);
#15110=EDGE_CURVE('',#11408,#11409,#7051,.T.);
#15111=EDGE_CURVE('',#11409,#11410,#7052,.T.);
#15112=EDGE_CURVE('',#11410,#11411,#7053,.T.);
#15113=EDGE_CURVE('',#11411,#11412,#5967,.T.);
#15114=EDGE_CURVE('',#11412,#11413,#7054,.T.);
#15115=EDGE_CURVE('',#11413,#11414,#7055,.T.);
#15116=EDGE_CURVE('',#11414,#11415,#7056,.T.);
#15117=EDGE_CURVE('',#11415,#11416,#5968,.T.);
#15118=EDGE_CURVE('',#11416,#11417,#7057,.T.);
#15119=EDGE_CURVE('',#11417,#11418,#5969,.T.);
#15120=EDGE_CURVE('',#11418,#11396,#7058,.T.);
#15121=EDGE_CURVE('',#11419,#11418,#5970,.T.);
#15122=EDGE_CURVE('',#11420,#11419,#7059,.T.);
#15123=EDGE_CURVE('',#11420,#11397,#5971,.T.);
#15124=EDGE_CURVE('',#11394,#11420,#5972,.T.);
#15125=EDGE_CURVE('',#11403,#11368,#113,.T.);
#15126=EDGE_CURVE('',#11369,#11402,#5973,.T.);
#15127=EDGE_CURVE('',#11370,#11401,#5974,.T.);
#15128=EDGE_CURVE('',#11371,#11400,#5975,.T.);
#15129=EDGE_CURVE('',#11404,#11367,#114,.T.);
#15130=EDGE_CURVE('',#11407,#11364,#115,.T.);
#15131=EDGE_CURVE('',#11365,#11406,#5976,.T.);
#15132=EDGE_CURVE('',#11366,#11405,#5977,.T.);
#15133=EDGE_CURVE('',#11421,#11422,#7060,.T.);
#15134=EDGE_CURVE('',#11410,#11421,#116,.T.);
#15135=EDGE_CURVE('',#11422,#11409,#5978,.T.);
#15136=EDGE_CURVE('',#11423,#11408,#5979,.T.);
#15137=EDGE_CURVE('',#11422,#11423,#7061,.T.);
#15138=EDGE_CURVE('',#11423,#11364,#7062,.T.);
#15139=EDGE_CURVE('',#11424,#11425,#7063,.T.);
#15140=EDGE_CURVE('',#11413,#11424,#117,.T.);
#15141=EDGE_CURVE('',#11425,#11412,#5980,.T.);
#15142=EDGE_CURVE('',#11426,#11411,#5981,.T.);
#15143=EDGE_CURVE('',#11425,#11426,#5982,.T.);
#15144=EDGE_CURVE('',#11426,#11421,#7064,.T.);
#15145=EDGE_CURVE('',#11427,#11424,#7065,.T.);
#15146=EDGE_CURVE('',#11414,#11427,#118,.T.);
#15147=EDGE_CURVE('',#11428,#11417,#5983,.T.);
#15148=EDGE_CURVE('',#11419,#11428,#5984,.T.);
#15149=EDGE_CURVE('',#11429,#11416,#5985,.T.);
#15150=EDGE_CURVE('',#11428,#11429,#7066,.T.);
#15151=EDGE_CURVE('',#11430,#11415,#5986,.T.);
#15152=EDGE_CURVE('',#11429,#11430,#5987,.T.);
#15153=EDGE_CURVE('',#11430,#11427,#7067,.T.);
#15154=EDGE_CURVE('',#11299,#11423,#7068,.T.);
#15155=EDGE_CURVE('',#11303,#11422,#7069,.T.);
#15156=EDGE_CURVE('',#11330,#11421,#7070,.T.);
#15157=EDGE_CURVE('',#11329,#11426,#7071,.T.);
#15158=EDGE_CURVE('',#11327,#11425,#7072,.T.);
#15159=EDGE_CURVE('',#11324,#11424,#7073,.T.);
#15160=EDGE_CURVE('',#11322,#11427,#7074,.T.);
#15161=EDGE_CURVE('',#11321,#11430,#7075,.T.);
#15162=EDGE_CURVE('',#11319,#11429,#7076,.T.);
#15163=EDGE_CURVE('',#11317,#11428,#7077,.T.);
#15164=EDGE_CURVE('',#11315,#11419,#7078,.T.);
#15165=EDGE_CURVE('',#11313,#11420,#7079,.T.);
#15166=EDGE_CURVE('',#11311,#11431,#7080,.T.);
#15167=EDGE_CURVE('',#11432,#11431,#5988,.T.);
#15168=EDGE_CURVE('',#11394,#11432,#7081,.T.);
#15169=EDGE_CURVE('',#11433,#11432,#5989,.T.);
#15170=EDGE_CURVE('',#11433,#11393,#7082,.T.);
#15171=EDGE_CURVE('',#11375,#11379,#5990,.T.);
#15172=EDGE_CURVE('',#11431,#11434,#7083,.T.);
#15173=EDGE_CURVE('',#11434,#11435,#5991,.T.);
#15174=EDGE_CURVE('',#11435,#11433,#7084,.T.);
#15175=EDGE_CURVE('',#11309,#11434,#7085,.T.);
#15176=EDGE_CURVE('',#11306,#11435,#7086,.T.);
#15177=EDGE_CURVE('',#11304,#11398,#7087,.T.);
#15178=EDGE_CURVE('',#11436,#11437,#5992,.T.);
#15179=EDGE_CURVE('',#11437,#11436,#5993,.T.);
#15180=EDGE_CURVE('',#11437,#11438,#7088,.T.);
#15181=EDGE_CURVE('',#11438,#11438,#5994,.T.);
#15182=EDGE_CURVE('',#11439,#11440,#5995,.T.);
#15183=EDGE_CURVE('',#11440,#11439,#5996,.T.);
#15184=EDGE_CURVE('',#11440,#11441,#7089,.T.);
#15185=EDGE_CURVE('',#11441,#11441,#5997,.T.);
#15186=EDGE_CURVE('',#11437,#11439,#7090,.T.);
#15187=EDGE_CURVE('',#11440,#11442,#7091,.T.);
#15188=EDGE_CURVE('',#11443,#11442,#7092,.T.);
#15189=EDGE_CURVE('',#11444,#11443,#7093,.T.);
#15190=EDGE_CURVE('',#11444,#11445,#7094,.T.);
#15191=EDGE_CURVE('',#11445,#11436,#7095,.T.);
#15192=EDGE_CURVE('',#11446,#11447,#7096,.T.);
#15193=EDGE_CURVE('',#11447,#11446,#5998,.T.);
#15194=EDGE_CURVE('',#11448,#11448,#5999,.T.);
#15195=EDGE_CURVE('',#11448,#11449,#7097,.T.);
#15196=EDGE_CURVE('',#11450,#11449,#1155,.F.);
#15197=EDGE_CURVE('',#11451,#11450,#6000,.T.);
#15198=EDGE_CURVE('',#11452,#11451,#1156,.T.);
#15199=EDGE_CURVE('',#11453,#11452,#7098,.T.);
#15200=EDGE_CURVE('',#11454,#11453,#1157,.T.);
#15201=EDGE_CURVE('',#11455,#11454,#7099,.T.);
#15202=EDGE_CURVE('',#11456,#11455,#1158,.T.);
#15203=EDGE_CURVE('',#11457,#11456,#6001,.T.);
#15204=EDGE_CURVE('',#11458,#11457,#1159,.T.);
#15205=EDGE_CURVE('',#11459,#11458,#119,.T.);
#15206=EDGE_CURVE('',#11460,#11459,#1160,.T.);
#15207=EDGE_CURVE('',#11461,#11460,#7100,.T.);
#15208=EDGE_CURVE('',#11462,#11461,#1161,.T.);
#15209=EDGE_CURVE('',#11463,#11462,#120,.T.);
#15210=EDGE_CURVE('',#11464,#11463,#1162,.T.);
#15211=EDGE_CURVE('',#11465,#11464,#7101,.T.);
#15212=EDGE_CURVE('',#11466,#11465,#1163,.T.);
#15213=EDGE_CURVE('',#11467,#11466,#7102,.T.);
#15214=EDGE_CURVE('',#11468,#11467,#1164,.T.);
#15215=EDGE_CURVE('',#11469,#11468,#121,.T.);
#15216=EDGE_CURVE('',#11469,#11470,#7103,.T.);
#15217=EDGE_CURVE('',#11471,#11470,#122,.T.);
#15218=EDGE_CURVE('',#11472,#11471,#1165,.T.);
#15219=EDGE_CURVE('',#11473,#11472,#7104,.T.);
#15220=EDGE_CURVE('',#11474,#11473,#1166,.T.);
#15221=EDGE_CURVE('',#11475,#11474,#7105,.T.);
#15222=EDGE_CURVE('',#11476,#11475,#1167,.T.);
#15223=EDGE_CURVE('',#11477,#11476,#123,.T.);
#15224=EDGE_CURVE('',#11478,#11477,#1168,.T.);
#15225=EDGE_CURVE('',#11479,#11478,#7106,.T.);
#15226=EDGE_CURVE('',#11480,#11479,#1169,.T.);
#15227=EDGE_CURVE('',#11481,#11480,#124,.T.);
#15228=EDGE_CURVE('',#11482,#11481,#1170,.T.);
#15229=EDGE_CURVE('',#11483,#11482,#6002,.T.);
#15230=EDGE_CURVE('',#11484,#11483,#1171,.T.);
#15231=EDGE_CURVE('',#11485,#11484,#7107,.T.);
#15232=EDGE_CURVE('',#11486,#11485,#1172,.T.);
#15233=EDGE_CURVE('',#11487,#11486,#7108,.T.);
#15234=EDGE_CURVE('',#11488,#11487,#1173,.T.);
#15235=EDGE_CURVE('',#11489,#11488,#6003,.T.);
#15236=EDGE_CURVE('',#11490,#11489,#1174,.T.);
#15237=EDGE_CURVE('',#11490,#11491,#7109,.T.);
#15238=EDGE_CURVE('',#11447,#11491,#6004,.T.);
#15239=EDGE_CURVE('',#11491,#11446,#6005,.T.);
#15240=EDGE_CURVE('',#11492,#11490,#1175,.T.);
#15241=EDGE_CURVE('',#11493,#11492,#125,.T.);
#15242=EDGE_CURVE('',#11494,#11493,#1176,.T.);
#15243=EDGE_CURVE('',#11495,#11494,#7110,.T.);
#15244=EDGE_CURVE('',#11496,#11495,#1177,.T.);
#15245=EDGE_CURVE('',#11470,#11496,#126,.T.);
#15246=EDGE_CURVE('',#11497,#11469,#127,.T.);
#15247=EDGE_CURVE('',#11498,#11497,#1178,.T.);
#15248=EDGE_CURVE('',#11499,#11498,#7111,.T.);
#15249=EDGE_CURVE('',#11500,#11499,#1179,.T.);
#15250=EDGE_CURVE('',#11501,#11500,#128,.T.);
#15251=EDGE_CURVE('',#11449,#11501,#1180,.F.);
#15252=EDGE_CURVE('',#11502,#11503,#7112,.T.);
#15253=EDGE_CURVE('',#11503,#11502,#6006,.T.);
#15254=EDGE_CURVE('',#11504,#11504,#6007,.T.);
#15255=EDGE_CURVE('',#11504,#11505,#7113,.T.);
#15256=EDGE_CURVE('',#11506,#11505,#1181,.F.);
#15257=EDGE_CURVE('',#11507,#11506,#6008,.T.);
#15258=EDGE_CURVE('',#11508,#11507,#1182,.T.);
#15259=EDGE_CURVE('',#11509,#11508,#7114,.T.);
#15260=EDGE_CURVE('',#11510,#11509,#1183,.T.);
#15261=EDGE_CURVE('',#11511,#11510,#7115,.T.);
#15262=EDGE_CURVE('',#11512,#11511,#1184,.T.);
#15263=EDGE_CURVE('',#11513,#11512,#6009,.T.);
#15264=EDGE_CURVE('',#11514,#11513,#1185,.T.);
#15265=EDGE_CURVE('',#11515,#11514,#129,.T.);
#15266=EDGE_CURVE('',#11516,#11515,#1186,.T.);
#15267=EDGE_CURVE('',#11517,#11516,#7116,.T.);
#15268=EDGE_CURVE('',#11518,#11517,#1187,.T.);
#15269=EDGE_CURVE('',#11519,#11518,#130,.T.);
#15270=EDGE_CURVE('',#11520,#11519,#1188,.T.);
#15271=EDGE_CURVE('',#11521,#11520,#7117,.T.);
#15272=EDGE_CURVE('',#11522,#11521,#1189,.T.);
#15273=EDGE_CURVE('',#11523,#11522,#7118,.T.);
#15274=EDGE_CURVE('',#11524,#11523,#1190,.T.);
#15275=EDGE_CURVE('',#11525,#11524,#131,.T.);
#15276=EDGE_CURVE('',#11525,#11526,#7119,.T.);
#15277=EDGE_CURVE('',#11527,#11526,#132,.T.);
#15278=EDGE_CURVE('',#11528,#11527,#1191,.T.);
#15279=EDGE_CURVE('',#11529,#11528,#7120,.T.);
#15280=EDGE_CURVE('',#11530,#11529,#1192,.T.);
#15281=EDGE_CURVE('',#11531,#11530,#7121,.T.);
#15282=EDGE_CURVE('',#11532,#11531,#1193,.T.);
#15283=EDGE_CURVE('',#11533,#11532,#133,.T.);
#15284=EDGE_CURVE('',#11534,#11533,#1194,.T.);
#15285=EDGE_CURVE('',#11535,#11534,#7122,.T.);
#15286=EDGE_CURVE('',#11536,#11535,#1195,.T.);
#15287=EDGE_CURVE('',#11537,#11536,#134,.T.);
#15288=EDGE_CURVE('',#11538,#11537,#1196,.T.);
#15289=EDGE_CURVE('',#11539,#11538,#6010,.T.);
#15290=EDGE_CURVE('',#11540,#11539,#1197,.T.);
#15291=EDGE_CURVE('',#11541,#11540,#7123,.T.);
#15292=EDGE_CURVE('',#11542,#11541,#1198,.T.);
#15293=EDGE_CURVE('',#11543,#11542,#7124,.T.);
#15294=EDGE_CURVE('',#11544,#11543,#1199,.T.);
#15295=EDGE_CURVE('',#11545,#11544,#6011,.T.);
#15296=EDGE_CURVE('',#11546,#11545,#1200,.T.);
#15297=EDGE_CURVE('',#11546,#11547,#7125,.T.);
#15298=EDGE_CURVE('',#11503,#11547,#6012,.T.);
#15299=EDGE_CURVE('',#11547,#11502,#6013,.T.);
#15300=EDGE_CURVE('',#11548,#11546,#1201,.T.);
#15301=EDGE_CURVE('',#11549,#11548,#135,.T.);
#15302=EDGE_CURVE('',#11550,#11549,#1202,.T.);
#15303=EDGE_CURVE('',#11551,#11550,#7126,.T.);
#15304=EDGE_CURVE('',#11552,#11551,#1203,.T.);
#15305=EDGE_CURVE('',#11526,#11552,#136,.T.);
#15306=EDGE_CURVE('',#11553,#11525,#137,.T.);
#15307=EDGE_CURVE('',#11554,#11553,#1204,.T.);
#15308=EDGE_CURVE('',#11555,#11554,#7127,.T.);
#15309=EDGE_CURVE('',#11556,#11555,#1205,.T.);
#15310=EDGE_CURVE('',#11557,#11556,#138,.T.);
#15311=EDGE_CURVE('',#11505,#11557,#1206,.F.);
#15312=EDGE_CURVE('',#11558,#11559,#7128,.T.);
#15313=EDGE_CURVE('',#11559,#11558,#6014,.T.);
#15314=EDGE_CURVE('',#11560,#11560,#6015,.T.);
#15315=EDGE_CURVE('',#11560,#11561,#7129,.T.);
#15316=EDGE_CURVE('',#11562,#11561,#1207,.F.);
#15317=EDGE_CURVE('',#11563,#11562,#6016,.T.);
#15318=EDGE_CURVE('',#11564,#11563,#1208,.T.);
#15319=EDGE_CURVE('',#11565,#11564,#7130,.T.);
#15320=EDGE_CURVE('',#11566,#11565,#1209,.T.);
#15321=EDGE_CURVE('',#11567,#11566,#7131,.T.);
#15322=EDGE_CURVE('',#11568,#11567,#1210,.T.);
#15323=EDGE_CURVE('',#11569,#11568,#6017,.T.);
#15324=EDGE_CURVE('',#11570,#11569,#1211,.T.);
#15325=EDGE_CURVE('',#11571,#11570,#139,.T.);
#15326=EDGE_CURVE('',#11572,#11571,#1212,.T.);
#15327=EDGE_CURVE('',#11573,#11572,#7132,.T.);
#15328=EDGE_CURVE('',#11574,#11573,#1213,.T.);
#15329=EDGE_CURVE('',#11575,#11574,#140,.T.);
#15330=EDGE_CURVE('',#11576,#11575,#1214,.T.);
#15331=EDGE_CURVE('',#11577,#11576,#7133,.T.);
#15332=EDGE_CURVE('',#11578,#11577,#1215,.T.);
#15333=EDGE_CURVE('',#11579,#11578,#7134,.T.);
#15334=EDGE_CURVE('',#11580,#11579,#1216,.T.);
#15335=EDGE_CURVE('',#11581,#11580,#141,.T.);
#15336=EDGE_CURVE('',#11581,#11582,#7135,.T.);
#15337=EDGE_CURVE('',#11583,#11582,#142,.T.);
#15338=EDGE_CURVE('',#11584,#11583,#1217,.T.);
#15339=EDGE_CURVE('',#11585,#11584,#7136,.T.);
#15340=EDGE_CURVE('',#11586,#11585,#1218,.T.);
#15341=EDGE_CURVE('',#11587,#11586,#7137,.T.);
#15342=EDGE_CURVE('',#11588,#11587,#1219,.T.);
#15343=EDGE_CURVE('',#11589,#11588,#143,.T.);
#15344=EDGE_CURVE('',#11590,#11589,#1220,.T.);
#15345=EDGE_CURVE('',#11591,#11590,#7138,.T.);
#15346=EDGE_CURVE('',#11592,#11591,#1221,.T.);
#15347=EDGE_CURVE('',#11593,#11592,#144,.T.);
#15348=EDGE_CURVE('',#11594,#11593,#1222,.T.);
#15349=EDGE_CURVE('',#11595,#11594,#6018,.T.);
#15350=EDGE_CURVE('',#11596,#11595,#1223,.T.);
#15351=EDGE_CURVE('',#11597,#11596,#7139,.T.);
#15352=EDGE_CURVE('',#11598,#11597,#1224,.T.);
#15353=EDGE_CURVE('',#11599,#11598,#7140,.T.);
#15354=EDGE_CURVE('',#11600,#11599,#1225,.T.);
#15355=EDGE_CURVE('',#11601,#11600,#6019,.T.);
#15356=EDGE_CURVE('',#11602,#11601,#1226,.T.);
#15357=EDGE_CURVE('',#11602,#11603,#7141,.T.);
#15358=EDGE_CURVE('',#11559,#11603,#6020,.T.);
#15359=EDGE_CURVE('',#11603,#11558,#6021,.T.);
#15360=EDGE_CURVE('',#11604,#11602,#1227,.T.);
#15361=EDGE_CURVE('',#11605,#11604,#145,.T.);
#15362=EDGE_CURVE('',#11606,#11605,#1228,.T.);
#15363=EDGE_CURVE('',#11607,#11606,#7142,.T.);
#15364=EDGE_CURVE('',#11608,#11607,#1229,.T.);
#15365=EDGE_CURVE('',#11582,#11608,#146,.T.);
#15366=EDGE_CURVE('',#11609,#11581,#147,.T.);
#15367=EDGE_CURVE('',#11610,#11609,#1230,.T.);
#15368=EDGE_CURVE('',#11611,#11610,#7143,.T.);
#15369=EDGE_CURVE('',#11612,#11611,#1231,.T.);
#15370=EDGE_CURVE('',#11613,#11612,#148,.T.);
#15371=EDGE_CURVE('',#11561,#11613,#1232,.F.);
#15372=EDGE_CURVE('',#11614,#11453,#7144,.T.);
#15373=EDGE_CURVE('',#11615,#11614,#6022,.T.);
#15374=EDGE_CURVE('',#11615,#11616,#7145,.T.);
#15375=EDGE_CURVE('',#11616,#11617,#6023,.T.);
#15376=EDGE_CURVE('',#11566,#11617,#7146,.T.);
#15377=EDGE_CURVE('',#11510,#11565,#7147,.T.);
#15378=EDGE_CURVE('',#11454,#11509,#7148,.T.);
#15379=EDGE_CURVE('',#11618,#11452,#7149,.T.);
#15380=EDGE_CURVE('',#11614,#11618,#7150,.T.);
#15381=EDGE_CURVE('',#11617,#11619,#7151,.T.);
#15382=EDGE_CURVE('',#11567,#11619,#7152,.T.);
#15383=EDGE_CURVE('',#11511,#11564,#7153,.T.);
#15384=EDGE_CURVE('',#11620,#11451,#7154,.T.);
#15385=EDGE_CURVE('',#11620,#11618,#6024,.T.);
#15386=EDGE_CURVE('',#11619,#11621,#6025,.T.);
#15387=EDGE_CURVE('',#11568,#11621,#7155,.T.);
#15388=EDGE_CURVE('',#11512,#11563,#7156,.T.);
#15389=EDGE_CURVE('',#11622,#11450,#7157,.T.);
#15390=EDGE_CURVE('',#11620,#11622,#7158,.T.);
#15391=EDGE_CURVE('',#11621,#11623,#7159,.T.);
#15392=EDGE_CURVE('',#11569,#11623,#7160,.T.);
#15393=EDGE_CURVE('',#11513,#11562,#7161,.T.);
#15394=EDGE_CURVE('',#11624,#11501,#7162,.T.);
#15395=EDGE_CURVE('',#11624,#11622,#6026,.T.);
#15396=EDGE_CURVE('',#11623,#11625,#6027,.T.);
#15397=EDGE_CURVE('',#11570,#11625,#7163,.T.);
#15398=EDGE_CURVE('',#11514,#11613,#7164,.T.);
#15399=EDGE_CURVE('',#11626,#11500,#7165,.T.);
#15400=EDGE_CURVE('',#11624,#11626,#7166,.T.);
#15401=EDGE_CURVE('',#11625,#11627,#7167,.T.);
#15402=EDGE_CURVE('',#11571,#11627,#7168,.T.);
#15403=EDGE_CURVE('',#11515,#11612,#7169,.T.);
#15404=EDGE_CURVE('',#11628,#11499,#7170,.T.);
#15405=EDGE_CURVE('',#11628,#11626,#6028,.T.);
#15406=EDGE_CURVE('',#11627,#11629,#6029,.T.);
#15407=EDGE_CURVE('',#11572,#11629,#7171,.T.);
#15408=EDGE_CURVE('',#11516,#11611,#7172,.T.);
#15409=EDGE_CURVE('',#11630,#11498,#7173,.T.);
#15410=EDGE_CURVE('',#11628,#11630,#7174,.T.);
#15411=EDGE_CURVE('',#11629,#11631,#7175,.T.);
#15412=EDGE_CURVE('',#11573,#11631,#7176,.T.);
#15413=EDGE_CURVE('',#11517,#11610,#7177,.T.);
#15414=EDGE_CURVE('',#11632,#11497,#7178,.T.);
#15415=EDGE_CURVE('',#11632,#11630,#6030,.T.);
#15416=EDGE_CURVE('',#11631,#11633,#6031,.T.);
#15417=EDGE_CURVE('',#11574,#11633,#7179,.T.);
#15418=EDGE_CURVE('',#11518,#11609,#7180,.T.);
#15419=EDGE_CURVE('',#11634,#11468,#7181,.T.);
#15420=EDGE_CURVE('',#11632,#11634,#7182,.T.);
#15421=EDGE_CURVE('',#11633,#11635,#7183,.T.);
#15422=EDGE_CURVE('',#11575,#11635,#7184,.T.);
#15423=EDGE_CURVE('',#11519,#11580,#7185,.T.);
#15424=EDGE_CURVE('',#11636,#11467,#7186,.T.);
#15425=EDGE_CURVE('',#11636,#11634,#6032,.T.);
#15426=EDGE_CURVE('',#11635,#11637,#6033,.T.);
#15427=EDGE_CURVE('',#11576,#11637,#7187,.T.);
#15428=EDGE_CURVE('',#11520,#11579,#7188,.T.);
#15429=EDGE_CURVE('',#11638,#11466,#7189,.T.);
#15430=EDGE_CURVE('',#11636,#11638,#7190,.T.);
#15431=EDGE_CURVE('',#11637,#11639,#7191,.T.);
#15432=EDGE_CURVE('',#11577,#11639,#7192,.T.);
#15433=EDGE_CURVE('',#11521,#11578,#7193,.T.);
#15434=EDGE_CURVE('',#11485,#11542,#7194,.T.);
#15435=EDGE_CURVE('',#11541,#11598,#7195,.T.);
#15436=EDGE_CURVE('',#11597,#11640,#7196,.T.);
#15437=EDGE_CURVE('',#11641,#11640,#6034,.T.);
#15438=EDGE_CURVE('',#11642,#11641,#7197,.T.);
#15439=EDGE_CURVE('',#11642,#11643,#6035,.T.);
#15440=EDGE_CURVE('',#11643,#11486,#7198,.T.);
#15441=EDGE_CURVE('',#11596,#11644,#7199,.T.);
#15442=EDGE_CURVE('',#11640,#11644,#7200,.T.);
#15443=EDGE_CURVE('',#11540,#11599,#7201,.T.);
#15444=EDGE_CURVE('',#11484,#11543,#7202,.T.);
#15445=EDGE_CURVE('',#11595,#11645,#7203,.T.);
#15446=EDGE_CURVE('',#11644,#11645,#6036,.T.);
#15447=EDGE_CURVE('',#11539,#11600,#7204,.T.);
#15448=EDGE_CURVE('',#11483,#11544,#7205,.T.);
#15449=EDGE_CURVE('',#11594,#11646,#7206,.T.);
#15450=EDGE_CURVE('',#11645,#11646,#7207,.T.);
#15451=EDGE_CURVE('',#11538,#11601,#7208,.T.);
#15452=EDGE_CURVE('',#11482,#11545,#7209,.T.);
#15453=EDGE_CURVE('',#11593,#11647,#7210,.T.);
#15454=EDGE_CURVE('',#11646,#11647,#6037,.T.);
#15455=EDGE_CURVE('',#11537,#11604,#7211,.T.);
#15456=EDGE_CURVE('',#11481,#11548,#7212,.T.);
#15457=EDGE_CURVE('',#11592,#11648,#7213,.T.);
#15458=EDGE_CURVE('',#11647,#11648,#7214,.T.);
#15459=EDGE_CURVE('',#11536,#11605,#7215,.T.);
#15460=EDGE_CURVE('',#11480,#11549,#7216,.T.);
#15461=EDGE_CURVE('',#11591,#11649,#7217,.T.);
#15462=EDGE_CURVE('',#11648,#11649,#6038,.T.);
#15463=EDGE_CURVE('',#11535,#11606,#7218,.T.);
#15464=EDGE_CURVE('',#11479,#11550,#7219,.T.);
#15465=EDGE_CURVE('',#11590,#11650,#7220,.T.);
#15466=EDGE_CURVE('',#11649,#11650,#7221,.T.);
#15467=EDGE_CURVE('',#11534,#11607,#7222,.T.);
#15468=EDGE_CURVE('',#11478,#11551,#7223,.T.);
#15469=EDGE_CURVE('',#11589,#11651,#7224,.T.);
#15470=EDGE_CURVE('',#11650,#11651,#6039,.T.);
#15471=EDGE_CURVE('',#11533,#11608,#7225,.T.);
#15472=EDGE_CURVE('',#11477,#11552,#7226,.T.);
#15473=EDGE_CURVE('',#11588,#11652,#7227,.T.);
#15474=EDGE_CURVE('',#11651,#11652,#7228,.T.);
#15475=EDGE_CURVE('',#11532,#11583,#7229,.T.);
#15476=EDGE_CURVE('',#11476,#11527,#7230,.T.);
#15477=EDGE_CURVE('',#11587,#11653,#7231,.T.);
#15478=EDGE_CURVE('',#11652,#11653,#6040,.T.);
#15479=EDGE_CURVE('',#11531,#11584,#7232,.T.);
#15480=EDGE_CURVE('',#11475,#11528,#7233,.T.);
#15481=EDGE_CURVE('',#11586,#11654,#7234,.T.);
#15482=EDGE_CURVE('',#11653,#11654,#7235,.T.);
#15483=EDGE_CURVE('',#11530,#11585,#7236,.T.);
#15484=EDGE_CURVE('',#11474,#11529,#7237,.T.);
#15485=EDGE_CURVE('',#11655,#11655,#6041,.T.);
#15486=EDGE_CURVE('',#11655,#11656,#7238,.T.);
#15487=EDGE_CURVE('',#11656,#11656,#6042,.T.);
#15488=EDGE_CURVE('',#11657,#11657,#6043,.T.);
#15489=EDGE_CURVE('',#11657,#11658,#7239,.T.);
#15490=EDGE_CURVE('',#11658,#11658,#6044,.T.);
#15491=EDGE_CURVE('',#11659,#11659,#6045,.T.);
#15492=EDGE_CURVE('',#11659,#11660,#7240,.T.);
#15493=EDGE_CURVE('',#11660,#11660,#6046,.T.);
#15494=EDGE_CURVE('',#11661,#11662,#7241,.T.);
#15495=EDGE_CURVE('',#11662,#11663,#7242,.T.);
#15496=EDGE_CURVE('',#11663,#11664,#7243,.T.);
#15497=EDGE_CURVE('',#11661,#11664,#7244,.T.);
#15498=EDGE_CURVE('',#11665,#11445,#7245,.T.);
#15499=EDGE_CURVE('',#11665,#11666,#7246,.T.);
#15500=EDGE_CURVE('',#11666,#11442,#7247,.T.);
#15501=EDGE_CURVE('',#11667,#11665,#6047,.T.);
#15502=EDGE_CURVE('',#11667,#11668,#7248,.T.);
#15503=EDGE_CURVE('',#11668,#11666,#6048,.T.);
#15504=EDGE_CURVE('',#11669,#11667,#7249,.T.);
#15505=EDGE_CURVE('',#11669,#11670,#7250,.T.);
#15506=EDGE_CURVE('',#11670,#11668,#7251,.T.);
#15507=EDGE_CURVE('',#11465,#11522,#7252,.T.);
#15508=EDGE_CURVE('',#11639,#11670,#6049,.T.);
#15509=EDGE_CURVE('',#11638,#11669,#6050,.T.);
#15510=EDGE_CURVE('',#11464,#11523,#7253,.T.);
#15511=EDGE_CURVE('',#11463,#11524,#7254,.T.);
#15512=EDGE_CURVE('',#11462,#11553,#7255,.T.);
#15513=EDGE_CURVE('',#11461,#11554,#7256,.T.);
#15514=EDGE_CURVE('',#11460,#11555,#7257,.T.);
#15515=EDGE_CURVE('',#11459,#11556,#7258,.T.);
#15516=EDGE_CURVE('',#11458,#11557,#7259,.T.);
#15517=EDGE_CURVE('',#11457,#11506,#7260,.T.);
#15518=EDGE_CURVE('',#11456,#11507,#7261,.T.);
#15519=EDGE_CURVE('',#11455,#11508,#7262,.T.);
#15520=EDGE_CURVE('',#11671,#11615,#7263,.T.);
#15521=EDGE_CURVE('',#11671,#11672,#7264,.T.);
#15522=EDGE_CURVE('',#11672,#11616,#7265,.T.);
#15523=EDGE_CURVE('',#11673,#11671,#6051,.T.);
#15524=EDGE_CURVE('',#11673,#11674,#7266,.T.);
#15525=EDGE_CURVE('',#11674,#11672,#6052,.T.);
#15526=EDGE_CURVE('',#11675,#11673,#7267,.T.);
#15527=EDGE_CURVE('',#11675,#11676,#7268,.T.);
#15528=EDGE_CURVE('',#11676,#11674,#7269,.T.);
#15529=EDGE_CURVE('',#11677,#11675,#6053,.T.);
#15530=EDGE_CURVE('',#11677,#11678,#7270,.T.);
#15531=EDGE_CURVE('',#11678,#11676,#6054,.T.);
#15532=EDGE_CURVE('',#11679,#11677,#7271,.T.);
#15533=EDGE_CURVE('',#11679,#11680,#7272,.T.);
#15534=EDGE_CURVE('',#11680,#11678,#7273,.T.);
#15535=EDGE_CURVE('',#11679,#11681,#6055,.T.);
#15536=EDGE_CURVE('',#11681,#11682,#7274,.T.);
#15537=EDGE_CURVE('',#11682,#11680,#6056,.T.);
#15538=EDGE_CURVE('',#11683,#11681,#7275,.T.);
#15539=EDGE_CURVE('',#11683,#11684,#7276,.T.);
#15540=EDGE_CURVE('',#11684,#11682,#7277,.T.);
#15541=EDGE_CURVE('',#11685,#11683,#6057,.T.);
#15542=EDGE_CURVE('',#11685,#11686,#7278,.T.);
#15543=EDGE_CURVE('',#11686,#11684,#6058,.T.);
#15544=EDGE_CURVE('',#11687,#11685,#7279,.T.);
#15545=EDGE_CURVE('',#11687,#11688,#7280,.T.);
#15546=EDGE_CURVE('',#11688,#11686,#7281,.T.);
#15547=EDGE_CURVE('',#11689,#11687,#6059,.T.);
#15548=EDGE_CURVE('',#11689,#11690,#7282,.T.);
#15549=EDGE_CURVE('',#11690,#11688,#6060,.T.);
#15550=EDGE_CURVE('',#11691,#11689,#7283,.T.);
#15551=EDGE_CURVE('',#11691,#11692,#7284,.T.);
#15552=EDGE_CURVE('',#11692,#11690,#7285,.T.);
#15553=EDGE_CURVE('',#11693,#11691,#6061,.T.);
#15554=EDGE_CURVE('',#11693,#11694,#7286,.T.);
#15555=EDGE_CURVE('',#11694,#11692,#6062,.T.);
#15556=EDGE_CURVE('',#11695,#11693,#7287,.T.);
#15557=EDGE_CURVE('',#11695,#11696,#7288,.T.);
#15558=EDGE_CURVE('',#11696,#11694,#7289,.T.);
#15559=EDGE_CURVE('',#11697,#11695,#7290,.T.);
#15560=EDGE_CURVE('',#11697,#11698,#7291,.T.);
#15561=EDGE_CURVE('',#11698,#11696,#7292,.T.);
#15562=EDGE_CURVE('',#11699,#11697,#7293,.T.);
#15563=EDGE_CURVE('',#11699,#11700,#7294,.T.);
#15564=EDGE_CURVE('',#11700,#11698,#7295,.T.);
#15565=EDGE_CURVE('',#11699,#11701,#6063,.T.);
#15566=EDGE_CURVE('',#11701,#11702,#7296,.T.);
#15567=EDGE_CURVE('',#11702,#11700,#6064,.T.);
#15568=EDGE_CURVE('',#11703,#11701,#7297,.T.);
#15569=EDGE_CURVE('',#11703,#11704,#7298,.T.);
#15570=EDGE_CURVE('',#11704,#11702,#7299,.T.);
#15571=EDGE_CURVE('',#11705,#11703,#7300,.T.);
#15572=EDGE_CURVE('',#11705,#11706,#7301,.T.);
#15573=EDGE_CURVE('',#11706,#11704,#7302,.T.);
#15574=EDGE_CURVE('',#11661,#11705,#7303,.T.);
#15575=EDGE_CURVE('',#11664,#11706,#7304,.T.);
#15576=EDGE_CURVE('',#11707,#11662,#7305,.T.);
#15577=EDGE_CURVE('',#11707,#11708,#7306,.T.);
#15578=EDGE_CURVE('',#11663,#11708,#7307,.T.);
#15579=EDGE_CURVE('',#11709,#11444,#6065,.T.);
#15580=EDGE_CURVE('',#11710,#11443,#6066,.T.);
#15581=EDGE_CURVE('',#11709,#11710,#7308,.T.);
#15582=EDGE_CURVE('',#11711,#11709,#7309,.T.);
#15583=EDGE_CURVE('',#11712,#11710,#7310,.T.);
#15584=EDGE_CURVE('',#11711,#11712,#7311,.T.);
#15585=EDGE_CURVE('',#11713,#11473,#7312,.T.);
#15586=EDGE_CURVE('',#11713,#11711,#6067,.T.);
#15587=EDGE_CURVE('',#11654,#11712,#6068,.T.);
#15588=EDGE_CURVE('',#11714,#11472,#7313,.T.);
#15589=EDGE_CURVE('',#11714,#11713,#7314,.T.);
#15590=EDGE_CURVE('',#11715,#11471,#7315,.T.);
#15591=EDGE_CURVE('',#11714,#11715,#6069,.T.);
#15592=EDGE_CURVE('',#11716,#11496,#7316,.T.);
#15593=EDGE_CURVE('',#11716,#11715,#7317,.T.);
#15594=EDGE_CURVE('',#11717,#11495,#7318,.T.);
#15595=EDGE_CURVE('',#11716,#11717,#6070,.T.);
#15596=EDGE_CURVE('',#11718,#11494,#7319,.T.);
#15597=EDGE_CURVE('',#11718,#11717,#7320,.T.);
#15598=EDGE_CURVE('',#11719,#11493,#7321,.T.);
#15599=EDGE_CURVE('',#11718,#11719,#6071,.T.);
#15600=EDGE_CURVE('',#11720,#11492,#7322,.T.);
#15601=EDGE_CURVE('',#11720,#11719,#7323,.T.);
#15602=EDGE_CURVE('',#11721,#11489,#7324,.T.);
#15603=EDGE_CURVE('',#11720,#11721,#6072,.T.);
#15604=EDGE_CURVE('',#11722,#11488,#7325,.T.);
#15605=EDGE_CURVE('',#11722,#11721,#7326,.T.);
#15606=EDGE_CURVE('',#11723,#11487,#7327,.T.);
#15607=EDGE_CURVE('',#11722,#11723,#6073,.T.);
#15608=EDGE_CURVE('',#11643,#11723,#7328,.T.);
#15609=EDGE_CURVE('',#11724,#11642,#7329,.T.);
#15610=EDGE_CURVE('',#11725,#11641,#7330,.T.);
#15611=EDGE_CURVE('',#11724,#11725,#7331,.T.);
#15612=EDGE_CURVE('',#11726,#11724,#6074,.T.);
#15613=EDGE_CURVE('',#11727,#11725,#6075,.T.);
#15614=EDGE_CURVE('',#11726,#11727,#7332,.T.);
#15615=EDGE_CURVE('',#11728,#11726,#7333,.T.);
#15616=EDGE_CURVE('',#11729,#11727,#7334,.T.);
#15617=EDGE_CURVE('',#11728,#11729,#7335,.T.);
#15618=EDGE_CURVE('',#11730,#11728,#6076,.T.);
#15619=EDGE_CURVE('',#11731,#11729,#6077,.T.);
#15620=EDGE_CURVE('',#11730,#11731,#7336,.T.);
#15621=EDGE_CURVE('',#11732,#11730,#7337,.T.);
#15622=EDGE_CURVE('',#11733,#11731,#7338,.T.);
#15623=EDGE_CURVE('',#11732,#11733,#7339,.T.);
#15624=EDGE_CURVE('',#11732,#11734,#6078,.T.);
#15625=EDGE_CURVE('',#11735,#11733,#6079,.T.);
#15626=EDGE_CURVE('',#11734,#11735,#7340,.T.);
#15627=EDGE_CURVE('',#11736,#11734,#7341,.T.);
#15628=EDGE_CURVE('',#11737,#11735,#7342,.T.);
#15629=EDGE_CURVE('',#11736,#11737,#7343,.T.);
#15630=EDGE_CURVE('',#11738,#11736,#6080,.T.);
#15631=EDGE_CURVE('',#11739,#11737,#6081,.T.);
#15632=EDGE_CURVE('',#11738,#11739,#7344,.T.);
#15633=EDGE_CURVE('',#11740,#11738,#7345,.T.);
#15634=EDGE_CURVE('',#11741,#11739,#7346,.T.);
#15635=EDGE_CURVE('',#11740,#11741,#7347,.T.);
#15636=EDGE_CURVE('',#11742,#11740,#6082,.T.);
#15637=EDGE_CURVE('',#11743,#11741,#6083,.T.);
#15638=EDGE_CURVE('',#11742,#11743,#7348,.T.);
#15639=EDGE_CURVE('',#11744,#11742,#7349,.T.);
#15640=EDGE_CURVE('',#11745,#11743,#7350,.T.);
#15641=EDGE_CURVE('',#11744,#11745,#7351,.T.);
#15642=EDGE_CURVE('',#11746,#11744,#6084,.T.);
#15643=EDGE_CURVE('',#11747,#11745,#6085,.T.);
#15644=EDGE_CURVE('',#11746,#11747,#7352,.T.);
#15645=EDGE_CURVE('',#11748,#11746,#7353,.T.);
#15646=EDGE_CURVE('',#11749,#11747,#7354,.T.);
#15647=EDGE_CURVE('',#11748,#11749,#7355,.T.);
#15648=EDGE_CURVE('',#11750,#11748,#7356,.T.);
#15649=EDGE_CURVE('',#11751,#11749,#7357,.T.);
#15650=EDGE_CURVE('',#11750,#11751,#7358,.T.);
#15651=EDGE_CURVE('',#11752,#11750,#7359,.T.);
#15652=EDGE_CURVE('',#11753,#11751,#7360,.T.);
#15653=EDGE_CURVE('',#11752,#11753,#7361,.T.);
#15654=EDGE_CURVE('',#11752,#11754,#6086,.T.);
#15655=EDGE_CURVE('',#11755,#11753,#6087,.T.);
#15656=EDGE_CURVE('',#11754,#11755,#7362,.T.);
#15657=EDGE_CURVE('',#11756,#11754,#7363,.T.);
#15658=EDGE_CURVE('',#11757,#11755,#7364,.T.);
#15659=EDGE_CURVE('',#11756,#11757,#7365,.T.);
#15660=EDGE_CURVE('',#11758,#11756,#7366,.T.);
#15661=EDGE_CURVE('',#11759,#11757,#7367,.T.);
#15662=EDGE_CURVE('',#11758,#11759,#7368,.T.);
#15663=EDGE_CURVE('',#11707,#11758,#7369,.T.);
#15664=EDGE_CURVE('',#11708,#11759,#7370,.T.);
#15665=EDGE_CURVE('',#11760,#11761,#7371,.T.);
#15666=EDGE_CURVE('',#11761,#11762,#7372,.F.);
#15667=EDGE_CURVE('',#11762,#11760,#6088,.T.);
#15668=EDGE_CURVE('',#11763,#11764,#7373,.T.);
#15669=EDGE_CURVE('',#11764,#11765,#6089,.T.);
#15670=EDGE_CURVE('',#11765,#11763,#7374,.T.);
#15671=EDGE_CURVE('',#11760,#11766,#6090,.T.);
#15672=EDGE_CURVE('',#11766,#11760,#7375,.T.);
#15673=EDGE_CURVE('',#11767,#11768,#7376,.T.);
#15674=EDGE_CURVE('',#11768,#11769,#7377,.T.);
#15675=EDGE_CURVE('',#11769,#11770,#7378,.F.);
#15676=EDGE_CURVE('',#11767,#11770,#7379,.T.);
#15677=EDGE_CURVE('',#11771,#11772,#6091,.T.);
#15678=EDGE_CURVE('',#11773,#11771,#7380,.T.);
#15679=EDGE_CURVE('',#11774,#11773,#7381,.T.);
#15680=EDGE_CURVE('',#11775,#11774,#7382,.T.);
#15681=EDGE_CURVE('',#11776,#11775,#6092,.T.);
#15682=EDGE_CURVE('',#11767,#11776,#6093,.T.);
#15683=EDGE_CURVE('',#11770,#11777,#7383,.T.);
#15684=EDGE_CURVE('',#11777,#11778,#6094,.T.);
#15685=EDGE_CURVE('',#11778,#11779,#7384,.T.);
#15686=EDGE_CURVE('',#11780,#11779,#7385,.F.);
#15687=EDGE_CURVE('',#11781,#11780,#7386,.F.);
#15688=EDGE_CURVE('',#11781,#11782,#6095,.T.);
#15689=EDGE_CURVE('',#11783,#11782,#7387,.F.);
#15690=EDGE_CURVE('',#11784,#11783,#7388,.F.);
#15691=EDGE_CURVE('',#11772,#11784,#6096,.T.);
#15692=EDGE_CURVE('',#11785,#11786,#6097,.T.);
#15693=EDGE_CURVE('',#11785,#11772,#7389,.T.);
#15694=EDGE_CURVE('',#11784,#11786,#7390,.T.);
#15695=EDGE_CURVE('',#11787,#11783,#7391,.F.);
#15696=EDGE_CURVE('',#11787,#11786,#7392,.T.);
#15697=EDGE_CURVE('',#11788,#11787,#7393,.T.);
#15698=EDGE_CURVE('',#11789,#11788,#6098,.T.);
#15699=EDGE_CURVE('',#11790,#11789,#7394,.T.);
#15700=EDGE_CURVE('',#11791,#11790,#7395,.T.);
#15701=EDGE_CURVE('',#11792,#11791,#7396,.T.);
#15702=EDGE_CURVE('',#11793,#11792,#6099,.T.);
#15703=EDGE_CURVE('',#11769,#11793,#7397,.T.);
#15704=EDGE_CURVE('',#11768,#11794,#6100,.T.);
#15705=EDGE_CURVE('',#11795,#11794,#6101,.T.);
#15706=EDGE_CURVE('',#11796,#11795,#7398,.T.);
#15707=EDGE_CURVE('',#11797,#11796,#6102,.T.);
#15708=EDGE_CURVE('',#11798,#11797,#7399,.T.);
#15709=EDGE_CURVE('',#11799,#11798,#6103,.T.);
#15710=EDGE_CURVE('',#11800,#11799,#7400,.T.);
#15711=EDGE_CURVE('',#11801,#11800,#6104,.T.);
#15712=EDGE_CURVE('',#11802,#11801,#7401,.T.);
#15713=EDGE_CURVE('',#11803,#11802,#6105,.T.);
#15714=EDGE_CURVE('',#11804,#11803,#7402,.T.);
#15715=EDGE_CURVE('',#11785,#11804,#6106,.T.);
#15716=EDGE_CURVE('',#11794,#11776,#7403,.T.);
#15717=EDGE_CURVE('',#11782,#11788,#7404,.T.);
#15718=EDGE_CURVE('',#11790,#11780,#7405,.F.);
#15719=EDGE_CURVE('',#11791,#11779,#7406,.F.);
#15720=EDGE_CURVE('',#11805,#11806,#7407,.F.);
#15721=EDGE_CURVE('',#11807,#11805,#7408,.F.);
#15722=EDGE_CURVE('',#11808,#11807,#7409,.F.);
#15723=EDGE_CURVE('',#11806,#11808,#7410,.F.);
#15724=EDGE_CURVE('',#11781,#11789,#7411,.T.);
#15725=EDGE_CURVE('',#11778,#11792,#7412,.T.);
#15726=EDGE_CURVE('',#11777,#11793,#7413,.T.);
#15727=EDGE_CURVE('',#11804,#11765,#7414,.T.);
#15728=EDGE_CURVE('',#11764,#11771,#7415,.F.);
#15729=EDGE_CURVE('',#11775,#11766,#7416,.F.);
#15730=EDGE_CURVE('',#11762,#11795,#7417,.T.);
#15731=EDGE_CURVE('',#11806,#11809,#7418,.F.);
#15732=EDGE_CURVE('',#11810,#11809,#7419,.T.);
#15733=EDGE_CURVE('',#11805,#11810,#7420,.F.);
#15734=EDGE_CURVE('',#11811,#11810,#7421,.T.);
#15735=EDGE_CURVE('',#11807,#11811,#7422,.F.);
#15736=EDGE_CURVE('',#11812,#11811,#7423,.T.);
#15737=EDGE_CURVE('',#11808,#11812,#7424,.F.);
#15738=EDGE_CURVE('',#11809,#11812,#7425,.T.);
#15739=EDGE_CURVE('',#11813,#11814,#7426,.T.);
#15740=EDGE_CURVE('',#11815,#11813,#6107,.T.);
#15741=EDGE_CURVE('',#11816,#11815,#7427,.T.);
#15742=EDGE_CURVE('',#11816,#11817,#6108,.T.);
#15743=EDGE_CURVE('',#11814,#11817,#7428,.T.);
#15744=EDGE_CURVE('',#11818,#11819,#7429,.T.);
#15745=EDGE_CURVE('',#11820,#11818,#7430,.T.);
#15746=EDGE_CURVE('',#11820,#11821,#6109,.T.);
#15747=EDGE_CURVE('',#11821,#11822,#7431,.T.);
#15748=EDGE_CURVE('',#11819,#11822,#6110,.T.);
#15749=EDGE_CURVE('',#11816,#11801,#7432,.T.);
#15750=EDGE_CURVE('',#11817,#11800,#7433,.T.);
#15751=EDGE_CURVE('',#11815,#11802,#7434,.T.);
#15752=EDGE_CURVE('',#11813,#11803,#7435,.T.);
#15753=EDGE_CURVE('',#11822,#11797,#7436,.T.);
#15754=EDGE_CURVE('',#11819,#11796,#7437,.T.);
#15755=EDGE_CURVE('',#11821,#11798,#7438,.T.);
#15756=EDGE_CURVE('',#11820,#11799,#7439,.T.);
#15757=EDGE_CURVE('',#11823,#11824,#7440,.T.);
#15758=EDGE_CURVE('',#11825,#11823,#6111,.T.);
#15759=EDGE_CURVE('',#11824,#11825,#7441,.F.);
#15760=EDGE_CURVE('',#11826,#11827,#7442,.T.);
#15761=EDGE_CURVE('',#11828,#11826,#7443,.T.);
#15762=EDGE_CURVE('',#11827,#11828,#6112,.T.);
#15763=EDGE_CURVE('',#11823,#11829,#6113,.T.);
#15764=EDGE_CURVE('',#11829,#11823,#7444,.T.);
#15765=EDGE_CURVE('',#11827,#11830,#7445,.F.);
#15766=EDGE_CURVE('',#11831,#11830,#7446,.T.);
#15767=EDGE_CURVE('',#11831,#11773,#7447,.T.);
#15768=EDGE_CURVE('',#11826,#11763,#7448,.F.);
#15769=EDGE_CURVE('',#11832,#11833,#7449,.T.);
#15770=EDGE_CURVE('',#11832,#11834,#7450,.T.);
#15771=EDGE_CURVE('',#11835,#11834,#7451,.F.);
#15772=EDGE_CURVE('',#11833,#11835,#7452,.T.);
#15773=EDGE_CURVE('',#11830,#11836,#6114,.T.);
#15774=EDGE_CURVE('',#11836,#11837,#6115,.T.);
#15775=EDGE_CURVE('',#11837,#11838,#7453,.F.);
#15776=EDGE_CURVE('',#11838,#11839,#7454,.F.);
#15777=EDGE_CURVE('',#11840,#11839,#6116,.T.);
#15778=EDGE_CURVE('',#11840,#11841,#7455,.F.);
#15779=EDGE_CURVE('',#11841,#11842,#7456,.F.);
#15780=EDGE_CURVE('',#11843,#11842,#7457,.T.);
#15781=EDGE_CURVE('',#11844,#11843,#6117,.T.);
#15782=EDGE_CURVE('',#11834,#11844,#7458,.T.);
#15783=EDGE_CURVE('',#11832,#11845,#6118,.T.);
#15784=EDGE_CURVE('',#11845,#11846,#6119,.T.);
#15785=EDGE_CURVE('',#11846,#11847,#7459,.T.);
#15786=EDGE_CURVE('',#11847,#11831,#7460,.T.);
#15787=EDGE_CURVE('',#11846,#11829,#7461,.F.);
#15788=EDGE_CURVE('',#11824,#11761,#7462,.T.);
#15789=EDGE_CURVE('',#11847,#11774,#7463,.F.);
#15790=EDGE_CURVE('',#11848,#11849,#6120,.T.);
#15791=EDGE_CURVE('',#11837,#11849,#7464,.T.);
#15792=EDGE_CURVE('',#11848,#11836,#7465,.T.);
#15793=EDGE_CURVE('',#11850,#11849,#7466,.T.);
#15794=EDGE_CURVE('',#11850,#11838,#7467,.F.);
#15795=EDGE_CURVE('',#11848,#11851,#6121,.T.);
#15796=EDGE_CURVE('',#11851,#11852,#7468,.T.);
#15797=EDGE_CURVE('',#11852,#11853,#6122,.T.);
#15798=EDGE_CURVE('',#11853,#11854,#7469,.T.);
#15799=EDGE_CURVE('',#11854,#11855,#6123,.T.);
#15800=EDGE_CURVE('',#11855,#11856,#7470,.T.);
#15801=EDGE_CURVE('',#11856,#11857,#6124,.T.);
#15802=EDGE_CURVE('',#11857,#11858,#7471,.T.);
#15803=EDGE_CURVE('',#11858,#11859,#6125,.T.);
#15804=EDGE_CURVE('',#11859,#11860,#7472,.T.);
#15805=EDGE_CURVE('',#11860,#11861,#6126,.T.);
#15806=EDGE_CURVE('',#11833,#11861,#6127,.T.);
#15807=EDGE_CURVE('',#11835,#11862,#7473,.T.);
#15808=EDGE_CURVE('',#11862,#11863,#6128,.T.);
#15809=EDGE_CURVE('',#11863,#11864,#7474,.T.);
#15810=EDGE_CURVE('',#11864,#11865,#7475,.T.);
#15811=EDGE_CURVE('',#11865,#11866,#7476,.T.);
#15812=EDGE_CURVE('',#11866,#11867,#6129,.T.);
#15813=EDGE_CURVE('',#11867,#11850,#7477,.T.);
#15814=EDGE_CURVE('',#11868,#11813,#7478,.T.);
#15815=EDGE_CURVE('',#11868,#11852,#7479,.T.);
#15816=EDGE_CURVE('',#11851,#11828,#7480,.T.);
#15817=EDGE_CURVE('',#11861,#11845,#7481,.T.);
#15818=EDGE_CURVE('',#11839,#11867,#7482,.T.);
#15819=EDGE_CURVE('',#11864,#11842,#7483,.F.);
#15820=EDGE_CURVE('',#11865,#11841,#7484,.F.);
#15821=EDGE_CURVE('',#11869,#11870,#7485,.F.);
#15822=EDGE_CURVE('',#11870,#11871,#7486,.F.);
#15823=EDGE_CURVE('',#11871,#11872,#7487,.F.);
#15824=EDGE_CURVE('',#11872,#11869,#7488,.F.);
#15825=EDGE_CURVE('',#11840,#11866,#7489,.T.);
#15826=EDGE_CURVE('',#11843,#11863,#7490,.T.);
#15827=EDGE_CURVE('',#11844,#11862,#7491,.T.);
#15828=EDGE_CURVE('',#11825,#11860,#7492,.T.);
#15829=EDGE_CURVE('',#11869,#11873,#7493,.F.);
#15830=EDGE_CURVE('',#11873,#11874,#7494,.T.);
#15831=EDGE_CURVE('',#11870,#11874,#7495,.F.);
#15832=EDGE_CURVE('',#11872,#11875,#7496,.F.);
#15833=EDGE_CURVE('',#11875,#11873,#7497,.T.);
#15834=EDGE_CURVE('',#11871,#11876,#7498,.F.);
#15835=EDGE_CURVE('',#11876,#11875,#7499,.T.);
#15836=EDGE_CURVE('',#11874,#11876,#7500,.T.);
#15837=EDGE_CURVE('',#11868,#11877,#7501,.T.);
#15838=EDGE_CURVE('',#11814,#11877,#7502,.T.);
#15839=EDGE_CURVE('',#11878,#11879,#7503,.T.);
#15840=EDGE_CURVE('',#11818,#11878,#7504,.T.);
#15841=EDGE_CURVE('',#11879,#11819,#7505,.T.);
#15842=EDGE_CURVE('',#11877,#11880,#7506,.T.);
#15843=EDGE_CURVE('',#11881,#11880,#6130,.T.);
#15844=EDGE_CURVE('',#11881,#11882,#7507,.T.);
#15845=EDGE_CURVE('',#11882,#11868,#6131,.T.);
#15846=EDGE_CURVE('',#11879,#11883,#6132,.T.);
#15847=EDGE_CURVE('',#11884,#11883,#7508,.T.);
#15848=EDGE_CURVE('',#11885,#11884,#6133,.T.);
#15849=EDGE_CURVE('',#11885,#11878,#7509,.T.);
#15850=EDGE_CURVE('',#11879,#11859,#7510,.T.);
#15851=EDGE_CURVE('',#11885,#11856,#7511,.T.);
#15852=EDGE_CURVE('',#11880,#11855,#7512,.T.);
#15853=EDGE_CURVE('',#11881,#11854,#7513,.T.);
#15854=EDGE_CURVE('',#11882,#11853,#7514,.T.);
#15855=EDGE_CURVE('',#11883,#11858,#7515,.T.);
#15856=EDGE_CURVE('',#11884,#11857,#7516,.T.);
#15857=EDGE_CURVE('',#11886,#11886,#6134,.T.);
#15858=EDGE_CURVE('',#11886,#11887,#7517,.T.);
#15859=EDGE_CURVE('',#11887,#11887,#6135,.T.);
#15860=EDGE_CURVE('',#11888,#11889,#6136,.T.);
#15861=EDGE_CURVE('',#11889,#11890,#7518,.T.);
#15862=EDGE_CURVE('',#11891,#11890,#6137,.T.);
#15863=EDGE_CURVE('',#11888,#11891,#7519,.T.);
#15864=EDGE_CURVE('',#11888,#11892,#7520,.T.);
#15865=EDGE_CURVE('',#11893,#11891,#7521,.T.);
#15866=EDGE_CURVE('',#11892,#11893,#7522,.T.);
#15867=EDGE_CURVE('',#11894,#11892,#7523,.T.);
#15868=EDGE_CURVE('',#11895,#11893,#7524,.T.);
#15869=EDGE_CURVE('',#11894,#11895,#7525,.T.);
#15870=EDGE_CURVE('',#11896,#11894,#7526,.T.);
#15871=EDGE_CURVE('',#11897,#11895,#7527,.T.);
#15872=EDGE_CURVE('',#11896,#11897,#7528,.T.);
#15873=EDGE_CURVE('',#11896,#11898,#7529,.T.);
#15874=EDGE_CURVE('',#11899,#11897,#7530,.T.);
#15875=EDGE_CURVE('',#11898,#11899,#7531,.T.);
#15876=EDGE_CURVE('',#11900,#11898,#7532,.T.);
#15877=EDGE_CURVE('',#11901,#11899,#7533,.T.);
#15878=EDGE_CURVE('',#11900,#11901,#7534,.T.);
#15879=EDGE_CURVE('',#11902,#11900,#6138,.T.);
#15880=EDGE_CURVE('',#11903,#11901,#6139,.T.);
#15881=EDGE_CURVE('',#11902,#11903,#7535,.T.);
#15882=EDGE_CURVE('',#11902,#11904,#7536,.T.);
#15883=EDGE_CURVE('',#11905,#11903,#7537,.T.);
#15884=EDGE_CURVE('',#11904,#11905,#7538,.T.);
#15885=EDGE_CURVE('',#11904,#11906,#7539,.T.);
#15886=EDGE_CURVE('',#11907,#11905,#7540,.T.);
#15887=EDGE_CURVE('',#11906,#11907,#7541,.T.);
#15888=EDGE_CURVE('',#11908,#11906,#6140,.T.);
#15889=EDGE_CURVE('',#11909,#11907,#6141,.T.);
#15890=EDGE_CURVE('',#11908,#11909,#7542,.T.);
#15891=EDGE_CURVE('',#11908,#11910,#6142,.T.);
#15892=EDGE_CURVE('',#11911,#11909,#6143,.T.);
#15893=EDGE_CURVE('',#11910,#11911,#7543,.T.);
#15894=EDGE_CURVE('',#11912,#11910,#6144,.T.);
#15895=EDGE_CURVE('',#11913,#11911,#6145,.T.);
#15896=EDGE_CURVE('',#11912,#11913,#7544,.T.);
#15897=EDGE_CURVE('',#11914,#11912,#7545,.T.);
#15898=EDGE_CURVE('',#11915,#11913,#7546,.T.);
#15899=EDGE_CURVE('',#11914,#11915,#7547,.T.);
#15900=EDGE_CURVE('',#11914,#11916,#7548,.T.);
#15901=EDGE_CURVE('',#11917,#11915,#7549,.T.);
#15902=EDGE_CURVE('',#11916,#11917,#7550,.T.);
#15903=EDGE_CURVE('',#11916,#11918,#7551,.T.);
#15904=EDGE_CURVE('',#11919,#11917,#7552,.T.);
#15905=EDGE_CURVE('',#11918,#11919,#7553,.T.);
#15906=EDGE_CURVE('',#11918,#11920,#6146,.T.);
#15907=EDGE_CURVE('',#11921,#11919,#6147,.T.);
#15908=EDGE_CURVE('',#11920,#11921,#7554,.T.);
#15909=EDGE_CURVE('',#11920,#11922,#7555,.T.);
#15910=EDGE_CURVE('',#11923,#11921,#7556,.T.);
#15911=EDGE_CURVE('',#11922,#11923,#7557,.T.);
#15912=EDGE_CURVE('',#11924,#11922,#6148,.T.);
#15913=EDGE_CURVE('',#11925,#11923,#6149,.T.);
#15914=EDGE_CURVE('',#11924,#11925,#7558,.T.);
#15915=EDGE_CURVE('',#11924,#11926,#7559,.T.);
#15916=EDGE_CURVE('',#11927,#11925,#7560,.T.);
#15917=EDGE_CURVE('',#11926,#11927,#7561,.T.);
#15918=EDGE_CURVE('',#11928,#11926,#6150,.T.);
#15919=EDGE_CURVE('',#11929,#11927,#6151,.T.);
#15920=EDGE_CURVE('',#11928,#11929,#7562,.T.);
#15921=EDGE_CURVE('',#11928,#11930,#7563,.T.);
#15922=EDGE_CURVE('',#11931,#11929,#7564,.T.);
#15923=EDGE_CURVE('',#11930,#11931,#7565,.T.);
#15924=EDGE_CURVE('',#11930,#11932,#7566,.T.);
#15925=EDGE_CURVE('',#11933,#11931,#7567,.T.);
#15926=EDGE_CURVE('',#11932,#11933,#7568,.T.);
#15927=EDGE_CURVE('',#11932,#11934,#7569,.T.);
#15928=EDGE_CURVE('',#11935,#11933,#7570,.T.);
#15929=EDGE_CURVE('',#11934,#11935,#7571,.T.);
#15930=EDGE_CURVE('',#11934,#11936,#6152,.T.);
#15931=EDGE_CURVE('',#11937,#11935,#6153,.T.);
#15932=EDGE_CURVE('',#11936,#11937,#7572,.T.);
#15933=EDGE_CURVE('',#11936,#11938,#7573,.T.);
#15934=EDGE_CURVE('',#11939,#11937,#7574,.T.);
#15935=EDGE_CURVE('',#11938,#11939,#7575,.T.);
#15936=EDGE_CURVE('',#11938,#11940,#6154,.T.);
#15937=EDGE_CURVE('',#11941,#11939,#6155,.T.);
#15938=EDGE_CURVE('',#11940,#11941,#7576,.T.);
#15939=EDGE_CURVE('',#11942,#11940,#7577,.T.);
#15940=EDGE_CURVE('',#11943,#11941,#7578,.T.);
#15941=EDGE_CURVE('',#11942,#11943,#7579,.T.);
#15942=EDGE_CURVE('',#11942,#11944,#6156,.T.);
#15943=EDGE_CURVE('',#11945,#11943,#6157,.T.);
#15944=EDGE_CURVE('',#11944,#11945,#7580,.T.);
#15945=EDGE_CURVE('',#11946,#11944,#7581,.T.);
#15946=EDGE_CURVE('',#11947,#11945,#7582,.T.);
#15947=EDGE_CURVE('',#11946,#11947,#7583,.T.);
#15948=EDGE_CURVE('',#11946,#11948,#6158,.T.);
#15949=EDGE_CURVE('',#11949,#11947,#6159,.T.);
#15950=EDGE_CURVE('',#11948,#11949,#7584,.T.);
#15951=EDGE_CURVE('',#11950,#11948,#7585,.T.);
#15952=EDGE_CURVE('',#11951,#11949,#7586,.T.);
#15953=EDGE_CURVE('',#11950,#11951,#7587,.T.);
#15954=EDGE_CURVE('',#11952,#11950,#7588,.T.);
#15955=EDGE_CURVE('',#11953,#11951,#7589,.T.);
#15956=EDGE_CURVE('',#11952,#11953,#7590,.T.);
#15957=EDGE_CURVE('',#11954,#11952,#7591,.T.);
#15958=EDGE_CURVE('',#11955,#11953,#7592,.T.);
#15959=EDGE_CURVE('',#11954,#11955,#7593,.T.);
#15960=EDGE_CURVE('',#11956,#11954,#6160,.T.);
#15961=EDGE_CURVE('',#11957,#11955,#6161,.T.);
#15962=EDGE_CURVE('',#11956,#11957,#7594,.T.);
#15963=EDGE_CURVE('',#11958,#11956,#7595,.T.);
#15964=EDGE_CURVE('',#11959,#11957,#7596,.T.);
#15965=EDGE_CURVE('',#11958,#11959,#7597,.T.);
#15966=EDGE_CURVE('',#11960,#11958,#6162,.T.);
#15967=EDGE_CURVE('',#11961,#11959,#6163,.T.);
#15968=EDGE_CURVE('',#11960,#11961,#7598,.T.);
#15969=EDGE_CURVE('',#11962,#11960,#7599,.T.);
#15970=EDGE_CURVE('',#11963,#11961,#7600,.T.);
#15971=EDGE_CURVE('',#11962,#11963,#7601,.T.);
#15972=EDGE_CURVE('',#11962,#11964,#6164,.T.);
#15973=EDGE_CURVE('',#11965,#11963,#6165,.T.);
#15974=EDGE_CURVE('',#11964,#11965,#7602,.T.);
#15975=EDGE_CURVE('',#11966,#11964,#7603,.T.);
#15976=EDGE_CURVE('',#11967,#11965,#7604,.T.);
#15977=EDGE_CURVE('',#11966,#11967,#7605,.T.);
#15978=EDGE_CURVE('',#11968,#11966,#7606,.T.);
#15979=EDGE_CURVE('',#11969,#11967,#7607,.T.);
#15980=EDGE_CURVE('',#11968,#11969,#7608,.T.);
#15981=EDGE_CURVE('',#11968,#11970,#7609,.T.);
#15982=EDGE_CURVE('',#11971,#11969,#7610,.T.);
#15983=EDGE_CURVE('',#11970,#11971,#7611,.T.);
#15984=EDGE_CURVE('',#11972,#11970,#6166,.T.);
#15985=EDGE_CURVE('',#11973,#11971,#6167,.T.);
#15986=EDGE_CURVE('',#11972,#11973,#7612,.T.);
#15987=EDGE_CURVE('',#11972,#11974,#6168,.T.);
#15988=EDGE_CURVE('',#11975,#11973,#6169,.T.);
#15989=EDGE_CURVE('',#11974,#11975,#7613,.T.);
#15990=EDGE_CURVE('',#11976,#11974,#6170,.T.);
#15991=EDGE_CURVE('',#11977,#11975,#6171,.T.);
#15992=EDGE_CURVE('',#11976,#11977,#7614,.T.);
#15993=EDGE_CURVE('',#11978,#11976,#7615,.T.);
#15994=EDGE_CURVE('',#11979,#11977,#7616,.T.);
#15995=EDGE_CURVE('',#11978,#11979,#7617,.T.);
#15996=EDGE_CURVE('',#11980,#11978,#7618,.T.);
#15997=EDGE_CURVE('',#11981,#11979,#7619,.T.);
#15998=EDGE_CURVE('',#11980,#11981,#7620,.T.);
#15999=EDGE_CURVE('',#11982,#11980,#6172,.T.);
#16000=EDGE_CURVE('',#11983,#11981,#6173,.T.);
#16001=EDGE_CURVE('',#11982,#11983,#7621,.T.);
#16002=EDGE_CURVE('',#11984,#11982,#7622,.T.);
#16003=EDGE_CURVE('',#11985,#11983,#7623,.T.);
#16004=EDGE_CURVE('',#11984,#11985,#7624,.T.);
#16005=EDGE_CURVE('',#11986,#11984,#7625,.T.);
#16006=EDGE_CURVE('',#11987,#11985,#7626,.T.);
#16007=EDGE_CURVE('',#11986,#11987,#7627,.T.);
#16008=EDGE_CURVE('',#11986,#11988,#7628,.T.);
#16009=EDGE_CURVE('',#11989,#11987,#7629,.T.);
#16010=EDGE_CURVE('',#11988,#11989,#7630,.T.);
#16011=EDGE_CURVE('',#11988,#11990,#7631,.T.);
#16012=EDGE_CURVE('',#11991,#11989,#7632,.T.);
#16013=EDGE_CURVE('',#11990,#11991,#7633,.T.);
#16014=EDGE_CURVE('',#11990,#11992,#7634,.T.);
#16015=EDGE_CURVE('',#11993,#11991,#7635,.T.);
#16016=EDGE_CURVE('',#11992,#11993,#7636,.T.);
#16017=EDGE_CURVE('',#11994,#11992,#6174,.T.);
#16018=EDGE_CURVE('',#11995,#11993,#6175,.T.);
#16019=EDGE_CURVE('',#11994,#11995,#7637,.T.);
#16020=EDGE_CURVE('',#11994,#11996,#7638,.T.);
#16021=EDGE_CURVE('',#11997,#11995,#7639,.T.);
#16022=EDGE_CURVE('',#11996,#11997,#7640,.T.);
#16023=EDGE_CURVE('',#11996,#11998,#7641,.T.);
#16024=EDGE_CURVE('',#11999,#11997,#7642,.T.);
#16025=EDGE_CURVE('',#11998,#11999,#7643,.T.);
#16026=EDGE_CURVE('',#12000,#11998,#6176,.T.);
#16027=EDGE_CURVE('',#12001,#11999,#6177,.T.);
#16028=EDGE_CURVE('',#12000,#12001,#7644,.T.);
#16029=EDGE_CURVE('',#12000,#12002,#6178,.T.);
#16030=EDGE_CURVE('',#12003,#12001,#6179,.T.);
#16031=EDGE_CURVE('',#12002,#12003,#7645,.T.);
#16032=EDGE_CURVE('',#12004,#12002,#6180,.T.);
#16033=EDGE_CURVE('',#12005,#12003,#6181,.T.);
#16034=EDGE_CURVE('',#12004,#12005,#7646,.T.);
#16035=EDGE_CURVE('',#12006,#12004,#7647,.T.);
#16036=EDGE_CURVE('',#12007,#12005,#7648,.T.);
#16037=EDGE_CURVE('',#12006,#12007,#7649,.T.);
#16038=EDGE_CURVE('',#12006,#12008,#7650,.T.);
#16039=EDGE_CURVE('',#12009,#12007,#7651,.T.);
#16040=EDGE_CURVE('',#12008,#12009,#7652,.T.);
#16041=EDGE_CURVE('',#12008,#12010,#7653,.T.);
#16042=EDGE_CURVE('',#12011,#12009,#7654,.T.);
#16043=EDGE_CURVE('',#12010,#12011,#7655,.T.);
#16044=EDGE_CURVE('',#12010,#12012,#6182,.T.);
#16045=EDGE_CURVE('',#12013,#12011,#6183,.T.);
#16046=EDGE_CURVE('',#12012,#12013,#7656,.T.);
#16047=EDGE_CURVE('',#12012,#12014,#7657,.T.);
#16048=EDGE_CURVE('',#12015,#12013,#7658,.T.);
#16049=EDGE_CURVE('',#12014,#12015,#7659,.T.);
#16050=EDGE_CURVE('',#12016,#12014,#6184,.T.);
#16051=EDGE_CURVE('',#12017,#12015,#6185,.T.);
#16052=EDGE_CURVE('',#12016,#12017,#7660,.T.);
#16053=EDGE_CURVE('',#12016,#12018,#7661,.T.);
#16054=EDGE_CURVE('',#12019,#12017,#7662,.T.);
#16055=EDGE_CURVE('',#12018,#12019,#7663,.T.);
#16056=EDGE_CURVE('',#12020,#12018,#6186,.T.);
#16057=EDGE_CURVE('',#12021,#12019,#6187,.T.);
#16058=EDGE_CURVE('',#12020,#12021,#7664,.T.);
#16059=EDGE_CURVE('',#12020,#12022,#7665,.T.);
#16060=EDGE_CURVE('',#12023,#12021,#7666,.T.);
#16061=EDGE_CURVE('',#12022,#12023,#7667,.T.);
#16062=EDGE_CURVE('',#12022,#12024,#7668,.T.);
#16063=EDGE_CURVE('',#12025,#12023,#7669,.T.);
#16064=EDGE_CURVE('',#12024,#12025,#7670,.T.);
#16065=EDGE_CURVE('',#12024,#12026,#7671,.T.);
#16066=EDGE_CURVE('',#12027,#12025,#7672,.T.);
#16067=EDGE_CURVE('',#12026,#12027,#7673,.T.);
#16068=EDGE_CURVE('',#12026,#12028,#6188,.T.);
#16069=EDGE_CURVE('',#12029,#12027,#6189,.T.);
#16070=EDGE_CURVE('',#12028,#12029,#7674,.T.);
#16071=EDGE_CURVE('',#12028,#12030,#7675,.T.);
#16072=EDGE_CURVE('',#12031,#12029,#7676,.T.);
#16073=EDGE_CURVE('',#12030,#12031,#7677,.T.);
#16074=EDGE_CURVE('',#12030,#12032,#6190,.T.);
#16075=EDGE_CURVE('',#12033,#12031,#6191,.T.);
#16076=EDGE_CURVE('',#12032,#12033,#7678,.T.);
#16077=EDGE_CURVE('',#12032,#12034,#7679,.T.);
#16078=EDGE_CURVE('',#12035,#12033,#7680,.T.);
#16079=EDGE_CURVE('',#12034,#12035,#7681,.T.);
#16080=EDGE_CURVE('',#12034,#12036,#6192,.T.);
#16081=EDGE_CURVE('',#12037,#12035,#6193,.T.);
#16082=EDGE_CURVE('',#12036,#12037,#7682,.T.);
#16083=EDGE_CURVE('',#12038,#12036,#7683,.T.);
#16084=EDGE_CURVE('',#12039,#12037,#7684,.T.);
#16085=EDGE_CURVE('',#12038,#12039,#7685,.T.);
#16086=EDGE_CURVE('',#12038,#12040,#6194,.T.);
#16087=EDGE_CURVE('',#12041,#12039,#6195,.T.);
#16088=EDGE_CURVE('',#12040,#12041,#7686,.T.);
#16089=EDGE_CURVE('',#12042,#12040,#7687,.T.);
#16090=EDGE_CURVE('',#12043,#12041,#7688,.T.);
#16091=EDGE_CURVE('',#12042,#12043,#7689,.T.);
#16092=EDGE_CURVE('',#12044,#12042,#7690,.T.);
#16093=EDGE_CURVE('',#12045,#12043,#7691,.T.);
#16094=EDGE_CURVE('',#12044,#12045,#7692,.T.);
#16095=EDGE_CURVE('',#12046,#12044,#7693,.T.);
#16096=EDGE_CURVE('',#12047,#12045,#7694,.T.);
#16097=EDGE_CURVE('',#12046,#12047,#7695,.T.);
#16098=EDGE_CURVE('',#12048,#12046,#6196,.T.);
#16099=EDGE_CURVE('',#12049,#12047,#6197,.T.);
#16100=EDGE_CURVE('',#12048,#12049,#7696,.T.);
#16101=EDGE_CURVE('',#12050,#12048,#7697,.T.);
#16102=EDGE_CURVE('',#12051,#12049,#7698,.T.);
#16103=EDGE_CURVE('',#12050,#12051,#7699,.T.);
#16104=EDGE_CURVE('',#12052,#12050,#6198,.T.);
#16105=EDGE_CURVE('',#12053,#12051,#6199,.T.);
#16106=EDGE_CURVE('',#12052,#12053,#7700,.T.);
#16107=EDGE_CURVE('',#12054,#12052,#7701,.T.);
#16108=EDGE_CURVE('',#12055,#12053,#7702,.T.);
#16109=EDGE_CURVE('',#12054,#12055,#7703,.T.);
#16110=EDGE_CURVE('',#12054,#12056,#6200,.T.);
#16111=EDGE_CURVE('',#12057,#12055,#6201,.T.);
#16112=EDGE_CURVE('',#12056,#12057,#7704,.T.);
#16113=EDGE_CURVE('',#12058,#12056,#7705,.T.);
#16114=EDGE_CURVE('',#12059,#12057,#7706,.T.);
#16115=EDGE_CURVE('',#12058,#12059,#7707,.T.);
#16116=EDGE_CURVE('',#12060,#12058,#7708,.T.);
#16117=EDGE_CURVE('',#12061,#12059,#7709,.T.);
#16118=EDGE_CURVE('',#12060,#12061,#7710,.T.);
#16119=EDGE_CURVE('',#12060,#12062,#7711,.T.);
#16120=EDGE_CURVE('',#12063,#12061,#7712,.T.);
#16121=EDGE_CURVE('',#12062,#12063,#7713,.T.);
#16122=EDGE_CURVE('',#12064,#12062,#6202,.T.);
#16123=EDGE_CURVE('',#12065,#12063,#6203,.T.);
#16124=EDGE_CURVE('',#12064,#12065,#7714,.T.);
#16125=EDGE_CURVE('',#12064,#12066,#6204,.T.);
#16126=EDGE_CURVE('',#12067,#12065,#6205,.T.);
#16127=EDGE_CURVE('',#12066,#12067,#7715,.T.);
#16128=EDGE_CURVE('',#12068,#12066,#6206,.T.);
#16129=EDGE_CURVE('',#12069,#12067,#6207,.T.);
#16130=EDGE_CURVE('',#12068,#12069,#7716,.T.);
#16131=EDGE_CURVE('',#12070,#12068,#7717,.T.);
#16132=EDGE_CURVE('',#12071,#12069,#7718,.T.);
#16133=EDGE_CURVE('',#12070,#12071,#7719,.T.);
#16134=EDGE_CURVE('',#11889,#12070,#7720,.T.);
#16135=EDGE_CURVE('',#11890,#12071,#7721,.T.);
#16136=EDGE_CURVE('',#12072,#12073,#7722,.T.);
#16137=EDGE_CURVE('',#12074,#12072,#1233,.T.);
#16138=EDGE_CURVE('',#12074,#12075,#6208,.T.);
#16139=EDGE_CURVE('',#12075,#12073,#1234,.T.);
#16140=EDGE_CURVE('',#12076,#12077,#7723,.T.);
#16141=EDGE_CURVE('',#12078,#12076,#1235,.T.);
#16142=EDGE_CURVE('',#12072,#12078,#1236,.T.);
#16143=EDGE_CURVE('',#12073,#12079,#1237,.T.);
#16144=EDGE_CURVE('',#12079,#12077,#1238,.T.);
#16145=EDGE_CURVE('',#12080,#12081,#7724,.T.);
#16146=EDGE_CURVE('',#12082,#12080,#1239,.T.);
#16147=EDGE_CURVE('',#12076,#12082,#1240,.T.);
#16148=EDGE_CURVE('',#12077,#12083,#1241,.T.);
#16149=EDGE_CURVE('',#12083,#12081,#1242,.T.);
#16150=EDGE_CURVE('',#12084,#12085,#7725,.T.);
#16151=EDGE_CURVE('',#12086,#12084,#1243,.T.);
#16152=EDGE_CURVE('',#12080,#12086,#1244,.T.);
#16153=EDGE_CURVE('',#12081,#12087,#1245,.T.);
#16154=EDGE_CURVE('',#12087,#12085,#1246,.T.);
#16155=EDGE_CURVE('',#12088,#12089,#7726,.T.);
#16156=EDGE_CURVE('',#12090,#12088,#1247,.T.);
#16157=EDGE_CURVE('',#12090,#12091,#6209,.T.);
#16158=EDGE_CURVE('',#12091,#12089,#1248,.T.);
#16159=EDGE_CURVE('',#12092,#12093,#7727,.T.);
#16160=EDGE_CURVE('',#12094,#12092,#1249,.T.);
#16161=EDGE_CURVE('',#12088,#12094,#1250,.T.);
#16162=EDGE_CURVE('',#12089,#12095,#1251,.T.);
#16163=EDGE_CURVE('',#12095,#12093,#1252,.T.);
#16164=EDGE_CURVE('',#12096,#12097,#7728,.T.);
#16165=EDGE_CURVE('',#12098,#12096,#1253,.T.);
#16166=EDGE_CURVE('',#12092,#12098,#1254,.T.);
#16167=EDGE_CURVE('',#12093,#12099,#1255,.T.);
#16168=EDGE_CURVE('',#12099,#12097,#1256,.T.);
#16169=EDGE_CURVE('',#12100,#12101,#7729,.T.);
#16170=EDGE_CURVE('',#12102,#12100,#1257,.T.);
#16171=EDGE_CURVE('',#12096,#12102,#1258,.T.);
#16172=EDGE_CURVE('',#12097,#12103,#1259,.T.);
#16173=EDGE_CURVE('',#12103,#12101,#1260,.T.);
#16174=EDGE_CURVE('',#12104,#12105,#7730,.T.);
#16175=EDGE_CURVE('',#12106,#12104,#1261,.T.);
#16176=EDGE_CURVE('',#12107,#12106,#1262,.T.);
#16177=EDGE_CURVE('',#12107,#12108,#6210,.T.);
#16178=EDGE_CURVE('',#12108,#12109,#1263,.T.);
#16179=EDGE_CURVE('',#12109,#12105,#1264,.T.);
#16180=EDGE_CURVE('',#12110,#12111,#7731,.T.);
#16181=EDGE_CURVE('',#12112,#12110,#1265,.T.);
#16182=EDGE_CURVE('',#12104,#12112,#1266,.T.);
#16183=EDGE_CURVE('',#12105,#12113,#1267,.T.);
#16184=EDGE_CURVE('',#12113,#12111,#1268,.T.);
#16185=EDGE_CURVE('',#12114,#12115,#7732,.T.);
#16186=EDGE_CURVE('',#12116,#12114,#1269,.T.);
#16187=EDGE_CURVE('',#12110,#12116,#1270,.T.);
#16188=EDGE_CURVE('',#12111,#12117,#1271,.T.);
#16189=EDGE_CURVE('',#12117,#12115,#1272,.T.);
#16190=EDGE_CURVE('',#12118,#12119,#7733,.T.);
#16191=EDGE_CURVE('',#12120,#12118,#1273,.T.);
#16192=EDGE_CURVE('',#12114,#12120,#1274,.T.);
#16193=EDGE_CURVE('',#12115,#12121,#1275,.T.);
#16194=EDGE_CURVE('',#12121,#12119,#1276,.T.);
#16195=EDGE_CURVE('',#12122,#12123,#7734,.T.);
#16196=EDGE_CURVE('',#12124,#12122,#1277,.T.);
#16197=EDGE_CURVE('',#12118,#12124,#1278,.T.);
#16198=EDGE_CURVE('',#12119,#12125,#1279,.T.);
#16199=EDGE_CURVE('',#12125,#12123,#1280,.T.);
#16200=EDGE_CURVE('',#12126,#12127,#7735,.T.);
#16201=EDGE_CURVE('',#12128,#12126,#1281,.T.);
#16202=EDGE_CURVE('',#12122,#12128,#1282,.T.);
#16203=EDGE_CURVE('',#12123,#12129,#1283,.T.);
#16204=EDGE_CURVE('',#12129,#12127,#1284,.T.);
#16205=EDGE_CURVE('',#12130,#12131,#7736,.T.);
#16206=EDGE_CURVE('',#12132,#12130,#1285,.T.);
#16207=EDGE_CURVE('',#12126,#12132,#1286,.T.);
#16208=EDGE_CURVE('',#12127,#12133,#1287,.T.);
#16209=EDGE_CURVE('',#12133,#12131,#1288,.T.);
#16210=EDGE_CURVE('',#12134,#12135,#7737,.T.);
#16211=EDGE_CURVE('',#12136,#12134,#1289,.T.);
#16212=EDGE_CURVE('',#12130,#12136,#1290,.T.);
#16213=EDGE_CURVE('',#12131,#12137,#1291,.T.);
#16214=EDGE_CURVE('',#12137,#12135,#1292,.T.);
#16215=EDGE_CURVE('',#12138,#12139,#7738,.T.);
#16216=EDGE_CURVE('',#12140,#12138,#1293,.T.);
#16217=EDGE_CURVE('',#12134,#12140,#1294,.T.);
#16218=EDGE_CURVE('',#12135,#12141,#1295,.T.);
#16219=EDGE_CURVE('',#12141,#12139,#1296,.T.);
#16220=EDGE_CURVE('',#12142,#12143,#7739,.T.);
#16221=EDGE_CURVE('',#12144,#12142,#1297,.T.);
#16222=EDGE_CURVE('',#12138,#12144,#1298,.T.);
#16223=EDGE_CURVE('',#12139,#12145,#1299,.T.);
#16224=EDGE_CURVE('',#12145,#12143,#1300,.T.);
#16225=EDGE_CURVE('',#12146,#12147,#7740,.T.);
#16226=EDGE_CURVE('',#12148,#12146,#1301,.T.);
#16227=EDGE_CURVE('',#12142,#12148,#1302,.T.);
#16228=EDGE_CURVE('',#12143,#12149,#1303,.T.);
#16229=EDGE_CURVE('',#12149,#12147,#1304,.T.);
#16230=EDGE_CURVE('',#12150,#12151,#7741,.T.);
#16231=EDGE_CURVE('',#12152,#12150,#1305,.T.);
#16232=EDGE_CURVE('',#12146,#12152,#1306,.T.);
#16233=EDGE_CURVE('',#12147,#12153,#1307,.T.);
#16234=EDGE_CURVE('',#12153,#12151,#1308,.T.);
#16235=EDGE_CURVE('',#12154,#12155,#7742,.T.);
#16236=EDGE_CURVE('',#12156,#12154,#1309,.T.);
#16237=EDGE_CURVE('',#12150,#12156,#1310,.T.);
#16238=EDGE_CURVE('',#12151,#12157,#1311,.T.);
#16239=EDGE_CURVE('',#12157,#12155,#1312,.T.);
#16240=EDGE_CURVE('',#12158,#12159,#7743,.T.);
#16241=EDGE_CURVE('',#12160,#12158,#1313,.T.);
#16242=EDGE_CURVE('',#12154,#12160,#1314,.T.);
#16243=EDGE_CURVE('',#12155,#12161,#1315,.T.);
#16244=EDGE_CURVE('',#12161,#12159,#1316,.T.);
#16245=EDGE_CURVE('',#12162,#12163,#7744,.T.);
#16246=EDGE_CURVE('',#12164,#12162,#1317,.T.);
#16247=EDGE_CURVE('',#12158,#12164,#1318,.T.);
#16248=EDGE_CURVE('',#12159,#12165,#1319,.T.);
#16249=EDGE_CURVE('',#12165,#12163,#1320,.T.);
#16250=EDGE_CURVE('',#12166,#12167,#7745,.T.);
#16251=EDGE_CURVE('',#12168,#12166,#1321,.T.);
#16252=EDGE_CURVE('',#12162,#12168,#1322,.T.);
#16253=EDGE_CURVE('',#12163,#12169,#1323,.T.);
#16254=EDGE_CURVE('',#12169,#12167,#1324,.T.);
#16255=EDGE_CURVE('',#12170,#12171,#7746,.T.);
#16256=EDGE_CURVE('',#12172,#12170,#1325,.T.);
#16257=EDGE_CURVE('',#12166,#12172,#1326,.T.);
#16258=EDGE_CURVE('',#12167,#12173,#1327,.T.);
#16259=EDGE_CURVE('',#12173,#12171,#1328,.T.);
#16260=EDGE_CURVE('',#12174,#12175,#7747,.T.);
#16261=EDGE_CURVE('',#12176,#12174,#1329,.T.);
#16262=EDGE_CURVE('',#12170,#12176,#1330,.T.);
#16263=EDGE_CURVE('',#12171,#12177,#1331,.T.);
#16264=EDGE_CURVE('',#12177,#12175,#1332,.T.);
#16265=EDGE_CURVE('',#12178,#12179,#7748,.T.);
#16266=EDGE_CURVE('',#12180,#12178,#1333,.T.);
#16267=EDGE_CURVE('',#12174,#12180,#1334,.T.);
#16268=EDGE_CURVE('',#12175,#12181,#1335,.T.);
#16269=EDGE_CURVE('',#12181,#12179,#1336,.T.);
#16270=EDGE_CURVE('',#12182,#12183,#7749,.T.);
#16271=EDGE_CURVE('',#12184,#12182,#1337,.T.);
#16272=EDGE_CURVE('',#12178,#12184,#1338,.T.);
#16273=EDGE_CURVE('',#12179,#12185,#1339,.T.);
#16274=EDGE_CURVE('',#12185,#12183,#1340,.T.);
#16275=EDGE_CURVE('',#12186,#12187,#7750,.T.);
#16276=EDGE_CURVE('',#12188,#12186,#1341,.T.);
#16277=EDGE_CURVE('',#12182,#12188,#1342,.T.);
#16278=EDGE_CURVE('',#12183,#12189,#1343,.T.);
#16279=EDGE_CURVE('',#12189,#12187,#1344,.T.);
#16280=EDGE_CURVE('',#12190,#12191,#7751,.T.);
#16281=EDGE_CURVE('',#12192,#12190,#1345,.T.);
#16282=EDGE_CURVE('',#12186,#12192,#1346,.T.);
#16283=EDGE_CURVE('',#12187,#12193,#1347,.T.);
#16284=EDGE_CURVE('',#12193,#12191,#1348,.T.);
#16285=EDGE_CURVE('',#12194,#12195,#7752,.T.);
#16286=EDGE_CURVE('',#12196,#12194,#1349,.T.);
#16287=EDGE_CURVE('',#12190,#12196,#1350,.T.);
#16288=EDGE_CURVE('',#12191,#12197,#1351,.T.);
#16289=EDGE_CURVE('',#12197,#12195,#1352,.T.);
#16290=EDGE_CURVE('',#12198,#12199,#7753,.T.);
#16291=EDGE_CURVE('',#12200,#12198,#1353,.T.);
#16292=EDGE_CURVE('',#12194,#12200,#1354,.T.);
#16293=EDGE_CURVE('',#12195,#12201,#1355,.T.);
#16294=EDGE_CURVE('',#12201,#12199,#1356,.T.);
#16295=EDGE_CURVE('',#12202,#12203,#7754,.T.);
#16296=EDGE_CURVE('',#12204,#12202,#1357,.T.);
#16297=EDGE_CURVE('',#12198,#12204,#1358,.T.);
#16298=EDGE_CURVE('',#12199,#12205,#1359,.T.);
#16299=EDGE_CURVE('',#12205,#12203,#1360,.T.);
#16300=EDGE_CURVE('',#12206,#12207,#7755,.T.);
#16301=EDGE_CURVE('',#12208,#12206,#1361,.T.);
#16302=EDGE_CURVE('',#12202,#12208,#1362,.T.);
#16303=EDGE_CURVE('',#12203,#12209,#1363,.T.);
#16304=EDGE_CURVE('',#12209,#12207,#1364,.T.);
#16305=EDGE_CURVE('',#12210,#12211,#7756,.T.);
#16306=EDGE_CURVE('',#12212,#12210,#1365,.T.);
#16307=EDGE_CURVE('',#12206,#12212,#1366,.T.);
#16308=EDGE_CURVE('',#12207,#12213,#1367,.T.);
#16309=EDGE_CURVE('',#12213,#12211,#1368,.T.);
#16310=EDGE_CURVE('',#12214,#12215,#7757,.T.);
#16311=EDGE_CURVE('',#12216,#12214,#1369,.T.);
#16312=EDGE_CURVE('',#12217,#12216,#1370,.T.);
#16313=EDGE_CURVE('',#12217,#12218,#6211,.T.);
#16314=EDGE_CURVE('',#12218,#12219,#1371,.T.);
#16315=EDGE_CURVE('',#12219,#12215,#1372,.T.);
#16316=EDGE_CURVE('',#12220,#12221,#7758,.T.);
#16317=EDGE_CURVE('',#12222,#12220,#1373,.T.);
#16318=EDGE_CURVE('',#12214,#12222,#1374,.T.);
#16319=EDGE_CURVE('',#12215,#12223,#1375,.T.);
#16320=EDGE_CURVE('',#12223,#12221,#1376,.T.);
#16321=EDGE_CURVE('',#12224,#12225,#7759,.T.);
#16322=EDGE_CURVE('',#12226,#12224,#1377,.T.);
#16323=EDGE_CURVE('',#12220,#12226,#1378,.T.);
#16324=EDGE_CURVE('',#12221,#12227,#1379,.T.);
#16325=EDGE_CURVE('',#12227,#12225,#1380,.T.);
#16326=EDGE_CURVE('',#12228,#12229,#7760,.T.);
#16327=EDGE_CURVE('',#12230,#12228,#1381,.T.);
#16328=EDGE_CURVE('',#12224,#12230,#1382,.T.);
#16329=EDGE_CURVE('',#12225,#12231,#1383,.T.);
#16330=EDGE_CURVE('',#12231,#12229,#1384,.T.);
#16331=EDGE_CURVE('',#12232,#12233,#7761,.T.);
#16332=EDGE_CURVE('',#12234,#12232,#1385,.T.);
#16333=EDGE_CURVE('',#12228,#12234,#1386,.T.);
#16334=EDGE_CURVE('',#12229,#12235,#1387,.T.);
#16335=EDGE_CURVE('',#12235,#12233,#1388,.T.);
#16336=EDGE_CURVE('',#12236,#12237,#7762,.T.);
#16337=EDGE_CURVE('',#12238,#12236,#1389,.T.);
#16338=EDGE_CURVE('',#12232,#12238,#1390,.T.);
#16339=EDGE_CURVE('',#12233,#12239,#1391,.T.);
#16340=EDGE_CURVE('',#12239,#12237,#1392,.T.);
#16341=EDGE_CURVE('',#12240,#12241,#7763,.T.);
#16342=EDGE_CURVE('',#12242,#12240,#1393,.T.);
#16343=EDGE_CURVE('',#12236,#12242,#1394,.T.);
#16344=EDGE_CURVE('',#12237,#12243,#1395,.T.);
#16345=EDGE_CURVE('',#12243,#12241,#1396,.T.);
#16346=EDGE_CURVE('',#12244,#12245,#7764,.T.);
#16347=EDGE_CURVE('',#12246,#12244,#1397,.T.);
#16348=EDGE_CURVE('',#12240,#12246,#1398,.T.);
#16349=EDGE_CURVE('',#12241,#12247,#1399,.T.);
#16350=EDGE_CURVE('',#12247,#12245,#1400,.T.);
#16351=EDGE_CURVE('',#12248,#12249,#7765,.T.);
#16352=EDGE_CURVE('',#12250,#12248,#1401,.T.);
#16353=EDGE_CURVE('',#12244,#12250,#1402,.T.);
#16354=EDGE_CURVE('',#12245,#12251,#1403,.T.);
#16355=EDGE_CURVE('',#12251,#12249,#1404,.T.);
#16356=EDGE_CURVE('',#12252,#12253,#7766,.T.);
#16357=EDGE_CURVE('',#12254,#12252,#1405,.T.);
#16358=EDGE_CURVE('',#12248,#12254,#1406,.T.);
#16359=EDGE_CURVE('',#12249,#12255,#1407,.T.);
#16360=EDGE_CURVE('',#12255,#12253,#1408,.T.);
#16361=EDGE_CURVE('',#12256,#12257,#7767,.T.);
#16362=EDGE_CURVE('',#12258,#12256,#1409,.T.);
#16363=EDGE_CURVE('',#12252,#12258,#1410,.T.);
#16364=EDGE_CURVE('',#12253,#12259,#1411,.T.);
#16365=EDGE_CURVE('',#12259,#12257,#1412,.T.);
#16366=EDGE_CURVE('',#12260,#12261,#7768,.T.);
#16367=EDGE_CURVE('',#12262,#12260,#1413,.T.);
#16368=EDGE_CURVE('',#12256,#12262,#1414,.T.);
#16369=EDGE_CURVE('',#12257,#12263,#1415,.T.);
#16370=EDGE_CURVE('',#12263,#12261,#1416,.T.);
#16371=EDGE_CURVE('',#12264,#12265,#7769,.T.);
#16372=EDGE_CURVE('',#12266,#12264,#1417,.T.);
#16373=EDGE_CURVE('',#12260,#12266,#1418,.T.);
#16374=EDGE_CURVE('',#12261,#12267,#1419,.T.);
#16375=EDGE_CURVE('',#12267,#12265,#1420,.T.);
#16376=EDGE_CURVE('',#12268,#12269,#7770,.T.);
#16377=EDGE_CURVE('',#12270,#12268,#1421,.T.);
#16378=EDGE_CURVE('',#12264,#12270,#1422,.T.);
#16379=EDGE_CURVE('',#12265,#12271,#1423,.T.);
#16380=EDGE_CURVE('',#12271,#12269,#1424,.T.);
#16381=EDGE_CURVE('',#12272,#12273,#7771,.T.);
#16382=EDGE_CURVE('',#12274,#12272,#1425,.T.);
#16383=EDGE_CURVE('',#12268,#12274,#1426,.T.);
#16384=EDGE_CURVE('',#12269,#12275,#1427,.T.);
#16385=EDGE_CURVE('',#12275,#12273,#1428,.T.);
#16386=EDGE_CURVE('',#12276,#12277,#7772,.T.);
#16387=EDGE_CURVE('',#12278,#12276,#1429,.T.);
#16388=EDGE_CURVE('',#12272,#12278,#1430,.T.);
#16389=EDGE_CURVE('',#12273,#12279,#1431,.T.);
#16390=EDGE_CURVE('',#12279,#12277,#1432,.T.);
#16391=EDGE_CURVE('',#12280,#12281,#7773,.T.);
#16392=EDGE_CURVE('',#12282,#12280,#1433,.T.);
#16393=EDGE_CURVE('',#12276,#12282,#1434,.T.);
#16394=EDGE_CURVE('',#12277,#12283,#1435,.T.);
#16395=EDGE_CURVE('',#12283,#12281,#1436,.T.);
#16396=EDGE_CURVE('',#12284,#12285,#7774,.T.);
#16397=EDGE_CURVE('',#12286,#12284,#1437,.T.);
#16398=EDGE_CURVE('',#12280,#12286,#1438,.T.);
#16399=EDGE_CURVE('',#12281,#12287,#1439,.T.);
#16400=EDGE_CURVE('',#12287,#12285,#1440,.T.);
#16401=EDGE_CURVE('',#12288,#12289,#7775,.T.);
#16402=EDGE_CURVE('',#12290,#12288,#1441,.T.);
#16403=EDGE_CURVE('',#12284,#12290,#1442,.T.);
#16404=EDGE_CURVE('',#12285,#12291,#1443,.T.);
#16405=EDGE_CURVE('',#12291,#12289,#1444,.T.);
#16406=EDGE_CURVE('',#12292,#12293,#7776,.T.);
#16407=EDGE_CURVE('',#12294,#12292,#1445,.T.);
#16408=EDGE_CURVE('',#12288,#12294,#1446,.T.);
#16409=EDGE_CURVE('',#12289,#12295,#1447,.T.);
#16410=EDGE_CURVE('',#12295,#12293,#1448,.T.);
#16411=EDGE_CURVE('',#12296,#12297,#7777,.T.);
#16412=EDGE_CURVE('',#12298,#12296,#1449,.T.);
#16413=EDGE_CURVE('',#12292,#12298,#1450,.T.);
#16414=EDGE_CURVE('',#12293,#12299,#1451,.T.);
#16415=EDGE_CURVE('',#12299,#12297,#1452,.T.);
#16416=EDGE_CURVE('',#12300,#12301,#7778,.T.);
#16417=EDGE_CURVE('',#12302,#12300,#1453,.T.);
#16418=EDGE_CURVE('',#12296,#12302,#1454,.T.);
#16419=EDGE_CURVE('',#12297,#12303,#1455,.T.);
#16420=EDGE_CURVE('',#12303,#12301,#1456,.T.);
#16421=EDGE_CURVE('',#12304,#12305,#7779,.T.);
#16422=EDGE_CURVE('',#12306,#12304,#1457,.T.);
#16423=EDGE_CURVE('',#12300,#12306,#1458,.T.);
#16424=EDGE_CURVE('',#12301,#12307,#1459,.T.);
#16425=EDGE_CURVE('',#12307,#12305,#1460,.T.);
#16426=EDGE_CURVE('',#12308,#12309,#7780,.T.);
#16427=EDGE_CURVE('',#12310,#12308,#1461,.T.);
#16428=EDGE_CURVE('',#12304,#12310,#1462,.T.);
#16429=EDGE_CURVE('',#12305,#12311,#1463,.T.);
#16430=EDGE_CURVE('',#12311,#12309,#1464,.T.);
#16431=EDGE_CURVE('',#12312,#12313,#7781,.T.);
#16432=EDGE_CURVE('',#12314,#12312,#1465,.T.);
#16433=EDGE_CURVE('',#12308,#12314,#1466,.T.);
#16434=EDGE_CURVE('',#12309,#12315,#1467,.T.);
#16435=EDGE_CURVE('',#12315,#12313,#1468,.T.);
#16436=EDGE_CURVE('',#12316,#12317,#7782,.T.);
#16437=EDGE_CURVE('',#12318,#12316,#1469,.T.);
#16438=EDGE_CURVE('',#12312,#12318,#1470,.T.);
#16439=EDGE_CURVE('',#12313,#12319,#1471,.T.);
#16440=EDGE_CURVE('',#12319,#12317,#1472,.T.);
#16441=EDGE_CURVE('',#12320,#12321,#7783,.T.);
#16442=EDGE_CURVE('',#12322,#12320,#1473,.T.);
#16443=EDGE_CURVE('',#12316,#12322,#1474,.T.);
#16444=EDGE_CURVE('',#12317,#12323,#1475,.T.);
#16445=EDGE_CURVE('',#12323,#12321,#1476,.T.);
#16446=EDGE_CURVE('',#12324,#12325,#7784,.T.);
#16447=EDGE_CURVE('',#12326,#12324,#1477,.T.);
#16448=EDGE_CURVE('',#12327,#12326,#1478,.T.);
#16449=EDGE_CURVE('',#12327,#12328,#6212,.T.);
#16450=EDGE_CURVE('',#12328,#12329,#1479,.T.);
#16451=EDGE_CURVE('',#12329,#12325,#1480,.T.);
#16452=EDGE_CURVE('',#12330,#12331,#7785,.T.);
#16453=EDGE_CURVE('',#12332,#12330,#1481,.T.);
#16454=EDGE_CURVE('',#12324,#12332,#1482,.T.);
#16455=EDGE_CURVE('',#12325,#12333,#1483,.T.);
#16456=EDGE_CURVE('',#12333,#12331,#1484,.T.);
#16457=EDGE_CURVE('',#12334,#12335,#7786,.T.);
#16458=EDGE_CURVE('',#12336,#12334,#1485,.T.);
#16459=EDGE_CURVE('',#12330,#12336,#1486,.T.);
#16460=EDGE_CURVE('',#12331,#12337,#1487,.T.);
#16461=EDGE_CURVE('',#12337,#12335,#1488,.T.);
#16462=EDGE_CURVE('',#12338,#12339,#7787,.T.);
#16463=EDGE_CURVE('',#12340,#12338,#1489,.T.);
#16464=EDGE_CURVE('',#12334,#12340,#1490,.T.);
#16465=EDGE_CURVE('',#12335,#12341,#1491,.T.);
#16466=EDGE_CURVE('',#12341,#12339,#1492,.T.);
#16467=EDGE_CURVE('',#12342,#12343,#7788,.T.);
#16468=EDGE_CURVE('',#12344,#12342,#1493,.T.);
#16469=EDGE_CURVE('',#12338,#12344,#1494,.T.);
#16470=EDGE_CURVE('',#12339,#12345,#1495,.T.);
#16471=EDGE_CURVE('',#12345,#12343,#1496,.T.);
#16472=EDGE_CURVE('',#12346,#12347,#7789,.T.);
#16473=EDGE_CURVE('',#12348,#12346,#1497,.T.);
#16474=EDGE_CURVE('',#12342,#12348,#1498,.T.);
#16475=EDGE_CURVE('',#12343,#12349,#1499,.T.);
#16476=EDGE_CURVE('',#12349,#12347,#1500,.T.);
#16477=EDGE_CURVE('',#12350,#12351,#7790,.T.);
#16478=EDGE_CURVE('',#12352,#12350,#1501,.T.);
#16479=EDGE_CURVE('',#12346,#12352,#1502,.T.);
#16480=EDGE_CURVE('',#12347,#12353,#1503,.T.);
#16481=EDGE_CURVE('',#12353,#12351,#1504,.T.);
#16482=EDGE_CURVE('',#12354,#12355,#7791,.T.);
#16483=EDGE_CURVE('',#12356,#12354,#1505,.T.);
#16484=EDGE_CURVE('',#12350,#12356,#1506,.T.);
#16485=EDGE_CURVE('',#12351,#12357,#1507,.T.);
#16486=EDGE_CURVE('',#12357,#12355,#1508,.T.);
#16487=EDGE_CURVE('',#12358,#12359,#7792,.T.);
#16488=EDGE_CURVE('',#12360,#12358,#1509,.T.);
#16489=EDGE_CURVE('',#12354,#12360,#1510,.T.);
#16490=EDGE_CURVE('',#12355,#12361,#1511,.T.);
#16491=EDGE_CURVE('',#12361,#12359,#1512,.T.);
#16492=EDGE_CURVE('',#12362,#12363,#7793,.T.);
#16493=EDGE_CURVE('',#12364,#12362,#1513,.T.);
#16494=EDGE_CURVE('',#12358,#12364,#1514,.T.);
#16495=EDGE_CURVE('',#12359,#12365,#1515,.T.);
#16496=EDGE_CURVE('',#12365,#12363,#1516,.T.);
#16497=EDGE_CURVE('',#12366,#12367,#7794,.T.);
#16498=EDGE_CURVE('',#12368,#12366,#1517,.T.);
#16499=EDGE_CURVE('',#12362,#12368,#1518,.T.);
#16500=EDGE_CURVE('',#12363,#12369,#1519,.T.);
#16501=EDGE_CURVE('',#12369,#12367,#1520,.T.);
#16502=EDGE_CURVE('',#12370,#12371,#7795,.T.);
#16503=EDGE_CURVE('',#12372,#12370,#1521,.T.);
#16504=EDGE_CURVE('',#12366,#12372,#1522,.T.);
#16505=EDGE_CURVE('',#12367,#12373,#1523,.T.);
#16506=EDGE_CURVE('',#12373,#12371,#1524,.T.);
#16507=EDGE_CURVE('',#12374,#12375,#7796,.T.);
#16508=EDGE_CURVE('',#12376,#12374,#1525,.T.);
#16509=EDGE_CURVE('',#12370,#12376,#1526,.T.);
#16510=EDGE_CURVE('',#12371,#12377,#1527,.T.);
#16511=EDGE_CURVE('',#12377,#12375,#1528,.T.);
#16512=EDGE_CURVE('',#12378,#12379,#7797,.T.);
#16513=EDGE_CURVE('',#12380,#12378,#1529,.T.);
#16514=EDGE_CURVE('',#12374,#12380,#1530,.T.);
#16515=EDGE_CURVE('',#12375,#12381,#1531,.T.);
#16516=EDGE_CURVE('',#12381,#12379,#1532,.T.);
#16517=EDGE_CURVE('',#12382,#12383,#7798,.T.);
#16518=EDGE_CURVE('',#12384,#12382,#1533,.T.);
#16519=EDGE_CURVE('',#12378,#12384,#1534,.T.);
#16520=EDGE_CURVE('',#12379,#12385,#1535,.T.);
#16521=EDGE_CURVE('',#12385,#12383,#1536,.T.);
#16522=EDGE_CURVE('',#12386,#12387,#7799,.T.);
#16523=EDGE_CURVE('',#12388,#12386,#1537,.T.);
#16524=EDGE_CURVE('',#12382,#12388,#1538,.T.);
#16525=EDGE_CURVE('',#12383,#12389,#1539,.T.);
#16526=EDGE_CURVE('',#12389,#12387,#1540,.T.);
#16527=EDGE_CURVE('',#12390,#12391,#7800,.T.);
#16528=EDGE_CURVE('',#12392,#12390,#1541,.T.);
#16529=EDGE_CURVE('',#12386,#12392,#1542,.T.);
#16530=EDGE_CURVE('',#12387,#12393,#1543,.T.);
#16531=EDGE_CURVE('',#12393,#12391,#1544,.T.);
#16532=EDGE_CURVE('',#12394,#12395,#7801,.T.);
#16533=EDGE_CURVE('',#12396,#12394,#1545,.T.);
#16534=EDGE_CURVE('',#12390,#12396,#1546,.T.);
#16535=EDGE_CURVE('',#12391,#12397,#1547,.T.);
#16536=EDGE_CURVE('',#12397,#12395,#1548,.T.);
#16537=EDGE_CURVE('',#12398,#12399,#7802,.T.);
#16538=EDGE_CURVE('',#12400,#12398,#1549,.T.);
#16539=EDGE_CURVE('',#12394,#12400,#1550,.T.);
#16540=EDGE_CURVE('',#12395,#12401,#1551,.T.);
#16541=EDGE_CURVE('',#12401,#12399,#1552,.T.);
#16542=EDGE_CURVE('',#12402,#12403,#7803,.T.);
#16543=EDGE_CURVE('',#12404,#12402,#1553,.T.);
#16544=EDGE_CURVE('',#12398,#12404,#1554,.T.);
#16545=EDGE_CURVE('',#12399,#12405,#1555,.T.);
#16546=EDGE_CURVE('',#12405,#12403,#1556,.T.);
#16547=EDGE_CURVE('',#12406,#12407,#7804,.T.);
#16548=EDGE_CURVE('',#12408,#12406,#1557,.T.);
#16549=EDGE_CURVE('',#12402,#12408,#1558,.T.);
#16550=EDGE_CURVE('',#12403,#12409,#1559,.T.);
#16551=EDGE_CURVE('',#12409,#12407,#1560,.T.);
#16552=EDGE_CURVE('',#12410,#12411,#7805,.T.);
#16553=EDGE_CURVE('',#12412,#12410,#1561,.T.);
#16554=EDGE_CURVE('',#12406,#12412,#1562,.T.);
#16555=EDGE_CURVE('',#12407,#12413,#1563,.T.);
#16556=EDGE_CURVE('',#12413,#12411,#1564,.T.);
#16557=EDGE_CURVE('',#12414,#12415,#7806,.T.);
#16558=EDGE_CURVE('',#12416,#12414,#1565,.T.);
#16559=EDGE_CURVE('',#12410,#12416,#1566,.T.);
#16560=EDGE_CURVE('',#12411,#12417,#1567,.T.);
#16561=EDGE_CURVE('',#12417,#12415,#1568,.T.);
#16562=EDGE_CURVE('',#12418,#12419,#7807,.T.);
#16563=EDGE_CURVE('',#12420,#12418,#1569,.T.);
#16564=EDGE_CURVE('',#12414,#12420,#1570,.T.);
#16565=EDGE_CURVE('',#12415,#12421,#1571,.T.);
#16566=EDGE_CURVE('',#12421,#12419,#1572,.T.);
#16567=EDGE_CURVE('',#12422,#12423,#7808,.T.);
#16568=EDGE_CURVE('',#12424,#12422,#1573,.T.);
#16569=EDGE_CURVE('',#12418,#12424,#1574,.T.);
#16570=EDGE_CURVE('',#12419,#12425,#1575,.T.);
#16571=EDGE_CURVE('',#12425,#12423,#1576,.T.);
#16572=EDGE_CURVE('',#12426,#12427,#7809,.T.);
#16573=EDGE_CURVE('',#12428,#12426,#1577,.T.);
#16574=EDGE_CURVE('',#12422,#12428,#1578,.T.);
#16575=EDGE_CURVE('',#12423,#12429,#1579,.T.);
#16576=EDGE_CURVE('',#12429,#12427,#1580,.T.);
#16577=EDGE_CURVE('',#12430,#12431,#7810,.T.);
#16578=EDGE_CURVE('',#12432,#12430,#1581,.T.);
#16579=EDGE_CURVE('',#12426,#12432,#1582,.T.);
#16580=EDGE_CURVE('',#12427,#12433,#1583,.T.);
#16581=EDGE_CURVE('',#12433,#12431,#1584,.T.);
#16582=EDGE_CURVE('',#12434,#12435,#7811,.T.);
#16583=EDGE_CURVE('',#12436,#12434,#1585,.T.);
#16584=EDGE_CURVE('',#12437,#12436,#1586,.T.);
#16585=EDGE_CURVE('',#12437,#12438,#6213,.T.);
#16586=EDGE_CURVE('',#12438,#12439,#1587,.T.);
#16587=EDGE_CURVE('',#12439,#12435,#1588,.T.);
#16588=EDGE_CURVE('',#12440,#12441,#7812,.T.);
#16589=EDGE_CURVE('',#12442,#12440,#1589,.T.);
#16590=EDGE_CURVE('',#12434,#12442,#1590,.T.);
#16591=EDGE_CURVE('',#12435,#12443,#1591,.T.);
#16592=EDGE_CURVE('',#12443,#12441,#1592,.T.);
#16593=EDGE_CURVE('',#12444,#12445,#7813,.T.);
#16594=EDGE_CURVE('',#12446,#12444,#1593,.T.);
#16595=EDGE_CURVE('',#12440,#12446,#1594,.T.);
#16596=EDGE_CURVE('',#12441,#12447,#1595,.T.);
#16597=EDGE_CURVE('',#12447,#12445,#1596,.T.);
#16598=EDGE_CURVE('',#12448,#12449,#7814,.T.);
#16599=EDGE_CURVE('',#12450,#12448,#1597,.T.);
#16600=EDGE_CURVE('',#12444,#12450,#1598,.T.);
#16601=EDGE_CURVE('',#12445,#12451,#1599,.T.);
#16602=EDGE_CURVE('',#12451,#12449,#1600,.T.);
#16603=EDGE_CURVE('',#12452,#12453,#7815,.T.);
#16604=EDGE_CURVE('',#12454,#12452,#1601,.T.);
#16605=EDGE_CURVE('',#12448,#12454,#1602,.T.);
#16606=EDGE_CURVE('',#12449,#12455,#1603,.T.);
#16607=EDGE_CURVE('',#12455,#12453,#1604,.T.);
#16608=EDGE_CURVE('',#12456,#12457,#7816,.T.);
#16609=EDGE_CURVE('',#12458,#12456,#1605,.T.);
#16610=EDGE_CURVE('',#12452,#12458,#1606,.T.);
#16611=EDGE_CURVE('',#12453,#12459,#1607,.T.);
#16612=EDGE_CURVE('',#12459,#12457,#1608,.T.);
#16613=EDGE_CURVE('',#12460,#12461,#7817,.T.);
#16614=EDGE_CURVE('',#12462,#12460,#1609,.T.);
#16615=EDGE_CURVE('',#12456,#12462,#1610,.T.);
#16616=EDGE_CURVE('',#12457,#12463,#1611,.T.);
#16617=EDGE_CURVE('',#12463,#12461,#1612,.T.);
#16618=EDGE_CURVE('',#12464,#12465,#7818,.T.);
#16619=EDGE_CURVE('',#12466,#12464,#1613,.T.);
#16620=EDGE_CURVE('',#12460,#12466,#1614,.T.);
#16621=EDGE_CURVE('',#12461,#12467,#1615,.T.);
#16622=EDGE_CURVE('',#12467,#12465,#1616,.T.);
#16623=EDGE_CURVE('',#12468,#12469,#7819,.T.);
#16624=EDGE_CURVE('',#12470,#12468,#1617,.T.);
#16625=EDGE_CURVE('',#12464,#12470,#1618,.T.);
#16626=EDGE_CURVE('',#12465,#12471,#1619,.T.);
#16627=EDGE_CURVE('',#12471,#12469,#1620,.T.);
#16628=EDGE_CURVE('',#12472,#12473,#7820,.T.);
#16629=EDGE_CURVE('',#12474,#12472,#1621,.T.);
#16630=EDGE_CURVE('',#12468,#12474,#1622,.T.);
#16631=EDGE_CURVE('',#12469,#12475,#1623,.T.);
#16632=EDGE_CURVE('',#12475,#12473,#1624,.T.);
#16633=EDGE_CURVE('',#12476,#12477,#7821,.T.);
#16634=EDGE_CURVE('',#12478,#12476,#1625,.T.);
#16635=EDGE_CURVE('',#12472,#12478,#1626,.T.);
#16636=EDGE_CURVE('',#12473,#12479,#1627,.T.);
#16637=EDGE_CURVE('',#12479,#12477,#1628,.T.);
#16638=EDGE_CURVE('',#12480,#12481,#7822,.T.);
#16639=EDGE_CURVE('',#12482,#12480,#1629,.T.);
#16640=EDGE_CURVE('',#12476,#12482,#1630,.T.);
#16641=EDGE_CURVE('',#12477,#12483,#1631,.T.);
#16642=EDGE_CURVE('',#12483,#12481,#1632,.T.);
#16643=EDGE_CURVE('',#12484,#12485,#7823,.T.);
#16644=EDGE_CURVE('',#12486,#12484,#1633,.T.);
#16645=EDGE_CURVE('',#12480,#12486,#1634,.T.);
#16646=EDGE_CURVE('',#12481,#12487,#1635,.T.);
#16647=EDGE_CURVE('',#12487,#12485,#1636,.T.);
#16648=EDGE_CURVE('',#12488,#12489,#7824,.T.);
#16649=EDGE_CURVE('',#12490,#12488,#1637,.T.);
#16650=EDGE_CURVE('',#12484,#12490,#1638,.T.);
#16651=EDGE_CURVE('',#12485,#12491,#1639,.T.);
#16652=EDGE_CURVE('',#12491,#12489,#1640,.T.);
#16653=EDGE_CURVE('',#12492,#12493,#7825,.T.);
#16654=EDGE_CURVE('',#12494,#12492,#1641,.T.);
#16655=EDGE_CURVE('',#12488,#12494,#1642,.T.);
#16656=EDGE_CURVE('',#12489,#12495,#1643,.T.);
#16657=EDGE_CURVE('',#12495,#12493,#1644,.T.);
#16658=EDGE_CURVE('',#12496,#12497,#7826,.T.);
#16659=EDGE_CURVE('',#12498,#12496,#1645,.T.);
#16660=EDGE_CURVE('',#12492,#12498,#1646,.T.);
#16661=EDGE_CURVE('',#12493,#12499,#1647,.T.);
#16662=EDGE_CURVE('',#12499,#12497,#1648,.T.);
#16663=EDGE_CURVE('',#12500,#12501,#7827,.T.);
#16664=EDGE_CURVE('',#12502,#12500,#1649,.T.);
#16665=EDGE_CURVE('',#12496,#12502,#1650,.T.);
#16666=EDGE_CURVE('',#12497,#12503,#1651,.T.);
#16667=EDGE_CURVE('',#12503,#12501,#1652,.T.);
#16668=EDGE_CURVE('',#12504,#12505,#7828,.T.);
#16669=EDGE_CURVE('',#12506,#12504,#1653,.T.);
#16670=EDGE_CURVE('',#12500,#12506,#1654,.T.);
#16671=EDGE_CURVE('',#12501,#12507,#1655,.T.);
#16672=EDGE_CURVE('',#12507,#12505,#1656,.T.);
#16673=EDGE_CURVE('',#12508,#12509,#7829,.T.);
#16674=EDGE_CURVE('',#12510,#12508,#1657,.T.);
#16675=EDGE_CURVE('',#12504,#12510,#1658,.T.);
#16676=EDGE_CURVE('',#12505,#12511,#1659,.T.);
#16677=EDGE_CURVE('',#12511,#12509,#1660,.T.);
#16678=EDGE_CURVE('',#12512,#12513,#7830,.T.);
#16679=EDGE_CURVE('',#12514,#12512,#1661,.T.);
#16680=EDGE_CURVE('',#12508,#12514,#1662,.T.);
#16681=EDGE_CURVE('',#12509,#12515,#1663,.T.);
#16682=EDGE_CURVE('',#12515,#12513,#1664,.T.);
#16683=EDGE_CURVE('',#12516,#12517,#7831,.T.);
#16684=EDGE_CURVE('',#12518,#12516,#1665,.T.);
#16685=EDGE_CURVE('',#12512,#12518,#1666,.T.);
#16686=EDGE_CURVE('',#12513,#12519,#1667,.T.);
#16687=EDGE_CURVE('',#12519,#12517,#1668,.T.);
#16688=EDGE_CURVE('',#12520,#12521,#7832,.T.);
#16689=EDGE_CURVE('',#12522,#12520,#1669,.T.);
#16690=EDGE_CURVE('',#12516,#12522,#1670,.T.);
#16691=EDGE_CURVE('',#12517,#12523,#1671,.T.);
#16692=EDGE_CURVE('',#12523,#12521,#1672,.T.);
#16693=EDGE_CURVE('',#12524,#12525,#7833,.T.);
#16694=EDGE_CURVE('',#12526,#12524,#1673,.T.);
#16695=EDGE_CURVE('',#12520,#12526,#1674,.T.);
#16696=EDGE_CURVE('',#12521,#12527,#1675,.T.);
#16697=EDGE_CURVE('',#12527,#12525,#1676,.T.);
#16698=EDGE_CURVE('',#12528,#12529,#7834,.T.);
#16699=EDGE_CURVE('',#12530,#12528,#1677,.T.);
#16700=EDGE_CURVE('',#12524,#12530,#1678,.T.);
#16701=EDGE_CURVE('',#12525,#12531,#1679,.T.);
#16702=EDGE_CURVE('',#12531,#12529,#1680,.T.);
#16703=EDGE_CURVE('',#12532,#12533,#7835,.T.);
#16704=EDGE_CURVE('',#12534,#12532,#1681,.T.);
#16705=EDGE_CURVE('',#12528,#12534,#1682,.T.);
#16706=EDGE_CURVE('',#12529,#12535,#1683,.T.);
#16707=EDGE_CURVE('',#12535,#12533,#1684,.T.);
#16708=EDGE_CURVE('',#12536,#12537,#7836,.T.);
#16709=EDGE_CURVE('',#12538,#12536,#1685,.T.);
#16710=EDGE_CURVE('',#12532,#12538,#1686,.T.);
#16711=EDGE_CURVE('',#12533,#12539,#1687,.T.);
#16712=EDGE_CURVE('',#12539,#12537,#1688,.T.);
#16713=EDGE_CURVE('',#12540,#12541,#7837,.T.);
#16714=EDGE_CURVE('',#12542,#12540,#1689,.T.);
#16715=EDGE_CURVE('',#12536,#12542,#1690,.T.);
#16716=EDGE_CURVE('',#12537,#12543,#1691,.T.);
#16717=EDGE_CURVE('',#12543,#12541,#1692,.T.);
#16718=EDGE_CURVE('',#12544,#12545,#7838,.T.);
#16719=EDGE_CURVE('',#12546,#12544,#1693,.T.);
#16720=EDGE_CURVE('',#12546,#12545,#6214,.F.);
#16721=EDGE_CURVE('',#12547,#12548,#7839,.T.);
#16722=EDGE_CURVE('',#12544,#12547,#1694,.T.);
#16723=EDGE_CURVE('',#12545,#12549,#6215,.F.);
#16724=EDGE_CURVE('',#12548,#12549,#1695,.F.);
#16725=EDGE_CURVE('',#12550,#12551,#7840,.T.);
#16726=EDGE_CURVE('',#12547,#12550,#1696,.T.);
#16727=EDGE_CURVE('',#12551,#12548,#1697,.F.);
#16728=EDGE_CURVE('',#12552,#12553,#7841,.T.);
#16729=EDGE_CURVE('',#12550,#12552,#1698,.F.);
#16730=EDGE_CURVE('',#12553,#12551,#1699,.T.);
#16731=EDGE_CURVE('',#12554,#12555,#7842,.T.);
#16732=EDGE_CURVE('',#12556,#12554,#1700,.T.);
#16733=EDGE_CURVE('',#12557,#12556,#6216,.F.);
#16734=EDGE_CURVE('',#12555,#12557,#1701,.F.);
#16735=EDGE_CURVE('',#12558,#12559,#7843,.T.);
#16736=EDGE_CURVE('',#12554,#12558,#1702,.T.);
#16737=EDGE_CURVE('',#12559,#12555,#1703,.F.);
#16738=EDGE_CURVE('',#12560,#12561,#7844,.T.);
#16739=EDGE_CURVE('',#12558,#12560,#1704,.F.);
#16740=EDGE_CURVE('',#12561,#12559,#1705,.T.);
#16741=EDGE_CURVE('',#12562,#12563,#7845,.T.);
#16742=EDGE_CURVE('',#12564,#12562,#6217,.T.);
#16743=EDGE_CURVE('',#12560,#12564,#1706,.F.);
#16744=EDGE_CURVE('',#12563,#12561,#1707,.T.);
#16745=EDGE_CURVE('',#12565,#12566,#7846,.T.);
#16746=EDGE_CURVE('',#12567,#12565,#1708,.T.);
#16747=EDGE_CURVE('',#12568,#12567,#1709,.T.);
#16748=EDGE_CURVE('',#12568,#12569,#6218,.F.);
#16749=EDGE_CURVE('',#12570,#12569,#1710,.T.);
#16750=EDGE_CURVE('',#12566,#12570,#1711,.F.);
#16751=EDGE_CURVE('',#12571,#12572,#7847,.T.);
#16752=EDGE_CURVE('',#12573,#12571,#1712,.F.);
#16753=EDGE_CURVE('',#12565,#12573,#1713,.T.);
#16754=EDGE_CURVE('',#12572,#12566,#1714,.F.);
#16755=EDGE_CURVE('',#12574,#12575,#7848,.T.);
#16756=EDGE_CURVE('',#12571,#12574,#1715,.F.);
#16757=EDGE_CURVE('',#12576,#12572,#1716,.F.);
#16758=EDGE_CURVE('',#12575,#12576,#1717,.T.);
#16759=EDGE_CURVE('',#12577,#12578,#7849,.T.);
#16760=EDGE_CURVE('',#12579,#12577,#1718,.F.);
#16761=EDGE_CURVE('',#12574,#12579,#1719,.F.);
#16762=EDGE_CURVE('',#12580,#12575,#1720,.T.);
#16763=EDGE_CURVE('',#12578,#12580,#1721,.F.);
#16764=EDGE_CURVE('',#12581,#12582,#7850,.T.);
#16765=EDGE_CURVE('',#12577,#12581,#1722,.F.);
#16766=EDGE_CURVE('',#12582,#12578,#1723,.F.);
#16767=EDGE_CURVE('',#12583,#12584,#7851,.T.);
#16768=EDGE_CURVE('',#12585,#12583,#1724,.F.);
#16769=EDGE_CURVE('',#12581,#12585,#1725,.F.);
#16770=EDGE_CURVE('',#12586,#12582,#1726,.F.);
#16771=EDGE_CURVE('',#12584,#12586,#1727,.F.);
#16772=EDGE_CURVE('',#12587,#12588,#7852,.T.);
#16773=EDGE_CURVE('',#12583,#12587,#1728,.F.);
#16774=EDGE_CURVE('',#12588,#12584,#1729,.F.);
#16775=EDGE_CURVE('',#12589,#12590,#7853,.T.);
#16776=EDGE_CURVE('',#12591,#12589,#1730,.F.);
#16777=EDGE_CURVE('',#12587,#12591,#1731,.F.);
#16778=EDGE_CURVE('',#12592,#12588,#1732,.F.);
#16779=EDGE_CURVE('',#12590,#12592,#1733,.T.);
#16780=EDGE_CURVE('',#12593,#12594,#7854,.T.);
#16781=EDGE_CURVE('',#12589,#12593,#1734,.F.);
#16782=EDGE_CURVE('',#12595,#12590,#1735,.T.);
#16783=EDGE_CURVE('',#12594,#12595,#1736,.T.);
#16784=EDGE_CURVE('',#12596,#12597,#7855,.T.);
#16785=EDGE_CURVE('',#12598,#12596,#1737,.F.);
#16786=EDGE_CURVE('',#12593,#12598,#1738,.F.);
#16787=EDGE_CURVE('',#12599,#12594,#1739,.T.);
#16788=EDGE_CURVE('',#12597,#12599,#1740,.F.);
#16789=EDGE_CURVE('',#12600,#12601,#7856,.T.);
#16790=EDGE_CURVE('',#12596,#12600,#1741,.F.);
#16791=EDGE_CURVE('',#12601,#12597,#1742,.F.);
#16792=EDGE_CURVE('',#12602,#12603,#7857,.T.);
#16793=EDGE_CURVE('',#12604,#12602,#1743,.T.);
#16794=EDGE_CURVE('',#12600,#12604,#1744,.F.);
#16795=EDGE_CURVE('',#12605,#12601,#1745,.F.);
#16796=EDGE_CURVE('',#12603,#12605,#1746,.F.);
#16797=EDGE_CURVE('',#12606,#12607,#7858,.T.);
#16798=EDGE_CURVE('',#12608,#12606,#1747,.T.);
#16799=EDGE_CURVE('',#12602,#12608,#1748,.T.);
#16800=EDGE_CURVE('',#12607,#12603,#1749,.F.);
#16801=EDGE_CURVE('',#12609,#12610,#7859,.T.);
#16802=EDGE_CURVE('',#12611,#12609,#1750,.F.);
#16803=EDGE_CURVE('',#12606,#12611,#1751,.T.);
#16804=EDGE_CURVE('',#12612,#12607,#1752,.F.);
#16805=EDGE_CURVE('',#12610,#12612,#1753,.T.);
#16806=EDGE_CURVE('',#12613,#12614,#7860,.T.);
#16807=EDGE_CURVE('',#12609,#12613,#1754,.F.);
#16808=EDGE_CURVE('',#12615,#12610,#1755,.T.);
#16809=EDGE_CURVE('',#12614,#12615,#1756,.T.);
#16810=EDGE_CURVE('',#12616,#12617,#7861,.T.);
#16811=EDGE_CURVE('',#12618,#12616,#1757,.F.);
#16812=EDGE_CURVE('',#12613,#12618,#1758,.F.);
#16813=EDGE_CURVE('',#12619,#12614,#1759,.T.);
#16814=EDGE_CURVE('',#12617,#12619,#1760,.F.);
#16815=EDGE_CURVE('',#12620,#12621,#7862,.T.);
#16816=EDGE_CURVE('',#12616,#12620,#1761,.F.);
#16817=EDGE_CURVE('',#12621,#12617,#1762,.F.);
#16818=EDGE_CURVE('',#12622,#12623,#7863,.T.);
#16819=EDGE_CURVE('',#12624,#12622,#1763,.T.);
#16820=EDGE_CURVE('',#12620,#12624,#1764,.F.);
#16821=EDGE_CURVE('',#12625,#12621,#1765,.F.);
#16822=EDGE_CURVE('',#12623,#12625,#1766,.F.);
#16823=EDGE_CURVE('',#12626,#12627,#7864,.T.);
#16824=EDGE_CURVE('',#12628,#12626,#1767,.T.);
#16825=EDGE_CURVE('',#12622,#12628,#1768,.T.);
#16826=EDGE_CURVE('',#12627,#12623,#1769,.F.);
#16827=EDGE_CURVE('',#12629,#12630,#7865,.T.);
#16828=EDGE_CURVE('',#12631,#12629,#1770,.F.);
#16829=EDGE_CURVE('',#12626,#12631,#1771,.T.);
#16830=EDGE_CURVE('',#12632,#12627,#1772,.F.);
#16831=EDGE_CURVE('',#12630,#12632,#1773,.F.);
#16832=EDGE_CURVE('',#12633,#12634,#7866,.T.);
#16833=EDGE_CURVE('',#12629,#12633,#1774,.F.);
#16834=EDGE_CURVE('',#12634,#12630,#1775,.F.);
#16835=EDGE_CURVE('',#12635,#12636,#7867,.T.);
#16836=EDGE_CURVE('',#12637,#12635,#1776,.F.);
#16837=EDGE_CURVE('',#12633,#12637,#1777,.F.);
#16838=EDGE_CURVE('',#12638,#12634,#1778,.F.);
#16839=EDGE_CURVE('',#12636,#12638,#1779,.F.);
#16840=EDGE_CURVE('',#12639,#12640,#7868,.T.);
#16841=EDGE_CURVE('',#12635,#12639,#1780,.F.);
#16842=EDGE_CURVE('',#12640,#12636,#1781,.F.);
#16843=EDGE_CURVE('',#12641,#12642,#7869,.T.);
#16844=EDGE_CURVE('',#12643,#12641,#1782,.T.);
#16845=EDGE_CURVE('',#12639,#12643,#1783,.F.);
#16846=EDGE_CURVE('',#12644,#12640,#1784,.F.);
#16847=EDGE_CURVE('',#12642,#12644,#1785,.F.);
#16848=EDGE_CURVE('',#12645,#12646,#7870,.T.);
#16849=EDGE_CURVE('',#12647,#12645,#1786,.F.);
#16850=EDGE_CURVE('',#12641,#12647,#1787,.T.);
#16851=EDGE_CURVE('',#12646,#12642,#1788,.F.);
#16852=EDGE_CURVE('',#12648,#12649,#7871,.T.);
#16853=EDGE_CURVE('',#12645,#12648,#1789,.F.);
#16854=EDGE_CURVE('',#12650,#12646,#1790,.F.);
#16855=EDGE_CURVE('',#12649,#12650,#1791,.T.);
#16856=EDGE_CURVE('',#12651,#12652,#7872,.T.);
#16857=EDGE_CURVE('',#12653,#12651,#1792,.T.);
#16858=EDGE_CURVE('',#12648,#12653,#1793,.F.);
#16859=EDGE_CURVE('',#12654,#12649,#1794,.T.);
#16860=EDGE_CURVE('',#12652,#12654,#1795,.T.);
#16861=EDGE_CURVE('',#12655,#12656,#7873,.T.);
#16862=EDGE_CURVE('',#12657,#12655,#1796,.T.);
#16863=EDGE_CURVE('',#12658,#12657,#1797,.T.);
#16864=EDGE_CURVE('',#12658,#12659,#6219,.F.);
#16865=EDGE_CURVE('',#12660,#12659,#1798,.T.);
#16866=EDGE_CURVE('',#12656,#12660,#1799,.F.);
#16867=EDGE_CURVE('',#12661,#12662,#7874,.T.);
#16868=EDGE_CURVE('',#12663,#12661,#1800,.F.);
#16869=EDGE_CURVE('',#12655,#12663,#1801,.T.);
#16870=EDGE_CURVE('',#12662,#12656,#1802,.F.);
#16871=EDGE_CURVE('',#12664,#12665,#7875,.T.);
#16872=EDGE_CURVE('',#12661,#12664,#1803,.F.);
#16873=EDGE_CURVE('',#12666,#12662,#1804,.F.);
#16874=EDGE_CURVE('',#12665,#12666,#1805,.T.);
#16875=EDGE_CURVE('',#12667,#12668,#7876,.T.);
#16876=EDGE_CURVE('',#12669,#12667,#1806,.F.);
#16877=EDGE_CURVE('',#12664,#12669,#1807,.F.);
#16878=EDGE_CURVE('',#12670,#12665,#1808,.T.);
#16879=EDGE_CURVE('',#12668,#12670,#1809,.F.);
#16880=EDGE_CURVE('',#12671,#12672,#7877,.T.);
#16881=EDGE_CURVE('',#12667,#12671,#1810,.F.);
#16882=EDGE_CURVE('',#12672,#12668,#1811,.F.);
#16883=EDGE_CURVE('',#12673,#12674,#7878,.T.);
#16884=EDGE_CURVE('',#12675,#12673,#1812,.F.);
#16885=EDGE_CURVE('',#12671,#12675,#1813,.F.);
#16886=EDGE_CURVE('',#12676,#12672,#1814,.F.);
#16887=EDGE_CURVE('',#12674,#12676,#1815,.F.);
#16888=EDGE_CURVE('',#12677,#12678,#7879,.T.);
#16889=EDGE_CURVE('',#12673,#12677,#1816,.F.);
#16890=EDGE_CURVE('',#12678,#12674,#1817,.F.);
#16891=EDGE_CURVE('',#12679,#12680,#7880,.T.);
#16892=EDGE_CURVE('',#12681,#12679,#1818,.F.);
#16893=EDGE_CURVE('',#12677,#12681,#1819,.F.);
#16894=EDGE_CURVE('',#12682,#12678,#1820,.F.);
#16895=EDGE_CURVE('',#12680,#12682,#1821,.T.);
#16896=EDGE_CURVE('',#12683,#12684,#7881,.T.);
#16897=EDGE_CURVE('',#12679,#12683,#1822,.F.);
#16898=EDGE_CURVE('',#12685,#12680,#1823,.T.);
#16899=EDGE_CURVE('',#12684,#12685,#1824,.T.);
#16900=EDGE_CURVE('',#12686,#12687,#7882,.T.);
#16901=EDGE_CURVE('',#12688,#12686,#1825,.F.);
#16902=EDGE_CURVE('',#12683,#12688,#1826,.F.);
#16903=EDGE_CURVE('',#12689,#12684,#1827,.T.);
#16904=EDGE_CURVE('',#12687,#12689,#1828,.F.);
#16905=EDGE_CURVE('',#12690,#12691,#7883,.T.);
#16906=EDGE_CURVE('',#12686,#12690,#1829,.F.);
#16907=EDGE_CURVE('',#12691,#12687,#1830,.F.);
#16908=EDGE_CURVE('',#12692,#12693,#7884,.T.);
#16909=EDGE_CURVE('',#12694,#12692,#1831,.T.);
#16910=EDGE_CURVE('',#12690,#12694,#1832,.F.);
#16911=EDGE_CURVE('',#12695,#12691,#1833,.F.);
#16912=EDGE_CURVE('',#12693,#12695,#1834,.F.);
#16913=EDGE_CURVE('',#12696,#12697,#7885,.T.);
#16914=EDGE_CURVE('',#12698,#12696,#1835,.T.);
#16915=EDGE_CURVE('',#12692,#12698,#1836,.T.);
#16916=EDGE_CURVE('',#12697,#12693,#1837,.F.);
#16917=EDGE_CURVE('',#12699,#12700,#7886,.T.);
#16918=EDGE_CURVE('',#12701,#12699,#1838,.F.);
#16919=EDGE_CURVE('',#12696,#12701,#1839,.T.);
#16920=EDGE_CURVE('',#12702,#12697,#1840,.F.);
#16921=EDGE_CURVE('',#12700,#12702,#1841,.T.);
#16922=EDGE_CURVE('',#12703,#12704,#7887,.T.);
#16923=EDGE_CURVE('',#12699,#12703,#1842,.F.);
#16924=EDGE_CURVE('',#12705,#12700,#1843,.T.);
#16925=EDGE_CURVE('',#12704,#12705,#1844,.T.);
#16926=EDGE_CURVE('',#12706,#12707,#7888,.T.);
#16927=EDGE_CURVE('',#12708,#12706,#1845,.F.);
#16928=EDGE_CURVE('',#12703,#12708,#1846,.F.);
#16929=EDGE_CURVE('',#12709,#12704,#1847,.T.);
#16930=EDGE_CURVE('',#12707,#12709,#1848,.F.);
#16931=EDGE_CURVE('',#12710,#12711,#7889,.T.);
#16932=EDGE_CURVE('',#12706,#12710,#1849,.F.);
#16933=EDGE_CURVE('',#12711,#12707,#1850,.F.);
#16934=EDGE_CURVE('',#12712,#12713,#7890,.T.);
#16935=EDGE_CURVE('',#12714,#12712,#1851,.T.);
#16936=EDGE_CURVE('',#12710,#12714,#1852,.F.);
#16937=EDGE_CURVE('',#12715,#12711,#1853,.F.);
#16938=EDGE_CURVE('',#12713,#12715,#1854,.F.);
#16939=EDGE_CURVE('',#12716,#12717,#7891,.T.);
#16940=EDGE_CURVE('',#12718,#12716,#1855,.T.);
#16941=EDGE_CURVE('',#12712,#12718,#1856,.T.);
#16942=EDGE_CURVE('',#12717,#12713,#1857,.F.);
#16943=EDGE_CURVE('',#12719,#12720,#7892,.T.);
#16944=EDGE_CURVE('',#12721,#12719,#1858,.F.);
#16945=EDGE_CURVE('',#12716,#12721,#1859,.T.);
#16946=EDGE_CURVE('',#12722,#12717,#1860,.F.);
#16947=EDGE_CURVE('',#12720,#12722,#1861,.F.);
#16948=EDGE_CURVE('',#12723,#12724,#7893,.T.);
#16949=EDGE_CURVE('',#12719,#12723,#1862,.F.);
#16950=EDGE_CURVE('',#12724,#12720,#1863,.F.);
#16951=EDGE_CURVE('',#12725,#12726,#7894,.T.);
#16952=EDGE_CURVE('',#12727,#12725,#1864,.F.);
#16953=EDGE_CURVE('',#12723,#12727,#1865,.F.);
#16954=EDGE_CURVE('',#12728,#12724,#1866,.F.);
#16955=EDGE_CURVE('',#12726,#12728,#1867,.F.);
#16956=EDGE_CURVE('',#12729,#12730,#7895,.T.);
#16957=EDGE_CURVE('',#12725,#12729,#1868,.F.);
#16958=EDGE_CURVE('',#12730,#12726,#1869,.F.);
#16959=EDGE_CURVE('',#12731,#12732,#7896,.T.);
#16960=EDGE_CURVE('',#12733,#12731,#1870,.T.);
#16961=EDGE_CURVE('',#12729,#12733,#1871,.F.);
#16962=EDGE_CURVE('',#12734,#12730,#1872,.F.);
#16963=EDGE_CURVE('',#12732,#12734,#1873,.F.);
#16964=EDGE_CURVE('',#12735,#12736,#7897,.T.);
#16965=EDGE_CURVE('',#12737,#12735,#1874,.F.);
#16966=EDGE_CURVE('',#12731,#12737,#1875,.T.);
#16967=EDGE_CURVE('',#12736,#12732,#1876,.F.);
#16968=EDGE_CURVE('',#12738,#12739,#7898,.T.);
#16969=EDGE_CURVE('',#12735,#12738,#1877,.F.);
#16970=EDGE_CURVE('',#12740,#12736,#1878,.F.);
#16971=EDGE_CURVE('',#12739,#12740,#1879,.T.);
#16972=EDGE_CURVE('',#12741,#12742,#7899,.T.);
#16973=EDGE_CURVE('',#12743,#12741,#1880,.T.);
#16974=EDGE_CURVE('',#12738,#12743,#1881,.F.);
#16975=EDGE_CURVE('',#12744,#12739,#1882,.T.);
#16976=EDGE_CURVE('',#12742,#12744,#1883,.T.);
#16977=EDGE_CURVE('',#12745,#12746,#7900,.T.);
#16978=EDGE_CURVE('',#12747,#12745,#1884,.T.);
#16979=EDGE_CURVE('',#12748,#12747,#1885,.T.);
#16980=EDGE_CURVE('',#12748,#12749,#6220,.F.);
#16981=EDGE_CURVE('',#12750,#12749,#1886,.T.);
#16982=EDGE_CURVE('',#12746,#12750,#1887,.F.);
#16983=EDGE_CURVE('',#12751,#12752,#7901,.T.);
#16984=EDGE_CURVE('',#12753,#12751,#1888,.F.);
#16985=EDGE_CURVE('',#12745,#12753,#1889,.T.);
#16986=EDGE_CURVE('',#12752,#12746,#1890,.F.);
#16987=EDGE_CURVE('',#12754,#12755,#7902,.T.);
#16988=EDGE_CURVE('',#12751,#12754,#1891,.F.);
#16989=EDGE_CURVE('',#12756,#12752,#1892,.F.);
#16990=EDGE_CURVE('',#12755,#12756,#1893,.T.);
#16991=EDGE_CURVE('',#12757,#12758,#7903,.T.);
#16992=EDGE_CURVE('',#12759,#12757,#1894,.F.);
#16993=EDGE_CURVE('',#12754,#12759,#1895,.F.);
#16994=EDGE_CURVE('',#12760,#12755,#1896,.T.);
#16995=EDGE_CURVE('',#12758,#12760,#1897,.F.);
#16996=EDGE_CURVE('',#12761,#12762,#7904,.T.);
#16997=EDGE_CURVE('',#12757,#12761,#1898,.F.);
#16998=EDGE_CURVE('',#12762,#12758,#1899,.F.);
#16999=EDGE_CURVE('',#12763,#12764,#7905,.T.);
#17000=EDGE_CURVE('',#12765,#12763,#1900,.F.);
#17001=EDGE_CURVE('',#12761,#12765,#1901,.F.);
#17002=EDGE_CURVE('',#12766,#12762,#1902,.F.);
#17003=EDGE_CURVE('',#12764,#12766,#1903,.F.);
#17004=EDGE_CURVE('',#12767,#12768,#7906,.T.);
#17005=EDGE_CURVE('',#12763,#12767,#1904,.F.);
#17006=EDGE_CURVE('',#12768,#12764,#1905,.F.);
#17007=EDGE_CURVE('',#12769,#12770,#7907,.T.);
#17008=EDGE_CURVE('',#12771,#12769,#1906,.F.);
#17009=EDGE_CURVE('',#12767,#12771,#1907,.F.);
#17010=EDGE_CURVE('',#12772,#12768,#1908,.F.);
#17011=EDGE_CURVE('',#12770,#12772,#1909,.T.);
#17012=EDGE_CURVE('',#12773,#12774,#7908,.T.);
#17013=EDGE_CURVE('',#12769,#12773,#1910,.F.);
#17014=EDGE_CURVE('',#12775,#12770,#1911,.T.);
#17015=EDGE_CURVE('',#12774,#12775,#1912,.T.);
#17016=EDGE_CURVE('',#12776,#12777,#7909,.T.);
#17017=EDGE_CURVE('',#12778,#12776,#1913,.F.);
#17018=EDGE_CURVE('',#12773,#12778,#1914,.F.);
#17019=EDGE_CURVE('',#12779,#12774,#1915,.T.);
#17020=EDGE_CURVE('',#12777,#12779,#1916,.F.);
#17021=EDGE_CURVE('',#12780,#12781,#7910,.T.);
#17022=EDGE_CURVE('',#12776,#12780,#1917,.F.);
#17023=EDGE_CURVE('',#12781,#12777,#1918,.F.);
#17024=EDGE_CURVE('',#12782,#12783,#7911,.T.);
#17025=EDGE_CURVE('',#12784,#12782,#1919,.T.);
#17026=EDGE_CURVE('',#12780,#12784,#1920,.F.);
#17027=EDGE_CURVE('',#12785,#12781,#1921,.F.);
#17028=EDGE_CURVE('',#12783,#12785,#1922,.F.);
#17029=EDGE_CURVE('',#12786,#12787,#7912,.T.);
#17030=EDGE_CURVE('',#12788,#12786,#1923,.T.);
#17031=EDGE_CURVE('',#12782,#12788,#1924,.T.);
#17032=EDGE_CURVE('',#12787,#12783,#1925,.F.);
#17033=EDGE_CURVE('',#12789,#12790,#7913,.T.);
#17034=EDGE_CURVE('',#12791,#12789,#1926,.F.);
#17035=EDGE_CURVE('',#12786,#12791,#1927,.T.);
#17036=EDGE_CURVE('',#12792,#12787,#1928,.F.);
#17037=EDGE_CURVE('',#12790,#12792,#1929,.T.);
#17038=EDGE_CURVE('',#12793,#12794,#7914,.T.);
#17039=EDGE_CURVE('',#12789,#12793,#1930,.F.);
#17040=EDGE_CURVE('',#12795,#12790,#1931,.T.);
#17041=EDGE_CURVE('',#12794,#12795,#1932,.T.);
#17042=EDGE_CURVE('',#12796,#12797,#7915,.T.);
#17043=EDGE_CURVE('',#12798,#12796,#1933,.F.);
#17044=EDGE_CURVE('',#12793,#12798,#1934,.F.);
#17045=EDGE_CURVE('',#12799,#12794,#1935,.T.);
#17046=EDGE_CURVE('',#12797,#12799,#1936,.F.);
#17047=EDGE_CURVE('',#12800,#12801,#7916,.T.);
#17048=EDGE_CURVE('',#12796,#12800,#1937,.F.);
#17049=EDGE_CURVE('',#12801,#12797,#1938,.F.);
#17050=EDGE_CURVE('',#12802,#12803,#7917,.T.);
#17051=EDGE_CURVE('',#12804,#12802,#1939,.T.);
#17052=EDGE_CURVE('',#12800,#12804,#1940,.F.);
#17053=EDGE_CURVE('',#12805,#12801,#1941,.F.);
#17054=EDGE_CURVE('',#12803,#12805,#1942,.F.);
#17055=EDGE_CURVE('',#12806,#12807,#7918,.T.);
#17056=EDGE_CURVE('',#12808,#12806,#1943,.T.);
#17057=EDGE_CURVE('',#12802,#12808,#1944,.T.);
#17058=EDGE_CURVE('',#12807,#12803,#1945,.F.);
#17059=EDGE_CURVE('',#12809,#12810,#7919,.T.);
#17060=EDGE_CURVE('',#12811,#12809,#1946,.F.);
#17061=EDGE_CURVE('',#12806,#12811,#1947,.T.);
#17062=EDGE_CURVE('',#12812,#12807,#1948,.F.);
#17063=EDGE_CURVE('',#12810,#12812,#1949,.F.);
#17064=EDGE_CURVE('',#12813,#12814,#7920,.T.);
#17065=EDGE_CURVE('',#12809,#12813,#1950,.F.);
#17066=EDGE_CURVE('',#12814,#12810,#1951,.F.);
#17067=EDGE_CURVE('',#12815,#12816,#7921,.T.);
#17068=EDGE_CURVE('',#12817,#12815,#1952,.F.);
#17069=EDGE_CURVE('',#12813,#12817,#1953,.F.);
#17070=EDGE_CURVE('',#12818,#12814,#1954,.F.);
#17071=EDGE_CURVE('',#12816,#12818,#1955,.F.);
#17072=EDGE_CURVE('',#12819,#12820,#7922,.T.);
#17073=EDGE_CURVE('',#12815,#12819,#1956,.F.);
#17074=EDGE_CURVE('',#12820,#12816,#1957,.F.);
#17075=EDGE_CURVE('',#12821,#12822,#7923,.T.);
#17076=EDGE_CURVE('',#12823,#12821,#1958,.T.);
#17077=EDGE_CURVE('',#12819,#12823,#1959,.F.);
#17078=EDGE_CURVE('',#12824,#12820,#1960,.F.);
#17079=EDGE_CURVE('',#12822,#12824,#1961,.F.);
#17080=EDGE_CURVE('',#12825,#12826,#7924,.T.);
#17081=EDGE_CURVE('',#12827,#12825,#1962,.F.);
#17082=EDGE_CURVE('',#12821,#12827,#1963,.T.);
#17083=EDGE_CURVE('',#12826,#12822,#1964,.F.);
#17084=EDGE_CURVE('',#12828,#12829,#7925,.T.);
#17085=EDGE_CURVE('',#12825,#12828,#1965,.F.);
#17086=EDGE_CURVE('',#12830,#12826,#1966,.F.);
#17087=EDGE_CURVE('',#12829,#12830,#1967,.T.);
#17088=EDGE_CURVE('',#12831,#12832,#7926,.T.);
#17089=EDGE_CURVE('',#12833,#12831,#1968,.T.);
#17090=EDGE_CURVE('',#12828,#12833,#1969,.F.);
#17091=EDGE_CURVE('',#12834,#12829,#1970,.T.);
#17092=EDGE_CURVE('',#12832,#12834,#1971,.T.);
#17093=EDGE_CURVE('',#12835,#12836,#7927,.T.);
#17094=EDGE_CURVE('',#12837,#12835,#1972,.T.);
#17095=EDGE_CURVE('',#12838,#12837,#1973,.T.);
#17096=EDGE_CURVE('',#12838,#12839,#6221,.F.);
#17097=EDGE_CURVE('',#12840,#12839,#1974,.T.);
#17098=EDGE_CURVE('',#12836,#12840,#1975,.F.);
#17099=EDGE_CURVE('',#12841,#12842,#7928,.T.);
#17100=EDGE_CURVE('',#12843,#12841,#1976,.F.);
#17101=EDGE_CURVE('',#12835,#12843,#1977,.T.);
#17102=EDGE_CURVE('',#12842,#12836,#1978,.F.);
#17103=EDGE_CURVE('',#12844,#12845,#7929,.T.);
#17104=EDGE_CURVE('',#12841,#12844,#1979,.F.);
#17105=EDGE_CURVE('',#12846,#12842,#1980,.F.);
#17106=EDGE_CURVE('',#12845,#12846,#1981,.T.);
#17107=EDGE_CURVE('',#12847,#12848,#7930,.T.);
#17108=EDGE_CURVE('',#12849,#12847,#1982,.F.);
#17109=EDGE_CURVE('',#12844,#12849,#1983,.F.);
#17110=EDGE_CURVE('',#12850,#12845,#1984,.T.);
#17111=EDGE_CURVE('',#12848,#12850,#1985,.F.);
#17112=EDGE_CURVE('',#12851,#12852,#7931,.T.);
#17113=EDGE_CURVE('',#12847,#12851,#1986,.F.);
#17114=EDGE_CURVE('',#12852,#12848,#1987,.F.);
#17115=EDGE_CURVE('',#12853,#12854,#7932,.T.);
#17116=EDGE_CURVE('',#12855,#12853,#1988,.F.);
#17117=EDGE_CURVE('',#12851,#12855,#1989,.F.);
#17118=EDGE_CURVE('',#12856,#12852,#1990,.F.);
#17119=EDGE_CURVE('',#12854,#12856,#1991,.F.);
#17120=EDGE_CURVE('',#12857,#12858,#7933,.T.);
#17121=EDGE_CURVE('',#12853,#12857,#1992,.F.);
#17122=EDGE_CURVE('',#12858,#12854,#1993,.F.);
#17123=EDGE_CURVE('',#12859,#12860,#7934,.T.);
#17124=EDGE_CURVE('',#12861,#12859,#1994,.F.);
#17125=EDGE_CURVE('',#12857,#12861,#1995,.F.);
#17126=EDGE_CURVE('',#12862,#12858,#1996,.F.);
#17127=EDGE_CURVE('',#12860,#12862,#1997,.T.);
#17128=EDGE_CURVE('',#12863,#12864,#7935,.T.);
#17129=EDGE_CURVE('',#12859,#12863,#1998,.F.);
#17130=EDGE_CURVE('',#12865,#12860,#1999,.T.);
#17131=EDGE_CURVE('',#12864,#12865,#2000,.T.);
#17132=EDGE_CURVE('',#12866,#12867,#7936,.T.);
#17133=EDGE_CURVE('',#12868,#12866,#2001,.F.);
#17134=EDGE_CURVE('',#12863,#12868,#2002,.F.);
#17135=EDGE_CURVE('',#12869,#12864,#2003,.T.);
#17136=EDGE_CURVE('',#12867,#12869,#2004,.F.);
#17137=EDGE_CURVE('',#12870,#12871,#7937,.T.);
#17138=EDGE_CURVE('',#12866,#12870,#2005,.F.);
#17139=EDGE_CURVE('',#12871,#12867,#2006,.F.);
#17140=EDGE_CURVE('',#12872,#12873,#7938,.T.);
#17141=EDGE_CURVE('',#12874,#12872,#2007,.T.);
#17142=EDGE_CURVE('',#12870,#12874,#2008,.F.);
#17143=EDGE_CURVE('',#12875,#12871,#2009,.F.);
#17144=EDGE_CURVE('',#12873,#12875,#2010,.F.);
#17145=EDGE_CURVE('',#12876,#12877,#7939,.T.);
#17146=EDGE_CURVE('',#12878,#12876,#2011,.T.);
#17147=EDGE_CURVE('',#12872,#12878,#2012,.T.);
#17148=EDGE_CURVE('',#12877,#12873,#2013,.F.);
#17149=EDGE_CURVE('',#12879,#12880,#7940,.T.);
#17150=EDGE_CURVE('',#12881,#12879,#2014,.F.);
#17151=EDGE_CURVE('',#12876,#12881,#2015,.T.);
#17152=EDGE_CURVE('',#12882,#12877,#2016,.F.);
#17153=EDGE_CURVE('',#12880,#12882,#2017,.T.);
#17154=EDGE_CURVE('',#12883,#12884,#7941,.T.);
#17155=EDGE_CURVE('',#12879,#12883,#2018,.F.);
#17156=EDGE_CURVE('',#12885,#12880,#2019,.T.);
#17157=EDGE_CURVE('',#12884,#12885,#2020,.T.);
#17158=EDGE_CURVE('',#12886,#12887,#7942,.T.);
#17159=EDGE_CURVE('',#12888,#12886,#2021,.F.);
#17160=EDGE_CURVE('',#12883,#12888,#2022,.F.);
#17161=EDGE_CURVE('',#12889,#12884,#2023,.T.);
#17162=EDGE_CURVE('',#12887,#12889,#2024,.F.);
#17163=EDGE_CURVE('',#12890,#12891,#7943,.T.);
#17164=EDGE_CURVE('',#12886,#12890,#2025,.F.);
#17165=EDGE_CURVE('',#12891,#12887,#2026,.F.);
#17166=EDGE_CURVE('',#12892,#12893,#7944,.T.);
#17167=EDGE_CURVE('',#12894,#12892,#2027,.T.);
#17168=EDGE_CURVE('',#12890,#12894,#2028,.F.);
#17169=EDGE_CURVE('',#12895,#12891,#2029,.F.);
#17170=EDGE_CURVE('',#12893,#12895,#2030,.F.);
#17171=EDGE_CURVE('',#12896,#12897,#7945,.T.);
#17172=EDGE_CURVE('',#12898,#12896,#2031,.T.);
#17173=EDGE_CURVE('',#12892,#12898,#2032,.T.);
#17174=EDGE_CURVE('',#12897,#12893,#2033,.F.);
#17175=EDGE_CURVE('',#12899,#12900,#7946,.T.);
#17176=EDGE_CURVE('',#12901,#12899,#2034,.F.);
#17177=EDGE_CURVE('',#12896,#12901,#2035,.T.);
#17178=EDGE_CURVE('',#12902,#12897,#2036,.F.);
#17179=EDGE_CURVE('',#12900,#12902,#2037,.F.);
#17180=EDGE_CURVE('',#12903,#12904,#7947,.T.);
#17181=EDGE_CURVE('',#12899,#12903,#2038,.F.);
#17182=EDGE_CURVE('',#12904,#12900,#2039,.F.);
#17183=EDGE_CURVE('',#12905,#12906,#7948,.T.);
#17184=EDGE_CURVE('',#12907,#12905,#2040,.F.);
#17185=EDGE_CURVE('',#12903,#12907,#2041,.F.);
#17186=EDGE_CURVE('',#12908,#12904,#2042,.F.);
#17187=EDGE_CURVE('',#12906,#12908,#2043,.F.);
#17188=EDGE_CURVE('',#12909,#12910,#7949,.T.);
#17189=EDGE_CURVE('',#12905,#12909,#2044,.F.);
#17190=EDGE_CURVE('',#12910,#12906,#2045,.F.);
#17191=EDGE_CURVE('',#12911,#12912,#7950,.T.);
#17192=EDGE_CURVE('',#12913,#12911,#2046,.T.);
#17193=EDGE_CURVE('',#12909,#12913,#2047,.F.);
#17194=EDGE_CURVE('',#12914,#12910,#2048,.F.);
#17195=EDGE_CURVE('',#12912,#12914,#2049,.F.);
#17196=EDGE_CURVE('',#12915,#12916,#7951,.T.);
#17197=EDGE_CURVE('',#12917,#12915,#2050,.F.);
#17198=EDGE_CURVE('',#12911,#12917,#2051,.T.);
#17199=EDGE_CURVE('',#12916,#12912,#2052,.F.);
#17200=EDGE_CURVE('',#12918,#12919,#7952,.T.);
#17201=EDGE_CURVE('',#12915,#12918,#2053,.F.);
#17202=EDGE_CURVE('',#12920,#12916,#2054,.F.);
#17203=EDGE_CURVE('',#12919,#12920,#2055,.T.);
#17204=EDGE_CURVE('',#12921,#12922,#7953,.T.);
#17205=EDGE_CURVE('',#12923,#12921,#2056,.T.);
#17206=EDGE_CURVE('',#12918,#12923,#2057,.F.);
#17207=EDGE_CURVE('',#12924,#12919,#2058,.T.);
#17208=EDGE_CURVE('',#12922,#12924,#2059,.T.);
#17209=EDGE_CURVE('',#12925,#12922,#2060,.T.);
#17210=EDGE_CURVE('',#12925,#12926,#6222,.T.);
#17211=EDGE_CURVE('',#12921,#12926,#2061,.T.);
#17212=EDGE_CURVE('',#12927,#12832,#2062,.T.);
#17213=EDGE_CURVE('',#12927,#12928,#6223,.T.);
#17214=EDGE_CURVE('',#12831,#12928,#2063,.T.);
#17215=EDGE_CURVE('',#12929,#12742,#2064,.T.);
#17216=EDGE_CURVE('',#12929,#12930,#6224,.T.);
#17217=EDGE_CURVE('',#12741,#12930,#2065,.T.);
#17218=EDGE_CURVE('',#12931,#12652,#2066,.T.);
#17219=EDGE_CURVE('',#12931,#12932,#6225,.T.);
#17220=EDGE_CURVE('',#12651,#12932,#2067,.T.);
#17221=EDGE_CURVE('',#12933,#12563,#2068,.T.);
#17222=EDGE_CURVE('',#12562,#12933,#6226,.T.);
#17223=EDGE_CURVE('',#12934,#12553,#2069,.T.);
#17224=EDGE_CURVE('',#12935,#12934,#6227,.F.);
#17225=EDGE_CURVE('',#12552,#12935,#2070,.F.);
#17226=EDGE_CURVE('',#12541,#12936,#2071,.T.);
#17227=EDGE_CURVE('',#12936,#12937,#2072,.T.);
#17228=EDGE_CURVE('',#12937,#12938,#6228,.T.);
#17229=EDGE_CURVE('',#12939,#12938,#2073,.T.);
#17230=EDGE_CURVE('',#12540,#12939,#2074,.T.);
#17231=EDGE_CURVE('',#12431,#12940,#2075,.T.);
#17232=EDGE_CURVE('',#12940,#12941,#2076,.T.);
#17233=EDGE_CURVE('',#12941,#12942,#6229,.T.);
#17234=EDGE_CURVE('',#12943,#12942,#2077,.T.);
#17235=EDGE_CURVE('',#12430,#12943,#2078,.T.);
#17236=EDGE_CURVE('',#12321,#12944,#2079,.T.);
#17237=EDGE_CURVE('',#12944,#12945,#2080,.T.);
#17238=EDGE_CURVE('',#12945,#12946,#6230,.T.);
#17239=EDGE_CURVE('',#12947,#12946,#2081,.T.);
#17240=EDGE_CURVE('',#12320,#12947,#2082,.T.);
#17241=EDGE_CURVE('',#12211,#12948,#2083,.T.);
#17242=EDGE_CURVE('',#12948,#12949,#2084,.T.);
#17243=EDGE_CURVE('',#12949,#12950,#6231,.T.);
#17244=EDGE_CURVE('',#12951,#12950,#2085,.T.);
#17245=EDGE_CURVE('',#12210,#12951,#2086,.T.);
#17246=EDGE_CURVE('',#12101,#12952,#2087,.T.);
#17247=EDGE_CURVE('',#12952,#12953,#2088,.T.);
#17248=EDGE_CURVE('',#12953,#12954,#6232,.T.);
#17249=EDGE_CURVE('',#12955,#12954,#2089,.T.);
#17250=EDGE_CURVE('',#12100,#12955,#2090,.T.);
#17251=EDGE_CURVE('',#12085,#12956,#2091,.T.);
#17252=EDGE_CURVE('',#12956,#12957,#2092,.T.);
#17253=EDGE_CURVE('',#12957,#12958,#6233,.T.);
#17254=EDGE_CURVE('',#12959,#12958,#2093,.T.);
#17255=EDGE_CURVE('',#12084,#12959,#2094,.T.);
#17256=EDGE_CURVE('',#12960,#12960,#6234,.T.);
#17257=EDGE_CURVE('',#12960,#12961,#7954,.T.);
#17258=EDGE_CURVE('',#12961,#12961,#6235,.T.);
#17259=EDGE_CURVE('',#12962,#12963,#6236,.T.);
#17260=EDGE_CURVE('',#12963,#12964,#7955,.T.);
#17261=EDGE_CURVE('',#12965,#12964,#6237,.T.);
#17262=EDGE_CURVE('',#12965,#12962,#7956,.T.);
#17263=EDGE_CURVE('',#12964,#12966,#7957,.T.);
#17264=EDGE_CURVE('',#12966,#12967,#6238,.T.);
#17265=EDGE_CURVE('',#12967,#12968,#7958,.T.);
#17266=EDGE_CURVE('',#12968,#12965,#7959,.T.);
#17267=EDGE_CURVE('',#12969,#12969,#6239,.T.);
#17268=EDGE_CURVE('',#12969,#12970,#7960,.T.);
#17269=EDGE_CURVE('',#12970,#12970,#6240,.T.);
#17270=EDGE_CURVE('',#12971,#12972,#6241,.T.);
#17271=EDGE_CURVE('',#12972,#12973,#7961,.T.);
#17272=EDGE_CURVE('',#12974,#12973,#6242,.T.);
#17273=EDGE_CURVE('',#12974,#12971,#7962,.T.);
#17274=EDGE_CURVE('',#12975,#12976,#7963,.T.);
#17275=EDGE_CURVE('',#12976,#12977,#6243,.T.);
#17276=EDGE_CURVE('',#12977,#12974,#7964,.T.);
#17277=EDGE_CURVE('',#12973,#12975,#7965,.T.);
#17278=EDGE_CURVE('',#12978,#12978,#6244,.T.);
#17279=EDGE_CURVE('',#12978,#12979,#7966,.T.);
#17280=EDGE_CURVE('',#12979,#12979,#6245,.T.);
#17281=EDGE_CURVE('',#12980,#12967,#7967,.T.);
#17282=EDGE_CURVE('',#12981,#12980,#7968,.T.);
#17283=EDGE_CURVE('',#12981,#12968,#7969,.T.);
#17284=EDGE_CURVE('',#12982,#12977,#7970,.T.);
#17285=EDGE_CURVE('',#12982,#12983,#7971,.T.);
#17286=EDGE_CURVE('',#12983,#12984,#7972,.T.);
#17287=EDGE_CURVE('',#12984,#12971,#7973,.T.);
#17288=EDGE_CURVE('',#12981,#12985,#7974,.T.);
#17289=EDGE_CURVE('',#12985,#12975,#7975,.T.);
#17290=EDGE_CURVE('',#12972,#12962,#7976,.T.);
#17291=EDGE_CURVE('',#12986,#12984,#6246,.T.);
#17292=EDGE_CURVE('',#12987,#12986,#7977,.T.);
#17293=EDGE_CURVE('',#12988,#12987,#6247,.T.);
#17294=EDGE_CURVE('',#12989,#12988,#7978,.T.);
#17295=EDGE_CURVE('',#12990,#12989,#6248,.T.);
#17296=EDGE_CURVE('',#12991,#12990,#7979,.T.);
#17297=EDGE_CURVE('',#12992,#12991,#6249,.T.);
#17298=EDGE_CURVE('',#12993,#12992,#7980,.T.);
#17299=EDGE_CURVE('',#12994,#12993,#7981,.T.);
#17300=EDGE_CURVE('',#12995,#12994,#7982,.T.);
#17301=EDGE_CURVE('',#12996,#12995,#7983,.T.);
#17302=EDGE_CURVE('',#12997,#12996,#7984,.T.);
#17303=EDGE_CURVE('',#12998,#12997,#6250,.T.);
#17304=EDGE_CURVE('',#12999,#12998,#7985,.T.);
#17305=EDGE_CURVE('',#13000,#12999,#6251,.T.);
#17306=EDGE_CURVE('',#13001,#13000,#7986,.T.);
#17307=EDGE_CURVE('',#13002,#13001,#7987,.T.);
#17308=EDGE_CURVE('',#13003,#13002,#7988,.T.);
#17309=EDGE_CURVE('',#13004,#13003,#7989,.T.);
#17310=EDGE_CURVE('',#13005,#13004,#7990,.T.);
#17311=EDGE_CURVE('',#13006,#13005,#6252,.T.);
#17312=EDGE_CURVE('',#13007,#13006,#7991,.T.);
#17313=EDGE_CURVE('',#13008,#13007,#6253,.T.);
#17314=EDGE_CURVE('',#13009,#13008,#7992,.T.);
#17315=EDGE_CURVE('',#13010,#13009,#6254,.T.);
#17316=EDGE_CURVE('',#13011,#13010,#7993,.T.);
#17317=EDGE_CURVE('',#13012,#13011,#6255,.T.);
#17318=EDGE_CURVE('',#12963,#13012,#7994,.T.);
#17319=EDGE_CURVE('',#13013,#13013,#6256,.T.);
#17320=EDGE_CURVE('',#13014,#13014,#6257,.T.);
#17321=EDGE_CURVE('',#12926,#12949,#2095,.T.);
#17322=EDGE_CURVE('',#12950,#12925,#2096,.T.);
#17323=EDGE_CURVE('',#12928,#12945,#2097,.T.);
#17324=EDGE_CURVE('',#12946,#12927,#2098,.T.);
#17325=EDGE_CURVE('',#12930,#12941,#2099,.T.);
#17326=EDGE_CURVE('',#12942,#12929,#2100,.T.);
#17327=EDGE_CURVE('',#12932,#12937,#2101,.T.);
#17328=EDGE_CURVE('',#12938,#12931,#2102,.T.);
#17329=EDGE_CURVE('',#12958,#12933,#2103,.T.);
#17330=EDGE_CURVE('',#12557,#12074,#2104,.T.);
#17331=EDGE_CURVE('',#12564,#12957,#2105,.T.);
#17332=EDGE_CURVE('',#12075,#12556,#2106,.T.);
#17333=EDGE_CURVE('',#12954,#12546,#2107,.T.);
#17334=EDGE_CURVE('',#12935,#12090,#2108,.T.);
#17335=EDGE_CURVE('',#12549,#12953,#2109,.T.);
#17336=EDGE_CURVE('',#12091,#12934,#2110,.T.);
#17337=EDGE_CURVE('',#12839,#12107,#2111,.T.);
#17338=EDGE_CURVE('',#12108,#12838,#2112,.T.);
#17339=EDGE_CURVE('',#12749,#12217,#2113,.T.);
#17340=EDGE_CURVE('',#12218,#12748,#2114,.T.);
#17341=EDGE_CURVE('',#12659,#12327,#2115,.T.);
#17342=EDGE_CURVE('',#12328,#12658,#2116,.T.);
#17343=EDGE_CURVE('',#12569,#12437,#2117,.T.);
#17344=EDGE_CURVE('',#12438,#12568,#2118,.T.);
#17345=EDGE_CURVE('',#13015,#13016,#7995,.T.);
#17346=EDGE_CURVE('',#13016,#13017,#7996,.T.);
#17347=EDGE_CURVE('',#13017,#13018,#7997,.T.);
#17348=EDGE_CURVE('',#13015,#13018,#7998,.T.);
#17349=EDGE_CURVE('',#13016,#13019,#7999,.T.);
#17350=EDGE_CURVE('',#13019,#13020,#8000,.T.);
#17351=EDGE_CURVE('',#13020,#13017,#8001,.T.);
#17352=EDGE_CURVE('',#13019,#13021,#8002,.T.);
#17353=EDGE_CURVE('',#13021,#13022,#8003,.T.);
#17354=EDGE_CURVE('',#13022,#13020,#8004,.T.);
#17355=EDGE_CURVE('',#13021,#13023,#8005,.T.);
#17356=EDGE_CURVE('',#13023,#13024,#8006,.T.);
#17357=EDGE_CURVE('',#13024,#13022,#8007,.T.);
#17358=EDGE_CURVE('',#13023,#13025,#8008,.T.);
#17359=EDGE_CURVE('',#13025,#13026,#8009,.T.);
#17360=EDGE_CURVE('',#13026,#13024,#8010,.T.);
#17361=EDGE_CURVE('',#13025,#13027,#8011,.T.);
#17362=EDGE_CURVE('',#13027,#13028,#8012,.T.);
#17363=EDGE_CURVE('',#13028,#13026,#8013,.T.);
#17364=EDGE_CURVE('',#13027,#13015,#8014,.T.);
#17365=EDGE_CURVE('',#13018,#13028,#8015,.T.);
#17366=EDGE_CURVE('',#13029,#13029,#6258,.T.);
#17367=EDGE_CURVE('',#13029,#13030,#8016,.T.);
#17368=EDGE_CURVE('',#13030,#13030,#6259,.T.);
#17369=EDGE_CURVE('',#13031,#13032,#6260,.T.);
#17370=EDGE_CURVE('',#13032,#13033,#8017,.T.);
#17371=EDGE_CURVE('',#13033,#13034,#6261,.T.);
#17372=EDGE_CURVE('',#13031,#13034,#8018,.T.);
#17373=EDGE_CURVE('',#13032,#13035,#8019,.T.);
#17374=EDGE_CURVE('',#13035,#13036,#8020,.T.);
#17375=EDGE_CURVE('',#13036,#13033,#8021,.T.);
#17376=EDGE_CURVE('',#13035,#13037,#6262,.T.);
#17377=EDGE_CURVE('',#13037,#13038,#8022,.T.);
#17378=EDGE_CURVE('',#13038,#13036,#6263,.T.);
#17379=EDGE_CURVE('',#13037,#13004,#8023,.T.);
#17380=EDGE_CURVE('',#13003,#13038,#8024,.T.);
#17381=EDGE_CURVE('',#13001,#13031,#8025,.T.);
#17382=EDGE_CURVE('',#13034,#13002,#8026,.T.);
#17383=EDGE_CURVE('',#13039,#13039,#6264,.T.);
#17384=EDGE_CURVE('',#13040,#13040,#6265,.T.);
#17385=EDGE_CURVE('',#13041,#13042,#8027,.T.);
#17386=EDGE_CURVE('',#13042,#13043,#8028,.T.);
#17387=EDGE_CURVE('',#13043,#13044,#8029,.T.);
#17388=EDGE_CURVE('',#13041,#13044,#8030,.T.);
#17389=EDGE_CURVE('',#13042,#13045,#8031,.T.);
#17390=EDGE_CURVE('',#13045,#13046,#8032,.T.);
#17391=EDGE_CURVE('',#13046,#13043,#8033,.T.);
#17392=EDGE_CURVE('',#13045,#13047,#8034,.T.);
#17393=EDGE_CURVE('',#13047,#13048,#8035,.T.);
#17394=EDGE_CURVE('',#13048,#13046,#8036,.T.);
#17395=EDGE_CURVE('',#13047,#13049,#8037,.T.);
#17396=EDGE_CURVE('',#13049,#13050,#8038,.T.);
#17397=EDGE_CURVE('',#13050,#13048,#8039,.T.);
#17398=EDGE_CURVE('',#13049,#13051,#8040,.T.);
#17399=EDGE_CURVE('',#13051,#13052,#8041,.T.);
#17400=EDGE_CURVE('',#13052,#13050,#8042,.T.);
#17401=EDGE_CURVE('',#13051,#13053,#8043,.T.);
#17402=EDGE_CURVE('',#13053,#13054,#8044,.T.);
#17403=EDGE_CURVE('',#13054,#13052,#8045,.T.);
#17404=EDGE_CURVE('',#13053,#13041,#8046,.T.);
#17405=EDGE_CURVE('',#13044,#13054,#8047,.T.);
#17406=EDGE_CURVE('',#13055,#13055,#6266,.T.);
#17407=EDGE_CURVE('',#13055,#13056,#8048,.T.);
#17408=EDGE_CURVE('',#13056,#13056,#6267,.T.);
#17409=EDGE_CURVE('',#13039,#13057,#8049,.T.);
#17410=EDGE_CURVE('',#13057,#13057,#6268,.T.);
#17411=EDGE_CURVE('',#13040,#13058,#8050,.T.);
#17412=EDGE_CURVE('',#13058,#13058,#6269,.T.);
#17413=EDGE_CURVE('',#13059,#13060,#6270,.T.);
#17414=EDGE_CURVE('',#13060,#13061,#8051,.T.);
#17415=EDGE_CURVE('',#13062,#13061,#6271,.T.);
#17416=EDGE_CURVE('',#13059,#13062,#8052,.T.);
#17417=EDGE_CURVE('',#13063,#13059,#8053,.T.);
#17418=EDGE_CURVE('',#13064,#13062,#8054,.T.);
#17419=EDGE_CURVE('',#13063,#13064,#8055,.T.);
#17420=EDGE_CURVE('',#13065,#13063,#6272,.T.);
#17421=EDGE_CURVE('',#13066,#13064,#6273,.T.);
#17422=EDGE_CURVE('',#13065,#13066,#8056,.T.);
#17423=EDGE_CURVE('',#12993,#13065,#8057,.T.);
#17424=EDGE_CURVE('',#12994,#13066,#8058,.T.);
#17425=EDGE_CURVE('',#13060,#12996,#8059,.T.);
#17426=EDGE_CURVE('',#13061,#12995,#8060,.T.);
#17427=EDGE_CURVE('',#13067,#13067,#6274,.T.);
#17428=EDGE_CURVE('',#13068,#13068,#6275,.T.);
#17429=EDGE_CURVE('',#13069,#13070,#8061,.T.);
#17430=EDGE_CURVE('',#13070,#13071,#8062,.T.);
#17431=EDGE_CURVE('',#13072,#13071,#8063,.T.);
#17432=EDGE_CURVE('',#13069,#13072,#8064,.T.);
#17433=EDGE_CURVE('',#13073,#13069,#8065,.T.);
#17434=EDGE_CURVE('',#13074,#13072,#8066,.T.);
#17435=EDGE_CURVE('',#13073,#13074,#8067,.T.);
#17436=EDGE_CURVE('',#13075,#13073,#8068,.T.);
#17437=EDGE_CURVE('',#13076,#13074,#8069,.T.);
#17438=EDGE_CURVE('',#13075,#13076,#8070,.T.);
#17439=EDGE_CURVE('',#13077,#13075,#8071,.T.);
#17440=EDGE_CURVE('',#13078,#13076,#8072,.T.);
#17441=EDGE_CURVE('',#13077,#13078,#8073,.T.);
#17442=EDGE_CURVE('',#13079,#13077,#8074,.T.);
#17443=EDGE_CURVE('',#13080,#13078,#8075,.T.);
#17444=EDGE_CURVE('',#13079,#13080,#8076,.T.);
#17445=EDGE_CURVE('',#13081,#13079,#8077,.T.);
#17446=EDGE_CURVE('',#13082,#13080,#8078,.T.);
#17447=EDGE_CURVE('',#13081,#13082,#8079,.T.);
#17448=EDGE_CURVE('',#13070,#13081,#8080,.T.);
#17449=EDGE_CURVE('',#13071,#13082,#8081,.T.);
#17450=EDGE_CURVE('',#13083,#13083,#6276,.T.);
#17451=EDGE_CURVE('',#13083,#13084,#8082,.T.);
#17452=EDGE_CURVE('',#13084,#13084,#6277,.T.);
#17453=EDGE_CURVE('',#13085,#13086,#8083,.T.);
#17454=EDGE_CURVE('',#13086,#13087,#8084,.T.);
#17455=EDGE_CURVE('',#13088,#13087,#8085,.T.);
#17456=EDGE_CURVE('',#13085,#13088,#8086,.T.);
#17457=EDGE_CURVE('',#13089,#13085,#8087,.T.);
#17458=EDGE_CURVE('',#13090,#13088,#8088,.T.);
#17459=EDGE_CURVE('',#13089,#13090,#8089,.T.);
#17460=EDGE_CURVE('',#13091,#13089,#8090,.T.);
#17461=EDGE_CURVE('',#13092,#13090,#8091,.T.);
#17462=EDGE_CURVE('',#13091,#13092,#8092,.T.);
#17463=EDGE_CURVE('',#13093,#13091,#8093,.T.);
#17464=EDGE_CURVE('',#13094,#13092,#8094,.T.);
#17465=EDGE_CURVE('',#13093,#13094,#8095,.T.);
#17466=EDGE_CURVE('',#13095,#13093,#8096,.T.);
#17467=EDGE_CURVE('',#13096,#13094,#8097,.T.);
#17468=EDGE_CURVE('',#13095,#13096,#8098,.T.);
#17469=EDGE_CURVE('',#13097,#13095,#8099,.T.);
#17470=EDGE_CURVE('',#13098,#13096,#8100,.T.);
#17471=EDGE_CURVE('',#13097,#13098,#8101,.T.);
#17472=EDGE_CURVE('',#13086,#13097,#8102,.T.);
#17473=EDGE_CURVE('',#13087,#13098,#8103,.T.);
#17474=EDGE_CURVE('',#13099,#13099,#6278,.T.);
#17475=EDGE_CURVE('',#13099,#13100,#8104,.T.);
#17476=EDGE_CURVE('',#13100,#13100,#6279,.T.);
#17477=EDGE_CURVE('',#13101,#12992,#8105,.T.);
#17478=EDGE_CURVE('',#13101,#13102,#8106,.T.);
#17479=EDGE_CURVE('',#13102,#12997,#8107,.T.);
#17480=EDGE_CURVE('',#13103,#13103,#6280,.T.);
#17481=EDGE_CURVE('',#13103,#13068,#8108,.T.);
#17482=EDGE_CURVE('',#13104,#13104,#6281,.T.);
#17483=EDGE_CURVE('',#13104,#13067,#8109,.T.);
#17484=EDGE_CURVE('',#13105,#13105,#6282,.T.);
#17485=EDGE_CURVE('',#13105,#13013,#8110,.T.);
#17486=EDGE_CURVE('',#13106,#13106,#6283,.T.);
#17487=EDGE_CURVE('',#13106,#13014,#8111,.T.);
#17488=EDGE_CURVE('',#12985,#13107,#8112,.T.);
#17489=EDGE_CURVE('',#13107,#12976,#8113,.T.);
#17490=EDGE_CURVE('',#13107,#12982,#6284,.T.);
#17491=EDGE_CURVE('',#13108,#12983,#6285,.T.);
#17492=EDGE_CURVE('',#13108,#12986,#8114,.T.);
#17493=EDGE_CURVE('',#13108,#13109,#8115,.T.);
#17494=EDGE_CURVE('',#13109,#12987,#8116,.T.);
#17495=EDGE_CURVE('',#13109,#13110,#6286,.T.);
#17496=EDGE_CURVE('',#13110,#12988,#8117,.T.);
#17497=EDGE_CURVE('',#13110,#13111,#8118,.T.);
#17498=EDGE_CURVE('',#13111,#12989,#8119,.T.);
#17499=EDGE_CURVE('',#13111,#13112,#6287,.T.);
#17500=EDGE_CURVE('',#13112,#12990,#8120,.T.);
#17501=EDGE_CURVE('',#13112,#13113,#8121,.T.);
#17502=EDGE_CURVE('',#13113,#12991,#8122,.T.);
#17503=EDGE_CURVE('',#13113,#13101,#6288,.T.);
#17504=EDGE_CURVE('',#13102,#13114,#6289,.T.);
#17505=EDGE_CURVE('',#13114,#12998,#8123,.T.);
#17506=EDGE_CURVE('',#13114,#13115,#8124,.T.);
#17507=EDGE_CURVE('',#13115,#12999,#8125,.T.);
#17508=EDGE_CURVE('',#13115,#13116,#6290,.T.);
#17509=EDGE_CURVE('',#13116,#13000,#8126,.T.);
#17510=EDGE_CURVE('',#13117,#13116,#8127,.T.);
#17511=EDGE_CURVE('',#13117,#13005,#8128,.T.);
#17512=EDGE_CURVE('',#13117,#13118,#6291,.T.);
#17513=EDGE_CURVE('',#13118,#13006,#8129,.T.);
#17514=EDGE_CURVE('',#13119,#13118,#8130,.T.);
#17515=EDGE_CURVE('',#13119,#13007,#8131,.T.);
#17516=EDGE_CURVE('',#13119,#13120,#6292,.T.);
#17517=EDGE_CURVE('',#13120,#13008,#8132,.T.);
#17518=EDGE_CURVE('',#13121,#13120,#8133,.T.);
#17519=EDGE_CURVE('',#13121,#13009,#8134,.T.);
#17520=EDGE_CURVE('',#13121,#13122,#6293,.T.);
#17521=EDGE_CURVE('',#13122,#13010,#8135,.T.);
#17522=EDGE_CURVE('',#13123,#13122,#8136,.T.);
#17523=EDGE_CURVE('',#13123,#13011,#8137,.T.);
#17524=EDGE_CURVE('',#13124,#13123,#6294,.T.);
#17525=EDGE_CURVE('',#13124,#13012,#8138,.T.);
#17526=EDGE_CURVE('',#13125,#13124,#8139,.T.);
#17527=EDGE_CURVE('',#13125,#12966,#8140,.T.);
#17528=EDGE_CURVE('',#13125,#12980,#6295,.T.);
#17529=ORIENTED_EDGE('',*,*,#13126,.T.);
#17530=ORIENTED_EDGE('',*,*,#13127,.T.);
#17531=ORIENTED_EDGE('',*,*,#13128,.T.);
#17532=ORIENTED_EDGE('',*,*,#13129,.T.);
#17533=ORIENTED_EDGE('',*,*,#13130,.T.);
#17534=ORIENTED_EDGE('',*,*,#13131,.T.);
#17535=ORIENTED_EDGE('',*,*,#13132,.T.);
#17536=ORIENTED_EDGE('',*,*,#13133,.T.);
#17537=ORIENTED_EDGE('',*,*,#13134,.T.);
#17538=ORIENTED_EDGE('',*,*,#13135,.T.);
#17539=ORIENTED_EDGE('',*,*,#13136,.T.);
#17540=ORIENTED_EDGE('',*,*,#13137,.T.);
#17541=ORIENTED_EDGE('',*,*,#13138,.T.);
#17542=ORIENTED_EDGE('',*,*,#13139,.T.);
#17543=ORIENTED_EDGE('',*,*,#13140,.T.);
#17544=ORIENTED_EDGE('',*,*,#13141,.T.);
#17545=ORIENTED_EDGE('',*,*,#13142,.T.);
#17546=ORIENTED_EDGE('',*,*,#13143,.T.);
#17547=ORIENTED_EDGE('',*,*,#13144,.T.);
#17548=ORIENTED_EDGE('',*,*,#13145,.T.);
#17549=ORIENTED_EDGE('',*,*,#13146,.T.);
#17550=ORIENTED_EDGE('',*,*,#13147,.T.);
#17551=ORIENTED_EDGE('',*,*,#13148,.T.);
#17552=ORIENTED_EDGE('',*,*,#13149,.T.);
#17553=ORIENTED_EDGE('',*,*,#13150,.T.);
#17554=ORIENTED_EDGE('',*,*,#13151,.F.);
#17555=ORIENTED_EDGE('',*,*,#13152,.F.);
#17556=ORIENTED_EDGE('',*,*,#13153,.F.);
#17557=ORIENTED_EDGE('',*,*,#13127,.F.);
#17558=ORIENTED_EDGE('',*,*,#13153,.T.);
#17559=ORIENTED_EDGE('',*,*,#13154,.F.);
#17560=ORIENTED_EDGE('',*,*,#13155,.F.);
#17561=ORIENTED_EDGE('',*,*,#13128,.F.);
#17562=ORIENTED_EDGE('',*,*,#13155,.T.);
#17563=ORIENTED_EDGE('',*,*,#13156,.F.);
#17564=ORIENTED_EDGE('',*,*,#13157,.F.);
#17565=ORIENTED_EDGE('',*,*,#13129,.F.);
#17566=ORIENTED_EDGE('',*,*,#13157,.T.);
#17567=ORIENTED_EDGE('',*,*,#13158,.F.);
#17568=ORIENTED_EDGE('',*,*,#13159,.F.);
#17569=ORIENTED_EDGE('',*,*,#13130,.F.);
#17570=ORIENTED_EDGE('',*,*,#13159,.T.);
#17571=ORIENTED_EDGE('',*,*,#13160,.F.);
#17572=ORIENTED_EDGE('',*,*,#13161,.F.);
#17573=ORIENTED_EDGE('',*,*,#13131,.F.);
#17574=ORIENTED_EDGE('',*,*,#13161,.T.);
#17575=ORIENTED_EDGE('',*,*,#13162,.F.);
#17576=ORIENTED_EDGE('',*,*,#13163,.F.);
#17577=ORIENTED_EDGE('',*,*,#13132,.F.);
#17578=ORIENTED_EDGE('',*,*,#13163,.T.);
#17579=ORIENTED_EDGE('',*,*,#13164,.F.);
#17580=ORIENTED_EDGE('',*,*,#13165,.F.);
#17581=ORIENTED_EDGE('',*,*,#13133,.F.);
#17582=ORIENTED_EDGE('',*,*,#13165,.T.);
#17583=ORIENTED_EDGE('',*,*,#13166,.F.);
#17584=ORIENTED_EDGE('',*,*,#13167,.F.);
#17585=ORIENTED_EDGE('',*,*,#13134,.F.);
#17586=ORIENTED_EDGE('',*,*,#13167,.T.);
#17587=ORIENTED_EDGE('',*,*,#13168,.F.);
#17588=ORIENTED_EDGE('',*,*,#13169,.F.);
#17589=ORIENTED_EDGE('',*,*,#13135,.F.);
#17590=ORIENTED_EDGE('',*,*,#13169,.T.);
#17591=ORIENTED_EDGE('',*,*,#13170,.F.);
#17592=ORIENTED_EDGE('',*,*,#13171,.F.);
#17593=ORIENTED_EDGE('',*,*,#13136,.F.);
#17594=ORIENTED_EDGE('',*,*,#13171,.T.);
#17595=ORIENTED_EDGE('',*,*,#13172,.F.);
#17596=ORIENTED_EDGE('',*,*,#13173,.F.);
#17597=ORIENTED_EDGE('',*,*,#13137,.F.);
#17598=ORIENTED_EDGE('',*,*,#13173,.T.);
#17599=ORIENTED_EDGE('',*,*,#13174,.F.);
#17600=ORIENTED_EDGE('',*,*,#13175,.F.);
#17601=ORIENTED_EDGE('',*,*,#13138,.F.);
#17602=ORIENTED_EDGE('',*,*,#13175,.T.);
#17603=ORIENTED_EDGE('',*,*,#13176,.F.);
#17604=ORIENTED_EDGE('',*,*,#13177,.F.);
#17605=ORIENTED_EDGE('',*,*,#13139,.F.);
#17606=ORIENTED_EDGE('',*,*,#13177,.T.);
#17607=ORIENTED_EDGE('',*,*,#13178,.F.);
#17608=ORIENTED_EDGE('',*,*,#13179,.F.);
#17609=ORIENTED_EDGE('',*,*,#13140,.F.);
#17610=ORIENTED_EDGE('',*,*,#13179,.T.);
#17611=ORIENTED_EDGE('',*,*,#13180,.F.);
#17612=ORIENTED_EDGE('',*,*,#13181,.F.);
#17613=ORIENTED_EDGE('',*,*,#13141,.F.);
#17614=ORIENTED_EDGE('',*,*,#13181,.T.);
#17615=ORIENTED_EDGE('',*,*,#13182,.F.);
#17616=ORIENTED_EDGE('',*,*,#13183,.F.);
#17617=ORIENTED_EDGE('',*,*,#13142,.F.);
#17618=ORIENTED_EDGE('',*,*,#13183,.T.);
#17619=ORIENTED_EDGE('',*,*,#13184,.F.);
#17620=ORIENTED_EDGE('',*,*,#13185,.F.);
#17621=ORIENTED_EDGE('',*,*,#13143,.F.);
#17622=ORIENTED_EDGE('',*,*,#13185,.T.);
#17623=ORIENTED_EDGE('',*,*,#13186,.F.);
#17624=ORIENTED_EDGE('',*,*,#13187,.F.);
#17625=ORIENTED_EDGE('',*,*,#13144,.F.);
#17626=ORIENTED_EDGE('',*,*,#13187,.T.);
#17627=ORIENTED_EDGE('',*,*,#13188,.F.);
#17628=ORIENTED_EDGE('',*,*,#13189,.F.);
#17629=ORIENTED_EDGE('',*,*,#13145,.F.);
#17630=ORIENTED_EDGE('',*,*,#13189,.T.);
#17631=ORIENTED_EDGE('',*,*,#13190,.F.);
#17632=ORIENTED_EDGE('',*,*,#13191,.F.);
#17633=ORIENTED_EDGE('',*,*,#13146,.F.);
#17634=ORIENTED_EDGE('',*,*,#13191,.T.);
#17635=ORIENTED_EDGE('',*,*,#13192,.F.);
#17636=ORIENTED_EDGE('',*,*,#13193,.F.);
#17637=ORIENTED_EDGE('',*,*,#13147,.F.);
#17638=ORIENTED_EDGE('',*,*,#13193,.T.);
#17639=ORIENTED_EDGE('',*,*,#13194,.F.);
#17640=ORIENTED_EDGE('',*,*,#13195,.F.);
#17641=ORIENTED_EDGE('',*,*,#13148,.F.);
#17642=ORIENTED_EDGE('',*,*,#13195,.T.);
#17643=ORIENTED_EDGE('',*,*,#13196,.F.);
#17644=ORIENTED_EDGE('',*,*,#13197,.F.);
#17645=ORIENTED_EDGE('',*,*,#13149,.F.);
#17646=ORIENTED_EDGE('',*,*,#13197,.T.);
#17647=ORIENTED_EDGE('',*,*,#13198,.F.);
#17648=ORIENTED_EDGE('',*,*,#13199,.F.);
#17649=ORIENTED_EDGE('',*,*,#13150,.F.);
#17650=ORIENTED_EDGE('',*,*,#13199,.T.);
#17651=ORIENTED_EDGE('',*,*,#13200,.F.);
#17652=ORIENTED_EDGE('',*,*,#13151,.T.);
#17653=ORIENTED_EDGE('',*,*,#13126,.F.);
#17654=ORIENTED_EDGE('',*,*,#13200,.T.);
#17655=ORIENTED_EDGE('',*,*,#13198,.T.);
#17656=ORIENTED_EDGE('',*,*,#13196,.T.);
#17657=ORIENTED_EDGE('',*,*,#13194,.T.);
#17658=ORIENTED_EDGE('',*,*,#13192,.T.);
#17659=ORIENTED_EDGE('',*,*,#13190,.T.);
#17660=ORIENTED_EDGE('',*,*,#13188,.T.);
#17661=ORIENTED_EDGE('',*,*,#13186,.T.);
#17662=ORIENTED_EDGE('',*,*,#13184,.T.);
#17663=ORIENTED_EDGE('',*,*,#13182,.T.);
#17664=ORIENTED_EDGE('',*,*,#13180,.T.);
#17665=ORIENTED_EDGE('',*,*,#13178,.T.);
#17666=ORIENTED_EDGE('',*,*,#13176,.T.);
#17667=ORIENTED_EDGE('',*,*,#13174,.T.);
#17668=ORIENTED_EDGE('',*,*,#13172,.T.);
#17669=ORIENTED_EDGE('',*,*,#13170,.T.);
#17670=ORIENTED_EDGE('',*,*,#13168,.T.);
#17671=ORIENTED_EDGE('',*,*,#13166,.T.);
#17672=ORIENTED_EDGE('',*,*,#13164,.T.);
#17673=ORIENTED_EDGE('',*,*,#13162,.T.);
#17674=ORIENTED_EDGE('',*,*,#13160,.T.);
#17675=ORIENTED_EDGE('',*,*,#13158,.T.);
#17676=ORIENTED_EDGE('',*,*,#13156,.T.);
#17677=ORIENTED_EDGE('',*,*,#13154,.T.);
#17678=ORIENTED_EDGE('',*,*,#13152,.T.);
#17679=ORIENTED_EDGE('',*,*,#13201,.T.);
#17680=ORIENTED_EDGE('',*,*,#13202,.T.);
#17681=ORIENTED_EDGE('',*,*,#13203,.T.);
#17682=ORIENTED_EDGE('',*,*,#13204,.T.);
#17683=ORIENTED_EDGE('',*,*,#13205,.T.);
#17684=ORIENTED_EDGE('',*,*,#13206,.T.);
#17685=ORIENTED_EDGE('',*,*,#13207,.T.);
#17686=ORIENTED_EDGE('',*,*,#13208,.T.);
#17687=ORIENTED_EDGE('',*,*,#13209,.T.);
#17688=ORIENTED_EDGE('',*,*,#13210,.T.);
#17689=ORIENTED_EDGE('',*,*,#13211,.T.);
#17690=ORIENTED_EDGE('',*,*,#13212,.T.);
#17691=ORIENTED_EDGE('',*,*,#13213,.T.);
#17692=ORIENTED_EDGE('',*,*,#13214,.T.);
#17693=ORIENTED_EDGE('',*,*,#13215,.T.);
#17694=ORIENTED_EDGE('',*,*,#13216,.T.);
#17695=ORIENTED_EDGE('',*,*,#13217,.T.);
#17696=ORIENTED_EDGE('',*,*,#13218,.T.);
#17697=ORIENTED_EDGE('',*,*,#13219,.T.);
#17698=ORIENTED_EDGE('',*,*,#13220,.T.);
#17699=ORIENTED_EDGE('',*,*,#13221,.T.);
#17700=ORIENTED_EDGE('',*,*,#13222,.T.);
#17701=ORIENTED_EDGE('',*,*,#13223,.T.);
#17702=ORIENTED_EDGE('',*,*,#13224,.T.);
#17703=ORIENTED_EDGE('',*,*,#13225,.T.);
#17704=ORIENTED_EDGE('',*,*,#13226,.T.);
#17705=ORIENTED_EDGE('',*,*,#13227,.F.);
#17706=ORIENTED_EDGE('',*,*,#13228,.F.);
#17707=ORIENTED_EDGE('',*,*,#13229,.F.);
#17708=ORIENTED_EDGE('',*,*,#13202,.F.);
#17709=ORIENTED_EDGE('',*,*,#13229,.T.);
#17710=ORIENTED_EDGE('',*,*,#13230,.F.);
#17711=ORIENTED_EDGE('',*,*,#13231,.F.);
#17712=ORIENTED_EDGE('',*,*,#13203,.F.);
#17713=ORIENTED_EDGE('',*,*,#13231,.T.);
#17714=ORIENTED_EDGE('',*,*,#13232,.F.);
#17715=ORIENTED_EDGE('',*,*,#13233,.F.);
#17716=ORIENTED_EDGE('',*,*,#13204,.F.);
#17717=ORIENTED_EDGE('',*,*,#13233,.T.);
#17718=ORIENTED_EDGE('',*,*,#13234,.F.);
#17719=ORIENTED_EDGE('',*,*,#13235,.F.);
#17720=ORIENTED_EDGE('',*,*,#13205,.F.);
#17721=ORIENTED_EDGE('',*,*,#13235,.T.);
#17722=ORIENTED_EDGE('',*,*,#13236,.F.);
#17723=ORIENTED_EDGE('',*,*,#13237,.F.);
#17724=ORIENTED_EDGE('',*,*,#13206,.F.);
#17725=ORIENTED_EDGE('',*,*,#13237,.T.);
#17726=ORIENTED_EDGE('',*,*,#13238,.F.);
#17727=ORIENTED_EDGE('',*,*,#13239,.F.);
#17728=ORIENTED_EDGE('',*,*,#13207,.F.);
#17729=ORIENTED_EDGE('',*,*,#13239,.T.);
#17730=ORIENTED_EDGE('',*,*,#13240,.F.);
#17731=ORIENTED_EDGE('',*,*,#13241,.F.);
#17732=ORIENTED_EDGE('',*,*,#13208,.F.);
#17733=ORIENTED_EDGE('',*,*,#13241,.T.);
#17734=ORIENTED_EDGE('',*,*,#13242,.F.);
#17735=ORIENTED_EDGE('',*,*,#13243,.F.);
#17736=ORIENTED_EDGE('',*,*,#13209,.F.);
#17737=ORIENTED_EDGE('',*,*,#13243,.T.);
#17738=ORIENTED_EDGE('',*,*,#13244,.F.);
#17739=ORIENTED_EDGE('',*,*,#13245,.F.);
#17740=ORIENTED_EDGE('',*,*,#13210,.F.);
#17741=ORIENTED_EDGE('',*,*,#13245,.T.);
#17742=ORIENTED_EDGE('',*,*,#13246,.F.);
#17743=ORIENTED_EDGE('',*,*,#13247,.F.);
#17744=ORIENTED_EDGE('',*,*,#13211,.F.);
#17745=ORIENTED_EDGE('',*,*,#13247,.T.);
#17746=ORIENTED_EDGE('',*,*,#13248,.F.);
#17747=ORIENTED_EDGE('',*,*,#13249,.F.);
#17748=ORIENTED_EDGE('',*,*,#13212,.F.);
#17749=ORIENTED_EDGE('',*,*,#13249,.T.);
#17750=ORIENTED_EDGE('',*,*,#13250,.F.);
#17751=ORIENTED_EDGE('',*,*,#13251,.F.);
#17752=ORIENTED_EDGE('',*,*,#13213,.F.);
#17753=ORIENTED_EDGE('',*,*,#13251,.T.);
#17754=ORIENTED_EDGE('',*,*,#13252,.F.);
#17755=ORIENTED_EDGE('',*,*,#13253,.F.);
#17756=ORIENTED_EDGE('',*,*,#13214,.F.);
#17757=ORIENTED_EDGE('',*,*,#13253,.T.);
#17758=ORIENTED_EDGE('',*,*,#13254,.F.);
#17759=ORIENTED_EDGE('',*,*,#13255,.F.);
#17760=ORIENTED_EDGE('',*,*,#13215,.F.);
#17761=ORIENTED_EDGE('',*,*,#13255,.T.);
#17762=ORIENTED_EDGE('',*,*,#13256,.F.);
#17763=ORIENTED_EDGE('',*,*,#13257,.F.);
#17764=ORIENTED_EDGE('',*,*,#13216,.F.);
#17765=ORIENTED_EDGE('',*,*,#13257,.T.);
#17766=ORIENTED_EDGE('',*,*,#13258,.F.);
#17767=ORIENTED_EDGE('',*,*,#13259,.F.);
#17768=ORIENTED_EDGE('',*,*,#13217,.F.);
#17769=ORIENTED_EDGE('',*,*,#13259,.T.);
#17770=ORIENTED_EDGE('',*,*,#13260,.F.);
#17771=ORIENTED_EDGE('',*,*,#13261,.F.);
#17772=ORIENTED_EDGE('',*,*,#13218,.F.);
#17773=ORIENTED_EDGE('',*,*,#13261,.T.);
#17774=ORIENTED_EDGE('',*,*,#13262,.F.);
#17775=ORIENTED_EDGE('',*,*,#13263,.F.);
#17776=ORIENTED_EDGE('',*,*,#13219,.F.);
#17777=ORIENTED_EDGE('',*,*,#13263,.T.);
#17778=ORIENTED_EDGE('',*,*,#13264,.F.);
#17779=ORIENTED_EDGE('',*,*,#13265,.F.);
#17780=ORIENTED_EDGE('',*,*,#13220,.F.);
#17781=ORIENTED_EDGE('',*,*,#13265,.T.);
#17782=ORIENTED_EDGE('',*,*,#13266,.F.);
#17783=ORIENTED_EDGE('',*,*,#13267,.F.);
#17784=ORIENTED_EDGE('',*,*,#13221,.F.);
#17785=ORIENTED_EDGE('',*,*,#13267,.T.);
#17786=ORIENTED_EDGE('',*,*,#13268,.F.);
#17787=ORIENTED_EDGE('',*,*,#13269,.F.);
#17788=ORIENTED_EDGE('',*,*,#13222,.F.);
#17789=ORIENTED_EDGE('',*,*,#13269,.T.);
#17790=ORIENTED_EDGE('',*,*,#13270,.F.);
#17791=ORIENTED_EDGE('',*,*,#13271,.F.);
#17792=ORIENTED_EDGE('',*,*,#13223,.F.);
#17793=ORIENTED_EDGE('',*,*,#13271,.T.);
#17794=ORIENTED_EDGE('',*,*,#13272,.F.);
#17795=ORIENTED_EDGE('',*,*,#13273,.F.);
#17796=ORIENTED_EDGE('',*,*,#13224,.F.);
#17797=ORIENTED_EDGE('',*,*,#13273,.T.);
#17798=ORIENTED_EDGE('',*,*,#13274,.F.);
#17799=ORIENTED_EDGE('',*,*,#13275,.F.);
#17800=ORIENTED_EDGE('',*,*,#13225,.F.);
#17801=ORIENTED_EDGE('',*,*,#13275,.T.);
#17802=ORIENTED_EDGE('',*,*,#13276,.F.);
#17803=ORIENTED_EDGE('',*,*,#13277,.F.);
#17804=ORIENTED_EDGE('',*,*,#13226,.F.);
#17805=ORIENTED_EDGE('',*,*,#13277,.T.);
#17806=ORIENTED_EDGE('',*,*,#13278,.F.);
#17807=ORIENTED_EDGE('',*,*,#13227,.T.);
#17808=ORIENTED_EDGE('',*,*,#13201,.F.);
#17809=ORIENTED_EDGE('',*,*,#13278,.T.);
#17810=ORIENTED_EDGE('',*,*,#13276,.T.);
#17811=ORIENTED_EDGE('',*,*,#13274,.T.);
#17812=ORIENTED_EDGE('',*,*,#13272,.T.);
#17813=ORIENTED_EDGE('',*,*,#13270,.T.);
#17814=ORIENTED_EDGE('',*,*,#13268,.T.);
#17815=ORIENTED_EDGE('',*,*,#13266,.T.);
#17816=ORIENTED_EDGE('',*,*,#13264,.T.);
#17817=ORIENTED_EDGE('',*,*,#13262,.T.);
#17818=ORIENTED_EDGE('',*,*,#13260,.T.);
#17819=ORIENTED_EDGE('',*,*,#13258,.T.);
#17820=ORIENTED_EDGE('',*,*,#13256,.T.);
#17821=ORIENTED_EDGE('',*,*,#13254,.T.);
#17822=ORIENTED_EDGE('',*,*,#13252,.T.);
#17823=ORIENTED_EDGE('',*,*,#13250,.T.);
#17824=ORIENTED_EDGE('',*,*,#13248,.T.);
#17825=ORIENTED_EDGE('',*,*,#13246,.T.);
#17826=ORIENTED_EDGE('',*,*,#13244,.T.);
#17827=ORIENTED_EDGE('',*,*,#13242,.T.);
#17828=ORIENTED_EDGE('',*,*,#13240,.T.);
#17829=ORIENTED_EDGE('',*,*,#13238,.T.);
#17830=ORIENTED_EDGE('',*,*,#13236,.T.);
#17831=ORIENTED_EDGE('',*,*,#13234,.T.);
#17832=ORIENTED_EDGE('',*,*,#13232,.T.);
#17833=ORIENTED_EDGE('',*,*,#13230,.T.);
#17834=ORIENTED_EDGE('',*,*,#13228,.T.);
#17835=ORIENTED_EDGE('',*,*,#13279,.T.);
#17836=ORIENTED_EDGE('',*,*,#13280,.T.);
#17837=ORIENTED_EDGE('',*,*,#13281,.F.);
#17838=ORIENTED_EDGE('',*,*,#13282,.F.);
#17839=ORIENTED_EDGE('',*,*,#13283,.T.);
#17840=ORIENTED_EDGE('',*,*,#13284,.T.);
#17841=ORIENTED_EDGE('',*,*,#13285,.T.);
#17842=ORIENTED_EDGE('',*,*,#13279,.F.);
#17843=ORIENTED_EDGE('',*,*,#13286,.F.);
#17844=ORIENTED_EDGE('',*,*,#13287,.F.);
#17845=ORIENTED_EDGE('',*,*,#13288,.T.);
#17846=ORIENTED_EDGE('',*,*,#13289,.T.);
#17847=ORIENTED_EDGE('',*,*,#13290,.T.);
#17848=ORIENTED_EDGE('',*,*,#13283,.F.);
#17849=ORIENTED_EDGE('',*,*,#13291,.F.);
#17850=ORIENTED_EDGE('',*,*,#13292,.F.);
#17851=ORIENTED_EDGE('',*,*,#13293,.F.);
#17852=ORIENTED_EDGE('',*,*,#13294,.F.);
#17853=ORIENTED_EDGE('',*,*,#13295,.F.);
#17854=ORIENTED_EDGE('',*,*,#13296,.F.);
#17855=ORIENTED_EDGE('',*,*,#13297,.T.);
#17856=ORIENTED_EDGE('',*,*,#13298,.T.);
#17857=ORIENTED_EDGE('',*,*,#13299,.T.);
#17858=ORIENTED_EDGE('',*,*,#13300,.T.);
#17859=ORIENTED_EDGE('',*,*,#13301,.F.);
#17860=ORIENTED_EDGE('',*,*,#13302,.F.);
#17861=ORIENTED_EDGE('',*,*,#13303,.T.);
#17862=ORIENTED_EDGE('',*,*,#13304,.T.);
#17863=ORIENTED_EDGE('',*,*,#13305,.T.);
#17864=ORIENTED_EDGE('',*,*,#13299,.F.);
#17865=ORIENTED_EDGE('',*,*,#13306,.F.);
#17866=ORIENTED_EDGE('',*,*,#13307,.F.);
#17867=ORIENTED_EDGE('',*,*,#13308,.T.);
#17868=ORIENTED_EDGE('',*,*,#13309,.T.);
#17869=ORIENTED_EDGE('',*,*,#13310,.T.);
#17870=ORIENTED_EDGE('',*,*,#13303,.F.);
#17871=ORIENTED_EDGE('',*,*,#13311,.F.);
#17872=ORIENTED_EDGE('',*,*,#13312,.F.);
#17873=ORIENTED_EDGE('',*,*,#13313,.F.);
#17874=ORIENTED_EDGE('',*,*,#13314,.F.);
#17875=ORIENTED_EDGE('',*,*,#13315,.F.);
#17876=ORIENTED_EDGE('',*,*,#13316,.F.);
#17877=ORIENTED_EDGE('',*,*,#13317,.T.);
#17878=ORIENTED_EDGE('',*,*,#13318,.T.);
#17879=ORIENTED_EDGE('',*,*,#13319,.T.);
#17880=ORIENTED_EDGE('',*,*,#13320,.T.);
#17881=ORIENTED_EDGE('',*,*,#13321,.T.);
#17882=ORIENTED_EDGE('',*,*,#13322,.F.);
#17883=ORIENTED_EDGE('',*,*,#13323,.F.);
#17884=ORIENTED_EDGE('',*,*,#13324,.F.);
#17885=ORIENTED_EDGE('',*,*,#13325,.T.);
#17886=ORIENTED_EDGE('',*,*,#13326,.T.);
#17887=ORIENTED_EDGE('',*,*,#13327,.T.);
#17888=ORIENTED_EDGE('',*,*,#13319,.F.);
#17889=ORIENTED_EDGE('',*,*,#13328,.F.);
#17890=ORIENTED_EDGE('',*,*,#13329,.F.);
#17891=ORIENTED_EDGE('',*,*,#13330,.T.);
#17892=ORIENTED_EDGE('',*,*,#13331,.T.);
#17893=ORIENTED_EDGE('',*,*,#13332,.T.);
#17894=ORIENTED_EDGE('',*,*,#13325,.F.);
#17895=ORIENTED_EDGE('',*,*,#13333,.F.);
#17896=ORIENTED_EDGE('',*,*,#13334,.F.);
#17897=ORIENTED_EDGE('',*,*,#13335,.T.);
#17898=ORIENTED_EDGE('',*,*,#13336,.T.);
#17899=ORIENTED_EDGE('',*,*,#13337,.T.);
#17900=ORIENTED_EDGE('',*,*,#13330,.F.);
#17901=ORIENTED_EDGE('',*,*,#13338,.F.);
#17902=ORIENTED_EDGE('',*,*,#13339,.F.);
#17903=ORIENTED_EDGE('',*,*,#13340,.T.);
#17904=ORIENTED_EDGE('',*,*,#13341,.T.);
#17905=ORIENTED_EDGE('',*,*,#13342,.T.);
#17906=ORIENTED_EDGE('',*,*,#13335,.F.);
#17907=ORIENTED_EDGE('',*,*,#13343,.F.);
#17908=ORIENTED_EDGE('',*,*,#13344,.F.);
#17909=ORIENTED_EDGE('',*,*,#13345,.T.);
#17910=ORIENTED_EDGE('',*,*,#13346,.T.);
#17911=ORIENTED_EDGE('',*,*,#13347,.T.);
#17912=ORIENTED_EDGE('',*,*,#13340,.F.);
#17913=ORIENTED_EDGE('',*,*,#13348,.F.);
#17914=ORIENTED_EDGE('',*,*,#13349,.F.);
#17915=ORIENTED_EDGE('',*,*,#13350,.T.);
#17916=ORIENTED_EDGE('',*,*,#13351,.T.);
#17917=ORIENTED_EDGE('',*,*,#13352,.T.);
#17918=ORIENTED_EDGE('',*,*,#13345,.F.);
#17919=ORIENTED_EDGE('',*,*,#13353,.F.);
#17920=ORIENTED_EDGE('',*,*,#13354,.F.);
#17921=ORIENTED_EDGE('',*,*,#13355,.T.);
#17922=ORIENTED_EDGE('',*,*,#13356,.T.);
#17923=ORIENTED_EDGE('',*,*,#13357,.T.);
#17924=ORIENTED_EDGE('',*,*,#13350,.F.);
#17925=ORIENTED_EDGE('',*,*,#13358,.F.);
#17926=ORIENTED_EDGE('',*,*,#13359,.F.);
#17927=ORIENTED_EDGE('',*,*,#13360,.T.);
#17928=ORIENTED_EDGE('',*,*,#13361,.T.);
#17929=ORIENTED_EDGE('',*,*,#13362,.T.);
#17930=ORIENTED_EDGE('',*,*,#13355,.F.);
#17931=ORIENTED_EDGE('',*,*,#13363,.F.);
#17932=ORIENTED_EDGE('',*,*,#13364,.F.);
#17933=ORIENTED_EDGE('',*,*,#13365,.T.);
#17934=ORIENTED_EDGE('',*,*,#13366,.T.);
#17935=ORIENTED_EDGE('',*,*,#13367,.T.);
#17936=ORIENTED_EDGE('',*,*,#13360,.F.);
#17937=ORIENTED_EDGE('',*,*,#13368,.F.);
#17938=ORIENTED_EDGE('',*,*,#13369,.F.);
#17939=ORIENTED_EDGE('',*,*,#13370,.T.);
#17940=ORIENTED_EDGE('',*,*,#13371,.T.);
#17941=ORIENTED_EDGE('',*,*,#13372,.T.);
#17942=ORIENTED_EDGE('',*,*,#13365,.F.);
#17943=ORIENTED_EDGE('',*,*,#13373,.F.);
#17944=ORIENTED_EDGE('',*,*,#13374,.F.);
#17945=ORIENTED_EDGE('',*,*,#13375,.T.);
#17946=ORIENTED_EDGE('',*,*,#13376,.T.);
#17947=ORIENTED_EDGE('',*,*,#13377,.T.);
#17948=ORIENTED_EDGE('',*,*,#13370,.F.);
#17949=ORIENTED_EDGE('',*,*,#13378,.F.);
#17950=ORIENTED_EDGE('',*,*,#13379,.F.);
#17951=ORIENTED_EDGE('',*,*,#13380,.T.);
#17952=ORIENTED_EDGE('',*,*,#13381,.T.);
#17953=ORIENTED_EDGE('',*,*,#13382,.T.);
#17954=ORIENTED_EDGE('',*,*,#13375,.F.);
#17955=ORIENTED_EDGE('',*,*,#13383,.F.);
#17956=ORIENTED_EDGE('',*,*,#13384,.F.);
#17957=ORIENTED_EDGE('',*,*,#13385,.T.);
#17958=ORIENTED_EDGE('',*,*,#13386,.T.);
#17959=ORIENTED_EDGE('',*,*,#13387,.T.);
#17960=ORIENTED_EDGE('',*,*,#13380,.F.);
#17961=ORIENTED_EDGE('',*,*,#13388,.F.);
#17962=ORIENTED_EDGE('',*,*,#13389,.F.);
#17963=ORIENTED_EDGE('',*,*,#13390,.T.);
#17964=ORIENTED_EDGE('',*,*,#13391,.T.);
#17965=ORIENTED_EDGE('',*,*,#13392,.T.);
#17966=ORIENTED_EDGE('',*,*,#13385,.F.);
#17967=ORIENTED_EDGE('',*,*,#13393,.F.);
#17968=ORIENTED_EDGE('',*,*,#13394,.F.);
#17969=ORIENTED_EDGE('',*,*,#13395,.T.);
#17970=ORIENTED_EDGE('',*,*,#13396,.T.);
#17971=ORIENTED_EDGE('',*,*,#13397,.T.);
#17972=ORIENTED_EDGE('',*,*,#13390,.F.);
#17973=ORIENTED_EDGE('',*,*,#13398,.F.);
#17974=ORIENTED_EDGE('',*,*,#13399,.F.);
#17975=ORIENTED_EDGE('',*,*,#13400,.T.);
#17976=ORIENTED_EDGE('',*,*,#13401,.T.);
#17977=ORIENTED_EDGE('',*,*,#13402,.T.);
#17978=ORIENTED_EDGE('',*,*,#13395,.F.);
#17979=ORIENTED_EDGE('',*,*,#13403,.F.);
#17980=ORIENTED_EDGE('',*,*,#13404,.F.);
#17981=ORIENTED_EDGE('',*,*,#13405,.T.);
#17982=ORIENTED_EDGE('',*,*,#13406,.T.);
#17983=ORIENTED_EDGE('',*,*,#13407,.T.);
#17984=ORIENTED_EDGE('',*,*,#13400,.F.);
#17985=ORIENTED_EDGE('',*,*,#13408,.F.);
#17986=ORIENTED_EDGE('',*,*,#13409,.F.);
#17987=ORIENTED_EDGE('',*,*,#13410,.T.);
#17988=ORIENTED_EDGE('',*,*,#13411,.T.);
#17989=ORIENTED_EDGE('',*,*,#13412,.T.);
#17990=ORIENTED_EDGE('',*,*,#13405,.F.);
#17991=ORIENTED_EDGE('',*,*,#13413,.F.);
#17992=ORIENTED_EDGE('',*,*,#13414,.F.);
#17993=ORIENTED_EDGE('',*,*,#13415,.T.);
#17994=ORIENTED_EDGE('',*,*,#13416,.T.);
#17995=ORIENTED_EDGE('',*,*,#13417,.T.);
#17996=ORIENTED_EDGE('',*,*,#13410,.F.);
#17997=ORIENTED_EDGE('',*,*,#13418,.F.);
#17998=ORIENTED_EDGE('',*,*,#13419,.F.);
#17999=ORIENTED_EDGE('',*,*,#13420,.T.);
#18000=ORIENTED_EDGE('',*,*,#13421,.T.);
#18001=ORIENTED_EDGE('',*,*,#13422,.T.);
#18002=ORIENTED_EDGE('',*,*,#13415,.F.);
#18003=ORIENTED_EDGE('',*,*,#13423,.F.);
#18004=ORIENTED_EDGE('',*,*,#13424,.F.);
#18005=ORIENTED_EDGE('',*,*,#13425,.T.);
#18006=ORIENTED_EDGE('',*,*,#13426,.T.);
#18007=ORIENTED_EDGE('',*,*,#13427,.T.);
#18008=ORIENTED_EDGE('',*,*,#13420,.F.);
#18009=ORIENTED_EDGE('',*,*,#13428,.F.);
#18010=ORIENTED_EDGE('',*,*,#13429,.F.);
#18011=ORIENTED_EDGE('',*,*,#13430,.T.);
#18012=ORIENTED_EDGE('',*,*,#13431,.T.);
#18013=ORIENTED_EDGE('',*,*,#13432,.T.);
#18014=ORIENTED_EDGE('',*,*,#13425,.F.);
#18015=ORIENTED_EDGE('',*,*,#13433,.F.);
#18016=ORIENTED_EDGE('',*,*,#13434,.F.);
#18017=ORIENTED_EDGE('',*,*,#13435,.T.);
#18018=ORIENTED_EDGE('',*,*,#13436,.T.);
#18019=ORIENTED_EDGE('',*,*,#13437,.T.);
#18020=ORIENTED_EDGE('',*,*,#13430,.F.);
#18021=ORIENTED_EDGE('',*,*,#13438,.F.);
#18022=ORIENTED_EDGE('',*,*,#13439,.F.);
#18023=ORIENTED_EDGE('',*,*,#13440,.T.);
#18024=ORIENTED_EDGE('',*,*,#13441,.T.);
#18025=ORIENTED_EDGE('',*,*,#13442,.T.);
#18026=ORIENTED_EDGE('',*,*,#13435,.F.);
#18027=ORIENTED_EDGE('',*,*,#13443,.F.);
#18028=ORIENTED_EDGE('',*,*,#13444,.F.);
#18029=ORIENTED_EDGE('',*,*,#13445,.T.);
#18030=ORIENTED_EDGE('',*,*,#13446,.T.);
#18031=ORIENTED_EDGE('',*,*,#13447,.T.);
#18032=ORIENTED_EDGE('',*,*,#13440,.F.);
#18033=ORIENTED_EDGE('',*,*,#13448,.F.);
#18034=ORIENTED_EDGE('',*,*,#13449,.F.);
#18035=ORIENTED_EDGE('',*,*,#13450,.F.);
#18036=ORIENTED_EDGE('',*,*,#13451,.F.);
#18037=ORIENTED_EDGE('',*,*,#13452,.F.);
#18038=ORIENTED_EDGE('',*,*,#13453,.F.);
#18039=ORIENTED_EDGE('',*,*,#13454,.T.);
#18040=ORIENTED_EDGE('',*,*,#13455,.T.);
#18041=ORIENTED_EDGE('',*,*,#13456,.T.);
#18042=ORIENTED_EDGE('',*,*,#13457,.T.);
#18043=ORIENTED_EDGE('',*,*,#13458,.T.);
#18044=ORIENTED_EDGE('',*,*,#13459,.F.);
#18045=ORIENTED_EDGE('',*,*,#13460,.F.);
#18046=ORIENTED_EDGE('',*,*,#13461,.F.);
#18047=ORIENTED_EDGE('',*,*,#13462,.T.);
#18048=ORIENTED_EDGE('',*,*,#13463,.T.);
#18049=ORIENTED_EDGE('',*,*,#13464,.T.);
#18050=ORIENTED_EDGE('',*,*,#13456,.F.);
#18051=ORIENTED_EDGE('',*,*,#13465,.F.);
#18052=ORIENTED_EDGE('',*,*,#13466,.F.);
#18053=ORIENTED_EDGE('',*,*,#13467,.T.);
#18054=ORIENTED_EDGE('',*,*,#13468,.T.);
#18055=ORIENTED_EDGE('',*,*,#13469,.T.);
#18056=ORIENTED_EDGE('',*,*,#13462,.F.);
#18057=ORIENTED_EDGE('',*,*,#13470,.F.);
#18058=ORIENTED_EDGE('',*,*,#13471,.F.);
#18059=ORIENTED_EDGE('',*,*,#13472,.T.);
#18060=ORIENTED_EDGE('',*,*,#13473,.T.);
#18061=ORIENTED_EDGE('',*,*,#13474,.T.);
#18062=ORIENTED_EDGE('',*,*,#13467,.F.);
#18063=ORIENTED_EDGE('',*,*,#13475,.F.);
#18064=ORIENTED_EDGE('',*,*,#13476,.F.);
#18065=ORIENTED_EDGE('',*,*,#13477,.T.);
#18066=ORIENTED_EDGE('',*,*,#13478,.T.);
#18067=ORIENTED_EDGE('',*,*,#13479,.T.);
#18068=ORIENTED_EDGE('',*,*,#13472,.F.);
#18069=ORIENTED_EDGE('',*,*,#13480,.F.);
#18070=ORIENTED_EDGE('',*,*,#13481,.F.);
#18071=ORIENTED_EDGE('',*,*,#13482,.T.);
#18072=ORIENTED_EDGE('',*,*,#13483,.T.);
#18073=ORIENTED_EDGE('',*,*,#13484,.T.);
#18074=ORIENTED_EDGE('',*,*,#13477,.F.);
#18075=ORIENTED_EDGE('',*,*,#13485,.F.);
#18076=ORIENTED_EDGE('',*,*,#13486,.F.);
#18077=ORIENTED_EDGE('',*,*,#13487,.T.);
#18078=ORIENTED_EDGE('',*,*,#13488,.T.);
#18079=ORIENTED_EDGE('',*,*,#13489,.T.);
#18080=ORIENTED_EDGE('',*,*,#13482,.F.);
#18081=ORIENTED_EDGE('',*,*,#13490,.F.);
#18082=ORIENTED_EDGE('',*,*,#13491,.F.);
#18083=ORIENTED_EDGE('',*,*,#13492,.T.);
#18084=ORIENTED_EDGE('',*,*,#13493,.T.);
#18085=ORIENTED_EDGE('',*,*,#13494,.T.);
#18086=ORIENTED_EDGE('',*,*,#13487,.F.);
#18087=ORIENTED_EDGE('',*,*,#13495,.F.);
#18088=ORIENTED_EDGE('',*,*,#13496,.F.);
#18089=ORIENTED_EDGE('',*,*,#13497,.T.);
#18090=ORIENTED_EDGE('',*,*,#13498,.T.);
#18091=ORIENTED_EDGE('',*,*,#13499,.T.);
#18092=ORIENTED_EDGE('',*,*,#13492,.F.);
#18093=ORIENTED_EDGE('',*,*,#13500,.F.);
#18094=ORIENTED_EDGE('',*,*,#13501,.F.);
#18095=ORIENTED_EDGE('',*,*,#13502,.T.);
#18096=ORIENTED_EDGE('',*,*,#13503,.T.);
#18097=ORIENTED_EDGE('',*,*,#13504,.T.);
#18098=ORIENTED_EDGE('',*,*,#13497,.F.);
#18099=ORIENTED_EDGE('',*,*,#13505,.F.);
#18100=ORIENTED_EDGE('',*,*,#13506,.F.);
#18101=ORIENTED_EDGE('',*,*,#13507,.T.);
#18102=ORIENTED_EDGE('',*,*,#13508,.T.);
#18103=ORIENTED_EDGE('',*,*,#13509,.T.);
#18104=ORIENTED_EDGE('',*,*,#13502,.F.);
#18105=ORIENTED_EDGE('',*,*,#13510,.F.);
#18106=ORIENTED_EDGE('',*,*,#13511,.F.);
#18107=ORIENTED_EDGE('',*,*,#13512,.T.);
#18108=ORIENTED_EDGE('',*,*,#13513,.T.);
#18109=ORIENTED_EDGE('',*,*,#13514,.T.);
#18110=ORIENTED_EDGE('',*,*,#13507,.F.);
#18111=ORIENTED_EDGE('',*,*,#13515,.F.);
#18112=ORIENTED_EDGE('',*,*,#13516,.F.);
#18113=ORIENTED_EDGE('',*,*,#13517,.T.);
#18114=ORIENTED_EDGE('',*,*,#13518,.T.);
#18115=ORIENTED_EDGE('',*,*,#13519,.T.);
#18116=ORIENTED_EDGE('',*,*,#13512,.F.);
#18117=ORIENTED_EDGE('',*,*,#13520,.F.);
#18118=ORIENTED_EDGE('',*,*,#13521,.F.);
#18119=ORIENTED_EDGE('',*,*,#13522,.T.);
#18120=ORIENTED_EDGE('',*,*,#13523,.T.);
#18121=ORIENTED_EDGE('',*,*,#13524,.T.);
#18122=ORIENTED_EDGE('',*,*,#13517,.F.);
#18123=ORIENTED_EDGE('',*,*,#13525,.F.);
#18124=ORIENTED_EDGE('',*,*,#13526,.F.);
#18125=ORIENTED_EDGE('',*,*,#13527,.T.);
#18126=ORIENTED_EDGE('',*,*,#13528,.T.);
#18127=ORIENTED_EDGE('',*,*,#13529,.T.);
#18128=ORIENTED_EDGE('',*,*,#13522,.F.);
#18129=ORIENTED_EDGE('',*,*,#13530,.F.);
#18130=ORIENTED_EDGE('',*,*,#13531,.F.);
#18131=ORIENTED_EDGE('',*,*,#13532,.T.);
#18132=ORIENTED_EDGE('',*,*,#13533,.T.);
#18133=ORIENTED_EDGE('',*,*,#13534,.T.);
#18134=ORIENTED_EDGE('',*,*,#13527,.F.);
#18135=ORIENTED_EDGE('',*,*,#13535,.F.);
#18136=ORIENTED_EDGE('',*,*,#13536,.F.);
#18137=ORIENTED_EDGE('',*,*,#13537,.T.);
#18138=ORIENTED_EDGE('',*,*,#13538,.T.);
#18139=ORIENTED_EDGE('',*,*,#13539,.T.);
#18140=ORIENTED_EDGE('',*,*,#13532,.F.);
#18141=ORIENTED_EDGE('',*,*,#13540,.F.);
#18142=ORIENTED_EDGE('',*,*,#13541,.F.);
#18143=ORIENTED_EDGE('',*,*,#13542,.T.);
#18144=ORIENTED_EDGE('',*,*,#13543,.T.);
#18145=ORIENTED_EDGE('',*,*,#13544,.T.);
#18146=ORIENTED_EDGE('',*,*,#13537,.F.);
#18147=ORIENTED_EDGE('',*,*,#13545,.F.);
#18148=ORIENTED_EDGE('',*,*,#13546,.F.);
#18149=ORIENTED_EDGE('',*,*,#13547,.T.);
#18150=ORIENTED_EDGE('',*,*,#13548,.T.);
#18151=ORIENTED_EDGE('',*,*,#13549,.T.);
#18152=ORIENTED_EDGE('',*,*,#13542,.F.);
#18153=ORIENTED_EDGE('',*,*,#13550,.F.);
#18154=ORIENTED_EDGE('',*,*,#13551,.F.);
#18155=ORIENTED_EDGE('',*,*,#13552,.T.);
#18156=ORIENTED_EDGE('',*,*,#13553,.T.);
#18157=ORIENTED_EDGE('',*,*,#13554,.T.);
#18158=ORIENTED_EDGE('',*,*,#13547,.F.);
#18159=ORIENTED_EDGE('',*,*,#13555,.F.);
#18160=ORIENTED_EDGE('',*,*,#13556,.F.);
#18161=ORIENTED_EDGE('',*,*,#13557,.T.);
#18162=ORIENTED_EDGE('',*,*,#13558,.T.);
#18163=ORIENTED_EDGE('',*,*,#13559,.T.);
#18164=ORIENTED_EDGE('',*,*,#13552,.F.);
#18165=ORIENTED_EDGE('',*,*,#13560,.F.);
#18166=ORIENTED_EDGE('',*,*,#13561,.F.);
#18167=ORIENTED_EDGE('',*,*,#13562,.T.);
#18168=ORIENTED_EDGE('',*,*,#13563,.T.);
#18169=ORIENTED_EDGE('',*,*,#13564,.T.);
#18170=ORIENTED_EDGE('',*,*,#13557,.F.);
#18171=ORIENTED_EDGE('',*,*,#13565,.F.);
#18172=ORIENTED_EDGE('',*,*,#13566,.F.);
#18173=ORIENTED_EDGE('',*,*,#13567,.T.);
#18174=ORIENTED_EDGE('',*,*,#13568,.T.);
#18175=ORIENTED_EDGE('',*,*,#13569,.T.);
#18176=ORIENTED_EDGE('',*,*,#13562,.F.);
#18177=ORIENTED_EDGE('',*,*,#13570,.F.);
#18178=ORIENTED_EDGE('',*,*,#13571,.F.);
#18179=ORIENTED_EDGE('',*,*,#13572,.T.);
#18180=ORIENTED_EDGE('',*,*,#13573,.T.);
#18181=ORIENTED_EDGE('',*,*,#13574,.T.);
#18182=ORIENTED_EDGE('',*,*,#13567,.F.);
#18183=ORIENTED_EDGE('',*,*,#13575,.F.);
#18184=ORIENTED_EDGE('',*,*,#13576,.F.);
#18185=ORIENTED_EDGE('',*,*,#13577,.T.);
#18186=ORIENTED_EDGE('',*,*,#13578,.T.);
#18187=ORIENTED_EDGE('',*,*,#13579,.T.);
#18188=ORIENTED_EDGE('',*,*,#13572,.F.);
#18189=ORIENTED_EDGE('',*,*,#13580,.F.);
#18190=ORIENTED_EDGE('',*,*,#13581,.F.);
#18191=ORIENTED_EDGE('',*,*,#13582,.T.);
#18192=ORIENTED_EDGE('',*,*,#13583,.T.);
#18193=ORIENTED_EDGE('',*,*,#13584,.T.);
#18194=ORIENTED_EDGE('',*,*,#13577,.F.);
#18195=ORIENTED_EDGE('',*,*,#13585,.F.);
#18196=ORIENTED_EDGE('',*,*,#13586,.F.);
#18197=ORIENTED_EDGE('',*,*,#13587,.F.);
#18198=ORIENTED_EDGE('',*,*,#13588,.F.);
#18199=ORIENTED_EDGE('',*,*,#13589,.F.);
#18200=ORIENTED_EDGE('',*,*,#13590,.F.);
#18201=ORIENTED_EDGE('',*,*,#13591,.T.);
#18202=ORIENTED_EDGE('',*,*,#13592,.T.);
#18203=ORIENTED_EDGE('',*,*,#13593,.T.);
#18204=ORIENTED_EDGE('',*,*,#13594,.T.);
#18205=ORIENTED_EDGE('',*,*,#13595,.T.);
#18206=ORIENTED_EDGE('',*,*,#13596,.F.);
#18207=ORIENTED_EDGE('',*,*,#13597,.F.);
#18208=ORIENTED_EDGE('',*,*,#13598,.F.);
#18209=ORIENTED_EDGE('',*,*,#13599,.T.);
#18210=ORIENTED_EDGE('',*,*,#13600,.T.);
#18211=ORIENTED_EDGE('',*,*,#13601,.T.);
#18212=ORIENTED_EDGE('',*,*,#13593,.F.);
#18213=ORIENTED_EDGE('',*,*,#13602,.F.);
#18214=ORIENTED_EDGE('',*,*,#13603,.F.);
#18215=ORIENTED_EDGE('',*,*,#13604,.T.);
#18216=ORIENTED_EDGE('',*,*,#13605,.T.);
#18217=ORIENTED_EDGE('',*,*,#13606,.T.);
#18218=ORIENTED_EDGE('',*,*,#13599,.F.);
#18219=ORIENTED_EDGE('',*,*,#13607,.F.);
#18220=ORIENTED_EDGE('',*,*,#13608,.F.);
#18221=ORIENTED_EDGE('',*,*,#13609,.T.);
#18222=ORIENTED_EDGE('',*,*,#13610,.T.);
#18223=ORIENTED_EDGE('',*,*,#13611,.T.);
#18224=ORIENTED_EDGE('',*,*,#13604,.F.);
#18225=ORIENTED_EDGE('',*,*,#13612,.F.);
#18226=ORIENTED_EDGE('',*,*,#13613,.F.);
#18227=ORIENTED_EDGE('',*,*,#13614,.T.);
#18228=ORIENTED_EDGE('',*,*,#13615,.T.);
#18229=ORIENTED_EDGE('',*,*,#13616,.T.);
#18230=ORIENTED_EDGE('',*,*,#13609,.F.);
#18231=ORIENTED_EDGE('',*,*,#13617,.F.);
#18232=ORIENTED_EDGE('',*,*,#13618,.F.);
#18233=ORIENTED_EDGE('',*,*,#13619,.T.);
#18234=ORIENTED_EDGE('',*,*,#13620,.T.);
#18235=ORIENTED_EDGE('',*,*,#13621,.T.);
#18236=ORIENTED_EDGE('',*,*,#13614,.F.);
#18237=ORIENTED_EDGE('',*,*,#13622,.F.);
#18238=ORIENTED_EDGE('',*,*,#13623,.F.);
#18239=ORIENTED_EDGE('',*,*,#13624,.T.);
#18240=ORIENTED_EDGE('',*,*,#13625,.T.);
#18241=ORIENTED_EDGE('',*,*,#13626,.T.);
#18242=ORIENTED_EDGE('',*,*,#13619,.F.);
#18243=ORIENTED_EDGE('',*,*,#13627,.F.);
#18244=ORIENTED_EDGE('',*,*,#13628,.F.);
#18245=ORIENTED_EDGE('',*,*,#13629,.T.);
#18246=ORIENTED_EDGE('',*,*,#13630,.T.);
#18247=ORIENTED_EDGE('',*,*,#13631,.T.);
#18248=ORIENTED_EDGE('',*,*,#13624,.F.);
#18249=ORIENTED_EDGE('',*,*,#13632,.F.);
#18250=ORIENTED_EDGE('',*,*,#13633,.F.);
#18251=ORIENTED_EDGE('',*,*,#13634,.T.);
#18252=ORIENTED_EDGE('',*,*,#13635,.T.);
#18253=ORIENTED_EDGE('',*,*,#13636,.T.);
#18254=ORIENTED_EDGE('',*,*,#13629,.F.);
#18255=ORIENTED_EDGE('',*,*,#13637,.F.);
#18256=ORIENTED_EDGE('',*,*,#13638,.F.);
#18257=ORIENTED_EDGE('',*,*,#13639,.T.);
#18258=ORIENTED_EDGE('',*,*,#13640,.T.);
#18259=ORIENTED_EDGE('',*,*,#13641,.T.);
#18260=ORIENTED_EDGE('',*,*,#13634,.F.);
#18261=ORIENTED_EDGE('',*,*,#13642,.F.);
#18262=ORIENTED_EDGE('',*,*,#13643,.F.);
#18263=ORIENTED_EDGE('',*,*,#13644,.T.);
#18264=ORIENTED_EDGE('',*,*,#13645,.T.);
#18265=ORIENTED_EDGE('',*,*,#13646,.T.);
#18266=ORIENTED_EDGE('',*,*,#13639,.F.);
#18267=ORIENTED_EDGE('',*,*,#13647,.F.);
#18268=ORIENTED_EDGE('',*,*,#13648,.F.);
#18269=ORIENTED_EDGE('',*,*,#13649,.T.);
#18270=ORIENTED_EDGE('',*,*,#13650,.T.);
#18271=ORIENTED_EDGE('',*,*,#13651,.T.);
#18272=ORIENTED_EDGE('',*,*,#13644,.F.);
#18273=ORIENTED_EDGE('',*,*,#13652,.F.);
#18274=ORIENTED_EDGE('',*,*,#13653,.F.);
#18275=ORIENTED_EDGE('',*,*,#13654,.T.);
#18276=ORIENTED_EDGE('',*,*,#13655,.T.);
#18277=ORIENTED_EDGE('',*,*,#13656,.T.);
#18278=ORIENTED_EDGE('',*,*,#13649,.F.);
#18279=ORIENTED_EDGE('',*,*,#13657,.F.);
#18280=ORIENTED_EDGE('',*,*,#13658,.F.);
#18281=ORIENTED_EDGE('',*,*,#13659,.T.);
#18282=ORIENTED_EDGE('',*,*,#13660,.T.);
#18283=ORIENTED_EDGE('',*,*,#13661,.T.);
#18284=ORIENTED_EDGE('',*,*,#13654,.F.);
#18285=ORIENTED_EDGE('',*,*,#13662,.F.);
#18286=ORIENTED_EDGE('',*,*,#13663,.F.);
#18287=ORIENTED_EDGE('',*,*,#13664,.T.);
#18288=ORIENTED_EDGE('',*,*,#13665,.T.);
#18289=ORIENTED_EDGE('',*,*,#13666,.T.);
#18290=ORIENTED_EDGE('',*,*,#13659,.F.);
#18291=ORIENTED_EDGE('',*,*,#13667,.F.);
#18292=ORIENTED_EDGE('',*,*,#13668,.F.);
#18293=ORIENTED_EDGE('',*,*,#13669,.T.);
#18294=ORIENTED_EDGE('',*,*,#13670,.T.);
#18295=ORIENTED_EDGE('',*,*,#13671,.T.);
#18296=ORIENTED_EDGE('',*,*,#13664,.F.);
#18297=ORIENTED_EDGE('',*,*,#13672,.F.);
#18298=ORIENTED_EDGE('',*,*,#13673,.F.);
#18299=ORIENTED_EDGE('',*,*,#13674,.T.);
#18300=ORIENTED_EDGE('',*,*,#13675,.T.);
#18301=ORIENTED_EDGE('',*,*,#13676,.T.);
#18302=ORIENTED_EDGE('',*,*,#13669,.F.);
#18303=ORIENTED_EDGE('',*,*,#13677,.F.);
#18304=ORIENTED_EDGE('',*,*,#13678,.F.);
#18305=ORIENTED_EDGE('',*,*,#13679,.T.);
#18306=ORIENTED_EDGE('',*,*,#13680,.T.);
#18307=ORIENTED_EDGE('',*,*,#13681,.T.);
#18308=ORIENTED_EDGE('',*,*,#13674,.F.);
#18309=ORIENTED_EDGE('',*,*,#13682,.F.);
#18310=ORIENTED_EDGE('',*,*,#13683,.F.);
#18311=ORIENTED_EDGE('',*,*,#13684,.T.);
#18312=ORIENTED_EDGE('',*,*,#13685,.T.);
#18313=ORIENTED_EDGE('',*,*,#13686,.T.);
#18314=ORIENTED_EDGE('',*,*,#13679,.F.);
#18315=ORIENTED_EDGE('',*,*,#13687,.F.);
#18316=ORIENTED_EDGE('',*,*,#13688,.F.);
#18317=ORIENTED_EDGE('',*,*,#13689,.T.);
#18318=ORIENTED_EDGE('',*,*,#13690,.T.);
#18319=ORIENTED_EDGE('',*,*,#13691,.T.);
#18320=ORIENTED_EDGE('',*,*,#13684,.F.);
#18321=ORIENTED_EDGE('',*,*,#13692,.F.);
#18322=ORIENTED_EDGE('',*,*,#13693,.F.);
#18323=ORIENTED_EDGE('',*,*,#13694,.T.);
#18324=ORIENTED_EDGE('',*,*,#13695,.T.);
#18325=ORIENTED_EDGE('',*,*,#13696,.T.);
#18326=ORIENTED_EDGE('',*,*,#13689,.F.);
#18327=ORIENTED_EDGE('',*,*,#13697,.F.);
#18328=ORIENTED_EDGE('',*,*,#13698,.F.);
#18329=ORIENTED_EDGE('',*,*,#13699,.T.);
#18330=ORIENTED_EDGE('',*,*,#13700,.T.);
#18331=ORIENTED_EDGE('',*,*,#13701,.T.);
#18332=ORIENTED_EDGE('',*,*,#13694,.F.);
#18333=ORIENTED_EDGE('',*,*,#13702,.F.);
#18334=ORIENTED_EDGE('',*,*,#13703,.F.);
#18335=ORIENTED_EDGE('',*,*,#13704,.T.);
#18336=ORIENTED_EDGE('',*,*,#13705,.T.);
#18337=ORIENTED_EDGE('',*,*,#13706,.T.);
#18338=ORIENTED_EDGE('',*,*,#13699,.F.);
#18339=ORIENTED_EDGE('',*,*,#13707,.F.);
#18340=ORIENTED_EDGE('',*,*,#13708,.F.);
#18341=ORIENTED_EDGE('',*,*,#13709,.T.);
#18342=ORIENTED_EDGE('',*,*,#13710,.T.);
#18343=ORIENTED_EDGE('',*,*,#13711,.T.);
#18344=ORIENTED_EDGE('',*,*,#13704,.F.);
#18345=ORIENTED_EDGE('',*,*,#13712,.F.);
#18346=ORIENTED_EDGE('',*,*,#13713,.F.);
#18347=ORIENTED_EDGE('',*,*,#13714,.T.);
#18348=ORIENTED_EDGE('',*,*,#13715,.T.);
#18349=ORIENTED_EDGE('',*,*,#13716,.T.);
#18350=ORIENTED_EDGE('',*,*,#13709,.F.);
#18351=ORIENTED_EDGE('',*,*,#13717,.F.);
#18352=ORIENTED_EDGE('',*,*,#13718,.F.);
#18353=ORIENTED_EDGE('',*,*,#13719,.T.);
#18354=ORIENTED_EDGE('',*,*,#13720,.T.);
#18355=ORIENTED_EDGE('',*,*,#13721,.T.);
#18356=ORIENTED_EDGE('',*,*,#13714,.F.);
#18357=ORIENTED_EDGE('',*,*,#13722,.F.);
#18358=ORIENTED_EDGE('',*,*,#13723,.F.);
#18359=ORIENTED_EDGE('',*,*,#13724,.F.);
#18360=ORIENTED_EDGE('',*,*,#13725,.F.);
#18361=ORIENTED_EDGE('',*,*,#13726,.F.);
#18362=ORIENTED_EDGE('',*,*,#13727,.F.);
#18363=ORIENTED_EDGE('',*,*,#13728,.T.);
#18364=ORIENTED_EDGE('',*,*,#13729,.T.);
#18365=ORIENTED_EDGE('',*,*,#13730,.T.);
#18366=ORIENTED_EDGE('',*,*,#13731,.T.);
#18367=ORIENTED_EDGE('',*,*,#13732,.T.);
#18368=ORIENTED_EDGE('',*,*,#13733,.F.);
#18369=ORIENTED_EDGE('',*,*,#13734,.F.);
#18370=ORIENTED_EDGE('',*,*,#13735,.F.);
#18371=ORIENTED_EDGE('',*,*,#13736,.T.);
#18372=ORIENTED_EDGE('',*,*,#13737,.T.);
#18373=ORIENTED_EDGE('',*,*,#13738,.T.);
#18374=ORIENTED_EDGE('',*,*,#13730,.F.);
#18375=ORIENTED_EDGE('',*,*,#13739,.F.);
#18376=ORIENTED_EDGE('',*,*,#13740,.F.);
#18377=ORIENTED_EDGE('',*,*,#13741,.T.);
#18378=ORIENTED_EDGE('',*,*,#13742,.T.);
#18379=ORIENTED_EDGE('',*,*,#13743,.T.);
#18380=ORIENTED_EDGE('',*,*,#13736,.F.);
#18381=ORIENTED_EDGE('',*,*,#13744,.F.);
#18382=ORIENTED_EDGE('',*,*,#13745,.F.);
#18383=ORIENTED_EDGE('',*,*,#13746,.T.);
#18384=ORIENTED_EDGE('',*,*,#13747,.T.);
#18385=ORIENTED_EDGE('',*,*,#13748,.T.);
#18386=ORIENTED_EDGE('',*,*,#13741,.F.);
#18387=ORIENTED_EDGE('',*,*,#13749,.F.);
#18388=ORIENTED_EDGE('',*,*,#13750,.F.);
#18389=ORIENTED_EDGE('',*,*,#13751,.T.);
#18390=ORIENTED_EDGE('',*,*,#13752,.T.);
#18391=ORIENTED_EDGE('',*,*,#13753,.T.);
#18392=ORIENTED_EDGE('',*,*,#13746,.F.);
#18393=ORIENTED_EDGE('',*,*,#13754,.F.);
#18394=ORIENTED_EDGE('',*,*,#13755,.F.);
#18395=ORIENTED_EDGE('',*,*,#13756,.T.);
#18396=ORIENTED_EDGE('',*,*,#13757,.T.);
#18397=ORIENTED_EDGE('',*,*,#13758,.T.);
#18398=ORIENTED_EDGE('',*,*,#13751,.F.);
#18399=ORIENTED_EDGE('',*,*,#13759,.F.);
#18400=ORIENTED_EDGE('',*,*,#13760,.F.);
#18401=ORIENTED_EDGE('',*,*,#13761,.T.);
#18402=ORIENTED_EDGE('',*,*,#13762,.T.);
#18403=ORIENTED_EDGE('',*,*,#13763,.T.);
#18404=ORIENTED_EDGE('',*,*,#13756,.F.);
#18405=ORIENTED_EDGE('',*,*,#13764,.F.);
#18406=ORIENTED_EDGE('',*,*,#13765,.F.);
#18407=ORIENTED_EDGE('',*,*,#13766,.T.);
#18408=ORIENTED_EDGE('',*,*,#13767,.T.);
#18409=ORIENTED_EDGE('',*,*,#13768,.T.);
#18410=ORIENTED_EDGE('',*,*,#13761,.F.);
#18411=ORIENTED_EDGE('',*,*,#13769,.F.);
#18412=ORIENTED_EDGE('',*,*,#13770,.F.);
#18413=ORIENTED_EDGE('',*,*,#13771,.T.);
#18414=ORIENTED_EDGE('',*,*,#13772,.T.);
#18415=ORIENTED_EDGE('',*,*,#13773,.T.);
#18416=ORIENTED_EDGE('',*,*,#13766,.F.);
#18417=ORIENTED_EDGE('',*,*,#13774,.F.);
#18418=ORIENTED_EDGE('',*,*,#13775,.F.);
#18419=ORIENTED_EDGE('',*,*,#13776,.T.);
#18420=ORIENTED_EDGE('',*,*,#13777,.T.);
#18421=ORIENTED_EDGE('',*,*,#13778,.T.);
#18422=ORIENTED_EDGE('',*,*,#13771,.F.);
#18423=ORIENTED_EDGE('',*,*,#13779,.F.);
#18424=ORIENTED_EDGE('',*,*,#13780,.F.);
#18425=ORIENTED_EDGE('',*,*,#13781,.T.);
#18426=ORIENTED_EDGE('',*,*,#13782,.T.);
#18427=ORIENTED_EDGE('',*,*,#13783,.T.);
#18428=ORIENTED_EDGE('',*,*,#13776,.F.);
#18429=ORIENTED_EDGE('',*,*,#13784,.F.);
#18430=ORIENTED_EDGE('',*,*,#13785,.F.);
#18431=ORIENTED_EDGE('',*,*,#13786,.T.);
#18432=ORIENTED_EDGE('',*,*,#13787,.T.);
#18433=ORIENTED_EDGE('',*,*,#13788,.T.);
#18434=ORIENTED_EDGE('',*,*,#13781,.F.);
#18435=ORIENTED_EDGE('',*,*,#13789,.F.);
#18436=ORIENTED_EDGE('',*,*,#13790,.F.);
#18437=ORIENTED_EDGE('',*,*,#13791,.T.);
#18438=ORIENTED_EDGE('',*,*,#13792,.T.);
#18439=ORIENTED_EDGE('',*,*,#13793,.T.);
#18440=ORIENTED_EDGE('',*,*,#13786,.F.);
#18441=ORIENTED_EDGE('',*,*,#13794,.F.);
#18442=ORIENTED_EDGE('',*,*,#13795,.F.);
#18443=ORIENTED_EDGE('',*,*,#13796,.T.);
#18444=ORIENTED_EDGE('',*,*,#13797,.T.);
#18445=ORIENTED_EDGE('',*,*,#13798,.T.);
#18446=ORIENTED_EDGE('',*,*,#13791,.F.);
#18447=ORIENTED_EDGE('',*,*,#13799,.F.);
#18448=ORIENTED_EDGE('',*,*,#13800,.F.);
#18449=ORIENTED_EDGE('',*,*,#13801,.T.);
#18450=ORIENTED_EDGE('',*,*,#13802,.T.);
#18451=ORIENTED_EDGE('',*,*,#13803,.T.);
#18452=ORIENTED_EDGE('',*,*,#13796,.F.);
#18453=ORIENTED_EDGE('',*,*,#13804,.F.);
#18454=ORIENTED_EDGE('',*,*,#13805,.F.);
#18455=ORIENTED_EDGE('',*,*,#13806,.T.);
#18456=ORIENTED_EDGE('',*,*,#13807,.T.);
#18457=ORIENTED_EDGE('',*,*,#13808,.T.);
#18458=ORIENTED_EDGE('',*,*,#13801,.F.);
#18459=ORIENTED_EDGE('',*,*,#13809,.F.);
#18460=ORIENTED_EDGE('',*,*,#13810,.F.);
#18461=ORIENTED_EDGE('',*,*,#13811,.T.);
#18462=ORIENTED_EDGE('',*,*,#13812,.T.);
#18463=ORIENTED_EDGE('',*,*,#13813,.T.);
#18464=ORIENTED_EDGE('',*,*,#13806,.F.);
#18465=ORIENTED_EDGE('',*,*,#13814,.F.);
#18466=ORIENTED_EDGE('',*,*,#13815,.F.);
#18467=ORIENTED_EDGE('',*,*,#13816,.T.);
#18468=ORIENTED_EDGE('',*,*,#13817,.T.);
#18469=ORIENTED_EDGE('',*,*,#13818,.T.);
#18470=ORIENTED_EDGE('',*,*,#13811,.F.);
#18471=ORIENTED_EDGE('',*,*,#13819,.F.);
#18472=ORIENTED_EDGE('',*,*,#13820,.F.);
#18473=ORIENTED_EDGE('',*,*,#13821,.T.);
#18474=ORIENTED_EDGE('',*,*,#13822,.T.);
#18475=ORIENTED_EDGE('',*,*,#13823,.T.);
#18476=ORIENTED_EDGE('',*,*,#13816,.F.);
#18477=ORIENTED_EDGE('',*,*,#13824,.F.);
#18478=ORIENTED_EDGE('',*,*,#13825,.F.);
#18479=ORIENTED_EDGE('',*,*,#13826,.T.);
#18480=ORIENTED_EDGE('',*,*,#13827,.T.);
#18481=ORIENTED_EDGE('',*,*,#13828,.T.);
#18482=ORIENTED_EDGE('',*,*,#13821,.F.);
#18483=ORIENTED_EDGE('',*,*,#13829,.F.);
#18484=ORIENTED_EDGE('',*,*,#13830,.F.);
#18485=ORIENTED_EDGE('',*,*,#13831,.T.);
#18486=ORIENTED_EDGE('',*,*,#13832,.T.);
#18487=ORIENTED_EDGE('',*,*,#13833,.T.);
#18488=ORIENTED_EDGE('',*,*,#13826,.F.);
#18489=ORIENTED_EDGE('',*,*,#13834,.F.);
#18490=ORIENTED_EDGE('',*,*,#13835,.F.);
#18491=ORIENTED_EDGE('',*,*,#13836,.T.);
#18492=ORIENTED_EDGE('',*,*,#13837,.T.);
#18493=ORIENTED_EDGE('',*,*,#13838,.T.);
#18494=ORIENTED_EDGE('',*,*,#13831,.F.);
#18495=ORIENTED_EDGE('',*,*,#13839,.F.);
#18496=ORIENTED_EDGE('',*,*,#13840,.F.);
#18497=ORIENTED_EDGE('',*,*,#13841,.T.);
#18498=ORIENTED_EDGE('',*,*,#13842,.T.);
#18499=ORIENTED_EDGE('',*,*,#13843,.T.);
#18500=ORIENTED_EDGE('',*,*,#13836,.F.);
#18501=ORIENTED_EDGE('',*,*,#13844,.F.);
#18502=ORIENTED_EDGE('',*,*,#13845,.F.);
#18503=ORIENTED_EDGE('',*,*,#13846,.T.);
#18504=ORIENTED_EDGE('',*,*,#13847,.T.);
#18505=ORIENTED_EDGE('',*,*,#13848,.T.);
#18506=ORIENTED_EDGE('',*,*,#13841,.F.);
#18507=ORIENTED_EDGE('',*,*,#13849,.F.);
#18508=ORIENTED_EDGE('',*,*,#13850,.F.);
#18509=ORIENTED_EDGE('',*,*,#13851,.T.);
#18510=ORIENTED_EDGE('',*,*,#13852,.T.);
#18511=ORIENTED_EDGE('',*,*,#13853,.T.);
#18512=ORIENTED_EDGE('',*,*,#13846,.F.);
#18513=ORIENTED_EDGE('',*,*,#13854,.F.);
#18514=ORIENTED_EDGE('',*,*,#13855,.F.);
#18515=ORIENTED_EDGE('',*,*,#13856,.T.);
#18516=ORIENTED_EDGE('',*,*,#13857,.T.);
#18517=ORIENTED_EDGE('',*,*,#13858,.T.);
#18518=ORIENTED_EDGE('',*,*,#13851,.F.);
#18519=ORIENTED_EDGE('',*,*,#13859,.F.);
#18520=ORIENTED_EDGE('',*,*,#13860,.F.);
#18521=ORIENTED_EDGE('',*,*,#13861,.F.);
#18522=ORIENTED_EDGE('',*,*,#13862,.F.);
#18523=ORIENTED_EDGE('',*,*,#13863,.F.);
#18524=ORIENTED_EDGE('',*,*,#13864,.F.);
#18525=ORIENTED_EDGE('',*,*,#13865,.T.);
#18526=ORIENTED_EDGE('',*,*,#13866,.T.);
#18527=ORIENTED_EDGE('',*,*,#13867,.T.);
#18528=ORIENTED_EDGE('',*,*,#13868,.T.);
#18529=ORIENTED_EDGE('',*,*,#13869,.T.);
#18530=ORIENTED_EDGE('',*,*,#13870,.T.);
#18531=ORIENTED_EDGE('',*,*,#13871,.T.);
#18532=ORIENTED_EDGE('',*,*,#13872,.T.);
#18533=ORIENTED_EDGE('',*,*,#13873,.T.);
#18534=ORIENTED_EDGE('',*,*,#13874,.T.);
#18535=ORIENTED_EDGE('',*,*,#13867,.F.);
#18536=ORIENTED_EDGE('',*,*,#13875,.T.);
#18537=ORIENTED_EDGE('',*,*,#13876,.T.);
#18538=ORIENTED_EDGE('',*,*,#13877,.T.);
#18539=ORIENTED_EDGE('',*,*,#13878,.T.);
#18540=ORIENTED_EDGE('',*,*,#13879,.T.);
#18541=ORIENTED_EDGE('',*,*,#13872,.F.);
#18542=ORIENTED_EDGE('',*,*,#13880,.T.);
#18543=ORIENTED_EDGE('',*,*,#13881,.T.);
#18544=ORIENTED_EDGE('',*,*,#13882,.F.);
#18545=ORIENTED_EDGE('',*,*,#13883,.F.);
#18546=ORIENTED_EDGE('',*,*,#13884,.T.);
#18547=ORIENTED_EDGE('',*,*,#13885,.T.);
#18548=ORIENTED_EDGE('',*,*,#13886,.T.);
#18549=ORIENTED_EDGE('',*,*,#13887,.T.);
#18550=ORIENTED_EDGE('',*,*,#13888,.T.);
#18551=ORIENTED_EDGE('',*,*,#13889,.T.);
#18552=ORIENTED_EDGE('',*,*,#13890,.T.);
#18553=ORIENTED_EDGE('',*,*,#13885,.F.);
#18554=ORIENTED_EDGE('',*,*,#13891,.T.);
#18555=ORIENTED_EDGE('',*,*,#13892,.T.);
#18556=ORIENTED_EDGE('',*,*,#13893,.T.);
#18557=ORIENTED_EDGE('',*,*,#13894,.T.);
#18558=ORIENTED_EDGE('',*,*,#13888,.F.);
#18559=ORIENTED_EDGE('',*,*,#13895,.T.);
#18560=ORIENTED_EDGE('',*,*,#13896,.T.);
#18561=ORIENTED_EDGE('',*,*,#13897,.F.);
#18562=ORIENTED_EDGE('',*,*,#13898,.T.);
#18563=ORIENTED_EDGE('',*,*,#13899,.T.);
#18564=ORIENTED_EDGE('',*,*,#13900,.T.);
#18565=ORIENTED_EDGE('',*,*,#13901,.T.);
#18566=ORIENTED_EDGE('',*,*,#13902,.T.);
#18567=ORIENTED_EDGE('',*,*,#13903,.T.);
#18568=ORIENTED_EDGE('',*,*,#13904,.T.);
#18569=ORIENTED_EDGE('',*,*,#13905,.F.);
#18570=ORIENTED_EDGE('',*,*,#13906,.T.);
#18571=ORIENTED_EDGE('',*,*,#13907,.T.);
#18572=ORIENTED_EDGE('',*,*,#13908,.T.);
#18573=ORIENTED_EDGE('',*,*,#13909,.T.);
#18574=ORIENTED_EDGE('',*,*,#13902,.F.);
#18575=ORIENTED_EDGE('',*,*,#13910,.T.);
#18576=ORIENTED_EDGE('',*,*,#13911,.T.);
#18577=ORIENTED_EDGE('',*,*,#13912,.T.);
#18578=ORIENTED_EDGE('',*,*,#13913,.T.);
#18579=ORIENTED_EDGE('',*,*,#13908,.F.);
#18580=ORIENTED_EDGE('',*,*,#13914,.T.);
#18581=ORIENTED_EDGE('',*,*,#13915,.T.);
#18582=ORIENTED_EDGE('',*,*,#13916,.T.);
#18583=ORIENTED_EDGE('',*,*,#13917,.T.);
#18584=ORIENTED_EDGE('',*,*,#13918,.T.);
#18585=ORIENTED_EDGE('',*,*,#13911,.F.);
#18586=ORIENTED_EDGE('',*,*,#13919,.T.);
#18587=ORIENTED_EDGE('',*,*,#13920,.T.);
#18588=ORIENTED_EDGE('',*,*,#13921,.T.);
#18589=ORIENTED_EDGE('',*,*,#13922,.T.);
#18590=ORIENTED_EDGE('',*,*,#13916,.F.);
#18591=ORIENTED_EDGE('',*,*,#13923,.T.);
#18592=ORIENTED_EDGE('',*,*,#13924,.T.);
#18593=ORIENTED_EDGE('',*,*,#13925,.T.);
#18594=ORIENTED_EDGE('',*,*,#13926,.T.);
#18595=ORIENTED_EDGE('',*,*,#13920,.F.);
#18596=ORIENTED_EDGE('',*,*,#13927,.T.);
#18597=ORIENTED_EDGE('',*,*,#13928,.T.);
#18598=ORIENTED_EDGE('',*,*,#13929,.T.);
#18599=ORIENTED_EDGE('',*,*,#13930,.T.);
#18600=ORIENTED_EDGE('',*,*,#13925,.F.);
#18601=ORIENTED_EDGE('',*,*,#13931,.T.);
#18602=ORIENTED_EDGE('',*,*,#13932,.T.);
#18603=ORIENTED_EDGE('',*,*,#13933,.T.);
#18604=ORIENTED_EDGE('',*,*,#13934,.T.);
#18605=ORIENTED_EDGE('',*,*,#13928,.F.);
#18606=ORIENTED_EDGE('',*,*,#13935,.T.);
#18607=ORIENTED_EDGE('',*,*,#13936,.T.);
#18608=ORIENTED_EDGE('',*,*,#13937,.T.);
#18609=ORIENTED_EDGE('',*,*,#13938,.T.);
#18610=ORIENTED_EDGE('',*,*,#13933,.F.);
#18611=ORIENTED_EDGE('',*,*,#13939,.T.);
#18612=ORIENTED_EDGE('',*,*,#13940,.T.);
#18613=ORIENTED_EDGE('',*,*,#13941,.T.);
#18614=ORIENTED_EDGE('',*,*,#13942,.T.);
#18615=ORIENTED_EDGE('',*,*,#13943,.T.);
#18616=ORIENTED_EDGE('',*,*,#13936,.F.);
#18617=ORIENTED_EDGE('',*,*,#13944,.T.);
#18618=ORIENTED_EDGE('',*,*,#13945,.T.);
#18619=ORIENTED_EDGE('',*,*,#13946,.T.);
#18620=ORIENTED_EDGE('',*,*,#13947,.T.);
#18621=ORIENTED_EDGE('',*,*,#13941,.F.);
#18622=ORIENTED_EDGE('',*,*,#13948,.T.);
#18623=ORIENTED_EDGE('',*,*,#13949,.T.);
#18624=ORIENTED_EDGE('',*,*,#13950,.T.);
#18625=ORIENTED_EDGE('',*,*,#13951,.T.);
#18626=ORIENTED_EDGE('',*,*,#13945,.F.);
#18627=ORIENTED_EDGE('',*,*,#13952,.T.);
#18628=ORIENTED_EDGE('',*,*,#13953,.T.);
#18629=ORIENTED_EDGE('',*,*,#13954,.T.);
#18630=ORIENTED_EDGE('',*,*,#13955,.T.);
#18631=ORIENTED_EDGE('',*,*,#13956,.T.);
#18632=ORIENTED_EDGE('',*,*,#13950,.F.);
#18633=ORIENTED_EDGE('',*,*,#13957,.T.);
#18634=ORIENTED_EDGE('',*,*,#13958,.T.);
#18635=ORIENTED_EDGE('',*,*,#13959,.T.);
#18636=ORIENTED_EDGE('',*,*,#13960,.T.);
#18637=ORIENTED_EDGE('',*,*,#13954,.F.);
#18638=ORIENTED_EDGE('',*,*,#13961,.T.);
#18639=ORIENTED_EDGE('',*,*,#13962,.T.);
#18640=ORIENTED_EDGE('',*,*,#13963,.T.);
#18641=ORIENTED_EDGE('',*,*,#13964,.T.);
#18642=ORIENTED_EDGE('',*,*,#13959,.F.);
#18643=ORIENTED_EDGE('',*,*,#13965,.T.);
#18644=ORIENTED_EDGE('',*,*,#13966,.T.);
#18645=ORIENTED_EDGE('',*,*,#13967,.T.);
#18646=ORIENTED_EDGE('',*,*,#13968,.T.);
#18647=ORIENTED_EDGE('',*,*,#13969,.T.);
#18648=ORIENTED_EDGE('',*,*,#13962,.F.);
#18649=ORIENTED_EDGE('',*,*,#13970,.T.);
#18650=ORIENTED_EDGE('',*,*,#13971,.T.);
#18651=ORIENTED_EDGE('',*,*,#13972,.T.);
#18652=ORIENTED_EDGE('',*,*,#13973,.T.);
#18653=ORIENTED_EDGE('',*,*,#13967,.F.);
#18654=ORIENTED_EDGE('',*,*,#13974,.T.);
#18655=ORIENTED_EDGE('',*,*,#13975,.T.);
#18656=ORIENTED_EDGE('',*,*,#13976,.T.);
#18657=ORIENTED_EDGE('',*,*,#13977,.T.);
#18658=ORIENTED_EDGE('',*,*,#13971,.F.);
#18659=ORIENTED_EDGE('',*,*,#13978,.T.);
#18660=ORIENTED_EDGE('',*,*,#13979,.T.);
#18661=ORIENTED_EDGE('',*,*,#13980,.T.);
#18662=ORIENTED_EDGE('',*,*,#13981,.T.);
#18663=ORIENTED_EDGE('',*,*,#13982,.T.);
#18664=ORIENTED_EDGE('',*,*,#13976,.F.);
#18665=ORIENTED_EDGE('',*,*,#13983,.T.);
#18666=ORIENTED_EDGE('',*,*,#13984,.T.);
#18667=ORIENTED_EDGE('',*,*,#13985,.T.);
#18668=ORIENTED_EDGE('',*,*,#13986,.T.);
#18669=ORIENTED_EDGE('',*,*,#13980,.F.);
#18670=ORIENTED_EDGE('',*,*,#13987,.T.);
#18671=ORIENTED_EDGE('',*,*,#13988,.T.);
#18672=ORIENTED_EDGE('',*,*,#13989,.T.);
#18673=ORIENTED_EDGE('',*,*,#13990,.T.);
#18674=ORIENTED_EDGE('',*,*,#13985,.F.);
#18675=ORIENTED_EDGE('',*,*,#13991,.T.);
#18676=ORIENTED_EDGE('',*,*,#13992,.T.);
#18677=ORIENTED_EDGE('',*,*,#13993,.T.);
#18678=ORIENTED_EDGE('',*,*,#13994,.T.);
#18679=ORIENTED_EDGE('',*,*,#13988,.F.);
#18680=ORIENTED_EDGE('',*,*,#13995,.T.);
#18681=ORIENTED_EDGE('',*,*,#13996,.T.);
#18682=ORIENTED_EDGE('',*,*,#13997,.T.);
#18683=ORIENTED_EDGE('',*,*,#13998,.T.);
#18684=ORIENTED_EDGE('',*,*,#13993,.F.);
#18685=ORIENTED_EDGE('',*,*,#13999,.T.);
#18686=ORIENTED_EDGE('',*,*,#14000,.T.);
#18687=ORIENTED_EDGE('',*,*,#14001,.T.);
#18688=ORIENTED_EDGE('',*,*,#14002,.T.);
#18689=ORIENTED_EDGE('',*,*,#13996,.F.);
#18690=ORIENTED_EDGE('',*,*,#14003,.T.);
#18691=ORIENTED_EDGE('',*,*,#14004,.T.);
#18692=ORIENTED_EDGE('',*,*,#14005,.T.);
#18693=ORIENTED_EDGE('',*,*,#14006,.T.);
#18694=ORIENTED_EDGE('',*,*,#14007,.T.);
#18695=ORIENTED_EDGE('',*,*,#14001,.F.);
#18696=ORIENTED_EDGE('',*,*,#14008,.T.);
#18697=ORIENTED_EDGE('',*,*,#14009,.T.);
#18698=ORIENTED_EDGE('',*,*,#14010,.T.);
#18699=ORIENTED_EDGE('',*,*,#14011,.T.);
#18700=ORIENTED_EDGE('',*,*,#14005,.F.);
#18701=ORIENTED_EDGE('',*,*,#14012,.T.);
#18702=ORIENTED_EDGE('',*,*,#14013,.F.);
#18703=ORIENTED_EDGE('',*,*,#14014,.T.);
#18704=ORIENTED_EDGE('',*,*,#14015,.F.);
#18705=ORIENTED_EDGE('',*,*,#14016,.T.);
#18706=ORIENTED_EDGE('',*,*,#14017,.T.);
#18707=ORIENTED_EDGE('',*,*,#14018,.T.);
#18708=ORIENTED_EDGE('',*,*,#14019,.T.);
#18709=ORIENTED_EDGE('',*,*,#14020,.F.);
#18710=ORIENTED_EDGE('',*,*,#14021,.T.);
#18711=ORIENTED_EDGE('',*,*,#14022,.T.);
#18712=ORIENTED_EDGE('',*,*,#14023,.T.);
#18713=ORIENTED_EDGE('',*,*,#14024,.T.);
#18714=ORIENTED_EDGE('',*,*,#14017,.F.);
#18715=ORIENTED_EDGE('',*,*,#14025,.T.);
#18716=ORIENTED_EDGE('',*,*,#14026,.T.);
#18717=ORIENTED_EDGE('',*,*,#14027,.T.);
#18718=ORIENTED_EDGE('',*,*,#14028,.T.);
#18719=ORIENTED_EDGE('',*,*,#14023,.F.);
#18720=ORIENTED_EDGE('',*,*,#14029,.T.);
#18721=ORIENTED_EDGE('',*,*,#14030,.T.);
#18722=ORIENTED_EDGE('',*,*,#14031,.T.);
#18723=ORIENTED_EDGE('',*,*,#14032,.T.);
#18724=ORIENTED_EDGE('',*,*,#14033,.T.);
#18725=ORIENTED_EDGE('',*,*,#14026,.F.);
#18726=ORIENTED_EDGE('',*,*,#14034,.T.);
#18727=ORIENTED_EDGE('',*,*,#14035,.T.);
#18728=ORIENTED_EDGE('',*,*,#14036,.T.);
#18729=ORIENTED_EDGE('',*,*,#14037,.T.);
#18730=ORIENTED_EDGE('',*,*,#14031,.F.);
#18731=ORIENTED_EDGE('',*,*,#14038,.T.);
#18732=ORIENTED_EDGE('',*,*,#14039,.T.);
#18733=ORIENTED_EDGE('',*,*,#14040,.T.);
#18734=ORIENTED_EDGE('',*,*,#14041,.T.);
#18735=ORIENTED_EDGE('',*,*,#14035,.F.);
#18736=ORIENTED_EDGE('',*,*,#14042,.T.);
#18737=ORIENTED_EDGE('',*,*,#14043,.T.);
#18738=ORIENTED_EDGE('',*,*,#14044,.T.);
#18739=ORIENTED_EDGE('',*,*,#14045,.T.);
#18740=ORIENTED_EDGE('',*,*,#14040,.F.);
#18741=ORIENTED_EDGE('',*,*,#14046,.T.);
#18742=ORIENTED_EDGE('',*,*,#14047,.T.);
#18743=ORIENTED_EDGE('',*,*,#14048,.T.);
#18744=ORIENTED_EDGE('',*,*,#14049,.T.);
#18745=ORIENTED_EDGE('',*,*,#14043,.F.);
#18746=ORIENTED_EDGE('',*,*,#14050,.T.);
#18747=ORIENTED_EDGE('',*,*,#14051,.T.);
#18748=ORIENTED_EDGE('',*,*,#14052,.T.);
#18749=ORIENTED_EDGE('',*,*,#14053,.T.);
#18750=ORIENTED_EDGE('',*,*,#14048,.F.);
#18751=ORIENTED_EDGE('',*,*,#14054,.T.);
#18752=ORIENTED_EDGE('',*,*,#14055,.T.);
#18753=ORIENTED_EDGE('',*,*,#14056,.T.);
#18754=ORIENTED_EDGE('',*,*,#14057,.T.);
#18755=ORIENTED_EDGE('',*,*,#14058,.T.);
#18756=ORIENTED_EDGE('',*,*,#14051,.F.);
#18757=ORIENTED_EDGE('',*,*,#14059,.T.);
#18758=ORIENTED_EDGE('',*,*,#14060,.T.);
#18759=ORIENTED_EDGE('',*,*,#14061,.T.);
#18760=ORIENTED_EDGE('',*,*,#14062,.T.);
#18761=ORIENTED_EDGE('',*,*,#14056,.F.);
#18762=ORIENTED_EDGE('',*,*,#14063,.T.);
#18763=ORIENTED_EDGE('',*,*,#14064,.T.);
#18764=ORIENTED_EDGE('',*,*,#14065,.T.);
#18765=ORIENTED_EDGE('',*,*,#14066,.T.);
#18766=ORIENTED_EDGE('',*,*,#14060,.F.);
#18767=ORIENTED_EDGE('',*,*,#14067,.T.);
#18768=ORIENTED_EDGE('',*,*,#14068,.T.);
#18769=ORIENTED_EDGE('',*,*,#14069,.T.);
#18770=ORIENTED_EDGE('',*,*,#14070,.T.);
#18771=ORIENTED_EDGE('',*,*,#14071,.T.);
#18772=ORIENTED_EDGE('',*,*,#14065,.F.);
#18773=ORIENTED_EDGE('',*,*,#14072,.T.);
#18774=ORIENTED_EDGE('',*,*,#14073,.T.);
#18775=ORIENTED_EDGE('',*,*,#14074,.T.);
#18776=ORIENTED_EDGE('',*,*,#14075,.T.);
#18777=ORIENTED_EDGE('',*,*,#14069,.F.);
#18778=ORIENTED_EDGE('',*,*,#14076,.T.);
#18779=ORIENTED_EDGE('',*,*,#14077,.T.);
#18780=ORIENTED_EDGE('',*,*,#14078,.T.);
#18781=ORIENTED_EDGE('',*,*,#14079,.T.);
#18782=ORIENTED_EDGE('',*,*,#14074,.F.);
#18783=ORIENTED_EDGE('',*,*,#14080,.T.);
#18784=ORIENTED_EDGE('',*,*,#14081,.T.);
#18785=ORIENTED_EDGE('',*,*,#14082,.T.);
#18786=ORIENTED_EDGE('',*,*,#14083,.T.);
#18787=ORIENTED_EDGE('',*,*,#14084,.T.);
#18788=ORIENTED_EDGE('',*,*,#14077,.F.);
#18789=ORIENTED_EDGE('',*,*,#14085,.T.);
#18790=ORIENTED_EDGE('',*,*,#14086,.T.);
#18791=ORIENTED_EDGE('',*,*,#14087,.T.);
#18792=ORIENTED_EDGE('',*,*,#14088,.T.);
#18793=ORIENTED_EDGE('',*,*,#14082,.F.);
#18794=ORIENTED_EDGE('',*,*,#14089,.T.);
#18795=ORIENTED_EDGE('',*,*,#14090,.T.);
#18796=ORIENTED_EDGE('',*,*,#14091,.T.);
#18797=ORIENTED_EDGE('',*,*,#14092,.T.);
#18798=ORIENTED_EDGE('',*,*,#14086,.F.);
#18799=ORIENTED_EDGE('',*,*,#14093,.T.);
#18800=ORIENTED_EDGE('',*,*,#14094,.T.);
#18801=ORIENTED_EDGE('',*,*,#14095,.T.);
#18802=ORIENTED_EDGE('',*,*,#14096,.T.);
#18803=ORIENTED_EDGE('',*,*,#14097,.T.);
#18804=ORIENTED_EDGE('',*,*,#14091,.F.);
#18805=ORIENTED_EDGE('',*,*,#14098,.T.);
#18806=ORIENTED_EDGE('',*,*,#14099,.T.);
#18807=ORIENTED_EDGE('',*,*,#14100,.T.);
#18808=ORIENTED_EDGE('',*,*,#14101,.T.);
#18809=ORIENTED_EDGE('',*,*,#14095,.F.);
#18810=ORIENTED_EDGE('',*,*,#14102,.T.);
#18811=ORIENTED_EDGE('',*,*,#14103,.T.);
#18812=ORIENTED_EDGE('',*,*,#14104,.T.);
#18813=ORIENTED_EDGE('',*,*,#14105,.T.);
#18814=ORIENTED_EDGE('',*,*,#14100,.F.);
#18815=ORIENTED_EDGE('',*,*,#14106,.T.);
#18816=ORIENTED_EDGE('',*,*,#14107,.T.);
#18817=ORIENTED_EDGE('',*,*,#14108,.T.);
#18818=ORIENTED_EDGE('',*,*,#14109,.T.);
#18819=ORIENTED_EDGE('',*,*,#14103,.F.);
#18820=ORIENTED_EDGE('',*,*,#14110,.T.);
#18821=ORIENTED_EDGE('',*,*,#14111,.T.);
#18822=ORIENTED_EDGE('',*,*,#14112,.T.);
#18823=ORIENTED_EDGE('',*,*,#14113,.T.);
#18824=ORIENTED_EDGE('',*,*,#14108,.F.);
#18825=ORIENTED_EDGE('',*,*,#14114,.T.);
#18826=ORIENTED_EDGE('',*,*,#14115,.T.);
#18827=ORIENTED_EDGE('',*,*,#14116,.T.);
#18828=ORIENTED_EDGE('',*,*,#14117,.T.);
#18829=ORIENTED_EDGE('',*,*,#14111,.F.);
#18830=ORIENTED_EDGE('',*,*,#14118,.T.);
#18831=ORIENTED_EDGE('',*,*,#14119,.T.);
#18832=ORIENTED_EDGE('',*,*,#14120,.T.);
#18833=ORIENTED_EDGE('',*,*,#14121,.T.);
#18834=ORIENTED_EDGE('',*,*,#14122,.T.);
#18835=ORIENTED_EDGE('',*,*,#14116,.F.);
#18836=ORIENTED_EDGE('',*,*,#14123,.T.);
#18837=ORIENTED_EDGE('',*,*,#14124,.T.);
#18838=ORIENTED_EDGE('',*,*,#14125,.T.);
#18839=ORIENTED_EDGE('',*,*,#14126,.T.);
#18840=ORIENTED_EDGE('',*,*,#14120,.F.);
#18841=ORIENTED_EDGE('',*,*,#14127,.T.);
#18842=ORIENTED_EDGE('',*,*,#14128,.F.);
#18843=ORIENTED_EDGE('',*,*,#14129,.T.);
#18844=ORIENTED_EDGE('',*,*,#14130,.F.);
#18845=ORIENTED_EDGE('',*,*,#14131,.T.);
#18846=ORIENTED_EDGE('',*,*,#14132,.T.);
#18847=ORIENTED_EDGE('',*,*,#14133,.T.);
#18848=ORIENTED_EDGE('',*,*,#14134,.T.);
#18849=ORIENTED_EDGE('',*,*,#14135,.F.);
#18850=ORIENTED_EDGE('',*,*,#14136,.T.);
#18851=ORIENTED_EDGE('',*,*,#14137,.T.);
#18852=ORIENTED_EDGE('',*,*,#14138,.T.);
#18853=ORIENTED_EDGE('',*,*,#14139,.T.);
#18854=ORIENTED_EDGE('',*,*,#14132,.F.);
#18855=ORIENTED_EDGE('',*,*,#14140,.T.);
#18856=ORIENTED_EDGE('',*,*,#14141,.T.);
#18857=ORIENTED_EDGE('',*,*,#14142,.T.);
#18858=ORIENTED_EDGE('',*,*,#14143,.T.);
#18859=ORIENTED_EDGE('',*,*,#14138,.F.);
#18860=ORIENTED_EDGE('',*,*,#14144,.T.);
#18861=ORIENTED_EDGE('',*,*,#14145,.T.);
#18862=ORIENTED_EDGE('',*,*,#14146,.T.);
#18863=ORIENTED_EDGE('',*,*,#14147,.T.);
#18864=ORIENTED_EDGE('',*,*,#14148,.T.);
#18865=ORIENTED_EDGE('',*,*,#14141,.F.);
#18866=ORIENTED_EDGE('',*,*,#14149,.T.);
#18867=ORIENTED_EDGE('',*,*,#14150,.T.);
#18868=ORIENTED_EDGE('',*,*,#14151,.T.);
#18869=ORIENTED_EDGE('',*,*,#14152,.T.);
#18870=ORIENTED_EDGE('',*,*,#14146,.F.);
#18871=ORIENTED_EDGE('',*,*,#14153,.T.);
#18872=ORIENTED_EDGE('',*,*,#14154,.T.);
#18873=ORIENTED_EDGE('',*,*,#14155,.T.);
#18874=ORIENTED_EDGE('',*,*,#14156,.T.);
#18875=ORIENTED_EDGE('',*,*,#14150,.F.);
#18876=ORIENTED_EDGE('',*,*,#14157,.T.);
#18877=ORIENTED_EDGE('',*,*,#14158,.T.);
#18878=ORIENTED_EDGE('',*,*,#14159,.T.);
#18879=ORIENTED_EDGE('',*,*,#14160,.T.);
#18880=ORIENTED_EDGE('',*,*,#14155,.F.);
#18881=ORIENTED_EDGE('',*,*,#14161,.T.);
#18882=ORIENTED_EDGE('',*,*,#14162,.T.);
#18883=ORIENTED_EDGE('',*,*,#14163,.T.);
#18884=ORIENTED_EDGE('',*,*,#14164,.T.);
#18885=ORIENTED_EDGE('',*,*,#14158,.F.);
#18886=ORIENTED_EDGE('',*,*,#14165,.T.);
#18887=ORIENTED_EDGE('',*,*,#14166,.T.);
#18888=ORIENTED_EDGE('',*,*,#14167,.T.);
#18889=ORIENTED_EDGE('',*,*,#14168,.T.);
#18890=ORIENTED_EDGE('',*,*,#14163,.F.);
#18891=ORIENTED_EDGE('',*,*,#14169,.T.);
#18892=ORIENTED_EDGE('',*,*,#14170,.T.);
#18893=ORIENTED_EDGE('',*,*,#14171,.T.);
#18894=ORIENTED_EDGE('',*,*,#14172,.T.);
#18895=ORIENTED_EDGE('',*,*,#14173,.T.);
#18896=ORIENTED_EDGE('',*,*,#14166,.F.);
#18897=ORIENTED_EDGE('',*,*,#14174,.T.);
#18898=ORIENTED_EDGE('',*,*,#14175,.T.);
#18899=ORIENTED_EDGE('',*,*,#14176,.T.);
#18900=ORIENTED_EDGE('',*,*,#14177,.T.);
#18901=ORIENTED_EDGE('',*,*,#14171,.F.);
#18902=ORIENTED_EDGE('',*,*,#14178,.T.);
#18903=ORIENTED_EDGE('',*,*,#14179,.T.);
#18904=ORIENTED_EDGE('',*,*,#14180,.T.);
#18905=ORIENTED_EDGE('',*,*,#14181,.T.);
#18906=ORIENTED_EDGE('',*,*,#14175,.F.);
#18907=ORIENTED_EDGE('',*,*,#14182,.T.);
#18908=ORIENTED_EDGE('',*,*,#14183,.T.);
#18909=ORIENTED_EDGE('',*,*,#14184,.T.);
#18910=ORIENTED_EDGE('',*,*,#14185,.T.);
#18911=ORIENTED_EDGE('',*,*,#14186,.T.);
#18912=ORIENTED_EDGE('',*,*,#14180,.F.);
#18913=ORIENTED_EDGE('',*,*,#14187,.T.);
#18914=ORIENTED_EDGE('',*,*,#14188,.T.);
#18915=ORIENTED_EDGE('',*,*,#14189,.T.);
#18916=ORIENTED_EDGE('',*,*,#14190,.T.);
#18917=ORIENTED_EDGE('',*,*,#14184,.F.);
#18918=ORIENTED_EDGE('',*,*,#14191,.T.);
#18919=ORIENTED_EDGE('',*,*,#14192,.T.);
#18920=ORIENTED_EDGE('',*,*,#14193,.T.);
#18921=ORIENTED_EDGE('',*,*,#14194,.T.);
#18922=ORIENTED_EDGE('',*,*,#14189,.F.);
#18923=ORIENTED_EDGE('',*,*,#14195,.T.);
#18924=ORIENTED_EDGE('',*,*,#14196,.T.);
#18925=ORIENTED_EDGE('',*,*,#14197,.T.);
#18926=ORIENTED_EDGE('',*,*,#14198,.T.);
#18927=ORIENTED_EDGE('',*,*,#14199,.T.);
#18928=ORIENTED_EDGE('',*,*,#14192,.F.);
#18929=ORIENTED_EDGE('',*,*,#14200,.T.);
#18930=ORIENTED_EDGE('',*,*,#14201,.T.);
#18931=ORIENTED_EDGE('',*,*,#14202,.T.);
#18932=ORIENTED_EDGE('',*,*,#14203,.T.);
#18933=ORIENTED_EDGE('',*,*,#14197,.F.);
#18934=ORIENTED_EDGE('',*,*,#14204,.T.);
#18935=ORIENTED_EDGE('',*,*,#14205,.T.);
#18936=ORIENTED_EDGE('',*,*,#14206,.T.);
#18937=ORIENTED_EDGE('',*,*,#14207,.T.);
#18938=ORIENTED_EDGE('',*,*,#14201,.F.);
#18939=ORIENTED_EDGE('',*,*,#14208,.T.);
#18940=ORIENTED_EDGE('',*,*,#14209,.T.);
#18941=ORIENTED_EDGE('',*,*,#14210,.T.);
#18942=ORIENTED_EDGE('',*,*,#14211,.T.);
#18943=ORIENTED_EDGE('',*,*,#14212,.T.);
#18944=ORIENTED_EDGE('',*,*,#14206,.F.);
#18945=ORIENTED_EDGE('',*,*,#14213,.T.);
#18946=ORIENTED_EDGE('',*,*,#14214,.T.);
#18947=ORIENTED_EDGE('',*,*,#14215,.T.);
#18948=ORIENTED_EDGE('',*,*,#14216,.T.);
#18949=ORIENTED_EDGE('',*,*,#14210,.F.);
#18950=ORIENTED_EDGE('',*,*,#14217,.T.);
#18951=ORIENTED_EDGE('',*,*,#14218,.T.);
#18952=ORIENTED_EDGE('',*,*,#14219,.T.);
#18953=ORIENTED_EDGE('',*,*,#14220,.T.);
#18954=ORIENTED_EDGE('',*,*,#14215,.F.);
#18955=ORIENTED_EDGE('',*,*,#14221,.T.);
#18956=ORIENTED_EDGE('',*,*,#14222,.T.);
#18957=ORIENTED_EDGE('',*,*,#14223,.T.);
#18958=ORIENTED_EDGE('',*,*,#14224,.T.);
#18959=ORIENTED_EDGE('',*,*,#14218,.F.);
#18960=ORIENTED_EDGE('',*,*,#14225,.T.);
#18961=ORIENTED_EDGE('',*,*,#14226,.T.);
#18962=ORIENTED_EDGE('',*,*,#14227,.T.);
#18963=ORIENTED_EDGE('',*,*,#14228,.T.);
#18964=ORIENTED_EDGE('',*,*,#14223,.F.);
#18965=ORIENTED_EDGE('',*,*,#14229,.T.);
#18966=ORIENTED_EDGE('',*,*,#14230,.T.);
#18967=ORIENTED_EDGE('',*,*,#14231,.T.);
#18968=ORIENTED_EDGE('',*,*,#14232,.T.);
#18969=ORIENTED_EDGE('',*,*,#14226,.F.);
#18970=ORIENTED_EDGE('',*,*,#14233,.T.);
#18971=ORIENTED_EDGE('',*,*,#14234,.T.);
#18972=ORIENTED_EDGE('',*,*,#14235,.T.);
#18973=ORIENTED_EDGE('',*,*,#14236,.T.);
#18974=ORIENTED_EDGE('',*,*,#14237,.T.);
#18975=ORIENTED_EDGE('',*,*,#14231,.F.);
#18976=ORIENTED_EDGE('',*,*,#14238,.T.);
#18977=ORIENTED_EDGE('',*,*,#14239,.T.);
#18978=ORIENTED_EDGE('',*,*,#14240,.T.);
#18979=ORIENTED_EDGE('',*,*,#14241,.T.);
#18980=ORIENTED_EDGE('',*,*,#14235,.F.);
#18981=ORIENTED_EDGE('',*,*,#14242,.T.);
#18982=ORIENTED_EDGE('',*,*,#14243,.F.);
#18983=ORIENTED_EDGE('',*,*,#14244,.T.);
#18984=ORIENTED_EDGE('',*,*,#14245,.F.);
#18985=ORIENTED_EDGE('',*,*,#14246,.T.);
#18986=ORIENTED_EDGE('',*,*,#14247,.T.);
#18987=ORIENTED_EDGE('',*,*,#14248,.T.);
#18988=ORIENTED_EDGE('',*,*,#14249,.T.);
#18989=ORIENTED_EDGE('',*,*,#14250,.F.);
#18990=ORIENTED_EDGE('',*,*,#14251,.T.);
#18991=ORIENTED_EDGE('',*,*,#14252,.T.);
#18992=ORIENTED_EDGE('',*,*,#14253,.T.);
#18993=ORIENTED_EDGE('',*,*,#14254,.T.);
#18994=ORIENTED_EDGE('',*,*,#14247,.F.);
#18995=ORIENTED_EDGE('',*,*,#14255,.T.);
#18996=ORIENTED_EDGE('',*,*,#14256,.T.);
#18997=ORIENTED_EDGE('',*,*,#14257,.T.);
#18998=ORIENTED_EDGE('',*,*,#14258,.T.);
#18999=ORIENTED_EDGE('',*,*,#14253,.F.);
#19000=ORIENTED_EDGE('',*,*,#14259,.T.);
#19001=ORIENTED_EDGE('',*,*,#14260,.T.);
#19002=ORIENTED_EDGE('',*,*,#14261,.T.);
#19003=ORIENTED_EDGE('',*,*,#14262,.T.);
#19004=ORIENTED_EDGE('',*,*,#14263,.T.);
#19005=ORIENTED_EDGE('',*,*,#14256,.F.);
#19006=ORIENTED_EDGE('',*,*,#14264,.T.);
#19007=ORIENTED_EDGE('',*,*,#14265,.T.);
#19008=ORIENTED_EDGE('',*,*,#14266,.T.);
#19009=ORIENTED_EDGE('',*,*,#14267,.T.);
#19010=ORIENTED_EDGE('',*,*,#14261,.F.);
#19011=ORIENTED_EDGE('',*,*,#14268,.T.);
#19012=ORIENTED_EDGE('',*,*,#14269,.T.);
#19013=ORIENTED_EDGE('',*,*,#14270,.T.);
#19014=ORIENTED_EDGE('',*,*,#14271,.T.);
#19015=ORIENTED_EDGE('',*,*,#14265,.F.);
#19016=ORIENTED_EDGE('',*,*,#14272,.T.);
#19017=ORIENTED_EDGE('',*,*,#14273,.T.);
#19018=ORIENTED_EDGE('',*,*,#14274,.T.);
#19019=ORIENTED_EDGE('',*,*,#14275,.T.);
#19020=ORIENTED_EDGE('',*,*,#14270,.F.);
#19021=ORIENTED_EDGE('',*,*,#14276,.T.);
#19022=ORIENTED_EDGE('',*,*,#14277,.T.);
#19023=ORIENTED_EDGE('',*,*,#14278,.T.);
#19024=ORIENTED_EDGE('',*,*,#14279,.T.);
#19025=ORIENTED_EDGE('',*,*,#14273,.F.);
#19026=ORIENTED_EDGE('',*,*,#14280,.T.);
#19027=ORIENTED_EDGE('',*,*,#14281,.T.);
#19028=ORIENTED_EDGE('',*,*,#14282,.T.);
#19029=ORIENTED_EDGE('',*,*,#14283,.T.);
#19030=ORIENTED_EDGE('',*,*,#14278,.F.);
#19031=ORIENTED_EDGE('',*,*,#14284,.T.);
#19032=ORIENTED_EDGE('',*,*,#14285,.T.);
#19033=ORIENTED_EDGE('',*,*,#14286,.T.);
#19034=ORIENTED_EDGE('',*,*,#14287,.T.);
#19035=ORIENTED_EDGE('',*,*,#14288,.T.);
#19036=ORIENTED_EDGE('',*,*,#14281,.F.);
#19037=ORIENTED_EDGE('',*,*,#14289,.T.);
#19038=ORIENTED_EDGE('',*,*,#14290,.T.);
#19039=ORIENTED_EDGE('',*,*,#14291,.T.);
#19040=ORIENTED_EDGE('',*,*,#14292,.T.);
#19041=ORIENTED_EDGE('',*,*,#14286,.F.);
#19042=ORIENTED_EDGE('',*,*,#14293,.T.);
#19043=ORIENTED_EDGE('',*,*,#14294,.T.);
#19044=ORIENTED_EDGE('',*,*,#14295,.T.);
#19045=ORIENTED_EDGE('',*,*,#14296,.T.);
#19046=ORIENTED_EDGE('',*,*,#14290,.F.);
#19047=ORIENTED_EDGE('',*,*,#14297,.T.);
#19048=ORIENTED_EDGE('',*,*,#14298,.T.);
#19049=ORIENTED_EDGE('',*,*,#14299,.T.);
#19050=ORIENTED_EDGE('',*,*,#14300,.T.);
#19051=ORIENTED_EDGE('',*,*,#14301,.T.);
#19052=ORIENTED_EDGE('',*,*,#14295,.F.);
#19053=ORIENTED_EDGE('',*,*,#14302,.T.);
#19054=ORIENTED_EDGE('',*,*,#14303,.T.);
#19055=ORIENTED_EDGE('',*,*,#14304,.T.);
#19056=ORIENTED_EDGE('',*,*,#14305,.T.);
#19057=ORIENTED_EDGE('',*,*,#14299,.F.);
#19058=ORIENTED_EDGE('',*,*,#14306,.T.);
#19059=ORIENTED_EDGE('',*,*,#14307,.T.);
#19060=ORIENTED_EDGE('',*,*,#14308,.T.);
#19061=ORIENTED_EDGE('',*,*,#14309,.T.);
#19062=ORIENTED_EDGE('',*,*,#14304,.F.);
#19063=ORIENTED_EDGE('',*,*,#14310,.T.);
#19064=ORIENTED_EDGE('',*,*,#14311,.T.);
#19065=ORIENTED_EDGE('',*,*,#14312,.T.);
#19066=ORIENTED_EDGE('',*,*,#14313,.T.);
#19067=ORIENTED_EDGE('',*,*,#14314,.T.);
#19068=ORIENTED_EDGE('',*,*,#14307,.F.);
#19069=ORIENTED_EDGE('',*,*,#14315,.T.);
#19070=ORIENTED_EDGE('',*,*,#14316,.T.);
#19071=ORIENTED_EDGE('',*,*,#14317,.T.);
#19072=ORIENTED_EDGE('',*,*,#14318,.T.);
#19073=ORIENTED_EDGE('',*,*,#14312,.F.);
#19074=ORIENTED_EDGE('',*,*,#14319,.T.);
#19075=ORIENTED_EDGE('',*,*,#14320,.T.);
#19076=ORIENTED_EDGE('',*,*,#14321,.T.);
#19077=ORIENTED_EDGE('',*,*,#14322,.T.);
#19078=ORIENTED_EDGE('',*,*,#14316,.F.);
#19079=ORIENTED_EDGE('',*,*,#14323,.T.);
#19080=ORIENTED_EDGE('',*,*,#14324,.T.);
#19081=ORIENTED_EDGE('',*,*,#14325,.T.);
#19082=ORIENTED_EDGE('',*,*,#14326,.T.);
#19083=ORIENTED_EDGE('',*,*,#14327,.T.);
#19084=ORIENTED_EDGE('',*,*,#14321,.F.);
#19085=ORIENTED_EDGE('',*,*,#14328,.T.);
#19086=ORIENTED_EDGE('',*,*,#14329,.T.);
#19087=ORIENTED_EDGE('',*,*,#14330,.T.);
#19088=ORIENTED_EDGE('',*,*,#14331,.T.);
#19089=ORIENTED_EDGE('',*,*,#14325,.F.);
#19090=ORIENTED_EDGE('',*,*,#14332,.T.);
#19091=ORIENTED_EDGE('',*,*,#14333,.T.);
#19092=ORIENTED_EDGE('',*,*,#14334,.T.);
#19093=ORIENTED_EDGE('',*,*,#14335,.T.);
#19094=ORIENTED_EDGE('',*,*,#14330,.F.);
#19095=ORIENTED_EDGE('',*,*,#14336,.T.);
#19096=ORIENTED_EDGE('',*,*,#14337,.T.);
#19097=ORIENTED_EDGE('',*,*,#14338,.T.);
#19098=ORIENTED_EDGE('',*,*,#14339,.T.);
#19099=ORIENTED_EDGE('',*,*,#14333,.F.);
#19100=ORIENTED_EDGE('',*,*,#14340,.T.);
#19101=ORIENTED_EDGE('',*,*,#14341,.T.);
#19102=ORIENTED_EDGE('',*,*,#14342,.T.);
#19103=ORIENTED_EDGE('',*,*,#14343,.T.);
#19104=ORIENTED_EDGE('',*,*,#14338,.F.);
#19105=ORIENTED_EDGE('',*,*,#14344,.T.);
#19106=ORIENTED_EDGE('',*,*,#14345,.T.);
#19107=ORIENTED_EDGE('',*,*,#14346,.T.);
#19108=ORIENTED_EDGE('',*,*,#14347,.T.);
#19109=ORIENTED_EDGE('',*,*,#14341,.F.);
#19110=ORIENTED_EDGE('',*,*,#14348,.T.);
#19111=ORIENTED_EDGE('',*,*,#14349,.T.);
#19112=ORIENTED_EDGE('',*,*,#14350,.T.);
#19113=ORIENTED_EDGE('',*,*,#14351,.T.);
#19114=ORIENTED_EDGE('',*,*,#14352,.T.);
#19115=ORIENTED_EDGE('',*,*,#14346,.F.);
#19116=ORIENTED_EDGE('',*,*,#14353,.T.);
#19117=ORIENTED_EDGE('',*,*,#14354,.T.);
#19118=ORIENTED_EDGE('',*,*,#14355,.T.);
#19119=ORIENTED_EDGE('',*,*,#14356,.T.);
#19120=ORIENTED_EDGE('',*,*,#14350,.F.);
#19121=ORIENTED_EDGE('',*,*,#14357,.T.);
#19122=ORIENTED_EDGE('',*,*,#14358,.F.);
#19123=ORIENTED_EDGE('',*,*,#14359,.T.);
#19124=ORIENTED_EDGE('',*,*,#14360,.F.);
#19125=ORIENTED_EDGE('',*,*,#14361,.T.);
#19126=ORIENTED_EDGE('',*,*,#14358,.T.);
#19127=ORIENTED_EDGE('',*,*,#14362,.T.);
#19128=ORIENTED_EDGE('',*,*,#14363,.T.);
#19129=ORIENTED_EDGE('',*,*,#14355,.F.);
#19130=ORIENTED_EDGE('',*,*,#14364,.T.);
#19131=ORIENTED_EDGE('',*,*,#14365,.T.);
#19132=ORIENTED_EDGE('',*,*,#14243,.T.);
#19133=ORIENTED_EDGE('',*,*,#14366,.T.);
#19134=ORIENTED_EDGE('',*,*,#14367,.T.);
#19135=ORIENTED_EDGE('',*,*,#14240,.F.);
#19136=ORIENTED_EDGE('',*,*,#14368,.T.);
#19137=ORIENTED_EDGE('',*,*,#14369,.T.);
#19138=ORIENTED_EDGE('',*,*,#14128,.T.);
#19139=ORIENTED_EDGE('',*,*,#14370,.T.);
#19140=ORIENTED_EDGE('',*,*,#14371,.T.);
#19141=ORIENTED_EDGE('',*,*,#14125,.F.);
#19142=ORIENTED_EDGE('',*,*,#14372,.T.);
#19143=ORIENTED_EDGE('',*,*,#14373,.T.);
#19144=ORIENTED_EDGE('',*,*,#14013,.T.);
#19145=ORIENTED_EDGE('',*,*,#14374,.T.);
#19146=ORIENTED_EDGE('',*,*,#14375,.T.);
#19147=ORIENTED_EDGE('',*,*,#14010,.F.);
#19148=ORIENTED_EDGE('',*,*,#14376,.T.);
#19149=ORIENTED_EDGE('',*,*,#14377,.T.);
#19150=ORIENTED_EDGE('',*,*,#13897,.T.);
#19151=ORIENTED_EDGE('',*,*,#14378,.T.);
#19152=ORIENTED_EDGE('',*,*,#14379,.T.);
#19153=ORIENTED_EDGE('',*,*,#13892,.F.);
#19154=ORIENTED_EDGE('',*,*,#14380,.T.);
#19155=ORIENTED_EDGE('',*,*,#14381,.T.);
#19156=ORIENTED_EDGE('',*,*,#13882,.T.);
#19157=ORIENTED_EDGE('',*,*,#14382,.T.);
#19158=ORIENTED_EDGE('',*,*,#13877,.F.);
#19159=ORIENTED_EDGE('',*,*,#14383,.T.);
#19160=ORIENTED_EDGE('',*,*,#14384,.F.);
#19161=ORIENTED_EDGE('',*,*,#13861,.T.);
#19162=ORIENTED_EDGE('',*,*,#14385,.T.);
#19163=ORIENTED_EDGE('',*,*,#14386,.T.);
#19164=ORIENTED_EDGE('',*,*,#13856,.F.);
#19165=ORIENTED_EDGE('',*,*,#14387,.F.);
#19166=ORIENTED_EDGE('',*,*,#14388,.F.);
#19167=ORIENTED_EDGE('',*,*,#13724,.T.);
#19168=ORIENTED_EDGE('',*,*,#14389,.T.);
#19169=ORIENTED_EDGE('',*,*,#14390,.T.);
#19170=ORIENTED_EDGE('',*,*,#13719,.F.);
#19171=ORIENTED_EDGE('',*,*,#14391,.F.);
#19172=ORIENTED_EDGE('',*,*,#14392,.F.);
#19173=ORIENTED_EDGE('',*,*,#13587,.T.);
#19174=ORIENTED_EDGE('',*,*,#14393,.T.);
#19175=ORIENTED_EDGE('',*,*,#14394,.T.);
#19176=ORIENTED_EDGE('',*,*,#13582,.F.);
#19177=ORIENTED_EDGE('',*,*,#14395,.F.);
#19178=ORIENTED_EDGE('',*,*,#14396,.F.);
#19179=ORIENTED_EDGE('',*,*,#13450,.T.);
#19180=ORIENTED_EDGE('',*,*,#14397,.T.);
#19181=ORIENTED_EDGE('',*,*,#14398,.T.);
#19182=ORIENTED_EDGE('',*,*,#13445,.F.);
#19183=ORIENTED_EDGE('',*,*,#14399,.F.);
#19184=ORIENTED_EDGE('',*,*,#14400,.F.);
#19185=ORIENTED_EDGE('',*,*,#13313,.T.);
#19186=ORIENTED_EDGE('',*,*,#14401,.T.);
#19187=ORIENTED_EDGE('',*,*,#14402,.T.);
#19188=ORIENTED_EDGE('',*,*,#13308,.F.);
#19189=ORIENTED_EDGE('',*,*,#14403,.F.);
#19190=ORIENTED_EDGE('',*,*,#14404,.F.);
#19191=ORIENTED_EDGE('',*,*,#13293,.T.);
#19192=ORIENTED_EDGE('',*,*,#14405,.T.);
#19193=ORIENTED_EDGE('',*,*,#14406,.T.);
#19194=ORIENTED_EDGE('',*,*,#13288,.F.);
#19195=ORIENTED_EDGE('',*,*,#14407,.F.);
#19196=ORIENTED_EDGE('',*,*,#14408,.F.);
#19197=ORIENTED_EDGE('',*,*,#14409,.F.);
#19198=ORIENTED_EDGE('',*,*,#14410,.T.);
#19199=ORIENTED_EDGE('',*,*,#14411,.T.);
#19200=ORIENTED_EDGE('',*,*,#14410,.F.);
#19201=ORIENTED_EDGE('',*,*,#14411,.F.);
#19202=ORIENTED_EDGE('',*,*,#14412,.F.);
#19203=ORIENTED_EDGE('',*,*,#14413,.F.);
#19204=ORIENTED_EDGE('',*,*,#14414,.T.);
#19205=ORIENTED_EDGE('',*,*,#14415,.F.);
#19206=ORIENTED_EDGE('',*,*,#14416,.F.);
#19207=ORIENTED_EDGE('',*,*,#14414,.F.);
#19208=ORIENTED_EDGE('',*,*,#14417,.F.);
#19209=ORIENTED_EDGE('',*,*,#14418,.F.);
#19210=ORIENTED_EDGE('',*,*,#14419,.F.);
#19211=ORIENTED_EDGE('',*,*,#14420,.F.);
#19212=ORIENTED_EDGE('',*,*,#14421,.T.);
#19213=ORIENTED_EDGE('',*,*,#14422,.T.);
#19214=ORIENTED_EDGE('',*,*,#14421,.F.);
#19215=ORIENTED_EDGE('',*,*,#14422,.F.);
#19216=ORIENTED_EDGE('',*,*,#14423,.F.);
#19217=ORIENTED_EDGE('',*,*,#14424,.F.);
#19218=ORIENTED_EDGE('',*,*,#14425,.T.);
#19219=ORIENTED_EDGE('',*,*,#14426,.F.);
#19220=ORIENTED_EDGE('',*,*,#14427,.F.);
#19221=ORIENTED_EDGE('',*,*,#14428,.F.);
#19222=ORIENTED_EDGE('',*,*,#14425,.F.);
#19223=ORIENTED_EDGE('',*,*,#14429,.F.);
#19224=ORIENTED_EDGE('',*,*,#14430,.F.);
#19225=ORIENTED_EDGE('',*,*,#14431,.F.);
#19226=ORIENTED_EDGE('',*,*,#14432,.T.);
#19227=ORIENTED_EDGE('',*,*,#14433,.T.);
#19228=ORIENTED_EDGE('',*,*,#14432,.F.);
#19229=ORIENTED_EDGE('',*,*,#14433,.F.);
#19230=ORIENTED_EDGE('',*,*,#14418,.T.);
#19231=ORIENTED_EDGE('',*,*,#14434,.F.);
#19232=ORIENTED_EDGE('',*,*,#14435,.T.);
#19233=ORIENTED_EDGE('',*,*,#14436,.T.);
#19234=ORIENTED_EDGE('',*,*,#14429,.T.);
#19235=ORIENTED_EDGE('',*,*,#14424,.T.);
#19236=ORIENTED_EDGE('',*,*,#14437,.F.);
#19237=ORIENTED_EDGE('',*,*,#14438,.F.);
#19238=ORIENTED_EDGE('',*,*,#14439,.F.);
#19239=ORIENTED_EDGE('',*,*,#14440,.T.);
#19240=ORIENTED_EDGE('',*,*,#14417,.T.);
#19241=ORIENTED_EDGE('',*,*,#14413,.T.);
#19242=ORIENTED_EDGE('',*,*,#14441,.F.);
#19243=ORIENTED_EDGE('',*,*,#14426,.T.);
#19244=ORIENTED_EDGE('',*,*,#14428,.T.);
#19245=ORIENTED_EDGE('',*,*,#14442,.F.);
#19246=ORIENTED_EDGE('',*,*,#14443,.F.);
#19247=ORIENTED_EDGE('',*,*,#14434,.T.);
#19248=ORIENTED_EDGE('',*,*,#14412,.T.);
#19249=ORIENTED_EDGE('',*,*,#14444,.T.);
#19250=ORIENTED_EDGE('',*,*,#14445,.T.);
#19251=ORIENTED_EDGE('',*,*,#14446,.T.);
#19252=ORIENTED_EDGE('',*,*,#14447,.T.);
#19253=ORIENTED_EDGE('',*,*,#14448,.T.);
#19254=ORIENTED_EDGE('',*,*,#14449,.T.);
#19255=ORIENTED_EDGE('',*,*,#14450,.T.);
#19256=ORIENTED_EDGE('',*,*,#14451,.T.);
#19257=ORIENTED_EDGE('',*,*,#14452,.T.);
#19258=ORIENTED_EDGE('',*,*,#14453,.T.);
#19259=ORIENTED_EDGE('',*,*,#14454,.T.);
#19260=ORIENTED_EDGE('',*,*,#14455,.T.);
#19261=ORIENTED_EDGE('',*,*,#14456,.T.);
#19262=ORIENTED_EDGE('',*,*,#14457,.T.);
#19263=ORIENTED_EDGE('',*,*,#14458,.T.);
#19264=ORIENTED_EDGE('',*,*,#14459,.T.);
#19265=ORIENTED_EDGE('',*,*,#14460,.T.);
#19266=ORIENTED_EDGE('',*,*,#14461,.T.);
#19267=ORIENTED_EDGE('',*,*,#14462,.T.);
#19268=ORIENTED_EDGE('',*,*,#14463,.T.);
#19269=ORIENTED_EDGE('',*,*,#14464,.T.);
#19270=ORIENTED_EDGE('',*,*,#14465,.T.);
#19271=ORIENTED_EDGE('',*,*,#14466,.T.);
#19272=ORIENTED_EDGE('',*,*,#14467,.T.);
#19273=ORIENTED_EDGE('',*,*,#14468,.T.);
#19274=ORIENTED_EDGE('',*,*,#14469,.T.);
#19275=ORIENTED_EDGE('',*,*,#14470,.T.);
#19276=ORIENTED_EDGE('',*,*,#14471,.T.);
#19277=ORIENTED_EDGE('',*,*,#14437,.T.);
#19278=ORIENTED_EDGE('',*,*,#14423,.T.);
#19279=ORIENTED_EDGE('',*,*,#14441,.T.);
#19280=ORIENTED_EDGE('',*,*,#14472,.T.);
#19281=ORIENTED_EDGE('',*,*,#14473,.T.);
#19282=ORIENTED_EDGE('',*,*,#14474,.T.);
#19283=ORIENTED_EDGE('',*,*,#13322,.T.);
#19284=ORIENTED_EDGE('',*,*,#14475,.T.);
#19285=ORIENTED_EDGE('',*,*,#14250,.T.);
#19286=ORIENTED_EDGE('',*,*,#14476,.T.);
#19287=ORIENTED_EDGE('',*,*,#13459,.T.);
#19288=ORIENTED_EDGE('',*,*,#14477,.T.);
#19289=ORIENTED_EDGE('',*,*,#14135,.T.);
#19290=ORIENTED_EDGE('',*,*,#14478,.T.);
#19291=ORIENTED_EDGE('',*,*,#13596,.T.);
#19292=ORIENTED_EDGE('',*,*,#14479,.T.);
#19293=ORIENTED_EDGE('',*,*,#14020,.T.);
#19294=ORIENTED_EDGE('',*,*,#14480,.T.);
#19295=ORIENTED_EDGE('',*,*,#13733,.T.);
#19296=ORIENTED_EDGE('',*,*,#14481,.T.);
#19297=ORIENTED_EDGE('',*,*,#13905,.T.);
#19298=ORIENTED_EDGE('',*,*,#14431,.T.);
#19299=ORIENTED_EDGE('',*,*,#14420,.T.);
#19300=ORIENTED_EDGE('',*,*,#14409,.T.);
#19301=ORIENTED_EDGE('',*,*,#14482,.F.);
#19302=ORIENTED_EDGE('',*,*,#13280,.F.);
#19303=ORIENTED_EDGE('',*,*,#13285,.F.);
#19304=ORIENTED_EDGE('',*,*,#13284,.F.);
#19305=ORIENTED_EDGE('',*,*,#13290,.F.);
#19306=ORIENTED_EDGE('',*,*,#13289,.F.);
#19307=ORIENTED_EDGE('',*,*,#14406,.F.);
#19308=ORIENTED_EDGE('',*,*,#14405,.F.);
#19309=ORIENTED_EDGE('',*,*,#13298,.F.);
#19310=ORIENTED_EDGE('',*,*,#13297,.F.);
#19311=ORIENTED_EDGE('',*,*,#14483,.F.);
#19312=ORIENTED_EDGE('',*,*,#13898,.F.);
#19313=ORIENTED_EDGE('',*,*,#14381,.F.);
#19314=ORIENTED_EDGE('',*,*,#14380,.F.);
#19315=ORIENTED_EDGE('',*,*,#13896,.F.);
#19316=ORIENTED_EDGE('',*,*,#13895,.F.);
#19317=ORIENTED_EDGE('',*,*,#13891,.F.);
#19318=ORIENTED_EDGE('',*,*,#13887,.F.);
#19319=ORIENTED_EDGE('',*,*,#14484,.F.);
#19320=ORIENTED_EDGE('',*,*,#13889,.F.);
#19321=ORIENTED_EDGE('',*,*,#13894,.F.);
#19322=ORIENTED_EDGE('',*,*,#13893,.F.);
#19323=ORIENTED_EDGE('',*,*,#14379,.F.);
#19324=ORIENTED_EDGE('',*,*,#14378,.F.);
#19325=ORIENTED_EDGE('',*,*,#13901,.F.);
#19326=ORIENTED_EDGE('',*,*,#13900,.F.);
#19327=ORIENTED_EDGE('',*,*,#14485,.F.);
#19328=ORIENTED_EDGE('',*,*,#13295,.T.);
#19329=ORIENTED_EDGE('',*,*,#13294,.T.);
#19330=ORIENTED_EDGE('',*,*,#14408,.T.);
#19331=ORIENTED_EDGE('',*,*,#14407,.T.);
#19332=ORIENTED_EDGE('',*,*,#13292,.T.);
#19333=ORIENTED_EDGE('',*,*,#13291,.T.);
#19334=ORIENTED_EDGE('',*,*,#13287,.T.);
#19335=ORIENTED_EDGE('',*,*,#13286,.T.);
#19336=ORIENTED_EDGE('',*,*,#13282,.T.);
#19337=ORIENTED_EDGE('',*,*,#14486,.F.);
#19338=ORIENTED_EDGE('',*,*,#13300,.F.);
#19339=ORIENTED_EDGE('',*,*,#13305,.F.);
#19340=ORIENTED_EDGE('',*,*,#13304,.F.);
#19341=ORIENTED_EDGE('',*,*,#13310,.F.);
#19342=ORIENTED_EDGE('',*,*,#13309,.F.);
#19343=ORIENTED_EDGE('',*,*,#14402,.F.);
#19344=ORIENTED_EDGE('',*,*,#14401,.F.);
#19345=ORIENTED_EDGE('',*,*,#13318,.F.);
#19346=ORIENTED_EDGE('',*,*,#13317,.F.);
#19347=ORIENTED_EDGE('',*,*,#14487,.F.);
#19348=ORIENTED_EDGE('',*,*,#13868,.F.);
#19349=ORIENTED_EDGE('',*,*,#13874,.F.);
#19350=ORIENTED_EDGE('',*,*,#13873,.F.);
#19351=ORIENTED_EDGE('',*,*,#13879,.F.);
#19352=ORIENTED_EDGE('',*,*,#13878,.F.);
#19353=ORIENTED_EDGE('',*,*,#14382,.F.);
#19354=ORIENTED_EDGE('',*,*,#13884,.F.);
#19355=ORIENTED_EDGE('',*,*,#14488,.F.);
#19356=ORIENTED_EDGE('',*,*,#14383,.F.);
#19357=ORIENTED_EDGE('',*,*,#13881,.F.);
#19358=ORIENTED_EDGE('',*,*,#13880,.F.);
#19359=ORIENTED_EDGE('',*,*,#13876,.F.);
#19360=ORIENTED_EDGE('',*,*,#13875,.F.);
#19361=ORIENTED_EDGE('',*,*,#13871,.F.);
#19362=ORIENTED_EDGE('',*,*,#13870,.F.);
#19363=ORIENTED_EDGE('',*,*,#14489,.F.);
#19364=ORIENTED_EDGE('',*,*,#13315,.T.);
#19365=ORIENTED_EDGE('',*,*,#13314,.T.);
#19366=ORIENTED_EDGE('',*,*,#14404,.T.);
#19367=ORIENTED_EDGE('',*,*,#14403,.T.);
#19368=ORIENTED_EDGE('',*,*,#13312,.T.);
#19369=ORIENTED_EDGE('',*,*,#13311,.T.);
#19370=ORIENTED_EDGE('',*,*,#13307,.T.);
#19371=ORIENTED_EDGE('',*,*,#13306,.T.);
#19372=ORIENTED_EDGE('',*,*,#13302,.T.);
#19373=ORIENTED_EDGE('',*,*,#14475,.F.);
#19374=ORIENTED_EDGE('',*,*,#13321,.F.);
#19375=ORIENTED_EDGE('',*,*,#13320,.F.);
#19376=ORIENTED_EDGE('',*,*,#13327,.F.);
#19377=ORIENTED_EDGE('',*,*,#13326,.F.);
#19378=ORIENTED_EDGE('',*,*,#13332,.F.);
#19379=ORIENTED_EDGE('',*,*,#13331,.F.);
#19380=ORIENTED_EDGE('',*,*,#13337,.F.);
#19381=ORIENTED_EDGE('',*,*,#13336,.F.);
#19382=ORIENTED_EDGE('',*,*,#13342,.F.);
#19383=ORIENTED_EDGE('',*,*,#13341,.F.);
#19384=ORIENTED_EDGE('',*,*,#13347,.F.);
#19385=ORIENTED_EDGE('',*,*,#13346,.F.);
#19386=ORIENTED_EDGE('',*,*,#13352,.F.);
#19387=ORIENTED_EDGE('',*,*,#13351,.F.);
#19388=ORIENTED_EDGE('',*,*,#13357,.F.);
#19389=ORIENTED_EDGE('',*,*,#13356,.F.);
#19390=ORIENTED_EDGE('',*,*,#13362,.F.);
#19391=ORIENTED_EDGE('',*,*,#13361,.F.);
#19392=ORIENTED_EDGE('',*,*,#13367,.F.);
#19393=ORIENTED_EDGE('',*,*,#13366,.F.);
#19394=ORIENTED_EDGE('',*,*,#13372,.F.);
#19395=ORIENTED_EDGE('',*,*,#13371,.F.);
#19396=ORIENTED_EDGE('',*,*,#13377,.F.);
#19397=ORIENTED_EDGE('',*,*,#13376,.F.);
#19398=ORIENTED_EDGE('',*,*,#13382,.F.);
#19399=ORIENTED_EDGE('',*,*,#13381,.F.);
#19400=ORIENTED_EDGE('',*,*,#13387,.F.);
#19401=ORIENTED_EDGE('',*,*,#13386,.F.);
#19402=ORIENTED_EDGE('',*,*,#13392,.F.);
#19403=ORIENTED_EDGE('',*,*,#13391,.F.);
#19404=ORIENTED_EDGE('',*,*,#13397,.F.);
#19405=ORIENTED_EDGE('',*,*,#13396,.F.);
#19406=ORIENTED_EDGE('',*,*,#13402,.F.);
#19407=ORIENTED_EDGE('',*,*,#13401,.F.);
#19408=ORIENTED_EDGE('',*,*,#13407,.F.);
#19409=ORIENTED_EDGE('',*,*,#13406,.F.);
#19410=ORIENTED_EDGE('',*,*,#13412,.F.);
#19411=ORIENTED_EDGE('',*,*,#13411,.F.);
#19412=ORIENTED_EDGE('',*,*,#13417,.F.);
#19413=ORIENTED_EDGE('',*,*,#13416,.F.);
#19414=ORIENTED_EDGE('',*,*,#13422,.F.);
#19415=ORIENTED_EDGE('',*,*,#13421,.F.);
#19416=ORIENTED_EDGE('',*,*,#13427,.F.);
#19417=ORIENTED_EDGE('',*,*,#13426,.F.);
#19418=ORIENTED_EDGE('',*,*,#13432,.F.);
#19419=ORIENTED_EDGE('',*,*,#13431,.F.);
#19420=ORIENTED_EDGE('',*,*,#13437,.F.);
#19421=ORIENTED_EDGE('',*,*,#13436,.F.);
#19422=ORIENTED_EDGE('',*,*,#13442,.F.);
#19423=ORIENTED_EDGE('',*,*,#13441,.F.);
#19424=ORIENTED_EDGE('',*,*,#13447,.F.);
#19425=ORIENTED_EDGE('',*,*,#13446,.F.);
#19426=ORIENTED_EDGE('',*,*,#14398,.F.);
#19427=ORIENTED_EDGE('',*,*,#14397,.F.);
#19428=ORIENTED_EDGE('',*,*,#13455,.F.);
#19429=ORIENTED_EDGE('',*,*,#13454,.F.);
#19430=ORIENTED_EDGE('',*,*,#14490,.F.);
#19431=ORIENTED_EDGE('',*,*,#14359,.F.);
#19432=ORIENTED_EDGE('',*,*,#14365,.F.);
#19433=ORIENTED_EDGE('',*,*,#14364,.F.);
#19434=ORIENTED_EDGE('',*,*,#14357,.F.);
#19435=ORIENTED_EDGE('',*,*,#14354,.F.);
#19436=ORIENTED_EDGE('',*,*,#14353,.F.);
#19437=ORIENTED_EDGE('',*,*,#14349,.F.);
#19438=ORIENTED_EDGE('',*,*,#14348,.F.);
#19439=ORIENTED_EDGE('',*,*,#14345,.F.);
#19440=ORIENTED_EDGE('',*,*,#14344,.F.);
#19441=ORIENTED_EDGE('',*,*,#14340,.F.);
#19442=ORIENTED_EDGE('',*,*,#14337,.F.);
#19443=ORIENTED_EDGE('',*,*,#14336,.F.);
#19444=ORIENTED_EDGE('',*,*,#14332,.F.);
#19445=ORIENTED_EDGE('',*,*,#14329,.F.);
#19446=ORIENTED_EDGE('',*,*,#14328,.F.);
#19447=ORIENTED_EDGE('',*,*,#14324,.F.);
#19448=ORIENTED_EDGE('',*,*,#14323,.F.);
#19449=ORIENTED_EDGE('',*,*,#14320,.F.);
#19450=ORIENTED_EDGE('',*,*,#14319,.F.);
#19451=ORIENTED_EDGE('',*,*,#14315,.F.);
#19452=ORIENTED_EDGE('',*,*,#14311,.F.);
#19453=ORIENTED_EDGE('',*,*,#14310,.F.);
#19454=ORIENTED_EDGE('',*,*,#14306,.F.);
#19455=ORIENTED_EDGE('',*,*,#14303,.F.);
#19456=ORIENTED_EDGE('',*,*,#14302,.F.);
#19457=ORIENTED_EDGE('',*,*,#14298,.F.);
#19458=ORIENTED_EDGE('',*,*,#14297,.F.);
#19459=ORIENTED_EDGE('',*,*,#14294,.F.);
#19460=ORIENTED_EDGE('',*,*,#14293,.F.);
#19461=ORIENTED_EDGE('',*,*,#14289,.F.);
#19462=ORIENTED_EDGE('',*,*,#14285,.F.);
#19463=ORIENTED_EDGE('',*,*,#14284,.F.);
#19464=ORIENTED_EDGE('',*,*,#14280,.F.);
#19465=ORIENTED_EDGE('',*,*,#14277,.F.);
#19466=ORIENTED_EDGE('',*,*,#14276,.F.);
#19467=ORIENTED_EDGE('',*,*,#14272,.F.);
#19468=ORIENTED_EDGE('',*,*,#14269,.F.);
#19469=ORIENTED_EDGE('',*,*,#14268,.F.);
#19470=ORIENTED_EDGE('',*,*,#14264,.F.);
#19471=ORIENTED_EDGE('',*,*,#14260,.F.);
#19472=ORIENTED_EDGE('',*,*,#14259,.F.);
#19473=ORIENTED_EDGE('',*,*,#14255,.F.);
#19474=ORIENTED_EDGE('',*,*,#14252,.F.);
#19475=ORIENTED_EDGE('',*,*,#14251,.F.);
#19476=ORIENTED_EDGE('',*,*,#14474,.F.);
#19477=ORIENTED_EDGE('',*,*,#14249,.F.);
#19478=ORIENTED_EDGE('',*,*,#14248,.F.);
#19479=ORIENTED_EDGE('',*,*,#14254,.F.);
#19480=ORIENTED_EDGE('',*,*,#14258,.F.);
#19481=ORIENTED_EDGE('',*,*,#14257,.F.);
#19482=ORIENTED_EDGE('',*,*,#14263,.F.);
#19483=ORIENTED_EDGE('',*,*,#14262,.F.);
#19484=ORIENTED_EDGE('',*,*,#14267,.F.);
#19485=ORIENTED_EDGE('',*,*,#14266,.F.);
#19486=ORIENTED_EDGE('',*,*,#14271,.F.);
#19487=ORIENTED_EDGE('',*,*,#14275,.F.);
#19488=ORIENTED_EDGE('',*,*,#14274,.F.);
#19489=ORIENTED_EDGE('',*,*,#14279,.F.);
#19490=ORIENTED_EDGE('',*,*,#14283,.F.);
#19491=ORIENTED_EDGE('',*,*,#14282,.F.);
#19492=ORIENTED_EDGE('',*,*,#14288,.F.);
#19493=ORIENTED_EDGE('',*,*,#14287,.F.);
#19494=ORIENTED_EDGE('',*,*,#14292,.F.);
#19495=ORIENTED_EDGE('',*,*,#14291,.F.);
#19496=ORIENTED_EDGE('',*,*,#14296,.F.);
#19497=ORIENTED_EDGE('',*,*,#14301,.F.);
#19498=ORIENTED_EDGE('',*,*,#14300,.F.);
#19499=ORIENTED_EDGE('',*,*,#14305,.F.);
#19500=ORIENTED_EDGE('',*,*,#14309,.F.);
#19501=ORIENTED_EDGE('',*,*,#14308,.F.);
#19502=ORIENTED_EDGE('',*,*,#14314,.F.);
#19503=ORIENTED_EDGE('',*,*,#14313,.F.);
#19504=ORIENTED_EDGE('',*,*,#14318,.F.);
#19505=ORIENTED_EDGE('',*,*,#14317,.F.);
#19506=ORIENTED_EDGE('',*,*,#14322,.F.);
#19507=ORIENTED_EDGE('',*,*,#14327,.F.);
#19508=ORIENTED_EDGE('',*,*,#14326,.F.);
#19509=ORIENTED_EDGE('',*,*,#14331,.F.);
#19510=ORIENTED_EDGE('',*,*,#14335,.F.);
#19511=ORIENTED_EDGE('',*,*,#14334,.F.);
#19512=ORIENTED_EDGE('',*,*,#14339,.F.);
#19513=ORIENTED_EDGE('',*,*,#14343,.F.);
#19514=ORIENTED_EDGE('',*,*,#14342,.F.);
#19515=ORIENTED_EDGE('',*,*,#14347,.F.);
#19516=ORIENTED_EDGE('',*,*,#14352,.F.);
#19517=ORIENTED_EDGE('',*,*,#14351,.F.);
#19518=ORIENTED_EDGE('',*,*,#14356,.F.);
#19519=ORIENTED_EDGE('',*,*,#14363,.F.);
#19520=ORIENTED_EDGE('',*,*,#14362,.F.);
#19521=ORIENTED_EDGE('',*,*,#14361,.F.);
#19522=ORIENTED_EDGE('',*,*,#14491,.F.);
#19523=ORIENTED_EDGE('',*,*,#13452,.T.);
#19524=ORIENTED_EDGE('',*,*,#13451,.T.);
#19525=ORIENTED_EDGE('',*,*,#14400,.T.);
#19526=ORIENTED_EDGE('',*,*,#14399,.T.);
#19527=ORIENTED_EDGE('',*,*,#13449,.T.);
#19528=ORIENTED_EDGE('',*,*,#13448,.T.);
#19529=ORIENTED_EDGE('',*,*,#13444,.T.);
#19530=ORIENTED_EDGE('',*,*,#13443,.T.);
#19531=ORIENTED_EDGE('',*,*,#13439,.T.);
#19532=ORIENTED_EDGE('',*,*,#13438,.T.);
#19533=ORIENTED_EDGE('',*,*,#13434,.T.);
#19534=ORIENTED_EDGE('',*,*,#13433,.T.);
#19535=ORIENTED_EDGE('',*,*,#13429,.T.);
#19536=ORIENTED_EDGE('',*,*,#13428,.T.);
#19537=ORIENTED_EDGE('',*,*,#13424,.T.);
#19538=ORIENTED_EDGE('',*,*,#13423,.T.);
#19539=ORIENTED_EDGE('',*,*,#13419,.T.);
#19540=ORIENTED_EDGE('',*,*,#13418,.T.);
#19541=ORIENTED_EDGE('',*,*,#13414,.T.);
#19542=ORIENTED_EDGE('',*,*,#13413,.T.);
#19543=ORIENTED_EDGE('',*,*,#13409,.T.);
#19544=ORIENTED_EDGE('',*,*,#13408,.T.);
#19545=ORIENTED_EDGE('',*,*,#13404,.T.);
#19546=ORIENTED_EDGE('',*,*,#13403,.T.);
#19547=ORIENTED_EDGE('',*,*,#13399,.T.);
#19548=ORIENTED_EDGE('',*,*,#13398,.T.);
#19549=ORIENTED_EDGE('',*,*,#13394,.T.);
#19550=ORIENTED_EDGE('',*,*,#13393,.T.);
#19551=ORIENTED_EDGE('',*,*,#13389,.T.);
#19552=ORIENTED_EDGE('',*,*,#13388,.T.);
#19553=ORIENTED_EDGE('',*,*,#13384,.T.);
#19554=ORIENTED_EDGE('',*,*,#13383,.T.);
#19555=ORIENTED_EDGE('',*,*,#13379,.T.);
#19556=ORIENTED_EDGE('',*,*,#13378,.T.);
#19557=ORIENTED_EDGE('',*,*,#13374,.T.);
#19558=ORIENTED_EDGE('',*,*,#13373,.T.);
#19559=ORIENTED_EDGE('',*,*,#13369,.T.);
#19560=ORIENTED_EDGE('',*,*,#13368,.T.);
#19561=ORIENTED_EDGE('',*,*,#13364,.T.);
#19562=ORIENTED_EDGE('',*,*,#13363,.T.);
#19563=ORIENTED_EDGE('',*,*,#13359,.T.);
#19564=ORIENTED_EDGE('',*,*,#13358,.T.);
#19565=ORIENTED_EDGE('',*,*,#13354,.T.);
#19566=ORIENTED_EDGE('',*,*,#13353,.T.);
#19567=ORIENTED_EDGE('',*,*,#13349,.T.);
#19568=ORIENTED_EDGE('',*,*,#13348,.T.);
#19569=ORIENTED_EDGE('',*,*,#13344,.T.);
#19570=ORIENTED_EDGE('',*,*,#13343,.T.);
#19571=ORIENTED_EDGE('',*,*,#13339,.T.);
#19572=ORIENTED_EDGE('',*,*,#13338,.T.);
#19573=ORIENTED_EDGE('',*,*,#13334,.T.);
#19574=ORIENTED_EDGE('',*,*,#13333,.T.);
#19575=ORIENTED_EDGE('',*,*,#13329,.T.);
#19576=ORIENTED_EDGE('',*,*,#13328,.T.);
#19577=ORIENTED_EDGE('',*,*,#13324,.T.);
#19578=ORIENTED_EDGE('',*,*,#13323,.T.);
#19579=ORIENTED_EDGE('',*,*,#14477,.F.);
#19580=ORIENTED_EDGE('',*,*,#13458,.F.);
#19581=ORIENTED_EDGE('',*,*,#13457,.F.);
#19582=ORIENTED_EDGE('',*,*,#13464,.F.);
#19583=ORIENTED_EDGE('',*,*,#13463,.F.);
#19584=ORIENTED_EDGE('',*,*,#13469,.F.);
#19585=ORIENTED_EDGE('',*,*,#13468,.F.);
#19586=ORIENTED_EDGE('',*,*,#13474,.F.);
#19587=ORIENTED_EDGE('',*,*,#13473,.F.);
#19588=ORIENTED_EDGE('',*,*,#13479,.F.);
#19589=ORIENTED_EDGE('',*,*,#13478,.F.);
#19590=ORIENTED_EDGE('',*,*,#13484,.F.);
#19591=ORIENTED_EDGE('',*,*,#13483,.F.);
#19592=ORIENTED_EDGE('',*,*,#13489,.F.);
#19593=ORIENTED_EDGE('',*,*,#13488,.F.);
#19594=ORIENTED_EDGE('',*,*,#13494,.F.);
#19595=ORIENTED_EDGE('',*,*,#13493,.F.);
#19596=ORIENTED_EDGE('',*,*,#13499,.F.);
#19597=ORIENTED_EDGE('',*,*,#13498,.F.);
#19598=ORIENTED_EDGE('',*,*,#13504,.F.);
#19599=ORIENTED_EDGE('',*,*,#13503,.F.);
#19600=ORIENTED_EDGE('',*,*,#13509,.F.);
#19601=ORIENTED_EDGE('',*,*,#13508,.F.);
#19602=ORIENTED_EDGE('',*,*,#13514,.F.);
#19603=ORIENTED_EDGE('',*,*,#13513,.F.);
#19604=ORIENTED_EDGE('',*,*,#13519,.F.);
#19605=ORIENTED_EDGE('',*,*,#13518,.F.);
#19606=ORIENTED_EDGE('',*,*,#13524,.F.);
#19607=ORIENTED_EDGE('',*,*,#13523,.F.);
#19608=ORIENTED_EDGE('',*,*,#13529,.F.);
#19609=ORIENTED_EDGE('',*,*,#13528,.F.);
#19610=ORIENTED_EDGE('',*,*,#13534,.F.);
#19611=ORIENTED_EDGE('',*,*,#13533,.F.);
#19612=ORIENTED_EDGE('',*,*,#13539,.F.);
#19613=ORIENTED_EDGE('',*,*,#13538,.F.);
#19614=ORIENTED_EDGE('',*,*,#13544,.F.);
#19615=ORIENTED_EDGE('',*,*,#13543,.F.);
#19616=ORIENTED_EDGE('',*,*,#13549,.F.);
#19617=ORIENTED_EDGE('',*,*,#13548,.F.);
#19618=ORIENTED_EDGE('',*,*,#13554,.F.);
#19619=ORIENTED_EDGE('',*,*,#13553,.F.);
#19620=ORIENTED_EDGE('',*,*,#13559,.F.);
#19621=ORIENTED_EDGE('',*,*,#13558,.F.);
#19622=ORIENTED_EDGE('',*,*,#13564,.F.);
#19623=ORIENTED_EDGE('',*,*,#13563,.F.);
#19624=ORIENTED_EDGE('',*,*,#13569,.F.);
#19625=ORIENTED_EDGE('',*,*,#13568,.F.);
#19626=ORIENTED_EDGE('',*,*,#13574,.F.);
#19627=ORIENTED_EDGE('',*,*,#13573,.F.);
#19628=ORIENTED_EDGE('',*,*,#13579,.F.);
#19629=ORIENTED_EDGE('',*,*,#13578,.F.);
#19630=ORIENTED_EDGE('',*,*,#13584,.F.);
#19631=ORIENTED_EDGE('',*,*,#13583,.F.);
#19632=ORIENTED_EDGE('',*,*,#14394,.F.);
#19633=ORIENTED_EDGE('',*,*,#14393,.F.);
#19634=ORIENTED_EDGE('',*,*,#13592,.F.);
#19635=ORIENTED_EDGE('',*,*,#13591,.F.);
#19636=ORIENTED_EDGE('',*,*,#14492,.F.);
#19637=ORIENTED_EDGE('',*,*,#14244,.F.);
#19638=ORIENTED_EDGE('',*,*,#14369,.F.);
#19639=ORIENTED_EDGE('',*,*,#14368,.F.);
#19640=ORIENTED_EDGE('',*,*,#14242,.F.);
#19641=ORIENTED_EDGE('',*,*,#14239,.F.);
#19642=ORIENTED_EDGE('',*,*,#14238,.F.);
#19643=ORIENTED_EDGE('',*,*,#14234,.F.);
#19644=ORIENTED_EDGE('',*,*,#14233,.F.);
#19645=ORIENTED_EDGE('',*,*,#14230,.F.);
#19646=ORIENTED_EDGE('',*,*,#14229,.F.);
#19647=ORIENTED_EDGE('',*,*,#14225,.F.);
#19648=ORIENTED_EDGE('',*,*,#14222,.F.);
#19649=ORIENTED_EDGE('',*,*,#14221,.F.);
#19650=ORIENTED_EDGE('',*,*,#14217,.F.);
#19651=ORIENTED_EDGE('',*,*,#14214,.F.);
#19652=ORIENTED_EDGE('',*,*,#14213,.F.);
#19653=ORIENTED_EDGE('',*,*,#14209,.F.);
#19654=ORIENTED_EDGE('',*,*,#14208,.F.);
#19655=ORIENTED_EDGE('',*,*,#14205,.F.);
#19656=ORIENTED_EDGE('',*,*,#14204,.F.);
#19657=ORIENTED_EDGE('',*,*,#14200,.F.);
#19658=ORIENTED_EDGE('',*,*,#14196,.F.);
#19659=ORIENTED_EDGE('',*,*,#14195,.F.);
#19660=ORIENTED_EDGE('',*,*,#14191,.F.);
#19661=ORIENTED_EDGE('',*,*,#14188,.F.);
#19662=ORIENTED_EDGE('',*,*,#14187,.F.);
#19663=ORIENTED_EDGE('',*,*,#14183,.F.);
#19664=ORIENTED_EDGE('',*,*,#14182,.F.);
#19665=ORIENTED_EDGE('',*,*,#14179,.F.);
#19666=ORIENTED_EDGE('',*,*,#14178,.F.);
#19667=ORIENTED_EDGE('',*,*,#14174,.F.);
#19668=ORIENTED_EDGE('',*,*,#14170,.F.);
#19669=ORIENTED_EDGE('',*,*,#14169,.F.);
#19670=ORIENTED_EDGE('',*,*,#14165,.F.);
#19671=ORIENTED_EDGE('',*,*,#14162,.F.);
#19672=ORIENTED_EDGE('',*,*,#14161,.F.);
#19673=ORIENTED_EDGE('',*,*,#14157,.F.);
#19674=ORIENTED_EDGE('',*,*,#14154,.F.);
#19675=ORIENTED_EDGE('',*,*,#14153,.F.);
#19676=ORIENTED_EDGE('',*,*,#14149,.F.);
#19677=ORIENTED_EDGE('',*,*,#14145,.F.);
#19678=ORIENTED_EDGE('',*,*,#14144,.F.);
#19679=ORIENTED_EDGE('',*,*,#14140,.F.);
#19680=ORIENTED_EDGE('',*,*,#14137,.F.);
#19681=ORIENTED_EDGE('',*,*,#14136,.F.);
#19682=ORIENTED_EDGE('',*,*,#14476,.F.);
#19683=ORIENTED_EDGE('',*,*,#14134,.F.);
#19684=ORIENTED_EDGE('',*,*,#14133,.F.);
#19685=ORIENTED_EDGE('',*,*,#14139,.F.);
#19686=ORIENTED_EDGE('',*,*,#14143,.F.);
#19687=ORIENTED_EDGE('',*,*,#14142,.F.);
#19688=ORIENTED_EDGE('',*,*,#14148,.F.);
#19689=ORIENTED_EDGE('',*,*,#14147,.F.);
#19690=ORIENTED_EDGE('',*,*,#14152,.F.);
#19691=ORIENTED_EDGE('',*,*,#14151,.F.);
#19692=ORIENTED_EDGE('',*,*,#14156,.F.);
#19693=ORIENTED_EDGE('',*,*,#14160,.F.);
#19694=ORIENTED_EDGE('',*,*,#14159,.F.);
#19695=ORIENTED_EDGE('',*,*,#14164,.F.);
#19696=ORIENTED_EDGE('',*,*,#14168,.F.);
#19697=ORIENTED_EDGE('',*,*,#14167,.F.);
#19698=ORIENTED_EDGE('',*,*,#14173,.F.);
#19699=ORIENTED_EDGE('',*,*,#14172,.F.);
#19700=ORIENTED_EDGE('',*,*,#14177,.F.);
#19701=ORIENTED_EDGE('',*,*,#14176,.F.);
#19702=ORIENTED_EDGE('',*,*,#14181,.F.);
#19703=ORIENTED_EDGE('',*,*,#14186,.F.);
#19704=ORIENTED_EDGE('',*,*,#14185,.F.);
#19705=ORIENTED_EDGE('',*,*,#14190,.F.);
#19706=ORIENTED_EDGE('',*,*,#14194,.F.);
#19707=ORIENTED_EDGE('',*,*,#14193,.F.);
#19708=ORIENTED_EDGE('',*,*,#14199,.F.);
#19709=ORIENTED_EDGE('',*,*,#14198,.F.);
#19710=ORIENTED_EDGE('',*,*,#14203,.F.);
#19711=ORIENTED_EDGE('',*,*,#14202,.F.);
#19712=ORIENTED_EDGE('',*,*,#14207,.F.);
#19713=ORIENTED_EDGE('',*,*,#14212,.F.);
#19714=ORIENTED_EDGE('',*,*,#14211,.F.);
#19715=ORIENTED_EDGE('',*,*,#14216,.F.);
#19716=ORIENTED_EDGE('',*,*,#14220,.F.);
#19717=ORIENTED_EDGE('',*,*,#14219,.F.);
#19718=ORIENTED_EDGE('',*,*,#14224,.F.);
#19719=ORIENTED_EDGE('',*,*,#14228,.F.);
#19720=ORIENTED_EDGE('',*,*,#14227,.F.);
#19721=ORIENTED_EDGE('',*,*,#14232,.F.);
#19722=ORIENTED_EDGE('',*,*,#14237,.F.);
#19723=ORIENTED_EDGE('',*,*,#14236,.F.);
#19724=ORIENTED_EDGE('',*,*,#14241,.F.);
#19725=ORIENTED_EDGE('',*,*,#14367,.F.);
#19726=ORIENTED_EDGE('',*,*,#14366,.F.);
#19727=ORIENTED_EDGE('',*,*,#14246,.F.);
#19728=ORIENTED_EDGE('',*,*,#14493,.F.);
#19729=ORIENTED_EDGE('',*,*,#13589,.T.);
#19730=ORIENTED_EDGE('',*,*,#13588,.T.);
#19731=ORIENTED_EDGE('',*,*,#14396,.T.);
#19732=ORIENTED_EDGE('',*,*,#14395,.T.);
#19733=ORIENTED_EDGE('',*,*,#13586,.T.);
#19734=ORIENTED_EDGE('',*,*,#13585,.T.);
#19735=ORIENTED_EDGE('',*,*,#13581,.T.);
#19736=ORIENTED_EDGE('',*,*,#13580,.T.);
#19737=ORIENTED_EDGE('',*,*,#13576,.T.);
#19738=ORIENTED_EDGE('',*,*,#13575,.T.);
#19739=ORIENTED_EDGE('',*,*,#13571,.T.);
#19740=ORIENTED_EDGE('',*,*,#13570,.T.);
#19741=ORIENTED_EDGE('',*,*,#13566,.T.);
#19742=ORIENTED_EDGE('',*,*,#13565,.T.);
#19743=ORIENTED_EDGE('',*,*,#13561,.T.);
#19744=ORIENTED_EDGE('',*,*,#13560,.T.);
#19745=ORIENTED_EDGE('',*,*,#13556,.T.);
#19746=ORIENTED_EDGE('',*,*,#13555,.T.);
#19747=ORIENTED_EDGE('',*,*,#13551,.T.);
#19748=ORIENTED_EDGE('',*,*,#13550,.T.);
#19749=ORIENTED_EDGE('',*,*,#13546,.T.);
#19750=ORIENTED_EDGE('',*,*,#13545,.T.);
#19751=ORIENTED_EDGE('',*,*,#13541,.T.);
#19752=ORIENTED_EDGE('',*,*,#13540,.T.);
#19753=ORIENTED_EDGE('',*,*,#13536,.T.);
#19754=ORIENTED_EDGE('',*,*,#13535,.T.);
#19755=ORIENTED_EDGE('',*,*,#13531,.T.);
#19756=ORIENTED_EDGE('',*,*,#13530,.T.);
#19757=ORIENTED_EDGE('',*,*,#13526,.T.);
#19758=ORIENTED_EDGE('',*,*,#13525,.T.);
#19759=ORIENTED_EDGE('',*,*,#13521,.T.);
#19760=ORIENTED_EDGE('',*,*,#13520,.T.);
#19761=ORIENTED_EDGE('',*,*,#13516,.T.);
#19762=ORIENTED_EDGE('',*,*,#13515,.T.);
#19763=ORIENTED_EDGE('',*,*,#13511,.T.);
#19764=ORIENTED_EDGE('',*,*,#13510,.T.);
#19765=ORIENTED_EDGE('',*,*,#13506,.T.);
#19766=ORIENTED_EDGE('',*,*,#13505,.T.);
#19767=ORIENTED_EDGE('',*,*,#13501,.T.);
#19768=ORIENTED_EDGE('',*,*,#13500,.T.);
#19769=ORIENTED_EDGE('',*,*,#13496,.T.);
#19770=ORIENTED_EDGE('',*,*,#13495,.T.);
#19771=ORIENTED_EDGE('',*,*,#13491,.T.);
#19772=ORIENTED_EDGE('',*,*,#13490,.T.);
#19773=ORIENTED_EDGE('',*,*,#13486,.T.);
#19774=ORIENTED_EDGE('',*,*,#13485,.T.);
#19775=ORIENTED_EDGE('',*,*,#13481,.T.);
#19776=ORIENTED_EDGE('',*,*,#13480,.T.);
#19777=ORIENTED_EDGE('',*,*,#13476,.T.);
#19778=ORIENTED_EDGE('',*,*,#13475,.T.);
#19779=ORIENTED_EDGE('',*,*,#13471,.T.);
#19780=ORIENTED_EDGE('',*,*,#13470,.T.);
#19781=ORIENTED_EDGE('',*,*,#13466,.T.);
#19782=ORIENTED_EDGE('',*,*,#13465,.T.);
#19783=ORIENTED_EDGE('',*,*,#13461,.T.);
#19784=ORIENTED_EDGE('',*,*,#13460,.T.);
#19785=ORIENTED_EDGE('',*,*,#14479,.F.);
#19786=ORIENTED_EDGE('',*,*,#13595,.F.);
#19787=ORIENTED_EDGE('',*,*,#13594,.F.);
#19788=ORIENTED_EDGE('',*,*,#13601,.F.);
#19789=ORIENTED_EDGE('',*,*,#13600,.F.);
#19790=ORIENTED_EDGE('',*,*,#13606,.F.);
#19791=ORIENTED_EDGE('',*,*,#13605,.F.);
#19792=ORIENTED_EDGE('',*,*,#13611,.F.);
#19793=ORIENTED_EDGE('',*,*,#13610,.F.);
#19794=ORIENTED_EDGE('',*,*,#13616,.F.);
#19795=ORIENTED_EDGE('',*,*,#13615,.F.);
#19796=ORIENTED_EDGE('',*,*,#13621,.F.);
#19797=ORIENTED_EDGE('',*,*,#13620,.F.);
#19798=ORIENTED_EDGE('',*,*,#13626,.F.);
#19799=ORIENTED_EDGE('',*,*,#13625,.F.);
#19800=ORIENTED_EDGE('',*,*,#13631,.F.);
#19801=ORIENTED_EDGE('',*,*,#13630,.F.);
#19802=ORIENTED_EDGE('',*,*,#13636,.F.);
#19803=ORIENTED_EDGE('',*,*,#13635,.F.);
#19804=ORIENTED_EDGE('',*,*,#13641,.F.);
#19805=ORIENTED_EDGE('',*,*,#13640,.F.);
#19806=ORIENTED_EDGE('',*,*,#13646,.F.);
#19807=ORIENTED_EDGE('',*,*,#13645,.F.);
#19808=ORIENTED_EDGE('',*,*,#13651,.F.);
#19809=ORIENTED_EDGE('',*,*,#13650,.F.);
#19810=ORIENTED_EDGE('',*,*,#13656,.F.);
#19811=ORIENTED_EDGE('',*,*,#13655,.F.);
#19812=ORIENTED_EDGE('',*,*,#13661,.F.);
#19813=ORIENTED_EDGE('',*,*,#13660,.F.);
#19814=ORIENTED_EDGE('',*,*,#13666,.F.);
#19815=ORIENTED_EDGE('',*,*,#13665,.F.);
#19816=ORIENTED_EDGE('',*,*,#13671,.F.);
#19817=ORIENTED_EDGE('',*,*,#13670,.F.);
#19818=ORIENTED_EDGE('',*,*,#13676,.F.);
#19819=ORIENTED_EDGE('',*,*,#13675,.F.);
#19820=ORIENTED_EDGE('',*,*,#13681,.F.);
#19821=ORIENTED_EDGE('',*,*,#13680,.F.);
#19822=ORIENTED_EDGE('',*,*,#13686,.F.);
#19823=ORIENTED_EDGE('',*,*,#13685,.F.);
#19824=ORIENTED_EDGE('',*,*,#13691,.F.);
#19825=ORIENTED_EDGE('',*,*,#13690,.F.);
#19826=ORIENTED_EDGE('',*,*,#13696,.F.);
#19827=ORIENTED_EDGE('',*,*,#13695,.F.);
#19828=ORIENTED_EDGE('',*,*,#13701,.F.);
#19829=ORIENTED_EDGE('',*,*,#13700,.F.);
#19830=ORIENTED_EDGE('',*,*,#13706,.F.);
#19831=ORIENTED_EDGE('',*,*,#13705,.F.);
#19832=ORIENTED_EDGE('',*,*,#13711,.F.);
#19833=ORIENTED_EDGE('',*,*,#13710,.F.);
#19834=ORIENTED_EDGE('',*,*,#13716,.F.);
#19835=ORIENTED_EDGE('',*,*,#13715,.F.);
#19836=ORIENTED_EDGE('',*,*,#13721,.F.);
#19837=ORIENTED_EDGE('',*,*,#13720,.F.);
#19838=ORIENTED_EDGE('',*,*,#14390,.F.);
#19839=ORIENTED_EDGE('',*,*,#14389,.F.);
#19840=ORIENTED_EDGE('',*,*,#13729,.F.);
#19841=ORIENTED_EDGE('',*,*,#13728,.F.);
#19842=ORIENTED_EDGE('',*,*,#14494,.F.);
#19843=ORIENTED_EDGE('',*,*,#14129,.F.);
#19844=ORIENTED_EDGE('',*,*,#14373,.F.);
#19845=ORIENTED_EDGE('',*,*,#14372,.F.);
#19846=ORIENTED_EDGE('',*,*,#14127,.F.);
#19847=ORIENTED_EDGE('',*,*,#14124,.F.);
#19848=ORIENTED_EDGE('',*,*,#14123,.F.);
#19849=ORIENTED_EDGE('',*,*,#14119,.F.);
#19850=ORIENTED_EDGE('',*,*,#14118,.F.);
#19851=ORIENTED_EDGE('',*,*,#14115,.F.);
#19852=ORIENTED_EDGE('',*,*,#14114,.F.);
#19853=ORIENTED_EDGE('',*,*,#14110,.F.);
#19854=ORIENTED_EDGE('',*,*,#14107,.F.);
#19855=ORIENTED_EDGE('',*,*,#14106,.F.);
#19856=ORIENTED_EDGE('',*,*,#14102,.F.);
#19857=ORIENTED_EDGE('',*,*,#14099,.F.);
#19858=ORIENTED_EDGE('',*,*,#14098,.F.);
#19859=ORIENTED_EDGE('',*,*,#14094,.F.);
#19860=ORIENTED_EDGE('',*,*,#14093,.F.);
#19861=ORIENTED_EDGE('',*,*,#14090,.F.);
#19862=ORIENTED_EDGE('',*,*,#14089,.F.);
#19863=ORIENTED_EDGE('',*,*,#14085,.F.);
#19864=ORIENTED_EDGE('',*,*,#14081,.F.);
#19865=ORIENTED_EDGE('',*,*,#14080,.F.);
#19866=ORIENTED_EDGE('',*,*,#14076,.F.);
#19867=ORIENTED_EDGE('',*,*,#14073,.F.);
#19868=ORIENTED_EDGE('',*,*,#14072,.F.);
#19869=ORIENTED_EDGE('',*,*,#14068,.F.);
#19870=ORIENTED_EDGE('',*,*,#14067,.F.);
#19871=ORIENTED_EDGE('',*,*,#14064,.F.);
#19872=ORIENTED_EDGE('',*,*,#14063,.F.);
#19873=ORIENTED_EDGE('',*,*,#14059,.F.);
#19874=ORIENTED_EDGE('',*,*,#14055,.F.);
#19875=ORIENTED_EDGE('',*,*,#14054,.F.);
#19876=ORIENTED_EDGE('',*,*,#14050,.F.);
#19877=ORIENTED_EDGE('',*,*,#14047,.F.);
#19878=ORIENTED_EDGE('',*,*,#14046,.F.);
#19879=ORIENTED_EDGE('',*,*,#14042,.F.);
#19880=ORIENTED_EDGE('',*,*,#14039,.F.);
#19881=ORIENTED_EDGE('',*,*,#14038,.F.);
#19882=ORIENTED_EDGE('',*,*,#14034,.F.);
#19883=ORIENTED_EDGE('',*,*,#14030,.F.);
#19884=ORIENTED_EDGE('',*,*,#14029,.F.);
#19885=ORIENTED_EDGE('',*,*,#14025,.F.);
#19886=ORIENTED_EDGE('',*,*,#14022,.F.);
#19887=ORIENTED_EDGE('',*,*,#14021,.F.);
#19888=ORIENTED_EDGE('',*,*,#14478,.F.);
#19889=ORIENTED_EDGE('',*,*,#14019,.F.);
#19890=ORIENTED_EDGE('',*,*,#14018,.F.);
#19891=ORIENTED_EDGE('',*,*,#14024,.F.);
#19892=ORIENTED_EDGE('',*,*,#14028,.F.);
#19893=ORIENTED_EDGE('',*,*,#14027,.F.);
#19894=ORIENTED_EDGE('',*,*,#14033,.F.);
#19895=ORIENTED_EDGE('',*,*,#14032,.F.);
#19896=ORIENTED_EDGE('',*,*,#14037,.F.);
#19897=ORIENTED_EDGE('',*,*,#14036,.F.);
#19898=ORIENTED_EDGE('',*,*,#14041,.F.);
#19899=ORIENTED_EDGE('',*,*,#14045,.F.);
#19900=ORIENTED_EDGE('',*,*,#14044,.F.);
#19901=ORIENTED_EDGE('',*,*,#14049,.F.);
#19902=ORIENTED_EDGE('',*,*,#14053,.F.);
#19903=ORIENTED_EDGE('',*,*,#14052,.F.);
#19904=ORIENTED_EDGE('',*,*,#14058,.F.);
#19905=ORIENTED_EDGE('',*,*,#14057,.F.);
#19906=ORIENTED_EDGE('',*,*,#14062,.F.);
#19907=ORIENTED_EDGE('',*,*,#14061,.F.);
#19908=ORIENTED_EDGE('',*,*,#14066,.F.);
#19909=ORIENTED_EDGE('',*,*,#14071,.F.);
#19910=ORIENTED_EDGE('',*,*,#14070,.F.);
#19911=ORIENTED_EDGE('',*,*,#14075,.F.);
#19912=ORIENTED_EDGE('',*,*,#14079,.F.);
#19913=ORIENTED_EDGE('',*,*,#14078,.F.);
#19914=ORIENTED_EDGE('',*,*,#14084,.F.);
#19915=ORIENTED_EDGE('',*,*,#14083,.F.);
#19916=ORIENTED_EDGE('',*,*,#14088,.F.);
#19917=ORIENTED_EDGE('',*,*,#14087,.F.);
#19918=ORIENTED_EDGE('',*,*,#14092,.F.);
#19919=ORIENTED_EDGE('',*,*,#14097,.F.);
#19920=ORIENTED_EDGE('',*,*,#14096,.F.);
#19921=ORIENTED_EDGE('',*,*,#14101,.F.);
#19922=ORIENTED_EDGE('',*,*,#14105,.F.);
#19923=ORIENTED_EDGE('',*,*,#14104,.F.);
#19924=ORIENTED_EDGE('',*,*,#14109,.F.);
#19925=ORIENTED_EDGE('',*,*,#14113,.F.);
#19926=ORIENTED_EDGE('',*,*,#14112,.F.);
#19927=ORIENTED_EDGE('',*,*,#14117,.F.);
#19928=ORIENTED_EDGE('',*,*,#14122,.F.);
#19929=ORIENTED_EDGE('',*,*,#14121,.F.);
#19930=ORIENTED_EDGE('',*,*,#14126,.F.);
#19931=ORIENTED_EDGE('',*,*,#14371,.F.);
#19932=ORIENTED_EDGE('',*,*,#14370,.F.);
#19933=ORIENTED_EDGE('',*,*,#14131,.F.);
#19934=ORIENTED_EDGE('',*,*,#14495,.F.);
#19935=ORIENTED_EDGE('',*,*,#13726,.T.);
#19936=ORIENTED_EDGE('',*,*,#13725,.T.);
#19937=ORIENTED_EDGE('',*,*,#14392,.T.);
#19938=ORIENTED_EDGE('',*,*,#14391,.T.);
#19939=ORIENTED_EDGE('',*,*,#13723,.T.);
#19940=ORIENTED_EDGE('',*,*,#13722,.T.);
#19941=ORIENTED_EDGE('',*,*,#13718,.T.);
#19942=ORIENTED_EDGE('',*,*,#13717,.T.);
#19943=ORIENTED_EDGE('',*,*,#13713,.T.);
#19944=ORIENTED_EDGE('',*,*,#13712,.T.);
#19945=ORIENTED_EDGE('',*,*,#13708,.T.);
#19946=ORIENTED_EDGE('',*,*,#13707,.T.);
#19947=ORIENTED_EDGE('',*,*,#13703,.T.);
#19948=ORIENTED_EDGE('',*,*,#13702,.T.);
#19949=ORIENTED_EDGE('',*,*,#13698,.T.);
#19950=ORIENTED_EDGE('',*,*,#13697,.T.);
#19951=ORIENTED_EDGE('',*,*,#13693,.T.);
#19952=ORIENTED_EDGE('',*,*,#13692,.T.);
#19953=ORIENTED_EDGE('',*,*,#13688,.T.);
#19954=ORIENTED_EDGE('',*,*,#13687,.T.);
#19955=ORIENTED_EDGE('',*,*,#13683,.T.);
#19956=ORIENTED_EDGE('',*,*,#13682,.T.);
#19957=ORIENTED_EDGE('',*,*,#13678,.T.);
#19958=ORIENTED_EDGE('',*,*,#13677,.T.);
#19959=ORIENTED_EDGE('',*,*,#13673,.T.);
#19960=ORIENTED_EDGE('',*,*,#13672,.T.);
#19961=ORIENTED_EDGE('',*,*,#13668,.T.);
#19962=ORIENTED_EDGE('',*,*,#13667,.T.);
#19963=ORIENTED_EDGE('',*,*,#13663,.T.);
#19964=ORIENTED_EDGE('',*,*,#13662,.T.);
#19965=ORIENTED_EDGE('',*,*,#13658,.T.);
#19966=ORIENTED_EDGE('',*,*,#13657,.T.);
#19967=ORIENTED_EDGE('',*,*,#13653,.T.);
#19968=ORIENTED_EDGE('',*,*,#13652,.T.);
#19969=ORIENTED_EDGE('',*,*,#13648,.T.);
#19970=ORIENTED_EDGE('',*,*,#13647,.T.);
#19971=ORIENTED_EDGE('',*,*,#13643,.T.);
#19972=ORIENTED_EDGE('',*,*,#13642,.T.);
#19973=ORIENTED_EDGE('',*,*,#13638,.T.);
#19974=ORIENTED_EDGE('',*,*,#13637,.T.);
#19975=ORIENTED_EDGE('',*,*,#13633,.T.);
#19976=ORIENTED_EDGE('',*,*,#13632,.T.);
#19977=ORIENTED_EDGE('',*,*,#13628,.T.);
#19978=ORIENTED_EDGE('',*,*,#13627,.T.);
#19979=ORIENTED_EDGE('',*,*,#13623,.T.);
#19980=ORIENTED_EDGE('',*,*,#13622,.T.);
#19981=ORIENTED_EDGE('',*,*,#13618,.T.);
#19982=ORIENTED_EDGE('',*,*,#13617,.T.);
#19983=ORIENTED_EDGE('',*,*,#13613,.T.);
#19984=ORIENTED_EDGE('',*,*,#13612,.T.);
#19985=ORIENTED_EDGE('',*,*,#13608,.T.);
#19986=ORIENTED_EDGE('',*,*,#13607,.T.);
#19987=ORIENTED_EDGE('',*,*,#13603,.T.);
#19988=ORIENTED_EDGE('',*,*,#13602,.T.);
#19989=ORIENTED_EDGE('',*,*,#13598,.T.);
#19990=ORIENTED_EDGE('',*,*,#13597,.T.);
#19991=ORIENTED_EDGE('',*,*,#14481,.F.);
#19992=ORIENTED_EDGE('',*,*,#13732,.F.);
#19993=ORIENTED_EDGE('',*,*,#13731,.F.);
#19994=ORIENTED_EDGE('',*,*,#13738,.F.);
#19995=ORIENTED_EDGE('',*,*,#13737,.F.);
#19996=ORIENTED_EDGE('',*,*,#13743,.F.);
#19997=ORIENTED_EDGE('',*,*,#13742,.F.);
#19998=ORIENTED_EDGE('',*,*,#13748,.F.);
#19999=ORIENTED_EDGE('',*,*,#13747,.F.);
#20000=ORIENTED_EDGE('',*,*,#13753,.F.);
#20001=ORIENTED_EDGE('',*,*,#13752,.F.);
#20002=ORIENTED_EDGE('',*,*,#13758,.F.);
#20003=ORIENTED_EDGE('',*,*,#13757,.F.);
#20004=ORIENTED_EDGE('',*,*,#13763,.F.);
#20005=ORIENTED_EDGE('',*,*,#13762,.F.);
#20006=ORIENTED_EDGE('',*,*,#13768,.F.);
#20007=ORIENTED_EDGE('',*,*,#13767,.F.);
#20008=ORIENTED_EDGE('',*,*,#13773,.F.);
#20009=ORIENTED_EDGE('',*,*,#13772,.F.);
#20010=ORIENTED_EDGE('',*,*,#13778,.F.);
#20011=ORIENTED_EDGE('',*,*,#13777,.F.);
#20012=ORIENTED_EDGE('',*,*,#13783,.F.);
#20013=ORIENTED_EDGE('',*,*,#13782,.F.);
#20014=ORIENTED_EDGE('',*,*,#13788,.F.);
#20015=ORIENTED_EDGE('',*,*,#13787,.F.);
#20016=ORIENTED_EDGE('',*,*,#13793,.F.);
#20017=ORIENTED_EDGE('',*,*,#13792,.F.);
#20018=ORIENTED_EDGE('',*,*,#13798,.F.);
#20019=ORIENTED_EDGE('',*,*,#13797,.F.);
#20020=ORIENTED_EDGE('',*,*,#13803,.F.);
#20021=ORIENTED_EDGE('',*,*,#13802,.F.);
#20022=ORIENTED_EDGE('',*,*,#13808,.F.);
#20023=ORIENTED_EDGE('',*,*,#13807,.F.);
#20024=ORIENTED_EDGE('',*,*,#13813,.F.);
#20025=ORIENTED_EDGE('',*,*,#13812,.F.);
#20026=ORIENTED_EDGE('',*,*,#13818,.F.);
#20027=ORIENTED_EDGE('',*,*,#13817,.F.);
#20028=ORIENTED_EDGE('',*,*,#13823,.F.);
#20029=ORIENTED_EDGE('',*,*,#13822,.F.);
#20030=ORIENTED_EDGE('',*,*,#13828,.F.);
#20031=ORIENTED_EDGE('',*,*,#13827,.F.);
#20032=ORIENTED_EDGE('',*,*,#13833,.F.);
#20033=ORIENTED_EDGE('',*,*,#13832,.F.);
#20034=ORIENTED_EDGE('',*,*,#13838,.F.);
#20035=ORIENTED_EDGE('',*,*,#13837,.F.);
#20036=ORIENTED_EDGE('',*,*,#13843,.F.);
#20037=ORIENTED_EDGE('',*,*,#13842,.F.);
#20038=ORIENTED_EDGE('',*,*,#13848,.F.);
#20039=ORIENTED_EDGE('',*,*,#13847,.F.);
#20040=ORIENTED_EDGE('',*,*,#13853,.F.);
#20041=ORIENTED_EDGE('',*,*,#13852,.F.);
#20042=ORIENTED_EDGE('',*,*,#13858,.F.);
#20043=ORIENTED_EDGE('',*,*,#13857,.F.);
#20044=ORIENTED_EDGE('',*,*,#14386,.F.);
#20045=ORIENTED_EDGE('',*,*,#14385,.F.);
#20046=ORIENTED_EDGE('',*,*,#13866,.F.);
#20047=ORIENTED_EDGE('',*,*,#13865,.F.);
#20048=ORIENTED_EDGE('',*,*,#14496,.F.);
#20049=ORIENTED_EDGE('',*,*,#14014,.F.);
#20050=ORIENTED_EDGE('',*,*,#14377,.F.);
#20051=ORIENTED_EDGE('',*,*,#14376,.F.);
#20052=ORIENTED_EDGE('',*,*,#14012,.F.);
#20053=ORIENTED_EDGE('',*,*,#14009,.F.);
#20054=ORIENTED_EDGE('',*,*,#14008,.F.);
#20055=ORIENTED_EDGE('',*,*,#14004,.F.);
#20056=ORIENTED_EDGE('',*,*,#14003,.F.);
#20057=ORIENTED_EDGE('',*,*,#14000,.F.);
#20058=ORIENTED_EDGE('',*,*,#13999,.F.);
#20059=ORIENTED_EDGE('',*,*,#13995,.F.);
#20060=ORIENTED_EDGE('',*,*,#13992,.F.);
#20061=ORIENTED_EDGE('',*,*,#13991,.F.);
#20062=ORIENTED_EDGE('',*,*,#13987,.F.);
#20063=ORIENTED_EDGE('',*,*,#13984,.F.);
#20064=ORIENTED_EDGE('',*,*,#13983,.F.);
#20065=ORIENTED_EDGE('',*,*,#13979,.F.);
#20066=ORIENTED_EDGE('',*,*,#13978,.F.);
#20067=ORIENTED_EDGE('',*,*,#13975,.F.);
#20068=ORIENTED_EDGE('',*,*,#13974,.F.);
#20069=ORIENTED_EDGE('',*,*,#13970,.F.);
#20070=ORIENTED_EDGE('',*,*,#13966,.F.);
#20071=ORIENTED_EDGE('',*,*,#13965,.F.);
#20072=ORIENTED_EDGE('',*,*,#13961,.F.);
#20073=ORIENTED_EDGE('',*,*,#13958,.F.);
#20074=ORIENTED_EDGE('',*,*,#13957,.F.);
#20075=ORIENTED_EDGE('',*,*,#13953,.F.);
#20076=ORIENTED_EDGE('',*,*,#13952,.F.);
#20077=ORIENTED_EDGE('',*,*,#13949,.F.);
#20078=ORIENTED_EDGE('',*,*,#13948,.F.);
#20079=ORIENTED_EDGE('',*,*,#13944,.F.);
#20080=ORIENTED_EDGE('',*,*,#13940,.F.);
#20081=ORIENTED_EDGE('',*,*,#13939,.F.);
#20082=ORIENTED_EDGE('',*,*,#13935,.F.);
#20083=ORIENTED_EDGE('',*,*,#13932,.F.);
#20084=ORIENTED_EDGE('',*,*,#13931,.F.);
#20085=ORIENTED_EDGE('',*,*,#13927,.F.);
#20086=ORIENTED_EDGE('',*,*,#13924,.F.);
#20087=ORIENTED_EDGE('',*,*,#13923,.F.);
#20088=ORIENTED_EDGE('',*,*,#13919,.F.);
#20089=ORIENTED_EDGE('',*,*,#13915,.F.);
#20090=ORIENTED_EDGE('',*,*,#13914,.F.);
#20091=ORIENTED_EDGE('',*,*,#13910,.F.);
#20092=ORIENTED_EDGE('',*,*,#13907,.F.);
#20093=ORIENTED_EDGE('',*,*,#13906,.F.);
#20094=ORIENTED_EDGE('',*,*,#14480,.F.);
#20095=ORIENTED_EDGE('',*,*,#13904,.F.);
#20096=ORIENTED_EDGE('',*,*,#13903,.F.);
#20097=ORIENTED_EDGE('',*,*,#13909,.F.);
#20098=ORIENTED_EDGE('',*,*,#13913,.F.);
#20099=ORIENTED_EDGE('',*,*,#13912,.F.);
#20100=ORIENTED_EDGE('',*,*,#13918,.F.);
#20101=ORIENTED_EDGE('',*,*,#13917,.F.);
#20102=ORIENTED_EDGE('',*,*,#13922,.F.);
#20103=ORIENTED_EDGE('',*,*,#13921,.F.);
#20104=ORIENTED_EDGE('',*,*,#13926,.F.);
#20105=ORIENTED_EDGE('',*,*,#13930,.F.);
#20106=ORIENTED_EDGE('',*,*,#13929,.F.);
#20107=ORIENTED_EDGE('',*,*,#13934,.F.);
#20108=ORIENTED_EDGE('',*,*,#13938,.F.);
#20109=ORIENTED_EDGE('',*,*,#13937,.F.);
#20110=ORIENTED_EDGE('',*,*,#13943,.F.);
#20111=ORIENTED_EDGE('',*,*,#13942,.F.);
#20112=ORIENTED_EDGE('',*,*,#13947,.F.);
#20113=ORIENTED_EDGE('',*,*,#13946,.F.);
#20114=ORIENTED_EDGE('',*,*,#13951,.F.);
#20115=ORIENTED_EDGE('',*,*,#13956,.F.);
#20116=ORIENTED_EDGE('',*,*,#13955,.F.);
#20117=ORIENTED_EDGE('',*,*,#13960,.F.);
#20118=ORIENTED_EDGE('',*,*,#13964,.F.);
#20119=ORIENTED_EDGE('',*,*,#13963,.F.);
#20120=ORIENTED_EDGE('',*,*,#13969,.F.);
#20121=ORIENTED_EDGE('',*,*,#13968,.F.);
#20122=ORIENTED_EDGE('',*,*,#13973,.F.);
#20123=ORIENTED_EDGE('',*,*,#13972,.F.);
#20124=ORIENTED_EDGE('',*,*,#13977,.F.);
#20125=ORIENTED_EDGE('',*,*,#13982,.F.);
#20126=ORIENTED_EDGE('',*,*,#13981,.F.);
#20127=ORIENTED_EDGE('',*,*,#13986,.F.);
#20128=ORIENTED_EDGE('',*,*,#13990,.F.);
#20129=ORIENTED_EDGE('',*,*,#13989,.F.);
#20130=ORIENTED_EDGE('',*,*,#13994,.F.);
#20131=ORIENTED_EDGE('',*,*,#13998,.F.);
#20132=ORIENTED_EDGE('',*,*,#13997,.F.);
#20133=ORIENTED_EDGE('',*,*,#14002,.F.);
#20134=ORIENTED_EDGE('',*,*,#14007,.F.);
#20135=ORIENTED_EDGE('',*,*,#14006,.F.);
#20136=ORIENTED_EDGE('',*,*,#14011,.F.);
#20137=ORIENTED_EDGE('',*,*,#14375,.F.);
#20138=ORIENTED_EDGE('',*,*,#14374,.F.);
#20139=ORIENTED_EDGE('',*,*,#14016,.F.);
#20140=ORIENTED_EDGE('',*,*,#14497,.F.);
#20141=ORIENTED_EDGE('',*,*,#13863,.T.);
#20142=ORIENTED_EDGE('',*,*,#13862,.T.);
#20143=ORIENTED_EDGE('',*,*,#14388,.T.);
#20144=ORIENTED_EDGE('',*,*,#14387,.T.);
#20145=ORIENTED_EDGE('',*,*,#13860,.T.);
#20146=ORIENTED_EDGE('',*,*,#13859,.T.);
#20147=ORIENTED_EDGE('',*,*,#13855,.T.);
#20148=ORIENTED_EDGE('',*,*,#13854,.T.);
#20149=ORIENTED_EDGE('',*,*,#13850,.T.);
#20150=ORIENTED_EDGE('',*,*,#13849,.T.);
#20151=ORIENTED_EDGE('',*,*,#13845,.T.);
#20152=ORIENTED_EDGE('',*,*,#13844,.T.);
#20153=ORIENTED_EDGE('',*,*,#13840,.T.);
#20154=ORIENTED_EDGE('',*,*,#13839,.T.);
#20155=ORIENTED_EDGE('',*,*,#13835,.T.);
#20156=ORIENTED_EDGE('',*,*,#13834,.T.);
#20157=ORIENTED_EDGE('',*,*,#13830,.T.);
#20158=ORIENTED_EDGE('',*,*,#13829,.T.);
#20159=ORIENTED_EDGE('',*,*,#13825,.T.);
#20160=ORIENTED_EDGE('',*,*,#13824,.T.);
#20161=ORIENTED_EDGE('',*,*,#13820,.T.);
#20162=ORIENTED_EDGE('',*,*,#13819,.T.);
#20163=ORIENTED_EDGE('',*,*,#13815,.T.);
#20164=ORIENTED_EDGE('',*,*,#13814,.T.);
#20165=ORIENTED_EDGE('',*,*,#13810,.T.);
#20166=ORIENTED_EDGE('',*,*,#13809,.T.);
#20167=ORIENTED_EDGE('',*,*,#13805,.T.);
#20168=ORIENTED_EDGE('',*,*,#13804,.T.);
#20169=ORIENTED_EDGE('',*,*,#13800,.T.);
#20170=ORIENTED_EDGE('',*,*,#13799,.T.);
#20171=ORIENTED_EDGE('',*,*,#13795,.T.);
#20172=ORIENTED_EDGE('',*,*,#13794,.T.);
#20173=ORIENTED_EDGE('',*,*,#13790,.T.);
#20174=ORIENTED_EDGE('',*,*,#13789,.T.);
#20175=ORIENTED_EDGE('',*,*,#13785,.T.);
#20176=ORIENTED_EDGE('',*,*,#13784,.T.);
#20177=ORIENTED_EDGE('',*,*,#13780,.T.);
#20178=ORIENTED_EDGE('',*,*,#13779,.T.);
#20179=ORIENTED_EDGE('',*,*,#13775,.T.);
#20180=ORIENTED_EDGE('',*,*,#13774,.T.);
#20181=ORIENTED_EDGE('',*,*,#13770,.T.);
#20182=ORIENTED_EDGE('',*,*,#13769,.T.);
#20183=ORIENTED_EDGE('',*,*,#13765,.T.);
#20184=ORIENTED_EDGE('',*,*,#13764,.T.);
#20185=ORIENTED_EDGE('',*,*,#13760,.T.);
#20186=ORIENTED_EDGE('',*,*,#13759,.T.);
#20187=ORIENTED_EDGE('',*,*,#13755,.T.);
#20188=ORIENTED_EDGE('',*,*,#13754,.T.);
#20189=ORIENTED_EDGE('',*,*,#13750,.T.);
#20190=ORIENTED_EDGE('',*,*,#13749,.T.);
#20191=ORIENTED_EDGE('',*,*,#13745,.T.);
#20192=ORIENTED_EDGE('',*,*,#13744,.T.);
#20193=ORIENTED_EDGE('',*,*,#13740,.T.);
#20194=ORIENTED_EDGE('',*,*,#13739,.T.);
#20195=ORIENTED_EDGE('',*,*,#13735,.T.);
#20196=ORIENTED_EDGE('',*,*,#13734,.T.);
#20197=ORIENTED_EDGE('',*,*,#14498,.F.);
#20198=ORIENTED_EDGE('',*,*,#14499,.T.);
#20199=ORIENTED_EDGE('',*,*,#14500,.F.);
#20200=ORIENTED_EDGE('',*,*,#14501,.F.);
#20201=ORIENTED_EDGE('',*,*,#14502,.F.);
#20202=ORIENTED_EDGE('',*,*,#14501,.T.);
#20203=ORIENTED_EDGE('',*,*,#14503,.F.);
#20204=ORIENTED_EDGE('',*,*,#14504,.F.);
#20205=ORIENTED_EDGE('',*,*,#14505,.F.);
#20206=ORIENTED_EDGE('',*,*,#14504,.T.);
#20207=ORIENTED_EDGE('',*,*,#14506,.F.);
#20208=ORIENTED_EDGE('',*,*,#14507,.F.);
#20209=ORIENTED_EDGE('',*,*,#14508,.F.);
#20210=ORIENTED_EDGE('',*,*,#14507,.T.);
#20211=ORIENTED_EDGE('',*,*,#14509,.F.);
#20212=ORIENTED_EDGE('',*,*,#14510,.F.);
#20213=ORIENTED_EDGE('',*,*,#14511,.F.);
#20214=ORIENTED_EDGE('',*,*,#14510,.T.);
#20215=ORIENTED_EDGE('',*,*,#14512,.F.);
#20216=ORIENTED_EDGE('',*,*,#14513,.F.);
#20217=ORIENTED_EDGE('',*,*,#14514,.F.);
#20218=ORIENTED_EDGE('',*,*,#14513,.T.);
#20219=ORIENTED_EDGE('',*,*,#14515,.F.);
#20220=ORIENTED_EDGE('',*,*,#14516,.F.);
#20221=ORIENTED_EDGE('',*,*,#14517,.F.);
#20222=ORIENTED_EDGE('',*,*,#14516,.T.);
#20223=ORIENTED_EDGE('',*,*,#14518,.F.);
#20224=ORIENTED_EDGE('',*,*,#14499,.F.);
#20225=ORIENTED_EDGE('',*,*,#14519,.F.);
#20226=ORIENTED_EDGE('',*,*,#14520,.T.);
#20227=ORIENTED_EDGE('',*,*,#14521,.F.);
#20228=ORIENTED_EDGE('',*,*,#14520,.F.);
#20229=ORIENTED_EDGE('',*,*,#14519,.T.);
#20230=ORIENTED_EDGE('',*,*,#14518,.T.);
#20231=ORIENTED_EDGE('',*,*,#14515,.T.);
#20232=ORIENTED_EDGE('',*,*,#14512,.T.);
#20233=ORIENTED_EDGE('',*,*,#14509,.T.);
#20234=ORIENTED_EDGE('',*,*,#14506,.T.);
#20235=ORIENTED_EDGE('',*,*,#14503,.T.);
#20236=ORIENTED_EDGE('',*,*,#14500,.T.);
#20237=ORIENTED_EDGE('',*,*,#14522,.F.);
#20238=ORIENTED_EDGE('',*,*,#14523,.T.);
#20239=ORIENTED_EDGE('',*,*,#14524,.F.);
#20240=ORIENTED_EDGE('',*,*,#14525,.F.);
#20241=ORIENTED_EDGE('',*,*,#14526,.F.);
#20242=ORIENTED_EDGE('',*,*,#14525,.T.);
#20243=ORIENTED_EDGE('',*,*,#14527,.F.);
#20244=ORIENTED_EDGE('',*,*,#14528,.F.);
#20245=ORIENTED_EDGE('',*,*,#14529,.F.);
#20246=ORIENTED_EDGE('',*,*,#14528,.T.);
#20247=ORIENTED_EDGE('',*,*,#14530,.F.);
#20248=ORIENTED_EDGE('',*,*,#14531,.F.);
#20249=ORIENTED_EDGE('',*,*,#14532,.F.);
#20250=ORIENTED_EDGE('',*,*,#14531,.T.);
#20251=ORIENTED_EDGE('',*,*,#14533,.F.);
#20252=ORIENTED_EDGE('',*,*,#14453,.F.);
#20253=ORIENTED_EDGE('',*,*,#14534,.F.);
#20254=ORIENTED_EDGE('',*,*,#14455,.F.);
#20255=ORIENTED_EDGE('',*,*,#14535,.F.);
#20256=ORIENTED_EDGE('',*,*,#14523,.F.);
#20257=ORIENTED_EDGE('',*,*,#14535,.T.);
#20258=ORIENTED_EDGE('',*,*,#14454,.F.);
#20259=ORIENTED_EDGE('',*,*,#14533,.T.);
#20260=ORIENTED_EDGE('',*,*,#14530,.T.);
#20261=ORIENTED_EDGE('',*,*,#14527,.T.);
#20262=ORIENTED_EDGE('',*,*,#14524,.T.);
#20263=ORIENTED_EDGE('',*,*,#14489,.T.);
#20264=ORIENTED_EDGE('',*,*,#13869,.F.);
#20265=ORIENTED_EDGE('',*,*,#14487,.T.);
#20266=ORIENTED_EDGE('',*,*,#13316,.T.);
#20267=ORIENTED_EDGE('',*,*,#14536,.F.);
#20268=ORIENTED_EDGE('',*,*,#14537,.F.);
#20269=ORIENTED_EDGE('',*,*,#14538,.F.);
#20270=ORIENTED_EDGE('',*,*,#14539,.T.);
#20271=ORIENTED_EDGE('',*,*,#14540,.F.);
#20272=ORIENTED_EDGE('',*,*,#14541,.F.);
#20273=ORIENTED_EDGE('',*,*,#14542,.F.);
#20274=ORIENTED_EDGE('',*,*,#14541,.T.);
#20275=ORIENTED_EDGE('',*,*,#14543,.F.);
#20276=ORIENTED_EDGE('',*,*,#14544,.F.);
#20277=ORIENTED_EDGE('',*,*,#14545,.F.);
#20278=ORIENTED_EDGE('',*,*,#14544,.T.);
#20279=ORIENTED_EDGE('',*,*,#14546,.F.);
#20280=ORIENTED_EDGE('',*,*,#14547,.F.);
#20281=ORIENTED_EDGE('',*,*,#14548,.F.);
#20282=ORIENTED_EDGE('',*,*,#14547,.T.);
#20283=ORIENTED_EDGE('',*,*,#14549,.F.);
#20284=ORIENTED_EDGE('',*,*,#14550,.F.);
#20285=ORIENTED_EDGE('',*,*,#14551,.F.);
#20286=ORIENTED_EDGE('',*,*,#14550,.T.);
#20287=ORIENTED_EDGE('',*,*,#14552,.F.);
#20288=ORIENTED_EDGE('',*,*,#14553,.F.);
#20289=ORIENTED_EDGE('',*,*,#14554,.F.);
#20290=ORIENTED_EDGE('',*,*,#14553,.T.);
#20291=ORIENTED_EDGE('',*,*,#14555,.F.);
#20292=ORIENTED_EDGE('',*,*,#14556,.F.);
#20293=ORIENTED_EDGE('',*,*,#14557,.F.);
#20294=ORIENTED_EDGE('',*,*,#14556,.T.);
#20295=ORIENTED_EDGE('',*,*,#14558,.F.);
#20296=ORIENTED_EDGE('',*,*,#14539,.F.);
#20297=ORIENTED_EDGE('',*,*,#14559,.F.);
#20298=ORIENTED_EDGE('',*,*,#14560,.T.);
#20299=ORIENTED_EDGE('',*,*,#14561,.F.);
#20300=ORIENTED_EDGE('',*,*,#14560,.F.);
#20301=ORIENTED_EDGE('',*,*,#14559,.T.);
#20302=ORIENTED_EDGE('',*,*,#14558,.T.);
#20303=ORIENTED_EDGE('',*,*,#14555,.T.);
#20304=ORIENTED_EDGE('',*,*,#14552,.T.);
#20305=ORIENTED_EDGE('',*,*,#14549,.T.);
#20306=ORIENTED_EDGE('',*,*,#14546,.T.);
#20307=ORIENTED_EDGE('',*,*,#14543,.T.);
#20308=ORIENTED_EDGE('',*,*,#14540,.T.);
#20309=ORIENTED_EDGE('',*,*,#14538,.T.);
#20310=ORIENTED_EDGE('',*,*,#14542,.T.);
#20311=ORIENTED_EDGE('',*,*,#14545,.T.);
#20312=ORIENTED_EDGE('',*,*,#14548,.T.);
#20313=ORIENTED_EDGE('',*,*,#14551,.T.);
#20314=ORIENTED_EDGE('',*,*,#14554,.T.);
#20315=ORIENTED_EDGE('',*,*,#14557,.T.);
#20316=ORIENTED_EDGE('',*,*,#14498,.T.);
#20317=ORIENTED_EDGE('',*,*,#14502,.T.);
#20318=ORIENTED_EDGE('',*,*,#14505,.T.);
#20319=ORIENTED_EDGE('',*,*,#14508,.T.);
#20320=ORIENTED_EDGE('',*,*,#14511,.T.);
#20321=ORIENTED_EDGE('',*,*,#14514,.T.);
#20322=ORIENTED_EDGE('',*,*,#14517,.T.);
#20323=ORIENTED_EDGE('',*,*,#14562,.F.);
#20324=ORIENTED_EDGE('',*,*,#14563,.T.);
#20325=ORIENTED_EDGE('',*,*,#14536,.T.);
#20326=ORIENTED_EDGE('',*,*,#14563,.F.);
#20327=ORIENTED_EDGE('',*,*,#14562,.T.);
#20328=ORIENTED_EDGE('',*,*,#13883,.T.);
#20329=ORIENTED_EDGE('',*,*,#14384,.T.);
#20330=ORIENTED_EDGE('',*,*,#14488,.T.);
#20331=ORIENTED_EDGE('',*,*,#13301,.T.);
#20332=ORIENTED_EDGE('',*,*,#14486,.T.);
#20333=ORIENTED_EDGE('',*,*,#14564,.F.);
#20334=ORIENTED_EDGE('',*,*,#14565,.T.);
#20335=ORIENTED_EDGE('',*,*,#14537,.T.);
#20336=ORIENTED_EDGE('',*,*,#14565,.F.);
#20337=ORIENTED_EDGE('',*,*,#14564,.T.);
#20338=ORIENTED_EDGE('',*,*,#14566,.F.);
#20339=ORIENTED_EDGE('',*,*,#14567,.T.);
#20340=ORIENTED_EDGE('',*,*,#14568,.T.);
#20341=ORIENTED_EDGE('',*,*,#14569,.F.);
#20342=ORIENTED_EDGE('',*,*,#14570,.F.);
#20343=ORIENTED_EDGE('',*,*,#14571,.T.);
#20344=ORIENTED_EDGE('',*,*,#14572,.T.);
#20345=ORIENTED_EDGE('',*,*,#14567,.F.);
#20346=ORIENTED_EDGE('',*,*,#14573,.F.);
#20347=ORIENTED_EDGE('',*,*,#14574,.T.);
#20348=ORIENTED_EDGE('',*,*,#14575,.T.);
#20349=ORIENTED_EDGE('',*,*,#14571,.F.);
#20350=ORIENTED_EDGE('',*,*,#14576,.F.);
#20351=ORIENTED_EDGE('',*,*,#14463,.F.);
#20352=ORIENTED_EDGE('',*,*,#14577,.T.);
#20353=ORIENTED_EDGE('',*,*,#14574,.F.);
#20354=ORIENTED_EDGE('',*,*,#14578,.F.);
#20355=ORIENTED_EDGE('',*,*,#14569,.T.);
#20356=ORIENTED_EDGE('',*,*,#14579,.T.);
#20357=ORIENTED_EDGE('',*,*,#14461,.F.);
#20358=ORIENTED_EDGE('',*,*,#14579,.F.);
#20359=ORIENTED_EDGE('',*,*,#14568,.F.);
#20360=ORIENTED_EDGE('',*,*,#14572,.F.);
#20361=ORIENTED_EDGE('',*,*,#14575,.F.);
#20362=ORIENTED_EDGE('',*,*,#14577,.F.);
#20363=ORIENTED_EDGE('',*,*,#14462,.F.);
#20364=ORIENTED_EDGE('',*,*,#14485,.T.);
#20365=ORIENTED_EDGE('',*,*,#13899,.F.);
#20366=ORIENTED_EDGE('',*,*,#14483,.T.);
#20367=ORIENTED_EDGE('',*,*,#13296,.T.);
#20368=ORIENTED_EDGE('',*,*,#14580,.F.);
#20369=ORIENTED_EDGE('',*,*,#14581,.F.);
#20370=ORIENTED_EDGE('',*,*,#14582,.F.);
#20371=ORIENTED_EDGE('',*,*,#14583,.T.);
#20372=ORIENTED_EDGE('',*,*,#14584,.T.);
#20373=ORIENTED_EDGE('',*,*,#14585,.F.);
#20374=ORIENTED_EDGE('',*,*,#14586,.F.);
#20375=ORIENTED_EDGE('',*,*,#14587,.T.);
#20376=ORIENTED_EDGE('',*,*,#14588,.T.);
#20377=ORIENTED_EDGE('',*,*,#14583,.F.);
#20378=ORIENTED_EDGE('',*,*,#14589,.F.);
#20379=ORIENTED_EDGE('',*,*,#14590,.T.);
#20380=ORIENTED_EDGE('',*,*,#14591,.T.);
#20381=ORIENTED_EDGE('',*,*,#14587,.F.);
#20382=ORIENTED_EDGE('',*,*,#14592,.F.);
#20383=ORIENTED_EDGE('',*,*,#14593,.T.);
#20384=ORIENTED_EDGE('',*,*,#14594,.T.);
#20385=ORIENTED_EDGE('',*,*,#14590,.F.);
#20386=ORIENTED_EDGE('',*,*,#14595,.F.);
#20387=ORIENTED_EDGE('',*,*,#14596,.T.);
#20388=ORIENTED_EDGE('',*,*,#14597,.T.);
#20389=ORIENTED_EDGE('',*,*,#14593,.F.);
#20390=ORIENTED_EDGE('',*,*,#14598,.F.);
#20391=ORIENTED_EDGE('',*,*,#14599,.T.);
#20392=ORIENTED_EDGE('',*,*,#14600,.T.);
#20393=ORIENTED_EDGE('',*,*,#14596,.F.);
#20394=ORIENTED_EDGE('',*,*,#14601,.F.);
#20395=ORIENTED_EDGE('',*,*,#14585,.T.);
#20396=ORIENTED_EDGE('',*,*,#14602,.T.);
#20397=ORIENTED_EDGE('',*,*,#14599,.F.);
#20398=ORIENTED_EDGE('',*,*,#14603,.F.);
#20399=ORIENTED_EDGE('',*,*,#14604,.T.);
#20400=ORIENTED_EDGE('',*,*,#14605,.T.);
#20401=ORIENTED_EDGE('',*,*,#14604,.F.);
#20402=ORIENTED_EDGE('',*,*,#14605,.F.);
#20403=ORIENTED_EDGE('',*,*,#14602,.F.);
#20404=ORIENTED_EDGE('',*,*,#14584,.F.);
#20405=ORIENTED_EDGE('',*,*,#14588,.F.);
#20406=ORIENTED_EDGE('',*,*,#14591,.F.);
#20407=ORIENTED_EDGE('',*,*,#14594,.F.);
#20408=ORIENTED_EDGE('',*,*,#14597,.F.);
#20409=ORIENTED_EDGE('',*,*,#14600,.F.);
#20410=ORIENTED_EDGE('',*,*,#14606,.F.);
#20411=ORIENTED_EDGE('',*,*,#14607,.T.);
#20412=ORIENTED_EDGE('',*,*,#14608,.T.);
#20413=ORIENTED_EDGE('',*,*,#14609,.F.);
#20414=ORIENTED_EDGE('',*,*,#14610,.F.);
#20415=ORIENTED_EDGE('',*,*,#14611,.T.);
#20416=ORIENTED_EDGE('',*,*,#14612,.T.);
#20417=ORIENTED_EDGE('',*,*,#14607,.F.);
#20418=ORIENTED_EDGE('',*,*,#14613,.F.);
#20419=ORIENTED_EDGE('',*,*,#14614,.T.);
#20420=ORIENTED_EDGE('',*,*,#14615,.T.);
#20421=ORIENTED_EDGE('',*,*,#14611,.F.);
#20422=ORIENTED_EDGE('',*,*,#14616,.F.);
#20423=ORIENTED_EDGE('',*,*,#14617,.T.);
#20424=ORIENTED_EDGE('',*,*,#14618,.T.);
#20425=ORIENTED_EDGE('',*,*,#14614,.F.);
#20426=ORIENTED_EDGE('',*,*,#14619,.F.);
#20427=ORIENTED_EDGE('',*,*,#14620,.T.);
#20428=ORIENTED_EDGE('',*,*,#14621,.T.);
#20429=ORIENTED_EDGE('',*,*,#14617,.F.);
#20430=ORIENTED_EDGE('',*,*,#14622,.F.);
#20431=ORIENTED_EDGE('',*,*,#14623,.T.);
#20432=ORIENTED_EDGE('',*,*,#14624,.T.);
#20433=ORIENTED_EDGE('',*,*,#14620,.F.);
#20434=ORIENTED_EDGE('',*,*,#14625,.F.);
#20435=ORIENTED_EDGE('',*,*,#14609,.T.);
#20436=ORIENTED_EDGE('',*,*,#14626,.T.);
#20437=ORIENTED_EDGE('',*,*,#14623,.F.);
#20438=ORIENTED_EDGE('',*,*,#14627,.F.);
#20439=ORIENTED_EDGE('',*,*,#14628,.T.);
#20440=ORIENTED_EDGE('',*,*,#14629,.T.);
#20441=ORIENTED_EDGE('',*,*,#14628,.F.);
#20442=ORIENTED_EDGE('',*,*,#14629,.F.);
#20443=ORIENTED_EDGE('',*,*,#14626,.F.);
#20444=ORIENTED_EDGE('',*,*,#14608,.F.);
#20445=ORIENTED_EDGE('',*,*,#14612,.F.);
#20446=ORIENTED_EDGE('',*,*,#14615,.F.);
#20447=ORIENTED_EDGE('',*,*,#14618,.F.);
#20448=ORIENTED_EDGE('',*,*,#14621,.F.);
#20449=ORIENTED_EDGE('',*,*,#14624,.F.);
#20450=ORIENTED_EDGE('',*,*,#14606,.T.);
#20451=ORIENTED_EDGE('',*,*,#14625,.T.);
#20452=ORIENTED_EDGE('',*,*,#14622,.T.);
#20453=ORIENTED_EDGE('',*,*,#14619,.T.);
#20454=ORIENTED_EDGE('',*,*,#14616,.T.);
#20455=ORIENTED_EDGE('',*,*,#14613,.T.);
#20456=ORIENTED_EDGE('',*,*,#14610,.T.);
#20457=ORIENTED_EDGE('',*,*,#14582,.T.);
#20458=ORIENTED_EDGE('',*,*,#14601,.T.);
#20459=ORIENTED_EDGE('',*,*,#14598,.T.);
#20460=ORIENTED_EDGE('',*,*,#14595,.T.);
#20461=ORIENTED_EDGE('',*,*,#14592,.T.);
#20462=ORIENTED_EDGE('',*,*,#14589,.T.);
#20463=ORIENTED_EDGE('',*,*,#14586,.T.);
#20464=ORIENTED_EDGE('',*,*,#14576,.T.);
#20465=ORIENTED_EDGE('',*,*,#14573,.T.);
#20466=ORIENTED_EDGE('',*,*,#14570,.T.);
#20467=ORIENTED_EDGE('',*,*,#14566,.T.);
#20468=ORIENTED_EDGE('',*,*,#14578,.T.);
#20469=ORIENTED_EDGE('',*,*,#14460,.F.);
#20470=ORIENTED_EDGE('',*,*,#14630,.F.);
#20471=ORIENTED_EDGE('',*,*,#14631,.F.);
#20472=ORIENTED_EDGE('',*,*,#14632,.T.);
#20473=ORIENTED_EDGE('',*,*,#14464,.F.);
#20474=ORIENTED_EDGE('',*,*,#14627,.T.);
#20475=ORIENTED_EDGE('',*,*,#14603,.T.);
#20476=ORIENTED_EDGE('',*,*,#13890,.F.);
#20477=ORIENTED_EDGE('',*,*,#14484,.T.);
#20478=ORIENTED_EDGE('',*,*,#13281,.T.);
#20479=ORIENTED_EDGE('',*,*,#14482,.T.);
#20480=ORIENTED_EDGE('',*,*,#13886,.F.);
#20481=ORIENTED_EDGE('',*,*,#14581,.T.);
#20482=ORIENTED_EDGE('',*,*,#14633,.T.);
#20483=ORIENTED_EDGE('',*,*,#14634,.T.);
#20484=ORIENTED_EDGE('',*,*,#14633,.F.);
#20485=ORIENTED_EDGE('',*,*,#14634,.F.);
#20486=ORIENTED_EDGE('',*,*,#14580,.T.);
#20487=ORIENTED_EDGE('',*,*,#14635,.T.);
#20488=ORIENTED_EDGE('',*,*,#14636,.T.);
#20489=ORIENTED_EDGE('',*,*,#14635,.F.);
#20490=ORIENTED_EDGE('',*,*,#14636,.F.);
#20491=ORIENTED_EDGE('',*,*,#14472,.F.);
#20492=ORIENTED_EDGE('',*,*,#14637,.T.);
#20493=ORIENTED_EDGE('',*,*,#14638,.T.);
#20494=ORIENTED_EDGE('',*,*,#14637,.F.);
#20495=ORIENTED_EDGE('',*,*,#14638,.F.);
#20496=ORIENTED_EDGE('',*,*,#14473,.F.);
#20497=ORIENTED_EDGE('',*,*,#14639,.T.);
#20498=ORIENTED_EDGE('',*,*,#14640,.T.);
#20499=ORIENTED_EDGE('',*,*,#14639,.F.);
#20500=ORIENTED_EDGE('',*,*,#14640,.F.);
#20501=ORIENTED_EDGE('',*,*,#14427,.T.);
#20502=ORIENTED_EDGE('',*,*,#14641,.F.);
#20503=ORIENTED_EDGE('',*,*,#14642,.F.);
#20504=ORIENTED_EDGE('',*,*,#14442,.T.);
#20505=ORIENTED_EDGE('',*,*,#14430,.T.);
#20506=ORIENTED_EDGE('',*,*,#14440,.F.);
#20507=ORIENTED_EDGE('',*,*,#14643,.F.);
#20508=ORIENTED_EDGE('',*,*,#14641,.T.);
#20509=ORIENTED_EDGE('',*,*,#14644,.T.);
#20510=ORIENTED_EDGE('',*,*,#14438,.T.);
#20511=ORIENTED_EDGE('',*,*,#14471,.F.);
#20512=ORIENTED_EDGE('',*,*,#14645,.F.);
#20513=ORIENTED_EDGE('',*,*,#14646,.F.);
#20514=ORIENTED_EDGE('',*,*,#14645,.T.);
#20515=ORIENTED_EDGE('',*,*,#14470,.F.);
#20516=ORIENTED_EDGE('',*,*,#14647,.F.);
#20517=ORIENTED_EDGE('',*,*,#14648,.F.);
#20518=ORIENTED_EDGE('',*,*,#14647,.T.);
#20519=ORIENTED_EDGE('',*,*,#14469,.F.);
#20520=ORIENTED_EDGE('',*,*,#14649,.F.);
#20521=ORIENTED_EDGE('',*,*,#14650,.F.);
#20522=ORIENTED_EDGE('',*,*,#14649,.T.);
#20523=ORIENTED_EDGE('',*,*,#14468,.F.);
#20524=ORIENTED_EDGE('',*,*,#14651,.F.);
#20525=ORIENTED_EDGE('',*,*,#14652,.F.);
#20526=ORIENTED_EDGE('',*,*,#14651,.T.);
#20527=ORIENTED_EDGE('',*,*,#14467,.F.);
#20528=ORIENTED_EDGE('',*,*,#14653,.F.);
#20529=ORIENTED_EDGE('',*,*,#14654,.F.);
#20530=ORIENTED_EDGE('',*,*,#14653,.T.);
#20531=ORIENTED_EDGE('',*,*,#14466,.F.);
#20532=ORIENTED_EDGE('',*,*,#14655,.F.);
#20533=ORIENTED_EDGE('',*,*,#14656,.F.);
#20534=ORIENTED_EDGE('',*,*,#14655,.T.);
#20535=ORIENTED_EDGE('',*,*,#14465,.F.);
#20536=ORIENTED_EDGE('',*,*,#14632,.F.);
#20537=ORIENTED_EDGE('',*,*,#14657,.F.);
#20538=ORIENTED_EDGE('',*,*,#14630,.T.);
#20539=ORIENTED_EDGE('',*,*,#14459,.F.);
#20540=ORIENTED_EDGE('',*,*,#14658,.F.);
#20541=ORIENTED_EDGE('',*,*,#14659,.F.);
#20542=ORIENTED_EDGE('',*,*,#14658,.T.);
#20543=ORIENTED_EDGE('',*,*,#14458,.F.);
#20544=ORIENTED_EDGE('',*,*,#14660,.F.);
#20545=ORIENTED_EDGE('',*,*,#14661,.F.);
#20546=ORIENTED_EDGE('',*,*,#14660,.T.);
#20547=ORIENTED_EDGE('',*,*,#14457,.F.);
#20548=ORIENTED_EDGE('',*,*,#14662,.F.);
#20549=ORIENTED_EDGE('',*,*,#14532,.T.);
#20550=ORIENTED_EDGE('',*,*,#14452,.F.);
#20551=ORIENTED_EDGE('',*,*,#14663,.F.);
#20552=ORIENTED_EDGE('',*,*,#14664,.T.);
#20553=ORIENTED_EDGE('',*,*,#14662,.T.);
#20554=ORIENTED_EDGE('',*,*,#14456,.F.);
#20555=ORIENTED_EDGE('',*,*,#14534,.T.);
#20556=ORIENTED_EDGE('',*,*,#14522,.T.);
#20557=ORIENTED_EDGE('',*,*,#14526,.T.);
#20558=ORIENTED_EDGE('',*,*,#14529,.T.);
#20559=ORIENTED_EDGE('',*,*,#14561,.T.);
#20560=ORIENTED_EDGE('',*,*,#14521,.T.);
#20561=ORIENTED_EDGE('',*,*,#14665,.F.);
#20562=ORIENTED_EDGE('',*,*,#14663,.T.);
#20563=ORIENTED_EDGE('',*,*,#14451,.F.);
#20564=ORIENTED_EDGE('',*,*,#14666,.F.);
#20565=ORIENTED_EDGE('',*,*,#14667,.T.);
#20566=ORIENTED_EDGE('',*,*,#14666,.T.);
#20567=ORIENTED_EDGE('',*,*,#14450,.F.);
#20568=ORIENTED_EDGE('',*,*,#14668,.F.);
#20569=ORIENTED_EDGE('',*,*,#14669,.F.);
#20570=ORIENTED_EDGE('',*,*,#14668,.T.);
#20571=ORIENTED_EDGE('',*,*,#14449,.F.);
#20572=ORIENTED_EDGE('',*,*,#14670,.F.);
#20573=ORIENTED_EDGE('',*,*,#14671,.T.);
#20574=ORIENTED_EDGE('',*,*,#14670,.T.);
#20575=ORIENTED_EDGE('',*,*,#14448,.F.);
#20576=ORIENTED_EDGE('',*,*,#14672,.F.);
#20577=ORIENTED_EDGE('',*,*,#14673,.F.);
#20578=ORIENTED_EDGE('',*,*,#14672,.T.);
#20579=ORIENTED_EDGE('',*,*,#14447,.F.);
#20580=ORIENTED_EDGE('',*,*,#14674,.F.);
#20581=ORIENTED_EDGE('',*,*,#14675,.T.);
#20582=ORIENTED_EDGE('',*,*,#14674,.T.);
#20583=ORIENTED_EDGE('',*,*,#14446,.F.);
#20584=ORIENTED_EDGE('',*,*,#14676,.F.);
#20585=ORIENTED_EDGE('',*,*,#14677,.T.);
#20586=ORIENTED_EDGE('',*,*,#14676,.T.);
#20587=ORIENTED_EDGE('',*,*,#14445,.F.);
#20588=ORIENTED_EDGE('',*,*,#14678,.F.);
#20589=ORIENTED_EDGE('',*,*,#14416,.T.);
#20590=ORIENTED_EDGE('',*,*,#14679,.F.);
#20591=ORIENTED_EDGE('',*,*,#14680,.T.);
#20592=ORIENTED_EDGE('',*,*,#14678,.T.);
#20593=ORIENTED_EDGE('',*,*,#14444,.F.);
#20594=ORIENTED_EDGE('',*,*,#14415,.T.);
#20595=ORIENTED_EDGE('',*,*,#14419,.T.);
#20596=ORIENTED_EDGE('',*,*,#14436,.F.);
#20597=ORIENTED_EDGE('',*,*,#14681,.F.);
#20598=ORIENTED_EDGE('',*,*,#14679,.T.);
#20599=ORIENTED_EDGE('',*,*,#14681,.T.);
#20600=ORIENTED_EDGE('',*,*,#14435,.F.);
#20601=ORIENTED_EDGE('',*,*,#14443,.T.);
#20602=ORIENTED_EDGE('',*,*,#14642,.T.);
#20603=ORIENTED_EDGE('',*,*,#14643,.T.);
#20604=ORIENTED_EDGE('',*,*,#14439,.T.);
#20605=ORIENTED_EDGE('',*,*,#14644,.F.);
#20606=ORIENTED_EDGE('',*,*,#14646,.T.);
#20607=ORIENTED_EDGE('',*,*,#14648,.T.);
#20608=ORIENTED_EDGE('',*,*,#14650,.T.);
#20609=ORIENTED_EDGE('',*,*,#14652,.T.);
#20610=ORIENTED_EDGE('',*,*,#14654,.T.);
#20611=ORIENTED_EDGE('',*,*,#14656,.T.);
#20612=ORIENTED_EDGE('',*,*,#14631,.T.);
#20613=ORIENTED_EDGE('',*,*,#14657,.T.);
#20614=ORIENTED_EDGE('',*,*,#14659,.T.);
#20615=ORIENTED_EDGE('',*,*,#14661,.T.);
#20616=ORIENTED_EDGE('',*,*,#14664,.F.);
#20617=ORIENTED_EDGE('',*,*,#14665,.T.);
#20618=ORIENTED_EDGE('',*,*,#14667,.F.);
#20619=ORIENTED_EDGE('',*,*,#14669,.T.);
#20620=ORIENTED_EDGE('',*,*,#14671,.F.);
#20621=ORIENTED_EDGE('',*,*,#14673,.T.);
#20622=ORIENTED_EDGE('',*,*,#14675,.F.);
#20623=ORIENTED_EDGE('',*,*,#14677,.F.);
#20624=ORIENTED_EDGE('',*,*,#14680,.F.);
#20625=ORIENTED_EDGE('',*,*,#14491,.T.);
#20626=ORIENTED_EDGE('',*,*,#14360,.T.);
#20627=ORIENTED_EDGE('',*,*,#14490,.T.);
#20628=ORIENTED_EDGE('',*,*,#13453,.T.);
#20629=ORIENTED_EDGE('',*,*,#14493,.T.);
#20630=ORIENTED_EDGE('',*,*,#14245,.T.);
#20631=ORIENTED_EDGE('',*,*,#14492,.T.);
#20632=ORIENTED_EDGE('',*,*,#13590,.T.);
#20633=ORIENTED_EDGE('',*,*,#14495,.T.);
#20634=ORIENTED_EDGE('',*,*,#14130,.T.);
#20635=ORIENTED_EDGE('',*,*,#14494,.T.);
#20636=ORIENTED_EDGE('',*,*,#13727,.T.);
#20637=ORIENTED_EDGE('',*,*,#14497,.T.);
#20638=ORIENTED_EDGE('',*,*,#14015,.T.);
#20639=ORIENTED_EDGE('',*,*,#14496,.T.);
#20640=ORIENTED_EDGE('',*,*,#13864,.T.);
#20641=ORIENTED_EDGE('',*,*,#14682,.F.);
#20642=ORIENTED_EDGE('',*,*,#14683,.T.);
#20643=ORIENTED_EDGE('',*,*,#14684,.F.);
#20644=ORIENTED_EDGE('',*,*,#14683,.F.);
#20645=ORIENTED_EDGE('',*,*,#14682,.T.);
#20646=ORIENTED_EDGE('',*,*,#14685,.F.);
#20647=ORIENTED_EDGE('',*,*,#14686,.T.);
#20648=ORIENTED_EDGE('',*,*,#14687,.T.);
#20649=ORIENTED_EDGE('',*,*,#14686,.F.);
#20650=ORIENTED_EDGE('',*,*,#14687,.F.);
#20651=ORIENTED_EDGE('',*,*,#14688,.T.);
#20652=ORIENTED_EDGE('',*,*,#14689,.T.);
#20653=ORIENTED_EDGE('',*,*,#14690,.T.);
#20654=ORIENTED_EDGE('',*,*,#14691,.T.);
#20655=ORIENTED_EDGE('',*,*,#14689,.F.);
#20656=ORIENTED_EDGE('',*,*,#14692,.T.);
#20657=ORIENTED_EDGE('',*,*,#14693,.T.);
#20658=ORIENTED_EDGE('',*,*,#14694,.T.);
#20659=ORIENTED_EDGE('',*,*,#14695,.T.);
#20660=ORIENTED_EDGE('',*,*,#14696,.T.);
#20661=ORIENTED_EDGE('',*,*,#14697,.T.);
#20662=ORIENTED_EDGE('',*,*,#14698,.T.);
#20663=ORIENTED_EDGE('',*,*,#14699,.T.);
#20664=ORIENTED_EDGE('',*,*,#14700,.T.);
#20665=ORIENTED_EDGE('',*,*,#14697,.F.);
#20666=ORIENTED_EDGE('',*,*,#14701,.T.);
#20667=ORIENTED_EDGE('',*,*,#14702,.T.);
#20668=ORIENTED_EDGE('',*,*,#14703,.T.);
#20669=ORIENTED_EDGE('',*,*,#14699,.F.);
#20670=ORIENTED_EDGE('',*,*,#14704,.T.);
#20671=ORIENTED_EDGE('',*,*,#14705,.T.);
#20672=ORIENTED_EDGE('',*,*,#14706,.T.);
#20673=ORIENTED_EDGE('',*,*,#14702,.F.);
#20674=ORIENTED_EDGE('',*,*,#14707,.T.);
#20675=ORIENTED_EDGE('',*,*,#14708,.T.);
#20676=ORIENTED_EDGE('',*,*,#14709,.T.);
#20677=ORIENTED_EDGE('',*,*,#14705,.F.);
#20678=ORIENTED_EDGE('',*,*,#14710,.T.);
#20679=ORIENTED_EDGE('',*,*,#14711,.T.);
#20680=ORIENTED_EDGE('',*,*,#14712,.T.);
#20681=ORIENTED_EDGE('',*,*,#14708,.F.);
#20682=ORIENTED_EDGE('',*,*,#14713,.T.);
#20683=ORIENTED_EDGE('',*,*,#14714,.T.);
#20684=ORIENTED_EDGE('',*,*,#14715,.T.);
#20685=ORIENTED_EDGE('',*,*,#14711,.F.);
#20686=ORIENTED_EDGE('',*,*,#14716,.T.);
#20687=ORIENTED_EDGE('',*,*,#14717,.T.);
#20688=ORIENTED_EDGE('',*,*,#14718,.T.);
#20689=ORIENTED_EDGE('',*,*,#14714,.F.);
#20690=ORIENTED_EDGE('',*,*,#14719,.T.);
#20691=ORIENTED_EDGE('',*,*,#14720,.T.);
#20692=ORIENTED_EDGE('',*,*,#14717,.F.);
#20693=ORIENTED_EDGE('',*,*,#14721,.T.);
#20694=ORIENTED_EDGE('',*,*,#14722,.T.);
#20695=ORIENTED_EDGE('',*,*,#14723,.T.);
#20696=ORIENTED_EDGE('',*,*,#14722,.F.);
#20697=ORIENTED_EDGE('',*,*,#14724,.T.);
#20698=ORIENTED_EDGE('',*,*,#14725,.T.);
#20699=ORIENTED_EDGE('',*,*,#14726,.T.);
#20700=ORIENTED_EDGE('',*,*,#14727,.T.);
#20701=ORIENTED_EDGE('',*,*,#14728,.T.);
#20702=ORIENTED_EDGE('',*,*,#14725,.F.);
#20703=ORIENTED_EDGE('',*,*,#14729,.T.);
#20704=ORIENTED_EDGE('',*,*,#14730,.T.);
#20705=ORIENTED_EDGE('',*,*,#14727,.F.);
#20706=ORIENTED_EDGE('',*,*,#14731,.T.);
#20707=ORIENTED_EDGE('',*,*,#14732,.T.);
#20708=ORIENTED_EDGE('',*,*,#14729,.F.);
#20709=ORIENTED_EDGE('',*,*,#14733,.T.);
#20710=ORIENTED_EDGE('',*,*,#14734,.T.);
#20711=ORIENTED_EDGE('',*,*,#14693,.F.);
#20712=ORIENTED_EDGE('',*,*,#14735,.T.);
#20713=ORIENTED_EDGE('',*,*,#14734,.F.);
#20714=ORIENTED_EDGE('',*,*,#14736,.T.);
#20715=ORIENTED_EDGE('',*,*,#14737,.T.);
#20716=ORIENTED_EDGE('',*,*,#14738,.T.);
#20717=ORIENTED_EDGE('',*,*,#14739,.T.);
#20718=ORIENTED_EDGE('',*,*,#14691,.F.);
#20719=ORIENTED_EDGE('',*,*,#14740,.T.);
#20720=ORIENTED_EDGE('',*,*,#14741,.T.);
#20721=ORIENTED_EDGE('',*,*,#14738,.F.);
#20722=ORIENTED_EDGE('',*,*,#14742,.T.);
#20723=ORIENTED_EDGE('',*,*,#14743,.T.);
#20724=ORIENTED_EDGE('',*,*,#14740,.F.);
#20725=ORIENTED_EDGE('',*,*,#14744,.T.);
#20726=ORIENTED_EDGE('',*,*,#14745,.T.);
#20727=ORIENTED_EDGE('',*,*,#14746,.T.);
#20728=ORIENTED_EDGE('',*,*,#14747,.T.);
#20729=ORIENTED_EDGE('',*,*,#14748,.T.);
#20730=ORIENTED_EDGE('',*,*,#14745,.F.);
#20731=ORIENTED_EDGE('',*,*,#14749,.T.);
#20732=ORIENTED_EDGE('',*,*,#14750,.T.);
#20733=ORIENTED_EDGE('',*,*,#14751,.T.);
#20734=ORIENTED_EDGE('',*,*,#14747,.F.);
#20735=ORIENTED_EDGE('',*,*,#14752,.T.);
#20736=ORIENTED_EDGE('',*,*,#14753,.T.);
#20737=ORIENTED_EDGE('',*,*,#14750,.F.);
#20738=ORIENTED_EDGE('',*,*,#14754,.T.);
#20739=ORIENTED_EDGE('',*,*,#14755,.T.);
#20740=ORIENTED_EDGE('',*,*,#14756,.T.);
#20741=ORIENTED_EDGE('',*,*,#14752,.F.);
#20742=ORIENTED_EDGE('',*,*,#14757,.T.);
#20743=ORIENTED_EDGE('',*,*,#14758,.T.);
#20744=ORIENTED_EDGE('',*,*,#14759,.T.);
#20745=ORIENTED_EDGE('',*,*,#14755,.F.);
#20746=ORIENTED_EDGE('',*,*,#14760,.T.);
#20747=ORIENTED_EDGE('',*,*,#14761,.T.);
#20748=ORIENTED_EDGE('',*,*,#14762,.T.);
#20749=ORIENTED_EDGE('',*,*,#14758,.F.);
#20750=ORIENTED_EDGE('',*,*,#14763,.T.);
#20751=ORIENTED_EDGE('',*,*,#14764,.T.);
#20752=ORIENTED_EDGE('',*,*,#14765,.T.);
#20753=ORIENTED_EDGE('',*,*,#14761,.F.);
#20754=ORIENTED_EDGE('',*,*,#14766,.T.);
#20755=ORIENTED_EDGE('',*,*,#14767,.T.);
#20756=ORIENTED_EDGE('',*,*,#14768,.T.);
#20757=ORIENTED_EDGE('',*,*,#14764,.F.);
#20758=ORIENTED_EDGE('',*,*,#14769,.T.);
#20759=ORIENTED_EDGE('',*,*,#14770,.T.);
#20760=ORIENTED_EDGE('',*,*,#14771,.T.);
#20761=ORIENTED_EDGE('',*,*,#14767,.F.);
#20762=ORIENTED_EDGE('',*,*,#14772,.T.);
#20763=ORIENTED_EDGE('',*,*,#14773,.T.);
#20764=ORIENTED_EDGE('',*,*,#14774,.T.);
#20765=ORIENTED_EDGE('',*,*,#14770,.F.);
#20766=ORIENTED_EDGE('',*,*,#14775,.T.);
#20767=ORIENTED_EDGE('',*,*,#14776,.T.);
#20768=ORIENTED_EDGE('',*,*,#14777,.T.);
#20769=ORIENTED_EDGE('',*,*,#14778,.T.);
#20770=ORIENTED_EDGE('',*,*,#14779,.T.);
#20771=ORIENTED_EDGE('',*,*,#14776,.F.);
#20772=ORIENTED_EDGE('',*,*,#14780,.T.);
#20773=ORIENTED_EDGE('',*,*,#14781,.T.);
#20774=ORIENTED_EDGE('',*,*,#14782,.T.);
#20775=ORIENTED_EDGE('',*,*,#14781,.F.);
#20776=ORIENTED_EDGE('',*,*,#14783,.T.);
#20777=ORIENTED_EDGE('',*,*,#14784,.T.);
#20778=ORIENTED_EDGE('',*,*,#14785,.T.);
#20779=ORIENTED_EDGE('',*,*,#14784,.F.);
#20780=ORIENTED_EDGE('',*,*,#14786,.T.);
#20781=ORIENTED_EDGE('',*,*,#14773,.F.);
#20782=ORIENTED_EDGE('',*,*,#14695,.F.);
#20783=ORIENTED_EDGE('',*,*,#14787,.T.);
#20784=ORIENTED_EDGE('',*,*,#14778,.F.);
#20785=ORIENTED_EDGE('',*,*,#14739,.F.);
#20786=ORIENTED_EDGE('',*,*,#14788,.T.);
#20787=ORIENTED_EDGE('',*,*,#14789,.F.);
#20788=ORIENTED_EDGE('',*,*,#14790,.F.);
#20789=ORIENTED_EDGE('',*,*,#14741,.F.);
#20790=ORIENTED_EDGE('',*,*,#14791,.T.);
#20791=ORIENTED_EDGE('',*,*,#14792,.F.);
#20792=ORIENTED_EDGE('',*,*,#14788,.F.);
#20793=ORIENTED_EDGE('',*,*,#14743,.F.);
#20794=ORIENTED_EDGE('',*,*,#14793,.T.);
#20795=ORIENTED_EDGE('',*,*,#14794,.F.);
#20796=ORIENTED_EDGE('',*,*,#14791,.F.);
#20797=ORIENTED_EDGE('',*,*,#14748,.F.);
#20798=ORIENTED_EDGE('',*,*,#14795,.T.);
#20799=ORIENTED_EDGE('',*,*,#14796,.F.);
#20800=ORIENTED_EDGE('',*,*,#14793,.F.);
#20801=ORIENTED_EDGE('',*,*,#14751,.F.);
#20802=ORIENTED_EDGE('',*,*,#14797,.T.);
#20803=ORIENTED_EDGE('',*,*,#14798,.F.);
#20804=ORIENTED_EDGE('',*,*,#14795,.F.);
#20805=ORIENTED_EDGE('',*,*,#14753,.F.);
#20806=ORIENTED_EDGE('',*,*,#14799,.T.);
#20807=ORIENTED_EDGE('',*,*,#14800,.F.);
#20808=ORIENTED_EDGE('',*,*,#14797,.F.);
#20809=ORIENTED_EDGE('',*,*,#14756,.F.);
#20810=ORIENTED_EDGE('',*,*,#14801,.T.);
#20811=ORIENTED_EDGE('',*,*,#14802,.F.);
#20812=ORIENTED_EDGE('',*,*,#14799,.F.);
#20813=ORIENTED_EDGE('',*,*,#14685,.T.);
#20814=ORIENTED_EDGE('',*,*,#14759,.F.);
#20815=ORIENTED_EDGE('',*,*,#14803,.T.);
#20816=ORIENTED_EDGE('',*,*,#14804,.F.);
#20817=ORIENTED_EDGE('',*,*,#14801,.F.);
#20818=ORIENTED_EDGE('',*,*,#14762,.F.);
#20819=ORIENTED_EDGE('',*,*,#14805,.T.);
#20820=ORIENTED_EDGE('',*,*,#14806,.F.);
#20821=ORIENTED_EDGE('',*,*,#14803,.F.);
#20822=ORIENTED_EDGE('',*,*,#14765,.F.);
#20823=ORIENTED_EDGE('',*,*,#14807,.T.);
#20824=ORIENTED_EDGE('',*,*,#14808,.T.);
#20825=ORIENTED_EDGE('',*,*,#14809,.T.);
#20826=ORIENTED_EDGE('',*,*,#14810,.F.);
#20827=ORIENTED_EDGE('',*,*,#14805,.F.);
#20828=ORIENTED_EDGE('',*,*,#14768,.F.);
#20829=ORIENTED_EDGE('',*,*,#14811,.T.);
#20830=ORIENTED_EDGE('',*,*,#14812,.T.);
#20831=ORIENTED_EDGE('',*,*,#14807,.F.);
#20832=ORIENTED_EDGE('',*,*,#14771,.F.);
#20833=ORIENTED_EDGE('',*,*,#14813,.T.);
#20834=ORIENTED_EDGE('',*,*,#14814,.T.);
#20835=ORIENTED_EDGE('',*,*,#14811,.F.);
#20836=ORIENTED_EDGE('',*,*,#14774,.F.);
#20837=ORIENTED_EDGE('',*,*,#14815,.T.);
#20838=ORIENTED_EDGE('',*,*,#14816,.F.);
#20839=ORIENTED_EDGE('',*,*,#14817,.T.);
#20840=ORIENTED_EDGE('',*,*,#14818,.T.);
#20841=ORIENTED_EDGE('',*,*,#14813,.F.);
#20842=ORIENTED_EDGE('',*,*,#14786,.F.);
#20843=ORIENTED_EDGE('',*,*,#14819,.T.);
#20844=ORIENTED_EDGE('',*,*,#14820,.F.);
#20845=ORIENTED_EDGE('',*,*,#14815,.F.);
#20846=ORIENTED_EDGE('',*,*,#14783,.F.);
#20847=ORIENTED_EDGE('',*,*,#14821,.T.);
#20848=ORIENTED_EDGE('',*,*,#14822,.F.);
#20849=ORIENTED_EDGE('',*,*,#14819,.F.);
#20850=ORIENTED_EDGE('',*,*,#14780,.F.);
#20851=ORIENTED_EDGE('',*,*,#14823,.T.);
#20852=ORIENTED_EDGE('',*,*,#14824,.F.);
#20853=ORIENTED_EDGE('',*,*,#14821,.F.);
#20854=ORIENTED_EDGE('',*,*,#14779,.F.);
#20855=ORIENTED_EDGE('',*,*,#14825,.T.);
#20856=ORIENTED_EDGE('',*,*,#14826,.F.);
#20857=ORIENTED_EDGE('',*,*,#14823,.F.);
#20858=ORIENTED_EDGE('',*,*,#14696,.F.);
#20859=ORIENTED_EDGE('',*,*,#14777,.F.);
#20860=ORIENTED_EDGE('',*,*,#14782,.F.);
#20861=ORIENTED_EDGE('',*,*,#14785,.F.);
#20862=ORIENTED_EDGE('',*,*,#14775,.F.);
#20863=ORIENTED_EDGE('',*,*,#14772,.F.);
#20864=ORIENTED_EDGE('',*,*,#14769,.F.);
#20865=ORIENTED_EDGE('',*,*,#14766,.F.);
#20866=ORIENTED_EDGE('',*,*,#14763,.F.);
#20867=ORIENTED_EDGE('',*,*,#14760,.F.);
#20868=ORIENTED_EDGE('',*,*,#14757,.F.);
#20869=ORIENTED_EDGE('',*,*,#14754,.F.);
#20870=ORIENTED_EDGE('',*,*,#14749,.F.);
#20871=ORIENTED_EDGE('',*,*,#14746,.F.);
#20872=ORIENTED_EDGE('',*,*,#14744,.F.);
#20873=ORIENTED_EDGE('',*,*,#14742,.F.);
#20874=ORIENTED_EDGE('',*,*,#14737,.F.);
#20875=ORIENTED_EDGE('',*,*,#14690,.F.);
#20876=ORIENTED_EDGE('',*,*,#14694,.F.);
#20877=ORIENTED_EDGE('',*,*,#14736,.F.);
#20878=ORIENTED_EDGE('',*,*,#14733,.F.);
#20879=ORIENTED_EDGE('',*,*,#14731,.F.);
#20880=ORIENTED_EDGE('',*,*,#14726,.F.);
#20881=ORIENTED_EDGE('',*,*,#14724,.F.);
#20882=ORIENTED_EDGE('',*,*,#14721,.F.);
#20883=ORIENTED_EDGE('',*,*,#14719,.F.);
#20884=ORIENTED_EDGE('',*,*,#14716,.F.);
#20885=ORIENTED_EDGE('',*,*,#14713,.F.);
#20886=ORIENTED_EDGE('',*,*,#14710,.F.);
#20887=ORIENTED_EDGE('',*,*,#14707,.F.);
#20888=ORIENTED_EDGE('',*,*,#14704,.F.);
#20889=ORIENTED_EDGE('',*,*,#14701,.F.);
#20890=ORIENTED_EDGE('',*,*,#14816,.T.);
#20891=ORIENTED_EDGE('',*,*,#14827,.T.);
#20892=ORIENTED_EDGE('',*,*,#14828,.T.);
#20893=ORIENTED_EDGE('',*,*,#14829,.T.);
#20894=ORIENTED_EDGE('',*,*,#14830,.T.);
#20895=ORIENTED_EDGE('',*,*,#14831,.T.);
#20896=ORIENTED_EDGE('',*,*,#14832,.T.);
#20897=ORIENTED_EDGE('',*,*,#14833,.T.);
#20898=ORIENTED_EDGE('',*,*,#14829,.F.);
#20899=ORIENTED_EDGE('',*,*,#14834,.T.);
#20900=ORIENTED_EDGE('',*,*,#14835,.T.);
#20901=ORIENTED_EDGE('',*,*,#14836,.T.);
#20902=ORIENTED_EDGE('',*,*,#14822,.T.);
#20903=ORIENTED_EDGE('',*,*,#14837,.T.);
#20904=ORIENTED_EDGE('',*,*,#14838,.T.);
#20905=ORIENTED_EDGE('',*,*,#14834,.F.);
#20906=ORIENTED_EDGE('',*,*,#14824,.T.);
#20907=ORIENTED_EDGE('',*,*,#14837,.F.);
#20908=ORIENTED_EDGE('',*,*,#14826,.T.);
#20909=ORIENTED_EDGE('',*,*,#14839,.T.);
#20910=ORIENTED_EDGE('',*,*,#14840,.T.);
#20911=ORIENTED_EDGE('',*,*,#14836,.F.);
#20912=ORIENTED_EDGE('',*,*,#14827,.F.);
#20913=ORIENTED_EDGE('',*,*,#14820,.T.);
#20914=ORIENTED_EDGE('',*,*,#14841,.T.);
#20915=ORIENTED_EDGE('',*,*,#14842,.T.);
#20916=ORIENTED_EDGE('',*,*,#14843,.T.);
#20917=ORIENTED_EDGE('',*,*,#14844,.T.);
#20918=ORIENTED_EDGE('',*,*,#14845,.T.);
#20919=ORIENTED_EDGE('',*,*,#14846,.T.);
#20920=ORIENTED_EDGE('',*,*,#14847,.T.);
#20921=ORIENTED_EDGE('',*,*,#14848,.T.);
#20922=ORIENTED_EDGE('',*,*,#14845,.F.);
#20923=ORIENTED_EDGE('',*,*,#14847,.F.);
#20924=ORIENTED_EDGE('',*,*,#14839,.F.);
#20925=ORIENTED_EDGE('',*,*,#14849,.T.);
#20926=ORIENTED_EDGE('',*,*,#14831,.F.);
#20927=ORIENTED_EDGE('',*,*,#14850,.T.);
#20928=ORIENTED_EDGE('',*,*,#14851,.F.);
#20929=ORIENTED_EDGE('',*,*,#14806,.T.);
#20930=ORIENTED_EDGE('',*,*,#14852,.T.);
#20931=ORIENTED_EDGE('',*,*,#14830,.F.);
#20932=ORIENTED_EDGE('',*,*,#14828,.F.);
#20933=ORIENTED_EDGE('',*,*,#14835,.F.);
#20934=ORIENTED_EDGE('',*,*,#14838,.F.);
#20935=ORIENTED_EDGE('',*,*,#14840,.F.);
#20936=ORIENTED_EDGE('',*,*,#14846,.F.);
#20937=ORIENTED_EDGE('',*,*,#14844,.F.);
#20938=ORIENTED_EDGE('',*,*,#14853,.F.);
#20939=ORIENTED_EDGE('',*,*,#14854,.F.);
#20940=ORIENTED_EDGE('',*,*,#14855,.F.);
#20941=ORIENTED_EDGE('',*,*,#14856,.F.);
#20942=ORIENTED_EDGE('',*,*,#14857,.F.);
#20943=ORIENTED_EDGE('',*,*,#14858,.F.);
#20944=ORIENTED_EDGE('',*,*,#14859,.F.);
#20945=ORIENTED_EDGE('',*,*,#14860,.F.);
#20946=ORIENTED_EDGE('',*,*,#14861,.F.);
#20947=ORIENTED_EDGE('',*,*,#14862,.F.);
#20948=ORIENTED_EDGE('',*,*,#14863,.F.);
#20949=ORIENTED_EDGE('',*,*,#14864,.F.);
#20950=ORIENTED_EDGE('',*,*,#14865,.F.);
#20951=ORIENTED_EDGE('',*,*,#14866,.F.);
#20952=ORIENTED_EDGE('',*,*,#14867,.F.);
#20953=ORIENTED_EDGE('',*,*,#14868,.F.);
#20954=ORIENTED_EDGE('',*,*,#14869,.F.);
#20955=ORIENTED_EDGE('',*,*,#14870,.F.);
#20956=ORIENTED_EDGE('',*,*,#14871,.F.);
#20957=ORIENTED_EDGE('',*,*,#14872,.F.);
#20958=ORIENTED_EDGE('',*,*,#14850,.F.);
#20959=ORIENTED_EDGE('',*,*,#14843,.F.);
#20960=ORIENTED_EDGE('',*,*,#14873,.F.);
#20961=ORIENTED_EDGE('',*,*,#14874,.T.);
#20962=ORIENTED_EDGE('',*,*,#14875,.T.);
#20963=ORIENTED_EDGE('',*,*,#14853,.T.);
#20964=ORIENTED_EDGE('',*,*,#14842,.F.);
#20965=ORIENTED_EDGE('',*,*,#14876,.T.);
#20966=ORIENTED_EDGE('',*,*,#14873,.T.);
#20967=ORIENTED_EDGE('',*,*,#14798,.T.);
#20968=ORIENTED_EDGE('',*,*,#14877,.T.);
#20969=ORIENTED_EDGE('',*,*,#14869,.T.);
#20970=ORIENTED_EDGE('',*,*,#14878,.T.);
#20971=ORIENTED_EDGE('',*,*,#14879,.T.);
#20972=ORIENTED_EDGE('',*,*,#14870,.T.);
#20973=ORIENTED_EDGE('',*,*,#14877,.F.);
#20974=ORIENTED_EDGE('',*,*,#14800,.T.);
#20975=ORIENTED_EDGE('',*,*,#14880,.T.);
#20976=ORIENTED_EDGE('',*,*,#14871,.T.);
#20977=ORIENTED_EDGE('',*,*,#14879,.F.);
#20978=ORIENTED_EDGE('',*,*,#14802,.T.);
#20979=ORIENTED_EDGE('',*,*,#14851,.T.);
#20980=ORIENTED_EDGE('',*,*,#14872,.T.);
#20981=ORIENTED_EDGE('',*,*,#14880,.F.);
#20982=ORIENTED_EDGE('',*,*,#14804,.T.);
#20983=ORIENTED_EDGE('',*,*,#14832,.F.);
#20984=ORIENTED_EDGE('',*,*,#14852,.F.);
#20985=ORIENTED_EDGE('',*,*,#14810,.T.);
#20986=ORIENTED_EDGE('',*,*,#14796,.T.);
#20987=ORIENTED_EDGE('',*,*,#14878,.F.);
#20988=ORIENTED_EDGE('',*,*,#14868,.T.);
#20989=ORIENTED_EDGE('',*,*,#14881,.T.);
#20990=ORIENTED_EDGE('',*,*,#14789,.T.);
#20991=ORIENTED_EDGE('',*,*,#14882,.T.);
#20992=ORIENTED_EDGE('',*,*,#14865,.T.);
#20993=ORIENTED_EDGE('',*,*,#14883,.T.);
#20994=ORIENTED_EDGE('',*,*,#14884,.T.);
#20995=ORIENTED_EDGE('',*,*,#14866,.T.);
#20996=ORIENTED_EDGE('',*,*,#14882,.F.);
#20997=ORIENTED_EDGE('',*,*,#14792,.T.);
#20998=ORIENTED_EDGE('',*,*,#14867,.T.);
#20999=ORIENTED_EDGE('',*,*,#14884,.F.);
#21000=ORIENTED_EDGE('',*,*,#14794,.T.);
#21001=ORIENTED_EDGE('',*,*,#14881,.F.);
#21002=ORIENTED_EDGE('',*,*,#14885,.T.);
#21003=ORIENTED_EDGE('',*,*,#14886,.T.);
#21004=ORIENTED_EDGE('',*,*,#14862,.T.);
#21005=ORIENTED_EDGE('',*,*,#14887,.T.);
#21006=ORIENTED_EDGE('',*,*,#14888,.T.);
#21007=ORIENTED_EDGE('',*,*,#14863,.T.);
#21008=ORIENTED_EDGE('',*,*,#14886,.F.);
#21009=ORIENTED_EDGE('',*,*,#14889,.T.);
#21010=ORIENTED_EDGE('',*,*,#14864,.T.);
#21011=ORIENTED_EDGE('',*,*,#14888,.F.);
#21012=ORIENTED_EDGE('',*,*,#14890,.T.);
#21013=ORIENTED_EDGE('',*,*,#14883,.F.);
#21014=ORIENTED_EDGE('',*,*,#14891,.T.);
#21015=ORIENTED_EDGE('',*,*,#14892,.T.);
#21016=ORIENTED_EDGE('',*,*,#14859,.T.);
#21017=ORIENTED_EDGE('',*,*,#14893,.T.);
#21018=ORIENTED_EDGE('',*,*,#14894,.T.);
#21019=ORIENTED_EDGE('',*,*,#14860,.T.);
#21020=ORIENTED_EDGE('',*,*,#14892,.F.);
#21021=ORIENTED_EDGE('',*,*,#14895,.T.);
#21022=ORIENTED_EDGE('',*,*,#14861,.T.);
#21023=ORIENTED_EDGE('',*,*,#14894,.F.);
#21024=ORIENTED_EDGE('',*,*,#14896,.T.);
#21025=ORIENTED_EDGE('',*,*,#14887,.F.);
#21026=ORIENTED_EDGE('',*,*,#14897,.T.);
#21027=ORIENTED_EDGE('',*,*,#14893,.F.);
#21028=ORIENTED_EDGE('',*,*,#14858,.T.);
#21029=ORIENTED_EDGE('',*,*,#14898,.T.);
#21030=ORIENTED_EDGE('',*,*,#14899,.T.);
#21031=ORIENTED_EDGE('',*,*,#14854,.T.);
#21032=ORIENTED_EDGE('',*,*,#14875,.F.);
#21033=ORIENTED_EDGE('',*,*,#14900,.T.);
#21034=ORIENTED_EDGE('',*,*,#14901,.T.);
#21035=ORIENTED_EDGE('',*,*,#14855,.T.);
#21036=ORIENTED_EDGE('',*,*,#14899,.F.);
#21037=ORIENTED_EDGE('',*,*,#14902,.T.);
#21038=ORIENTED_EDGE('',*,*,#14903,.T.);
#21039=ORIENTED_EDGE('',*,*,#14856,.T.);
#21040=ORIENTED_EDGE('',*,*,#14901,.F.);
#21041=ORIENTED_EDGE('',*,*,#14904,.T.);
#21042=ORIENTED_EDGE('',*,*,#14857,.T.);
#21043=ORIENTED_EDGE('',*,*,#14903,.F.);
#21044=ORIENTED_EDGE('',*,*,#14905,.T.);
#21045=ORIENTED_EDGE('',*,*,#14898,.F.);
#21046=ORIENTED_EDGE('',*,*,#14688,.F.);
#21047=ORIENTED_EDGE('',*,*,#14790,.T.);
#21048=ORIENTED_EDGE('',*,*,#14890,.F.);
#21049=ORIENTED_EDGE('',*,*,#14906,.F.);
#21050=ORIENTED_EDGE('',*,*,#14692,.F.);
#21051=ORIENTED_EDGE('',*,*,#14906,.T.);
#21052=ORIENTED_EDGE('',*,*,#14889,.F.);
#21053=ORIENTED_EDGE('',*,*,#14907,.F.);
#21054=ORIENTED_EDGE('',*,*,#14735,.F.);
#21055=ORIENTED_EDGE('',*,*,#14907,.T.);
#21056=ORIENTED_EDGE('',*,*,#14885,.F.);
#21057=ORIENTED_EDGE('',*,*,#14908,.F.);
#21058=ORIENTED_EDGE('',*,*,#14732,.F.);
#21059=ORIENTED_EDGE('',*,*,#14908,.T.);
#21060=ORIENTED_EDGE('',*,*,#14896,.F.);
#21061=ORIENTED_EDGE('',*,*,#14909,.F.);
#21062=ORIENTED_EDGE('',*,*,#14730,.F.);
#21063=ORIENTED_EDGE('',*,*,#14909,.T.);
#21064=ORIENTED_EDGE('',*,*,#14895,.F.);
#21065=ORIENTED_EDGE('',*,*,#14910,.F.);
#21066=ORIENTED_EDGE('',*,*,#14728,.F.);
#21067=ORIENTED_EDGE('',*,*,#14910,.T.);
#21068=ORIENTED_EDGE('',*,*,#14891,.F.);
#21069=ORIENTED_EDGE('',*,*,#14911,.F.);
#21070=ORIENTED_EDGE('',*,*,#14723,.F.);
#21071=ORIENTED_EDGE('',*,*,#14911,.T.);
#21072=ORIENTED_EDGE('',*,*,#14897,.F.);
#21073=ORIENTED_EDGE('',*,*,#14912,.F.);
#21074=ORIENTED_EDGE('',*,*,#14720,.F.);
#21075=ORIENTED_EDGE('',*,*,#14912,.T.);
#21076=ORIENTED_EDGE('',*,*,#14905,.F.);
#21077=ORIENTED_EDGE('',*,*,#14913,.F.);
#21078=ORIENTED_EDGE('',*,*,#14718,.F.);
#21079=ORIENTED_EDGE('',*,*,#14913,.T.);
#21080=ORIENTED_EDGE('',*,*,#14904,.F.);
#21081=ORIENTED_EDGE('',*,*,#14914,.F.);
#21082=ORIENTED_EDGE('',*,*,#14715,.F.);
#21083=ORIENTED_EDGE('',*,*,#14914,.T.);
#21084=ORIENTED_EDGE('',*,*,#14902,.F.);
#21085=ORIENTED_EDGE('',*,*,#14915,.F.);
#21086=ORIENTED_EDGE('',*,*,#14684,.T.);
#21087=ORIENTED_EDGE('',*,*,#14712,.F.);
#21088=ORIENTED_EDGE('',*,*,#14915,.T.);
#21089=ORIENTED_EDGE('',*,*,#14900,.F.);
#21090=ORIENTED_EDGE('',*,*,#14916,.F.);
#21091=ORIENTED_EDGE('',*,*,#14709,.F.);
#21092=ORIENTED_EDGE('',*,*,#14916,.T.);
#21093=ORIENTED_EDGE('',*,*,#14874,.F.);
#21094=ORIENTED_EDGE('',*,*,#14917,.F.);
#21095=ORIENTED_EDGE('',*,*,#14706,.F.);
#21096=ORIENTED_EDGE('',*,*,#14917,.T.);
#21097=ORIENTED_EDGE('',*,*,#14876,.F.);
#21098=ORIENTED_EDGE('',*,*,#14918,.T.);
#21099=ORIENTED_EDGE('',*,*,#14919,.T.);
#21100=ORIENTED_EDGE('',*,*,#14920,.F.);
#21101=ORIENTED_EDGE('',*,*,#14841,.F.);
#21102=ORIENTED_EDGE('',*,*,#14921,.F.);
#21103=ORIENTED_EDGE('',*,*,#14922,.T.);
#21104=ORIENTED_EDGE('',*,*,#14918,.F.);
#21105=ORIENTED_EDGE('',*,*,#14833,.F.);
#21106=ORIENTED_EDGE('',*,*,#14809,.F.);
#21107=ORIENTED_EDGE('',*,*,#14923,.T.);
#21108=ORIENTED_EDGE('',*,*,#14817,.F.);
#21109=ORIENTED_EDGE('',*,*,#14818,.F.);
#21110=ORIENTED_EDGE('',*,*,#14923,.F.);
#21111=ORIENTED_EDGE('',*,*,#14808,.F.);
#21112=ORIENTED_EDGE('',*,*,#14812,.F.);
#21113=ORIENTED_EDGE('',*,*,#14814,.F.);
#21114=ORIENTED_EDGE('',*,*,#14924,.F.);
#21115=ORIENTED_EDGE('',*,*,#14919,.F.);
#21116=ORIENTED_EDGE('',*,*,#14922,.F.);
#21117=ORIENTED_EDGE('',*,*,#14925,.F.);
#21118=ORIENTED_EDGE('',*,*,#14926,.F.);
#21119=ORIENTED_EDGE('',*,*,#14703,.F.);
#21120=ORIENTED_EDGE('',*,*,#14920,.T.);
#21121=ORIENTED_EDGE('',*,*,#14924,.T.);
#21122=ORIENTED_EDGE('',*,*,#14927,.F.);
#21123=ORIENTED_EDGE('',*,*,#14700,.F.);
#21124=ORIENTED_EDGE('',*,*,#14927,.T.);
#21125=ORIENTED_EDGE('',*,*,#14926,.T.);
#21126=ORIENTED_EDGE('',*,*,#14928,.F.);
#21127=ORIENTED_EDGE('',*,*,#14698,.F.);
#21128=ORIENTED_EDGE('',*,*,#14928,.T.);
#21129=ORIENTED_EDGE('',*,*,#14925,.T.);
#21130=ORIENTED_EDGE('',*,*,#14921,.T.);
#21131=ORIENTED_EDGE('',*,*,#14848,.F.);
#21132=ORIENTED_EDGE('',*,*,#14929,.F.);
#21133=ORIENTED_EDGE('',*,*,#14787,.F.);
#21134=ORIENTED_EDGE('',*,*,#14929,.T.);
#21135=ORIENTED_EDGE('',*,*,#14849,.F.);
#21136=ORIENTED_EDGE('',*,*,#14825,.F.);
#21137=ORIENTED_EDGE('',*,*,#14930,.T.);
#21138=ORIENTED_EDGE('',*,*,#14931,.T.);
#21139=ORIENTED_EDGE('',*,*,#14932,.T.);
#21140=ORIENTED_EDGE('',*,*,#14931,.F.);
#21141=ORIENTED_EDGE('',*,*,#14932,.F.);
#21142=ORIENTED_EDGE('',*,*,#14933,.F.);
#21143=ORIENTED_EDGE('',*,*,#14934,.T.);
#21144=ORIENTED_EDGE('',*,*,#14935,.T.);
#21145=ORIENTED_EDGE('',*,*,#14934,.F.);
#21146=ORIENTED_EDGE('',*,*,#14933,.T.);
#21147=ORIENTED_EDGE('',*,*,#14936,.F.);
#21148=ORIENTED_EDGE('',*,*,#14937,.F.);
#21149=ORIENTED_EDGE('',*,*,#14938,.F.);
#21150=ORIENTED_EDGE('',*,*,#14939,.F.);
#21151=ORIENTED_EDGE('',*,*,#14939,.T.);
#21152=ORIENTED_EDGE('',*,*,#14940,.F.);
#21153=ORIENTED_EDGE('',*,*,#14941,.F.);
#21154=ORIENTED_EDGE('',*,*,#14942,.F.);
#21155=ORIENTED_EDGE('',*,*,#14943,.F.);
#21156=ORIENTED_EDGE('',*,*,#14944,.F.);
#21157=ORIENTED_EDGE('',*,*,#14945,.F.);
#21158=ORIENTED_EDGE('',*,*,#14946,.F.);
#21159=ORIENTED_EDGE('',*,*,#14947,.F.);
#21160=ORIENTED_EDGE('',*,*,#14948,.F.);
#21161=ORIENTED_EDGE('',*,*,#14945,.T.);
#21162=ORIENTED_EDGE('',*,*,#14949,.F.);
#21163=ORIENTED_EDGE('',*,*,#14950,.F.);
#21164=ORIENTED_EDGE('',*,*,#14951,.F.);
#21165=ORIENTED_EDGE('',*,*,#14947,.T.);
#21166=ORIENTED_EDGE('',*,*,#14952,.F.);
#21167=ORIENTED_EDGE('',*,*,#14953,.F.);
#21168=ORIENTED_EDGE('',*,*,#14954,.F.);
#21169=ORIENTED_EDGE('',*,*,#14950,.T.);
#21170=ORIENTED_EDGE('',*,*,#14955,.F.);
#21171=ORIENTED_EDGE('',*,*,#14956,.F.);
#21172=ORIENTED_EDGE('',*,*,#14957,.F.);
#21173=ORIENTED_EDGE('',*,*,#14953,.T.);
#21174=ORIENTED_EDGE('',*,*,#14958,.F.);
#21175=ORIENTED_EDGE('',*,*,#14959,.F.);
#21176=ORIENTED_EDGE('',*,*,#14960,.F.);
#21177=ORIENTED_EDGE('',*,*,#14956,.T.);
#21178=ORIENTED_EDGE('',*,*,#14961,.F.);
#21179=ORIENTED_EDGE('',*,*,#14962,.F.);
#21180=ORIENTED_EDGE('',*,*,#14963,.F.);
#21181=ORIENTED_EDGE('',*,*,#14959,.T.);
#21182=ORIENTED_EDGE('',*,*,#14964,.F.);
#21183=ORIENTED_EDGE('',*,*,#14965,.F.);
#21184=ORIENTED_EDGE('',*,*,#14966,.F.);
#21185=ORIENTED_EDGE('',*,*,#14962,.T.);
#21186=ORIENTED_EDGE('',*,*,#14967,.F.);
#21187=ORIENTED_EDGE('',*,*,#14968,.F.);
#21188=ORIENTED_EDGE('',*,*,#14969,.F.);
#21189=ORIENTED_EDGE('',*,*,#14970,.F.);
#21190=ORIENTED_EDGE('',*,*,#14965,.T.);
#21191=ORIENTED_EDGE('',*,*,#14971,.F.);
#21192=ORIENTED_EDGE('',*,*,#14972,.F.);
#21193=ORIENTED_EDGE('',*,*,#14973,.F.);
#21194=ORIENTED_EDGE('',*,*,#14969,.T.);
#21195=ORIENTED_EDGE('',*,*,#14974,.F.);
#21196=ORIENTED_EDGE('',*,*,#14972,.T.);
#21197=ORIENTED_EDGE('',*,*,#14975,.F.);
#21198=ORIENTED_EDGE('',*,*,#14976,.F.);
#21199=ORIENTED_EDGE('',*,*,#14977,.F.);
#21200=ORIENTED_EDGE('',*,*,#14978,.F.);
#21201=ORIENTED_EDGE('',*,*,#14976,.T.);
#21202=ORIENTED_EDGE('',*,*,#14979,.F.);
#21203=ORIENTED_EDGE('',*,*,#14980,.F.);
#21204=ORIENTED_EDGE('',*,*,#14981,.F.);
#21205=ORIENTED_EDGE('',*,*,#14982,.F.);
#21206=ORIENTED_EDGE('',*,*,#14977,.T.);
#21207=ORIENTED_EDGE('',*,*,#14941,.T.);
#21208=ORIENTED_EDGE('',*,*,#14983,.F.);
#21209=ORIENTED_EDGE('',*,*,#14981,.T.);
#21210=ORIENTED_EDGE('',*,*,#14984,.F.);
#21211=ORIENTED_EDGE('',*,*,#14985,.F.);
#21212=ORIENTED_EDGE('',*,*,#14937,.T.);
#21213=ORIENTED_EDGE('',*,*,#14986,.F.);
#21214=ORIENTED_EDGE('',*,*,#14987,.F.);
#21215=ORIENTED_EDGE('',*,*,#14988,.F.);
#21216=ORIENTED_EDGE('',*,*,#14989,.F.);
#21217=ORIENTED_EDGE('',*,*,#14987,.T.);
#21218=ORIENTED_EDGE('',*,*,#14990,.F.);
#21219=ORIENTED_EDGE('',*,*,#14991,.F.);
#21220=ORIENTED_EDGE('',*,*,#14992,.F.);
#21221=ORIENTED_EDGE('',*,*,#14993,.F.);
#21222=ORIENTED_EDGE('',*,*,#14988,.T.);
#21223=ORIENTED_EDGE('',*,*,#14994,.F.);
#21224=ORIENTED_EDGE('',*,*,#14992,.T.);
#21225=ORIENTED_EDGE('',*,*,#14995,.F.);
#21226=ORIENTED_EDGE('',*,*,#14996,.F.);
#21227=ORIENTED_EDGE('',*,*,#14997,.F.);
#21228=ORIENTED_EDGE('',*,*,#14996,.T.);
#21229=ORIENTED_EDGE('',*,*,#14998,.F.);
#21230=ORIENTED_EDGE('',*,*,#14999,.F.);
#21231=ORIENTED_EDGE('',*,*,#15000,.F.);
#21232=ORIENTED_EDGE('',*,*,#15001,.F.);
#21233=ORIENTED_EDGE('',*,*,#14999,.T.);
#21234=ORIENTED_EDGE('',*,*,#15002,.F.);
#21235=ORIENTED_EDGE('',*,*,#15003,.F.);
#21236=ORIENTED_EDGE('',*,*,#15004,.F.);
#21237=ORIENTED_EDGE('',*,*,#15000,.T.);
#21238=ORIENTED_EDGE('',*,*,#15005,.F.);
#21239=ORIENTED_EDGE('',*,*,#15006,.F.);
#21240=ORIENTED_EDGE('',*,*,#15007,.F.);
#21241=ORIENTED_EDGE('',*,*,#15003,.T.);
#21242=ORIENTED_EDGE('',*,*,#15008,.F.);
#21243=ORIENTED_EDGE('',*,*,#15009,.F.);
#21244=ORIENTED_EDGE('',*,*,#15010,.F.);
#21245=ORIENTED_EDGE('',*,*,#15006,.T.);
#21246=ORIENTED_EDGE('',*,*,#15011,.F.);
#21247=ORIENTED_EDGE('',*,*,#15012,.F.);
#21248=ORIENTED_EDGE('',*,*,#15013,.F.);
#21249=ORIENTED_EDGE('',*,*,#15009,.T.);
#21250=ORIENTED_EDGE('',*,*,#15014,.F.);
#21251=ORIENTED_EDGE('',*,*,#15015,.F.);
#21252=ORIENTED_EDGE('',*,*,#15016,.F.);
#21253=ORIENTED_EDGE('',*,*,#15012,.T.);
#21254=ORIENTED_EDGE('',*,*,#15017,.F.);
#21255=ORIENTED_EDGE('',*,*,#15018,.F.);
#21256=ORIENTED_EDGE('',*,*,#15019,.F.);
#21257=ORIENTED_EDGE('',*,*,#15015,.T.);
#21258=ORIENTED_EDGE('',*,*,#15020,.F.);
#21259=ORIENTED_EDGE('',*,*,#15021,.F.);
#21260=ORIENTED_EDGE('',*,*,#15022,.F.);
#21261=ORIENTED_EDGE('',*,*,#15018,.T.);
#21262=ORIENTED_EDGE('',*,*,#15023,.F.);
#21263=ORIENTED_EDGE('',*,*,#15024,.F.);
#21264=ORIENTED_EDGE('',*,*,#15025,.F.);
#21265=ORIENTED_EDGE('',*,*,#15026,.F.);
#21266=ORIENTED_EDGE('',*,*,#15027,.F.);
#21267=ORIENTED_EDGE('',*,*,#15024,.T.);
#21268=ORIENTED_EDGE('',*,*,#15028,.F.);
#21269=ORIENTED_EDGE('',*,*,#15029,.F.);
#21270=ORIENTED_EDGE('',*,*,#15030,.F.);
#21271=ORIENTED_EDGE('',*,*,#15029,.T.);
#21272=ORIENTED_EDGE('',*,*,#15031,.F.);
#21273=ORIENTED_EDGE('',*,*,#15032,.F.);
#21274=ORIENTED_EDGE('',*,*,#15033,.F.);
#21275=ORIENTED_EDGE('',*,*,#15032,.T.);
#21276=ORIENTED_EDGE('',*,*,#15021,.T.);
#21277=ORIENTED_EDGE('',*,*,#15034,.F.);
#21278=ORIENTED_EDGE('',*,*,#14943,.T.);
#21279=ORIENTED_EDGE('',*,*,#15026,.T.);
#21280=ORIENTED_EDGE('',*,*,#15035,.F.);
#21281=ORIENTED_EDGE('',*,*,#14986,.T.);
#21282=ORIENTED_EDGE('',*,*,#15036,.T.);
#21283=ORIENTED_EDGE('',*,*,#15037,.T.);
#21284=ORIENTED_EDGE('',*,*,#15038,.F.);
#21285=ORIENTED_EDGE('',*,*,#14990,.T.);
#21286=ORIENTED_EDGE('',*,*,#15038,.T.);
#21287=ORIENTED_EDGE('',*,*,#15039,.T.);
#21288=ORIENTED_EDGE('',*,*,#15040,.F.);
#21289=ORIENTED_EDGE('',*,*,#14991,.T.);
#21290=ORIENTED_EDGE('',*,*,#15040,.T.);
#21291=ORIENTED_EDGE('',*,*,#15041,.T.);
#21292=ORIENTED_EDGE('',*,*,#15042,.F.);
#21293=ORIENTED_EDGE('',*,*,#14995,.T.);
#21294=ORIENTED_EDGE('',*,*,#15042,.T.);
#21295=ORIENTED_EDGE('',*,*,#15043,.T.);
#21296=ORIENTED_EDGE('',*,*,#15044,.F.);
#21297=ORIENTED_EDGE('',*,*,#14998,.T.);
#21298=ORIENTED_EDGE('',*,*,#15044,.T.);
#21299=ORIENTED_EDGE('',*,*,#15045,.T.);
#21300=ORIENTED_EDGE('',*,*,#15046,.F.);
#21301=ORIENTED_EDGE('',*,*,#15002,.T.);
#21302=ORIENTED_EDGE('',*,*,#15046,.T.);
#21303=ORIENTED_EDGE('',*,*,#15047,.T.);
#21304=ORIENTED_EDGE('',*,*,#15048,.F.);
#21305=ORIENTED_EDGE('',*,*,#15005,.T.);
#21306=ORIENTED_EDGE('',*,*,#15048,.T.);
#21307=ORIENTED_EDGE('',*,*,#15049,.T.);
#21308=ORIENTED_EDGE('',*,*,#15050,.F.);
#21309=ORIENTED_EDGE('',*,*,#14935,.F.);
#21310=ORIENTED_EDGE('',*,*,#15008,.T.);
#21311=ORIENTED_EDGE('',*,*,#15050,.T.);
#21312=ORIENTED_EDGE('',*,*,#15051,.T.);
#21313=ORIENTED_EDGE('',*,*,#15052,.F.);
#21314=ORIENTED_EDGE('',*,*,#15011,.T.);
#21315=ORIENTED_EDGE('',*,*,#15052,.T.);
#21316=ORIENTED_EDGE('',*,*,#15053,.T.);
#21317=ORIENTED_EDGE('',*,*,#15054,.F.);
#21318=ORIENTED_EDGE('',*,*,#15014,.T.);
#21319=ORIENTED_EDGE('',*,*,#15054,.T.);
#21320=ORIENTED_EDGE('',*,*,#15055,.T.);
#21321=ORIENTED_EDGE('',*,*,#15056,.F.);
#21322=ORIENTED_EDGE('',*,*,#15057,.F.);
#21323=ORIENTED_EDGE('',*,*,#15058,.F.);
#21324=ORIENTED_EDGE('',*,*,#15017,.T.);
#21325=ORIENTED_EDGE('',*,*,#15058,.T.);
#21326=ORIENTED_EDGE('',*,*,#15059,.F.);
#21327=ORIENTED_EDGE('',*,*,#15060,.F.);
#21328=ORIENTED_EDGE('',*,*,#15020,.T.);
#21329=ORIENTED_EDGE('',*,*,#15060,.T.);
#21330=ORIENTED_EDGE('',*,*,#15061,.F.);
#21331=ORIENTED_EDGE('',*,*,#15062,.F.);
#21332=ORIENTED_EDGE('',*,*,#15023,.T.);
#21333=ORIENTED_EDGE('',*,*,#15062,.T.);
#21334=ORIENTED_EDGE('',*,*,#15063,.F.);
#21335=ORIENTED_EDGE('',*,*,#15064,.F.);
#21336=ORIENTED_EDGE('',*,*,#15065,.T.);
#21337=ORIENTED_EDGE('',*,*,#15066,.F.);
#21338=ORIENTED_EDGE('',*,*,#15034,.T.);
#21339=ORIENTED_EDGE('',*,*,#15066,.T.);
#21340=ORIENTED_EDGE('',*,*,#15067,.T.);
#21341=ORIENTED_EDGE('',*,*,#15068,.F.);
#21342=ORIENTED_EDGE('',*,*,#15033,.T.);
#21343=ORIENTED_EDGE('',*,*,#15068,.T.);
#21344=ORIENTED_EDGE('',*,*,#15069,.T.);
#21345=ORIENTED_EDGE('',*,*,#15070,.F.);
#21346=ORIENTED_EDGE('',*,*,#15030,.T.);
#21347=ORIENTED_EDGE('',*,*,#15070,.T.);
#21348=ORIENTED_EDGE('',*,*,#15071,.T.);
#21349=ORIENTED_EDGE('',*,*,#15072,.F.);
#21350=ORIENTED_EDGE('',*,*,#15025,.T.);
#21351=ORIENTED_EDGE('',*,*,#15072,.T.);
#21352=ORIENTED_EDGE('',*,*,#15073,.T.);
#21353=ORIENTED_EDGE('',*,*,#15074,.F.);
#21354=ORIENTED_EDGE('',*,*,#14946,.T.);
#21355=ORIENTED_EDGE('',*,*,#14948,.T.);
#21356=ORIENTED_EDGE('',*,*,#14951,.T.);
#21357=ORIENTED_EDGE('',*,*,#14954,.T.);
#21358=ORIENTED_EDGE('',*,*,#14957,.T.);
#21359=ORIENTED_EDGE('',*,*,#14960,.T.);
#21360=ORIENTED_EDGE('',*,*,#14963,.T.);
#21361=ORIENTED_EDGE('',*,*,#14966,.T.);
#21362=ORIENTED_EDGE('',*,*,#14970,.T.);
#21363=ORIENTED_EDGE('',*,*,#14973,.T.);
#21364=ORIENTED_EDGE('',*,*,#14974,.T.);
#21365=ORIENTED_EDGE('',*,*,#14978,.T.);
#21366=ORIENTED_EDGE('',*,*,#14982,.T.);
#21367=ORIENTED_EDGE('',*,*,#14983,.T.);
#21368=ORIENTED_EDGE('',*,*,#14940,.T.);
#21369=ORIENTED_EDGE('',*,*,#14938,.T.);
#21370=ORIENTED_EDGE('',*,*,#14985,.T.);
#21371=ORIENTED_EDGE('',*,*,#14989,.T.);
#21372=ORIENTED_EDGE('',*,*,#14993,.T.);
#21373=ORIENTED_EDGE('',*,*,#14994,.T.);
#21374=ORIENTED_EDGE('',*,*,#14997,.T.);
#21375=ORIENTED_EDGE('',*,*,#15001,.T.);
#21376=ORIENTED_EDGE('',*,*,#15004,.T.);
#21377=ORIENTED_EDGE('',*,*,#15007,.T.);
#21378=ORIENTED_EDGE('',*,*,#15010,.T.);
#21379=ORIENTED_EDGE('',*,*,#15013,.T.);
#21380=ORIENTED_EDGE('',*,*,#15016,.T.);
#21381=ORIENTED_EDGE('',*,*,#15019,.T.);
#21382=ORIENTED_EDGE('',*,*,#15022,.T.);
#21383=ORIENTED_EDGE('',*,*,#15031,.T.);
#21384=ORIENTED_EDGE('',*,*,#15028,.T.);
#21385=ORIENTED_EDGE('',*,*,#15027,.T.);
#21386=ORIENTED_EDGE('',*,*,#15065,.F.);
#21387=ORIENTED_EDGE('',*,*,#15075,.F.);
#21388=ORIENTED_EDGE('',*,*,#15076,.F.);
#21389=ORIENTED_EDGE('',*,*,#15077,.F.);
#21390=ORIENTED_EDGE('',*,*,#15078,.F.);
#21391=ORIENTED_EDGE('',*,*,#15075,.T.);
#21392=ORIENTED_EDGE('',*,*,#15079,.F.);
#21393=ORIENTED_EDGE('',*,*,#15080,.F.);
#21394=ORIENTED_EDGE('',*,*,#15081,.F.);
#21395=ORIENTED_EDGE('',*,*,#15082,.F.);
#21396=ORIENTED_EDGE('',*,*,#15069,.F.);
#21397=ORIENTED_EDGE('',*,*,#15083,.F.);
#21398=ORIENTED_EDGE('',*,*,#15084,.F.);
#21399=ORIENTED_EDGE('',*,*,#15085,.F.);
#21400=ORIENTED_EDGE('',*,*,#15071,.F.);
#21401=ORIENTED_EDGE('',*,*,#15082,.T.);
#21402=ORIENTED_EDGE('',*,*,#15086,.F.);
#21403=ORIENTED_EDGE('',*,*,#15085,.T.);
#21404=ORIENTED_EDGE('',*,*,#15087,.F.);
#21405=ORIENTED_EDGE('',*,*,#15088,.F.);
#21406=ORIENTED_EDGE('',*,*,#15073,.F.);
#21407=ORIENTED_EDGE('',*,*,#15083,.T.);
#21408=ORIENTED_EDGE('',*,*,#15067,.F.);
#21409=ORIENTED_EDGE('',*,*,#15077,.T.);
#21410=ORIENTED_EDGE('',*,*,#15089,.F.);
#21411=ORIENTED_EDGE('',*,*,#15090,.F.);
#21412=ORIENTED_EDGE('',*,*,#15091,.F.);
#21413=ORIENTED_EDGE('',*,*,#15092,.F.);
#21414=ORIENTED_EDGE('',*,*,#15093,.F.);
#21415=ORIENTED_EDGE('',*,*,#15094,.F.);
#21416=ORIENTED_EDGE('',*,*,#15090,.T.);
#21417=ORIENTED_EDGE('',*,*,#15095,.F.);
#21418=ORIENTED_EDGE('',*,*,#15096,.F.);
#21419=ORIENTED_EDGE('',*,*,#15096,.T.);
#21420=ORIENTED_EDGE('',*,*,#15097,.F.);
#21421=ORIENTED_EDGE('',*,*,#15088,.T.);
#21422=ORIENTED_EDGE('',*,*,#15081,.T.);
#21423=ORIENTED_EDGE('',*,*,#15098,.F.);
#21424=ORIENTED_EDGE('',*,*,#15053,.F.);
#21425=ORIENTED_EDGE('',*,*,#15099,.T.);
#21426=ORIENTED_EDGE('',*,*,#15100,.F.);
#21427=ORIENTED_EDGE('',*,*,#15078,.T.);
#21428=ORIENTED_EDGE('',*,*,#15100,.T.);
#21429=ORIENTED_EDGE('',*,*,#15101,.T.);
#21430=ORIENTED_EDGE('',*,*,#15102,.T.);
#21431=ORIENTED_EDGE('',*,*,#15103,.T.);
#21432=ORIENTED_EDGE('',*,*,#15104,.T.);
#21433=ORIENTED_EDGE('',*,*,#15105,.T.);
#21434=ORIENTED_EDGE('',*,*,#15106,.T.);
#21435=ORIENTED_EDGE('',*,*,#15107,.T.);
#21436=ORIENTED_EDGE('',*,*,#15108,.T.);
#21437=ORIENTED_EDGE('',*,*,#15109,.T.);
#21438=ORIENTED_EDGE('',*,*,#15110,.T.);
#21439=ORIENTED_EDGE('',*,*,#15111,.T.);
#21440=ORIENTED_EDGE('',*,*,#15112,.T.);
#21441=ORIENTED_EDGE('',*,*,#15113,.T.);
#21442=ORIENTED_EDGE('',*,*,#15114,.T.);
#21443=ORIENTED_EDGE('',*,*,#15115,.T.);
#21444=ORIENTED_EDGE('',*,*,#15116,.T.);
#21445=ORIENTED_EDGE('',*,*,#15117,.T.);
#21446=ORIENTED_EDGE('',*,*,#15118,.T.);
#21447=ORIENTED_EDGE('',*,*,#15119,.T.);
#21448=ORIENTED_EDGE('',*,*,#15120,.T.);
#21449=ORIENTED_EDGE('',*,*,#15091,.T.);
#21450=ORIENTED_EDGE('',*,*,#15094,.T.);
#21451=ORIENTED_EDGE('',*,*,#15087,.T.);
#21452=ORIENTED_EDGE('',*,*,#15086,.T.);
#21453=ORIENTED_EDGE('',*,*,#15084,.T.);
#21454=ORIENTED_EDGE('',*,*,#15076,.T.);
#21455=ORIENTED_EDGE('',*,*,#15092,.T.);
#21456=ORIENTED_EDGE('',*,*,#15120,.F.);
#21457=ORIENTED_EDGE('',*,*,#15121,.F.);
#21458=ORIENTED_EDGE('',*,*,#15122,.F.);
#21459=ORIENTED_EDGE('',*,*,#15123,.T.);
#21460=ORIENTED_EDGE('',*,*,#15093,.T.);
#21461=ORIENTED_EDGE('',*,*,#15123,.F.);
#21462=ORIENTED_EDGE('',*,*,#15124,.F.);
#21463=ORIENTED_EDGE('',*,*,#15045,.F.);
#21464=ORIENTED_EDGE('',*,*,#15125,.F.);
#21465=ORIENTED_EDGE('',*,*,#15104,.F.);
#21466=ORIENTED_EDGE('',*,*,#15126,.F.);
#21467=ORIENTED_EDGE('',*,*,#15127,.F.);
#21468=ORIENTED_EDGE('',*,*,#15047,.F.);
#21469=ORIENTED_EDGE('',*,*,#15126,.T.);
#21470=ORIENTED_EDGE('',*,*,#15103,.F.);
#21471=ORIENTED_EDGE('',*,*,#15128,.F.);
#21472=ORIENTED_EDGE('',*,*,#15049,.F.);
#21473=ORIENTED_EDGE('',*,*,#15127,.T.);
#21474=ORIENTED_EDGE('',*,*,#15102,.F.);
#21475=ORIENTED_EDGE('',*,*,#15099,.F.);
#21476=ORIENTED_EDGE('',*,*,#15051,.F.);
#21477=ORIENTED_EDGE('',*,*,#15128,.T.);
#21478=ORIENTED_EDGE('',*,*,#15101,.F.);
#21479=ORIENTED_EDGE('',*,*,#15080,.T.);
#21480=ORIENTED_EDGE('',*,*,#15055,.F.);
#21481=ORIENTED_EDGE('',*,*,#15098,.T.);
#21482=ORIENTED_EDGE('',*,*,#15043,.F.);
#21483=ORIENTED_EDGE('',*,*,#15129,.F.);
#21484=ORIENTED_EDGE('',*,*,#15105,.F.);
#21485=ORIENTED_EDGE('',*,*,#15125,.T.);
#21486=ORIENTED_EDGE('',*,*,#15037,.F.);
#21487=ORIENTED_EDGE('',*,*,#15130,.F.);
#21488=ORIENTED_EDGE('',*,*,#15108,.F.);
#21489=ORIENTED_EDGE('',*,*,#15131,.F.);
#21490=ORIENTED_EDGE('',*,*,#15132,.F.);
#21491=ORIENTED_EDGE('',*,*,#15039,.F.);
#21492=ORIENTED_EDGE('',*,*,#15131,.T.);
#21493=ORIENTED_EDGE('',*,*,#15107,.F.);
#21494=ORIENTED_EDGE('',*,*,#15106,.F.);
#21495=ORIENTED_EDGE('',*,*,#15129,.T.);
#21496=ORIENTED_EDGE('',*,*,#15041,.F.);
#21497=ORIENTED_EDGE('',*,*,#15132,.T.);
#21498=ORIENTED_EDGE('',*,*,#15133,.F.);
#21499=ORIENTED_EDGE('',*,*,#15134,.F.);
#21500=ORIENTED_EDGE('',*,*,#15111,.F.);
#21501=ORIENTED_EDGE('',*,*,#15135,.F.);
#21502=ORIENTED_EDGE('',*,*,#15136,.F.);
#21503=ORIENTED_EDGE('',*,*,#15137,.F.);
#21504=ORIENTED_EDGE('',*,*,#15135,.T.);
#21505=ORIENTED_EDGE('',*,*,#15110,.F.);
#21506=ORIENTED_EDGE('',*,*,#15109,.F.);
#21507=ORIENTED_EDGE('',*,*,#15130,.T.);
#21508=ORIENTED_EDGE('',*,*,#15138,.F.);
#21509=ORIENTED_EDGE('',*,*,#15136,.T.);
#21510=ORIENTED_EDGE('',*,*,#15139,.F.);
#21511=ORIENTED_EDGE('',*,*,#15140,.F.);
#21512=ORIENTED_EDGE('',*,*,#15114,.F.);
#21513=ORIENTED_EDGE('',*,*,#15141,.F.);
#21514=ORIENTED_EDGE('',*,*,#15142,.F.);
#21515=ORIENTED_EDGE('',*,*,#15143,.F.);
#21516=ORIENTED_EDGE('',*,*,#15141,.T.);
#21517=ORIENTED_EDGE('',*,*,#15113,.F.);
#21518=ORIENTED_EDGE('',*,*,#15112,.F.);
#21519=ORIENTED_EDGE('',*,*,#15134,.T.);
#21520=ORIENTED_EDGE('',*,*,#15144,.F.);
#21521=ORIENTED_EDGE('',*,*,#15142,.T.);
#21522=ORIENTED_EDGE('',*,*,#15145,.F.);
#21523=ORIENTED_EDGE('',*,*,#15146,.F.);
#21524=ORIENTED_EDGE('',*,*,#15115,.F.);
#21525=ORIENTED_EDGE('',*,*,#15140,.T.);
#21526=ORIENTED_EDGE('',*,*,#15147,.F.);
#21527=ORIENTED_EDGE('',*,*,#15148,.F.);
#21528=ORIENTED_EDGE('',*,*,#15121,.T.);
#21529=ORIENTED_EDGE('',*,*,#15119,.F.);
#21530=ORIENTED_EDGE('',*,*,#15149,.F.);
#21531=ORIENTED_EDGE('',*,*,#15150,.F.);
#21532=ORIENTED_EDGE('',*,*,#15147,.T.);
#21533=ORIENTED_EDGE('',*,*,#15118,.F.);
#21534=ORIENTED_EDGE('',*,*,#15151,.F.);
#21535=ORIENTED_EDGE('',*,*,#15152,.F.);
#21536=ORIENTED_EDGE('',*,*,#15149,.T.);
#21537=ORIENTED_EDGE('',*,*,#15117,.F.);
#21538=ORIENTED_EDGE('',*,*,#15116,.F.);
#21539=ORIENTED_EDGE('',*,*,#15146,.T.);
#21540=ORIENTED_EDGE('',*,*,#15153,.F.);
#21541=ORIENTED_EDGE('',*,*,#15151,.T.);
#21542=ORIENTED_EDGE('',*,*,#14936,.T.);
#21543=ORIENTED_EDGE('',*,*,#15154,.T.);
#21544=ORIENTED_EDGE('',*,*,#15138,.T.);
#21545=ORIENTED_EDGE('',*,*,#15036,.F.);
#21546=ORIENTED_EDGE('',*,*,#14942,.T.);
#21547=ORIENTED_EDGE('',*,*,#15155,.T.);
#21548=ORIENTED_EDGE('',*,*,#15137,.T.);
#21549=ORIENTED_EDGE('',*,*,#15154,.F.);
#21550=ORIENTED_EDGE('',*,*,#14984,.T.);
#21551=ORIENTED_EDGE('',*,*,#15156,.T.);
#21552=ORIENTED_EDGE('',*,*,#15133,.T.);
#21553=ORIENTED_EDGE('',*,*,#15155,.F.);
#21554=ORIENTED_EDGE('',*,*,#14980,.T.);
#21555=ORIENTED_EDGE('',*,*,#15157,.T.);
#21556=ORIENTED_EDGE('',*,*,#15144,.T.);
#21557=ORIENTED_EDGE('',*,*,#15156,.F.);
#21558=ORIENTED_EDGE('',*,*,#14979,.T.);
#21559=ORIENTED_EDGE('',*,*,#15158,.T.);
#21560=ORIENTED_EDGE('',*,*,#15143,.T.);
#21561=ORIENTED_EDGE('',*,*,#15157,.F.);
#21562=ORIENTED_EDGE('',*,*,#14975,.T.);
#21563=ORIENTED_EDGE('',*,*,#15159,.T.);
#21564=ORIENTED_EDGE('',*,*,#15139,.T.);
#21565=ORIENTED_EDGE('',*,*,#15158,.F.);
#21566=ORIENTED_EDGE('',*,*,#14971,.T.);
#21567=ORIENTED_EDGE('',*,*,#15160,.T.);
#21568=ORIENTED_EDGE('',*,*,#15145,.T.);
#21569=ORIENTED_EDGE('',*,*,#15159,.F.);
#21570=ORIENTED_EDGE('',*,*,#14968,.T.);
#21571=ORIENTED_EDGE('',*,*,#15161,.T.);
#21572=ORIENTED_EDGE('',*,*,#15153,.T.);
#21573=ORIENTED_EDGE('',*,*,#15160,.F.);
#21574=ORIENTED_EDGE('',*,*,#14967,.T.);
#21575=ORIENTED_EDGE('',*,*,#15162,.T.);
#21576=ORIENTED_EDGE('',*,*,#15152,.T.);
#21577=ORIENTED_EDGE('',*,*,#15161,.F.);
#21578=ORIENTED_EDGE('',*,*,#14964,.T.);
#21579=ORIENTED_EDGE('',*,*,#15163,.T.);
#21580=ORIENTED_EDGE('',*,*,#15150,.T.);
#21581=ORIENTED_EDGE('',*,*,#15162,.F.);
#21582=ORIENTED_EDGE('',*,*,#14930,.F.);
#21583=ORIENTED_EDGE('',*,*,#14961,.T.);
#21584=ORIENTED_EDGE('',*,*,#15164,.T.);
#21585=ORIENTED_EDGE('',*,*,#15148,.T.);
#21586=ORIENTED_EDGE('',*,*,#15163,.F.);
#21587=ORIENTED_EDGE('',*,*,#14958,.T.);
#21588=ORIENTED_EDGE('',*,*,#15165,.T.);
#21589=ORIENTED_EDGE('',*,*,#15122,.T.);
#21590=ORIENTED_EDGE('',*,*,#15164,.F.);
#21591=ORIENTED_EDGE('',*,*,#14955,.T.);
#21592=ORIENTED_EDGE('',*,*,#15166,.T.);
#21593=ORIENTED_EDGE('',*,*,#15167,.F.);
#21594=ORIENTED_EDGE('',*,*,#15168,.F.);
#21595=ORIENTED_EDGE('',*,*,#15124,.T.);
#21596=ORIENTED_EDGE('',*,*,#15165,.F.);
#21597=ORIENTED_EDGE('',*,*,#15089,.T.);
#21598=ORIENTED_EDGE('',*,*,#15168,.T.);
#21599=ORIENTED_EDGE('',*,*,#15169,.F.);
#21600=ORIENTED_EDGE('',*,*,#15170,.T.);
#21601=ORIENTED_EDGE('',*,*,#15079,.T.);
#21602=ORIENTED_EDGE('',*,*,#15064,.T.);
#21603=ORIENTED_EDGE('',*,*,#15171,.F.);
#21604=ORIENTED_EDGE('',*,*,#15056,.T.);
#21605=ORIENTED_EDGE('',*,*,#15063,.T.);
#21606=ORIENTED_EDGE('',*,*,#15061,.T.);
#21607=ORIENTED_EDGE('',*,*,#15059,.T.);
#21608=ORIENTED_EDGE('',*,*,#15057,.T.);
#21609=ORIENTED_EDGE('',*,*,#15171,.T.);
#21610=ORIENTED_EDGE('',*,*,#15172,.T.);
#21611=ORIENTED_EDGE('',*,*,#15173,.T.);
#21612=ORIENTED_EDGE('',*,*,#15174,.T.);
#21613=ORIENTED_EDGE('',*,*,#15169,.T.);
#21614=ORIENTED_EDGE('',*,*,#15167,.T.);
#21615=ORIENTED_EDGE('',*,*,#14952,.T.);
#21616=ORIENTED_EDGE('',*,*,#15175,.T.);
#21617=ORIENTED_EDGE('',*,*,#15172,.F.);
#21618=ORIENTED_EDGE('',*,*,#15166,.F.);
#21619=ORIENTED_EDGE('',*,*,#14949,.T.);
#21620=ORIENTED_EDGE('',*,*,#15176,.T.);
#21621=ORIENTED_EDGE('',*,*,#15173,.F.);
#21622=ORIENTED_EDGE('',*,*,#15175,.F.);
#21623=ORIENTED_EDGE('',*,*,#14944,.T.);
#21624=ORIENTED_EDGE('',*,*,#15177,.T.);
#21625=ORIENTED_EDGE('',*,*,#15095,.T.);
#21626=ORIENTED_EDGE('',*,*,#15170,.F.);
#21627=ORIENTED_EDGE('',*,*,#15174,.F.);
#21628=ORIENTED_EDGE('',*,*,#15176,.F.);
#21629=ORIENTED_EDGE('',*,*,#15035,.T.);
#21630=ORIENTED_EDGE('',*,*,#15074,.T.);
#21631=ORIENTED_EDGE('',*,*,#15097,.T.);
#21632=ORIENTED_EDGE('',*,*,#15177,.F.);
#21633=ORIENTED_EDGE('',*,*,#15178,.F.);
#21634=ORIENTED_EDGE('',*,*,#15179,.F.);
#21635=ORIENTED_EDGE('',*,*,#15180,.T.);
#21636=ORIENTED_EDGE('',*,*,#15181,.T.);
#21637=ORIENTED_EDGE('',*,*,#15180,.F.);
#21638=ORIENTED_EDGE('',*,*,#15181,.F.);
#21639=ORIENTED_EDGE('',*,*,#15182,.F.);
#21640=ORIENTED_EDGE('',*,*,#15183,.F.);
#21641=ORIENTED_EDGE('',*,*,#15184,.T.);
#21642=ORIENTED_EDGE('',*,*,#15185,.T.);
#21643=ORIENTED_EDGE('',*,*,#15184,.F.);
#21644=ORIENTED_EDGE('',*,*,#15185,.F.);
#21645=ORIENTED_EDGE('',*,*,#15178,.T.);
#21646=ORIENTED_EDGE('',*,*,#15186,.T.);
#21647=ORIENTED_EDGE('',*,*,#15182,.T.);
#21648=ORIENTED_EDGE('',*,*,#15187,.T.);
#21649=ORIENTED_EDGE('',*,*,#15188,.F.);
#21650=ORIENTED_EDGE('',*,*,#15189,.F.);
#21651=ORIENTED_EDGE('',*,*,#15190,.T.);
#21652=ORIENTED_EDGE('',*,*,#15191,.T.);
#21653=ORIENTED_EDGE('',*,*,#15192,.F.);
#21654=ORIENTED_EDGE('',*,*,#15193,.F.);
#21655=ORIENTED_EDGE('',*,*,#15194,.F.);
#21656=ORIENTED_EDGE('',*,*,#15195,.T.);
#21657=ORIENTED_EDGE('',*,*,#15196,.F.);
#21658=ORIENTED_EDGE('',*,*,#15197,.F.);
#21659=ORIENTED_EDGE('',*,*,#15198,.F.);
#21660=ORIENTED_EDGE('',*,*,#15199,.F.);
#21661=ORIENTED_EDGE('',*,*,#15200,.F.);
#21662=ORIENTED_EDGE('',*,*,#15201,.F.);
#21663=ORIENTED_EDGE('',*,*,#15202,.F.);
#21664=ORIENTED_EDGE('',*,*,#15203,.F.);
#21665=ORIENTED_EDGE('',*,*,#15204,.F.);
#21666=ORIENTED_EDGE('',*,*,#15205,.F.);
#21667=ORIENTED_EDGE('',*,*,#15206,.F.);
#21668=ORIENTED_EDGE('',*,*,#15207,.F.);
#21669=ORIENTED_EDGE('',*,*,#15208,.F.);
#21670=ORIENTED_EDGE('',*,*,#15209,.F.);
#21671=ORIENTED_EDGE('',*,*,#15210,.F.);
#21672=ORIENTED_EDGE('',*,*,#15211,.F.);
#21673=ORIENTED_EDGE('',*,*,#15212,.F.);
#21674=ORIENTED_EDGE('',*,*,#15213,.F.);
#21675=ORIENTED_EDGE('',*,*,#15214,.F.);
#21676=ORIENTED_EDGE('',*,*,#15215,.F.);
#21677=ORIENTED_EDGE('',*,*,#15216,.T.);
#21678=ORIENTED_EDGE('',*,*,#15217,.F.);
#21679=ORIENTED_EDGE('',*,*,#15218,.F.);
#21680=ORIENTED_EDGE('',*,*,#15219,.F.);
#21681=ORIENTED_EDGE('',*,*,#15220,.F.);
#21682=ORIENTED_EDGE('',*,*,#15221,.F.);
#21683=ORIENTED_EDGE('',*,*,#15222,.F.);
#21684=ORIENTED_EDGE('',*,*,#15223,.F.);
#21685=ORIENTED_EDGE('',*,*,#15224,.F.);
#21686=ORIENTED_EDGE('',*,*,#15225,.F.);
#21687=ORIENTED_EDGE('',*,*,#15226,.F.);
#21688=ORIENTED_EDGE('',*,*,#15227,.F.);
#21689=ORIENTED_EDGE('',*,*,#15228,.F.);
#21690=ORIENTED_EDGE('',*,*,#15229,.F.);
#21691=ORIENTED_EDGE('',*,*,#15230,.F.);
#21692=ORIENTED_EDGE('',*,*,#15231,.F.);
#21693=ORIENTED_EDGE('',*,*,#15232,.F.);
#21694=ORIENTED_EDGE('',*,*,#15233,.F.);
#21695=ORIENTED_EDGE('',*,*,#15234,.F.);
#21696=ORIENTED_EDGE('',*,*,#15235,.F.);
#21697=ORIENTED_EDGE('',*,*,#15236,.F.);
#21698=ORIENTED_EDGE('',*,*,#15237,.T.);
#21699=ORIENTED_EDGE('',*,*,#15238,.F.);
#21700=ORIENTED_EDGE('',*,*,#15193,.T.);
#21701=ORIENTED_EDGE('',*,*,#15239,.F.);
#21702=ORIENTED_EDGE('',*,*,#15237,.F.);
#21703=ORIENTED_EDGE('',*,*,#15240,.F.);
#21704=ORIENTED_EDGE('',*,*,#15241,.F.);
#21705=ORIENTED_EDGE('',*,*,#15242,.F.);
#21706=ORIENTED_EDGE('',*,*,#15243,.F.);
#21707=ORIENTED_EDGE('',*,*,#15244,.F.);
#21708=ORIENTED_EDGE('',*,*,#15245,.F.);
#21709=ORIENTED_EDGE('',*,*,#15216,.F.);
#21710=ORIENTED_EDGE('',*,*,#15246,.F.);
#21711=ORIENTED_EDGE('',*,*,#15247,.F.);
#21712=ORIENTED_EDGE('',*,*,#15248,.F.);
#21713=ORIENTED_EDGE('',*,*,#15249,.F.);
#21714=ORIENTED_EDGE('',*,*,#15250,.F.);
#21715=ORIENTED_EDGE('',*,*,#15251,.F.);
#21716=ORIENTED_EDGE('',*,*,#15195,.F.);
#21717=ORIENTED_EDGE('',*,*,#15252,.F.);
#21718=ORIENTED_EDGE('',*,*,#15253,.F.);
#21719=ORIENTED_EDGE('',*,*,#15254,.F.);
#21720=ORIENTED_EDGE('',*,*,#15255,.T.);
#21721=ORIENTED_EDGE('',*,*,#15256,.F.);
#21722=ORIENTED_EDGE('',*,*,#15257,.F.);
#21723=ORIENTED_EDGE('',*,*,#15258,.F.);
#21724=ORIENTED_EDGE('',*,*,#15259,.F.);
#21725=ORIENTED_EDGE('',*,*,#15260,.F.);
#21726=ORIENTED_EDGE('',*,*,#15261,.F.);
#21727=ORIENTED_EDGE('',*,*,#15262,.F.);
#21728=ORIENTED_EDGE('',*,*,#15263,.F.);
#21729=ORIENTED_EDGE('',*,*,#15264,.F.);
#21730=ORIENTED_EDGE('',*,*,#15265,.F.);
#21731=ORIENTED_EDGE('',*,*,#15266,.F.);
#21732=ORIENTED_EDGE('',*,*,#15267,.F.);
#21733=ORIENTED_EDGE('',*,*,#15268,.F.);
#21734=ORIENTED_EDGE('',*,*,#15269,.F.);
#21735=ORIENTED_EDGE('',*,*,#15270,.F.);
#21736=ORIENTED_EDGE('',*,*,#15271,.F.);
#21737=ORIENTED_EDGE('',*,*,#15272,.F.);
#21738=ORIENTED_EDGE('',*,*,#15273,.F.);
#21739=ORIENTED_EDGE('',*,*,#15274,.F.);
#21740=ORIENTED_EDGE('',*,*,#15275,.F.);
#21741=ORIENTED_EDGE('',*,*,#15276,.T.);
#21742=ORIENTED_EDGE('',*,*,#15277,.F.);
#21743=ORIENTED_EDGE('',*,*,#15278,.F.);
#21744=ORIENTED_EDGE('',*,*,#15279,.F.);
#21745=ORIENTED_EDGE('',*,*,#15280,.F.);
#21746=ORIENTED_EDGE('',*,*,#15281,.F.);
#21747=ORIENTED_EDGE('',*,*,#15282,.F.);
#21748=ORIENTED_EDGE('',*,*,#15283,.F.);
#21749=ORIENTED_EDGE('',*,*,#15284,.F.);
#21750=ORIENTED_EDGE('',*,*,#15285,.F.);
#21751=ORIENTED_EDGE('',*,*,#15286,.F.);
#21752=ORIENTED_EDGE('',*,*,#15287,.F.);
#21753=ORIENTED_EDGE('',*,*,#15288,.F.);
#21754=ORIENTED_EDGE('',*,*,#15289,.F.);
#21755=ORIENTED_EDGE('',*,*,#15290,.F.);
#21756=ORIENTED_EDGE('',*,*,#15291,.F.);
#21757=ORIENTED_EDGE('',*,*,#15292,.F.);
#21758=ORIENTED_EDGE('',*,*,#15293,.F.);
#21759=ORIENTED_EDGE('',*,*,#15294,.F.);
#21760=ORIENTED_EDGE('',*,*,#15295,.F.);
#21761=ORIENTED_EDGE('',*,*,#15296,.F.);
#21762=ORIENTED_EDGE('',*,*,#15297,.T.);
#21763=ORIENTED_EDGE('',*,*,#15298,.F.);
#21764=ORIENTED_EDGE('',*,*,#15253,.T.);
#21765=ORIENTED_EDGE('',*,*,#15299,.F.);
#21766=ORIENTED_EDGE('',*,*,#15297,.F.);
#21767=ORIENTED_EDGE('',*,*,#15300,.F.);
#21768=ORIENTED_EDGE('',*,*,#15301,.F.);
#21769=ORIENTED_EDGE('',*,*,#15302,.F.);
#21770=ORIENTED_EDGE('',*,*,#15303,.F.);
#21771=ORIENTED_EDGE('',*,*,#15304,.F.);
#21772=ORIENTED_EDGE('',*,*,#15305,.F.);
#21773=ORIENTED_EDGE('',*,*,#15276,.F.);
#21774=ORIENTED_EDGE('',*,*,#15306,.F.);
#21775=ORIENTED_EDGE('',*,*,#15307,.F.);
#21776=ORIENTED_EDGE('',*,*,#15308,.F.);
#21777=ORIENTED_EDGE('',*,*,#15309,.F.);
#21778=ORIENTED_EDGE('',*,*,#15310,.F.);
#21779=ORIENTED_EDGE('',*,*,#15311,.F.);
#21780=ORIENTED_EDGE('',*,*,#15255,.F.);
#21781=ORIENTED_EDGE('',*,*,#15312,.F.);
#21782=ORIENTED_EDGE('',*,*,#15313,.F.);
#21783=ORIENTED_EDGE('',*,*,#15314,.F.);
#21784=ORIENTED_EDGE('',*,*,#15315,.T.);
#21785=ORIENTED_EDGE('',*,*,#15316,.F.);
#21786=ORIENTED_EDGE('',*,*,#15317,.F.);
#21787=ORIENTED_EDGE('',*,*,#15318,.F.);
#21788=ORIENTED_EDGE('',*,*,#15319,.F.);
#21789=ORIENTED_EDGE('',*,*,#15320,.F.);
#21790=ORIENTED_EDGE('',*,*,#15321,.F.);
#21791=ORIENTED_EDGE('',*,*,#15322,.F.);
#21792=ORIENTED_EDGE('',*,*,#15323,.F.);
#21793=ORIENTED_EDGE('',*,*,#15324,.F.);
#21794=ORIENTED_EDGE('',*,*,#15325,.F.);
#21795=ORIENTED_EDGE('',*,*,#15326,.F.);
#21796=ORIENTED_EDGE('',*,*,#15327,.F.);
#21797=ORIENTED_EDGE('',*,*,#15328,.F.);
#21798=ORIENTED_EDGE('',*,*,#15329,.F.);
#21799=ORIENTED_EDGE('',*,*,#15330,.F.);
#21800=ORIENTED_EDGE('',*,*,#15331,.F.);
#21801=ORIENTED_EDGE('',*,*,#15332,.F.);
#21802=ORIENTED_EDGE('',*,*,#15333,.F.);
#21803=ORIENTED_EDGE('',*,*,#15334,.F.);
#21804=ORIENTED_EDGE('',*,*,#15335,.F.);
#21805=ORIENTED_EDGE('',*,*,#15336,.T.);
#21806=ORIENTED_EDGE('',*,*,#15337,.F.);
#21807=ORIENTED_EDGE('',*,*,#15338,.F.);
#21808=ORIENTED_EDGE('',*,*,#15339,.F.);
#21809=ORIENTED_EDGE('',*,*,#15340,.F.);
#21810=ORIENTED_EDGE('',*,*,#15341,.F.);
#21811=ORIENTED_EDGE('',*,*,#15342,.F.);
#21812=ORIENTED_EDGE('',*,*,#15343,.F.);
#21813=ORIENTED_EDGE('',*,*,#15344,.F.);
#21814=ORIENTED_EDGE('',*,*,#15345,.F.);
#21815=ORIENTED_EDGE('',*,*,#15346,.F.);
#21816=ORIENTED_EDGE('',*,*,#15347,.F.);
#21817=ORIENTED_EDGE('',*,*,#15348,.F.);
#21818=ORIENTED_EDGE('',*,*,#15349,.F.);
#21819=ORIENTED_EDGE('',*,*,#15350,.F.);
#21820=ORIENTED_EDGE('',*,*,#15351,.F.);
#21821=ORIENTED_EDGE('',*,*,#15352,.F.);
#21822=ORIENTED_EDGE('',*,*,#15353,.F.);
#21823=ORIENTED_EDGE('',*,*,#15354,.F.);
#21824=ORIENTED_EDGE('',*,*,#15355,.F.);
#21825=ORIENTED_EDGE('',*,*,#15356,.F.);
#21826=ORIENTED_EDGE('',*,*,#15357,.T.);
#21827=ORIENTED_EDGE('',*,*,#15358,.F.);
#21828=ORIENTED_EDGE('',*,*,#15313,.T.);
#21829=ORIENTED_EDGE('',*,*,#15359,.F.);
#21830=ORIENTED_EDGE('',*,*,#15357,.F.);
#21831=ORIENTED_EDGE('',*,*,#15360,.F.);
#21832=ORIENTED_EDGE('',*,*,#15361,.F.);
#21833=ORIENTED_EDGE('',*,*,#15362,.F.);
#21834=ORIENTED_EDGE('',*,*,#15363,.F.);
#21835=ORIENTED_EDGE('',*,*,#15364,.F.);
#21836=ORIENTED_EDGE('',*,*,#15365,.F.);
#21837=ORIENTED_EDGE('',*,*,#15336,.F.);
#21838=ORIENTED_EDGE('',*,*,#15366,.F.);
#21839=ORIENTED_EDGE('',*,*,#15367,.F.);
#21840=ORIENTED_EDGE('',*,*,#15368,.F.);
#21841=ORIENTED_EDGE('',*,*,#15369,.F.);
#21842=ORIENTED_EDGE('',*,*,#15370,.F.);
#21843=ORIENTED_EDGE('',*,*,#15371,.F.);
#21844=ORIENTED_EDGE('',*,*,#15315,.F.);
#21845=ORIENTED_EDGE('',*,*,#15200,.T.);
#21846=ORIENTED_EDGE('',*,*,#15372,.F.);
#21847=ORIENTED_EDGE('',*,*,#15373,.F.);
#21848=ORIENTED_EDGE('',*,*,#15374,.T.);
#21849=ORIENTED_EDGE('',*,*,#15375,.T.);
#21850=ORIENTED_EDGE('',*,*,#15376,.F.);
#21851=ORIENTED_EDGE('',*,*,#15320,.T.);
#21852=ORIENTED_EDGE('',*,*,#15377,.F.);
#21853=ORIENTED_EDGE('',*,*,#15260,.T.);
#21854=ORIENTED_EDGE('',*,*,#15378,.F.);
#21855=ORIENTED_EDGE('',*,*,#15199,.T.);
#21856=ORIENTED_EDGE('',*,*,#15379,.F.);
#21857=ORIENTED_EDGE('',*,*,#15380,.F.);
#21858=ORIENTED_EDGE('',*,*,#15372,.T.);
#21859=ORIENTED_EDGE('',*,*,#15321,.T.);
#21860=ORIENTED_EDGE('',*,*,#15376,.T.);
#21861=ORIENTED_EDGE('',*,*,#15381,.T.);
#21862=ORIENTED_EDGE('',*,*,#15382,.F.);
#21863=ORIENTED_EDGE('',*,*,#15261,.T.);
#21864=ORIENTED_EDGE('',*,*,#15377,.T.);
#21865=ORIENTED_EDGE('',*,*,#15319,.T.);
#21866=ORIENTED_EDGE('',*,*,#15383,.F.);
#21867=ORIENTED_EDGE('',*,*,#15198,.T.);
#21868=ORIENTED_EDGE('',*,*,#15384,.F.);
#21869=ORIENTED_EDGE('',*,*,#15385,.T.);
#21870=ORIENTED_EDGE('',*,*,#15379,.T.);
#21871=ORIENTED_EDGE('',*,*,#15322,.T.);
#21872=ORIENTED_EDGE('',*,*,#15382,.T.);
#21873=ORIENTED_EDGE('',*,*,#15386,.T.);
#21874=ORIENTED_EDGE('',*,*,#15387,.F.);
#21875=ORIENTED_EDGE('',*,*,#15262,.T.);
#21876=ORIENTED_EDGE('',*,*,#15383,.T.);
#21877=ORIENTED_EDGE('',*,*,#15318,.T.);
#21878=ORIENTED_EDGE('',*,*,#15388,.F.);
#21879=ORIENTED_EDGE('',*,*,#15197,.T.);
#21880=ORIENTED_EDGE('',*,*,#15389,.F.);
#21881=ORIENTED_EDGE('',*,*,#15390,.F.);
#21882=ORIENTED_EDGE('',*,*,#15384,.T.);
#21883=ORIENTED_EDGE('',*,*,#15323,.T.);
#21884=ORIENTED_EDGE('',*,*,#15387,.T.);
#21885=ORIENTED_EDGE('',*,*,#15391,.T.);
#21886=ORIENTED_EDGE('',*,*,#15392,.F.);
#21887=ORIENTED_EDGE('',*,*,#15263,.T.);
#21888=ORIENTED_EDGE('',*,*,#15388,.T.);
#21889=ORIENTED_EDGE('',*,*,#15317,.T.);
#21890=ORIENTED_EDGE('',*,*,#15393,.F.);
#21891=ORIENTED_EDGE('',*,*,#15196,.T.);
#21892=ORIENTED_EDGE('',*,*,#15251,.T.);
#21893=ORIENTED_EDGE('',*,*,#15394,.F.);
#21894=ORIENTED_EDGE('',*,*,#15395,.T.);
#21895=ORIENTED_EDGE('',*,*,#15389,.T.);
#21896=ORIENTED_EDGE('',*,*,#15324,.T.);
#21897=ORIENTED_EDGE('',*,*,#15392,.T.);
#21898=ORIENTED_EDGE('',*,*,#15396,.T.);
#21899=ORIENTED_EDGE('',*,*,#15397,.F.);
#21900=ORIENTED_EDGE('',*,*,#15264,.T.);
#21901=ORIENTED_EDGE('',*,*,#15393,.T.);
#21902=ORIENTED_EDGE('',*,*,#15316,.T.);
#21903=ORIENTED_EDGE('',*,*,#15371,.T.);
#21904=ORIENTED_EDGE('',*,*,#15398,.F.);
#21905=ORIENTED_EDGE('',*,*,#15250,.T.);
#21906=ORIENTED_EDGE('',*,*,#15399,.F.);
#21907=ORIENTED_EDGE('',*,*,#15400,.F.);
#21908=ORIENTED_EDGE('',*,*,#15394,.T.);
#21909=ORIENTED_EDGE('',*,*,#15325,.T.);
#21910=ORIENTED_EDGE('',*,*,#15397,.T.);
#21911=ORIENTED_EDGE('',*,*,#15401,.T.);
#21912=ORIENTED_EDGE('',*,*,#15402,.F.);
#21913=ORIENTED_EDGE('',*,*,#15265,.T.);
#21914=ORIENTED_EDGE('',*,*,#15398,.T.);
#21915=ORIENTED_EDGE('',*,*,#15370,.T.);
#21916=ORIENTED_EDGE('',*,*,#15403,.F.);
#21917=ORIENTED_EDGE('',*,*,#15249,.T.);
#21918=ORIENTED_EDGE('',*,*,#15404,.F.);
#21919=ORIENTED_EDGE('',*,*,#15405,.T.);
#21920=ORIENTED_EDGE('',*,*,#15399,.T.);
#21921=ORIENTED_EDGE('',*,*,#15326,.T.);
#21922=ORIENTED_EDGE('',*,*,#15402,.T.);
#21923=ORIENTED_EDGE('',*,*,#15406,.T.);
#21924=ORIENTED_EDGE('',*,*,#15407,.F.);
#21925=ORIENTED_EDGE('',*,*,#15266,.T.);
#21926=ORIENTED_EDGE('',*,*,#15403,.T.);
#21927=ORIENTED_EDGE('',*,*,#15369,.T.);
#21928=ORIENTED_EDGE('',*,*,#15408,.F.);
#21929=ORIENTED_EDGE('',*,*,#15248,.T.);
#21930=ORIENTED_EDGE('',*,*,#15409,.F.);
#21931=ORIENTED_EDGE('',*,*,#15410,.F.);
#21932=ORIENTED_EDGE('',*,*,#15404,.T.);
#21933=ORIENTED_EDGE('',*,*,#15327,.T.);
#21934=ORIENTED_EDGE('',*,*,#15407,.T.);
#21935=ORIENTED_EDGE('',*,*,#15411,.T.);
#21936=ORIENTED_EDGE('',*,*,#15412,.F.);
#21937=ORIENTED_EDGE('',*,*,#15267,.T.);
#21938=ORIENTED_EDGE('',*,*,#15408,.T.);
#21939=ORIENTED_EDGE('',*,*,#15368,.T.);
#21940=ORIENTED_EDGE('',*,*,#15413,.F.);
#21941=ORIENTED_EDGE('',*,*,#15247,.T.);
#21942=ORIENTED_EDGE('',*,*,#15414,.F.);
#21943=ORIENTED_EDGE('',*,*,#15415,.T.);
#21944=ORIENTED_EDGE('',*,*,#15409,.T.);
#21945=ORIENTED_EDGE('',*,*,#15328,.T.);
#21946=ORIENTED_EDGE('',*,*,#15412,.T.);
#21947=ORIENTED_EDGE('',*,*,#15416,.T.);
#21948=ORIENTED_EDGE('',*,*,#15417,.F.);
#21949=ORIENTED_EDGE('',*,*,#15268,.T.);
#21950=ORIENTED_EDGE('',*,*,#15413,.T.);
#21951=ORIENTED_EDGE('',*,*,#15367,.T.);
#21952=ORIENTED_EDGE('',*,*,#15418,.F.);
#21953=ORIENTED_EDGE('',*,*,#15246,.T.);
#21954=ORIENTED_EDGE('',*,*,#15215,.T.);
#21955=ORIENTED_EDGE('',*,*,#15419,.F.);
#21956=ORIENTED_EDGE('',*,*,#15420,.F.);
#21957=ORIENTED_EDGE('',*,*,#15414,.T.);
#21958=ORIENTED_EDGE('',*,*,#15329,.T.);
#21959=ORIENTED_EDGE('',*,*,#15417,.T.);
#21960=ORIENTED_EDGE('',*,*,#15421,.T.);
#21961=ORIENTED_EDGE('',*,*,#15422,.F.);
#21962=ORIENTED_EDGE('',*,*,#15269,.T.);
#21963=ORIENTED_EDGE('',*,*,#15418,.T.);
#21964=ORIENTED_EDGE('',*,*,#15366,.T.);
#21965=ORIENTED_EDGE('',*,*,#15335,.T.);
#21966=ORIENTED_EDGE('',*,*,#15423,.F.);
#21967=ORIENTED_EDGE('',*,*,#15214,.T.);
#21968=ORIENTED_EDGE('',*,*,#15424,.F.);
#21969=ORIENTED_EDGE('',*,*,#15425,.T.);
#21970=ORIENTED_EDGE('',*,*,#15419,.T.);
#21971=ORIENTED_EDGE('',*,*,#15330,.T.);
#21972=ORIENTED_EDGE('',*,*,#15422,.T.);
#21973=ORIENTED_EDGE('',*,*,#15426,.T.);
#21974=ORIENTED_EDGE('',*,*,#15427,.F.);
#21975=ORIENTED_EDGE('',*,*,#15270,.T.);
#21976=ORIENTED_EDGE('',*,*,#15423,.T.);
#21977=ORIENTED_EDGE('',*,*,#15334,.T.);
#21978=ORIENTED_EDGE('',*,*,#15428,.F.);
#21979=ORIENTED_EDGE('',*,*,#15213,.T.);
#21980=ORIENTED_EDGE('',*,*,#15429,.F.);
#21981=ORIENTED_EDGE('',*,*,#15430,.F.);
#21982=ORIENTED_EDGE('',*,*,#15424,.T.);
#21983=ORIENTED_EDGE('',*,*,#15331,.T.);
#21984=ORIENTED_EDGE('',*,*,#15427,.T.);
#21985=ORIENTED_EDGE('',*,*,#15431,.T.);
#21986=ORIENTED_EDGE('',*,*,#15432,.F.);
#21987=ORIENTED_EDGE('',*,*,#15271,.T.);
#21988=ORIENTED_EDGE('',*,*,#15428,.T.);
#21989=ORIENTED_EDGE('',*,*,#15333,.T.);
#21990=ORIENTED_EDGE('',*,*,#15433,.F.);
#21991=ORIENTED_EDGE('',*,*,#15232,.T.);
#21992=ORIENTED_EDGE('',*,*,#15434,.T.);
#21993=ORIENTED_EDGE('',*,*,#15292,.T.);
#21994=ORIENTED_EDGE('',*,*,#15435,.T.);
#21995=ORIENTED_EDGE('',*,*,#15352,.T.);
#21996=ORIENTED_EDGE('',*,*,#15436,.T.);
#21997=ORIENTED_EDGE('',*,*,#15437,.F.);
#21998=ORIENTED_EDGE('',*,*,#15438,.F.);
#21999=ORIENTED_EDGE('',*,*,#15439,.T.);
#22000=ORIENTED_EDGE('',*,*,#15440,.T.);
#22001=ORIENTED_EDGE('',*,*,#15351,.T.);
#22002=ORIENTED_EDGE('',*,*,#15441,.T.);
#22003=ORIENTED_EDGE('',*,*,#15442,.F.);
#22004=ORIENTED_EDGE('',*,*,#15436,.F.);
#22005=ORIENTED_EDGE('',*,*,#15291,.T.);
#22006=ORIENTED_EDGE('',*,*,#15443,.T.);
#22007=ORIENTED_EDGE('',*,*,#15353,.T.);
#22008=ORIENTED_EDGE('',*,*,#15435,.F.);
#22009=ORIENTED_EDGE('',*,*,#15231,.T.);
#22010=ORIENTED_EDGE('',*,*,#15444,.T.);
#22011=ORIENTED_EDGE('',*,*,#15293,.T.);
#22012=ORIENTED_EDGE('',*,*,#15434,.F.);
#22013=ORIENTED_EDGE('',*,*,#15350,.T.);
#22014=ORIENTED_EDGE('',*,*,#15445,.T.);
#22015=ORIENTED_EDGE('',*,*,#15446,.F.);
#22016=ORIENTED_EDGE('',*,*,#15441,.F.);
#22017=ORIENTED_EDGE('',*,*,#15290,.T.);
#22018=ORIENTED_EDGE('',*,*,#15447,.T.);
#22019=ORIENTED_EDGE('',*,*,#15354,.T.);
#22020=ORIENTED_EDGE('',*,*,#15443,.F.);
#22021=ORIENTED_EDGE('',*,*,#15230,.T.);
#22022=ORIENTED_EDGE('',*,*,#15448,.T.);
#22023=ORIENTED_EDGE('',*,*,#15294,.T.);
#22024=ORIENTED_EDGE('',*,*,#15444,.F.);
#22025=ORIENTED_EDGE('',*,*,#15349,.T.);
#22026=ORIENTED_EDGE('',*,*,#15449,.T.);
#22027=ORIENTED_EDGE('',*,*,#15450,.F.);
#22028=ORIENTED_EDGE('',*,*,#15445,.F.);
#22029=ORIENTED_EDGE('',*,*,#15289,.T.);
#22030=ORIENTED_EDGE('',*,*,#15451,.T.);
#22031=ORIENTED_EDGE('',*,*,#15355,.T.);
#22032=ORIENTED_EDGE('',*,*,#15447,.F.);
#22033=ORIENTED_EDGE('',*,*,#15229,.T.);
#22034=ORIENTED_EDGE('',*,*,#15452,.T.);
#22035=ORIENTED_EDGE('',*,*,#15295,.T.);
#22036=ORIENTED_EDGE('',*,*,#15448,.F.);
#22037=ORIENTED_EDGE('',*,*,#15348,.T.);
#22038=ORIENTED_EDGE('',*,*,#15453,.T.);
#22039=ORIENTED_EDGE('',*,*,#15454,.F.);
#22040=ORIENTED_EDGE('',*,*,#15449,.F.);
#22041=ORIENTED_EDGE('',*,*,#15288,.T.);
#22042=ORIENTED_EDGE('',*,*,#15455,.T.);
#22043=ORIENTED_EDGE('',*,*,#15360,.T.);
#22044=ORIENTED_EDGE('',*,*,#15356,.T.);
#22045=ORIENTED_EDGE('',*,*,#15451,.F.);
#22046=ORIENTED_EDGE('',*,*,#15228,.T.);
#22047=ORIENTED_EDGE('',*,*,#15456,.T.);
#22048=ORIENTED_EDGE('',*,*,#15300,.T.);
#22049=ORIENTED_EDGE('',*,*,#15296,.T.);
#22050=ORIENTED_EDGE('',*,*,#15452,.F.);
#22051=ORIENTED_EDGE('',*,*,#15347,.T.);
#22052=ORIENTED_EDGE('',*,*,#15457,.T.);
#22053=ORIENTED_EDGE('',*,*,#15458,.F.);
#22054=ORIENTED_EDGE('',*,*,#15453,.F.);
#22055=ORIENTED_EDGE('',*,*,#15287,.T.);
#22056=ORIENTED_EDGE('',*,*,#15459,.T.);
#22057=ORIENTED_EDGE('',*,*,#15361,.T.);
#22058=ORIENTED_EDGE('',*,*,#15455,.F.);
#22059=ORIENTED_EDGE('',*,*,#15227,.T.);
#22060=ORIENTED_EDGE('',*,*,#15460,.T.);
#22061=ORIENTED_EDGE('',*,*,#15301,.T.);
#22062=ORIENTED_EDGE('',*,*,#15456,.F.);
#22063=ORIENTED_EDGE('',*,*,#15346,.T.);
#22064=ORIENTED_EDGE('',*,*,#15461,.T.);
#22065=ORIENTED_EDGE('',*,*,#15462,.F.);
#22066=ORIENTED_EDGE('',*,*,#15457,.F.);
#22067=ORIENTED_EDGE('',*,*,#15286,.T.);
#22068=ORIENTED_EDGE('',*,*,#15463,.T.);
#22069=ORIENTED_EDGE('',*,*,#15362,.T.);
#22070=ORIENTED_EDGE('',*,*,#15459,.F.);
#22071=ORIENTED_EDGE('',*,*,#15226,.T.);
#22072=ORIENTED_EDGE('',*,*,#15464,.T.);
#22073=ORIENTED_EDGE('',*,*,#15302,.T.);
#22074=ORIENTED_EDGE('',*,*,#15460,.F.);
#22075=ORIENTED_EDGE('',*,*,#15345,.T.);
#22076=ORIENTED_EDGE('',*,*,#15465,.T.);
#22077=ORIENTED_EDGE('',*,*,#15466,.F.);
#22078=ORIENTED_EDGE('',*,*,#15461,.F.);
#22079=ORIENTED_EDGE('',*,*,#15285,.T.);
#22080=ORIENTED_EDGE('',*,*,#15467,.T.);
#22081=ORIENTED_EDGE('',*,*,#15363,.T.);
#22082=ORIENTED_EDGE('',*,*,#15463,.F.);
#22083=ORIENTED_EDGE('',*,*,#15225,.T.);
#22084=ORIENTED_EDGE('',*,*,#15468,.T.);
#22085=ORIENTED_EDGE('',*,*,#15303,.T.);
#22086=ORIENTED_EDGE('',*,*,#15464,.F.);
#22087=ORIENTED_EDGE('',*,*,#15344,.T.);
#22088=ORIENTED_EDGE('',*,*,#15469,.T.);
#22089=ORIENTED_EDGE('',*,*,#15470,.F.);
#22090=ORIENTED_EDGE('',*,*,#15465,.F.);
#22091=ORIENTED_EDGE('',*,*,#15284,.T.);
#22092=ORIENTED_EDGE('',*,*,#15471,.T.);
#22093=ORIENTED_EDGE('',*,*,#15364,.T.);
#22094=ORIENTED_EDGE('',*,*,#15467,.F.);
#22095=ORIENTED_EDGE('',*,*,#15224,.T.);
#22096=ORIENTED_EDGE('',*,*,#15472,.T.);
#22097=ORIENTED_EDGE('',*,*,#15304,.T.);
#22098=ORIENTED_EDGE('',*,*,#15468,.F.);
#22099=ORIENTED_EDGE('',*,*,#15343,.T.);
#22100=ORIENTED_EDGE('',*,*,#15473,.T.);
#22101=ORIENTED_EDGE('',*,*,#15474,.F.);
#22102=ORIENTED_EDGE('',*,*,#15469,.F.);
#22103=ORIENTED_EDGE('',*,*,#15283,.T.);
#22104=ORIENTED_EDGE('',*,*,#15475,.T.);
#22105=ORIENTED_EDGE('',*,*,#15337,.T.);
#22106=ORIENTED_EDGE('',*,*,#15365,.T.);
#22107=ORIENTED_EDGE('',*,*,#15471,.F.);
#22108=ORIENTED_EDGE('',*,*,#15223,.T.);
#22109=ORIENTED_EDGE('',*,*,#15476,.T.);
#22110=ORIENTED_EDGE('',*,*,#15277,.T.);
#22111=ORIENTED_EDGE('',*,*,#15305,.T.);
#22112=ORIENTED_EDGE('',*,*,#15472,.F.);
#22113=ORIENTED_EDGE('',*,*,#15342,.T.);
#22114=ORIENTED_EDGE('',*,*,#15477,.T.);
#22115=ORIENTED_EDGE('',*,*,#15478,.F.);
#22116=ORIENTED_EDGE('',*,*,#15473,.F.);
#22117=ORIENTED_EDGE('',*,*,#15282,.T.);
#22118=ORIENTED_EDGE('',*,*,#15479,.T.);
#22119=ORIENTED_EDGE('',*,*,#15338,.T.);
#22120=ORIENTED_EDGE('',*,*,#15475,.F.);
#22121=ORIENTED_EDGE('',*,*,#15222,.T.);
#22122=ORIENTED_EDGE('',*,*,#15480,.T.);
#22123=ORIENTED_EDGE('',*,*,#15278,.T.);
#22124=ORIENTED_EDGE('',*,*,#15476,.F.);
#22125=ORIENTED_EDGE('',*,*,#15341,.T.);
#22126=ORIENTED_EDGE('',*,*,#15481,.T.);
#22127=ORIENTED_EDGE('',*,*,#15482,.F.);
#22128=ORIENTED_EDGE('',*,*,#15477,.F.);
#22129=ORIENTED_EDGE('',*,*,#15281,.T.);
#22130=ORIENTED_EDGE('',*,*,#15483,.T.);
#22131=ORIENTED_EDGE('',*,*,#15339,.T.);
#22132=ORIENTED_EDGE('',*,*,#15479,.F.);
#22133=ORIENTED_EDGE('',*,*,#15221,.T.);
#22134=ORIENTED_EDGE('',*,*,#15484,.T.);
#22135=ORIENTED_EDGE('',*,*,#15279,.T.);
#22136=ORIENTED_EDGE('',*,*,#15480,.F.);
#22137=ORIENTED_EDGE('',*,*,#15485,.F.);
#22138=ORIENTED_EDGE('',*,*,#15486,.T.);
#22139=ORIENTED_EDGE('',*,*,#15487,.F.);
#22140=ORIENTED_EDGE('',*,*,#15486,.F.);
#22141=ORIENTED_EDGE('',*,*,#15488,.F.);
#22142=ORIENTED_EDGE('',*,*,#15489,.T.);
#22143=ORIENTED_EDGE('',*,*,#15490,.F.);
#22144=ORIENTED_EDGE('',*,*,#15489,.F.);
#22145=ORIENTED_EDGE('',*,*,#15491,.F.);
#22146=ORIENTED_EDGE('',*,*,#15492,.T.);
#22147=ORIENTED_EDGE('',*,*,#15493,.F.);
#22148=ORIENTED_EDGE('',*,*,#15492,.F.);
#22149=ORIENTED_EDGE('',*,*,#15494,.T.);
#22150=ORIENTED_EDGE('',*,*,#15495,.T.);
#22151=ORIENTED_EDGE('',*,*,#15496,.T.);
#22152=ORIENTED_EDGE('',*,*,#15497,.F.);
#22153=ORIENTED_EDGE('',*,*,#15179,.T.);
#22154=ORIENTED_EDGE('',*,*,#15191,.F.);
#22155=ORIENTED_EDGE('',*,*,#15498,.F.);
#22156=ORIENTED_EDGE('',*,*,#15499,.T.);
#22157=ORIENTED_EDGE('',*,*,#15500,.T.);
#22158=ORIENTED_EDGE('',*,*,#15187,.F.);
#22159=ORIENTED_EDGE('',*,*,#15183,.T.);
#22160=ORIENTED_EDGE('',*,*,#15186,.F.);
#22161=ORIENTED_EDGE('',*,*,#15501,.F.);
#22162=ORIENTED_EDGE('',*,*,#15502,.T.);
#22163=ORIENTED_EDGE('',*,*,#15503,.T.);
#22164=ORIENTED_EDGE('',*,*,#15499,.F.);
#22165=ORIENTED_EDGE('',*,*,#15504,.F.);
#22166=ORIENTED_EDGE('',*,*,#15505,.T.);
#22167=ORIENTED_EDGE('',*,*,#15506,.T.);
#22168=ORIENTED_EDGE('',*,*,#15502,.F.);
#22169=ORIENTED_EDGE('',*,*,#15212,.T.);
#22170=ORIENTED_EDGE('',*,*,#15507,.T.);
#22171=ORIENTED_EDGE('',*,*,#15272,.T.);
#22172=ORIENTED_EDGE('',*,*,#15433,.T.);
#22173=ORIENTED_EDGE('',*,*,#15332,.T.);
#22174=ORIENTED_EDGE('',*,*,#15432,.T.);
#22175=ORIENTED_EDGE('',*,*,#15508,.T.);
#22176=ORIENTED_EDGE('',*,*,#15505,.F.);
#22177=ORIENTED_EDGE('',*,*,#15509,.F.);
#22178=ORIENTED_EDGE('',*,*,#15429,.T.);
#22179=ORIENTED_EDGE('',*,*,#15211,.T.);
#22180=ORIENTED_EDGE('',*,*,#15510,.T.);
#22181=ORIENTED_EDGE('',*,*,#15273,.T.);
#22182=ORIENTED_EDGE('',*,*,#15507,.F.);
#22183=ORIENTED_EDGE('',*,*,#15210,.T.);
#22184=ORIENTED_EDGE('',*,*,#15511,.T.);
#22185=ORIENTED_EDGE('',*,*,#15274,.T.);
#22186=ORIENTED_EDGE('',*,*,#15510,.F.);
#22187=ORIENTED_EDGE('',*,*,#15209,.T.);
#22188=ORIENTED_EDGE('',*,*,#15512,.T.);
#22189=ORIENTED_EDGE('',*,*,#15306,.T.);
#22190=ORIENTED_EDGE('',*,*,#15275,.T.);
#22191=ORIENTED_EDGE('',*,*,#15511,.F.);
#22192=ORIENTED_EDGE('',*,*,#15208,.T.);
#22193=ORIENTED_EDGE('',*,*,#15513,.T.);
#22194=ORIENTED_EDGE('',*,*,#15307,.T.);
#22195=ORIENTED_EDGE('',*,*,#15512,.F.);
#22196=ORIENTED_EDGE('',*,*,#15207,.T.);
#22197=ORIENTED_EDGE('',*,*,#15514,.T.);
#22198=ORIENTED_EDGE('',*,*,#15308,.T.);
#22199=ORIENTED_EDGE('',*,*,#15513,.F.);
#22200=ORIENTED_EDGE('',*,*,#15206,.T.);
#22201=ORIENTED_EDGE('',*,*,#15515,.T.);
#22202=ORIENTED_EDGE('',*,*,#15309,.T.);
#22203=ORIENTED_EDGE('',*,*,#15514,.F.);
#22204=ORIENTED_EDGE('',*,*,#15205,.T.);
#22205=ORIENTED_EDGE('',*,*,#15516,.T.);
#22206=ORIENTED_EDGE('',*,*,#15310,.T.);
#22207=ORIENTED_EDGE('',*,*,#15515,.F.);
#22208=ORIENTED_EDGE('',*,*,#15204,.T.);
#22209=ORIENTED_EDGE('',*,*,#15517,.T.);
#22210=ORIENTED_EDGE('',*,*,#15256,.T.);
#22211=ORIENTED_EDGE('',*,*,#15311,.T.);
#22212=ORIENTED_EDGE('',*,*,#15516,.F.);
#22213=ORIENTED_EDGE('',*,*,#15203,.T.);
#22214=ORIENTED_EDGE('',*,*,#15518,.T.);
#22215=ORIENTED_EDGE('',*,*,#15257,.T.);
#22216=ORIENTED_EDGE('',*,*,#15517,.F.);
#22217=ORIENTED_EDGE('',*,*,#15202,.T.);
#22218=ORIENTED_EDGE('',*,*,#15519,.T.);
#22219=ORIENTED_EDGE('',*,*,#15258,.T.);
#22220=ORIENTED_EDGE('',*,*,#15518,.F.);
#22221=ORIENTED_EDGE('',*,*,#15201,.T.);
#22222=ORIENTED_EDGE('',*,*,#15378,.T.);
#22223=ORIENTED_EDGE('',*,*,#15259,.T.);
#22224=ORIENTED_EDGE('',*,*,#15519,.F.);
#22225=ORIENTED_EDGE('',*,*,#15520,.F.);
#22226=ORIENTED_EDGE('',*,*,#15521,.T.);
#22227=ORIENTED_EDGE('',*,*,#15522,.T.);
#22228=ORIENTED_EDGE('',*,*,#15374,.F.);
#22229=ORIENTED_EDGE('',*,*,#15523,.F.);
#22230=ORIENTED_EDGE('',*,*,#15524,.T.);
#22231=ORIENTED_EDGE('',*,*,#15525,.T.);
#22232=ORIENTED_EDGE('',*,*,#15521,.F.);
#22233=ORIENTED_EDGE('',*,*,#15526,.F.);
#22234=ORIENTED_EDGE('',*,*,#15527,.T.);
#22235=ORIENTED_EDGE('',*,*,#15528,.T.);
#22236=ORIENTED_EDGE('',*,*,#15524,.F.);
#22237=ORIENTED_EDGE('',*,*,#15529,.F.);
#22238=ORIENTED_EDGE('',*,*,#15530,.T.);
#22239=ORIENTED_EDGE('',*,*,#15531,.T.);
#22240=ORIENTED_EDGE('',*,*,#15527,.F.);
#22241=ORIENTED_EDGE('',*,*,#15532,.F.);
#22242=ORIENTED_EDGE('',*,*,#15533,.T.);
#22243=ORIENTED_EDGE('',*,*,#15534,.T.);
#22244=ORIENTED_EDGE('',*,*,#15530,.F.);
#22245=ORIENTED_EDGE('',*,*,#15194,.T.);
#22246=ORIENTED_EDGE('',*,*,#15254,.T.);
#22247=ORIENTED_EDGE('',*,*,#15314,.T.);
#22248=ORIENTED_EDGE('',*,*,#15535,.T.);
#22249=ORIENTED_EDGE('',*,*,#15536,.T.);
#22250=ORIENTED_EDGE('',*,*,#15537,.T.);
#22251=ORIENTED_EDGE('',*,*,#15533,.F.);
#22252=ORIENTED_EDGE('',*,*,#15538,.F.);
#22253=ORIENTED_EDGE('',*,*,#15539,.T.);
#22254=ORIENTED_EDGE('',*,*,#15540,.T.);
#22255=ORIENTED_EDGE('',*,*,#15536,.F.);
#22256=ORIENTED_EDGE('',*,*,#15541,.F.);
#22257=ORIENTED_EDGE('',*,*,#15542,.T.);
#22258=ORIENTED_EDGE('',*,*,#15543,.T.);
#22259=ORIENTED_EDGE('',*,*,#15539,.F.);
#22260=ORIENTED_EDGE('',*,*,#15544,.F.);
#22261=ORIENTED_EDGE('',*,*,#15545,.T.);
#22262=ORIENTED_EDGE('',*,*,#15546,.T.);
#22263=ORIENTED_EDGE('',*,*,#15542,.F.);
#22264=ORIENTED_EDGE('',*,*,#15547,.F.);
#22265=ORIENTED_EDGE('',*,*,#15548,.T.);
#22266=ORIENTED_EDGE('',*,*,#15549,.T.);
#22267=ORIENTED_EDGE('',*,*,#15545,.F.);
#22268=ORIENTED_EDGE('',*,*,#15550,.F.);
#22269=ORIENTED_EDGE('',*,*,#15551,.T.);
#22270=ORIENTED_EDGE('',*,*,#15552,.T.);
#22271=ORIENTED_EDGE('',*,*,#15548,.F.);
#22272=ORIENTED_EDGE('',*,*,#15485,.T.);
#22273=ORIENTED_EDGE('',*,*,#15488,.T.);
#22274=ORIENTED_EDGE('',*,*,#15491,.T.);
#22275=ORIENTED_EDGE('',*,*,#15553,.F.);
#22276=ORIENTED_EDGE('',*,*,#15554,.T.);
#22277=ORIENTED_EDGE('',*,*,#15555,.T.);
#22278=ORIENTED_EDGE('',*,*,#15551,.F.);
#22279=ORIENTED_EDGE('',*,*,#15556,.F.);
#22280=ORIENTED_EDGE('',*,*,#15557,.T.);
#22281=ORIENTED_EDGE('',*,*,#15558,.T.);
#22282=ORIENTED_EDGE('',*,*,#15554,.F.);
#22283=ORIENTED_EDGE('',*,*,#15559,.F.);
#22284=ORIENTED_EDGE('',*,*,#15560,.T.);
#22285=ORIENTED_EDGE('',*,*,#15561,.T.);
#22286=ORIENTED_EDGE('',*,*,#15557,.F.);
#22287=ORIENTED_EDGE('',*,*,#15562,.F.);
#22288=ORIENTED_EDGE('',*,*,#15563,.T.);
#22289=ORIENTED_EDGE('',*,*,#15564,.T.);
#22290=ORIENTED_EDGE('',*,*,#15560,.F.);
#22291=ORIENTED_EDGE('',*,*,#15487,.T.);
#22292=ORIENTED_EDGE('',*,*,#15490,.T.);
#22293=ORIENTED_EDGE('',*,*,#15493,.T.);
#22294=ORIENTED_EDGE('',*,*,#15565,.T.);
#22295=ORIENTED_EDGE('',*,*,#15566,.T.);
#22296=ORIENTED_EDGE('',*,*,#15567,.T.);
#22297=ORIENTED_EDGE('',*,*,#15563,.F.);
#22298=ORIENTED_EDGE('',*,*,#15568,.F.);
#22299=ORIENTED_EDGE('',*,*,#15569,.T.);
#22300=ORIENTED_EDGE('',*,*,#15570,.T.);
#22301=ORIENTED_EDGE('',*,*,#15566,.F.);
#22302=ORIENTED_EDGE('',*,*,#15571,.F.);
#22303=ORIENTED_EDGE('',*,*,#15572,.T.);
#22304=ORIENTED_EDGE('',*,*,#15573,.T.);
#22305=ORIENTED_EDGE('',*,*,#15569,.F.);
#22306=ORIENTED_EDGE('',*,*,#15574,.F.);
#22307=ORIENTED_EDGE('',*,*,#15497,.T.);
#22308=ORIENTED_EDGE('',*,*,#15575,.T.);
#22309=ORIENTED_EDGE('',*,*,#15572,.F.);
#22310=ORIENTED_EDGE('',*,*,#15576,.F.);
#22311=ORIENTED_EDGE('',*,*,#15577,.T.);
#22312=ORIENTED_EDGE('',*,*,#15578,.F.);
#22313=ORIENTED_EDGE('',*,*,#15495,.F.);
#22314=ORIENTED_EDGE('',*,*,#15579,.T.);
#22315=ORIENTED_EDGE('',*,*,#15189,.T.);
#22316=ORIENTED_EDGE('',*,*,#15580,.F.);
#22317=ORIENTED_EDGE('',*,*,#15581,.F.);
#22318=ORIENTED_EDGE('',*,*,#15582,.T.);
#22319=ORIENTED_EDGE('',*,*,#15581,.T.);
#22320=ORIENTED_EDGE('',*,*,#15583,.F.);
#22321=ORIENTED_EDGE('',*,*,#15584,.F.);
#22322=ORIENTED_EDGE('',*,*,#15220,.T.);
#22323=ORIENTED_EDGE('',*,*,#15585,.F.);
#22324=ORIENTED_EDGE('',*,*,#15586,.T.);
#22325=ORIENTED_EDGE('',*,*,#15584,.T.);
#22326=ORIENTED_EDGE('',*,*,#15587,.F.);
#22327=ORIENTED_EDGE('',*,*,#15481,.F.);
#22328=ORIENTED_EDGE('',*,*,#15340,.T.);
#22329=ORIENTED_EDGE('',*,*,#15483,.F.);
#22330=ORIENTED_EDGE('',*,*,#15280,.T.);
#22331=ORIENTED_EDGE('',*,*,#15484,.F.);
#22332=ORIENTED_EDGE('',*,*,#15219,.T.);
#22333=ORIENTED_EDGE('',*,*,#15588,.F.);
#22334=ORIENTED_EDGE('',*,*,#15589,.T.);
#22335=ORIENTED_EDGE('',*,*,#15585,.T.);
#22336=ORIENTED_EDGE('',*,*,#15218,.T.);
#22337=ORIENTED_EDGE('',*,*,#15590,.F.);
#22338=ORIENTED_EDGE('',*,*,#15591,.F.);
#22339=ORIENTED_EDGE('',*,*,#15588,.T.);
#22340=ORIENTED_EDGE('',*,*,#15217,.T.);
#22341=ORIENTED_EDGE('',*,*,#15245,.T.);
#22342=ORIENTED_EDGE('',*,*,#15592,.F.);
#22343=ORIENTED_EDGE('',*,*,#15593,.T.);
#22344=ORIENTED_EDGE('',*,*,#15590,.T.);
#22345=ORIENTED_EDGE('',*,*,#15244,.T.);
#22346=ORIENTED_EDGE('',*,*,#15594,.F.);
#22347=ORIENTED_EDGE('',*,*,#15595,.F.);
#22348=ORIENTED_EDGE('',*,*,#15592,.T.);
#22349=ORIENTED_EDGE('',*,*,#15243,.T.);
#22350=ORIENTED_EDGE('',*,*,#15596,.F.);
#22351=ORIENTED_EDGE('',*,*,#15597,.T.);
#22352=ORIENTED_EDGE('',*,*,#15594,.T.);
#22353=ORIENTED_EDGE('',*,*,#15242,.T.);
#22354=ORIENTED_EDGE('',*,*,#15598,.F.);
#22355=ORIENTED_EDGE('',*,*,#15599,.F.);
#22356=ORIENTED_EDGE('',*,*,#15596,.T.);
#22357=ORIENTED_EDGE('',*,*,#15241,.T.);
#22358=ORIENTED_EDGE('',*,*,#15600,.F.);
#22359=ORIENTED_EDGE('',*,*,#15601,.T.);
#22360=ORIENTED_EDGE('',*,*,#15598,.T.);
#22361=ORIENTED_EDGE('',*,*,#15240,.T.);
#22362=ORIENTED_EDGE('',*,*,#15236,.T.);
#22363=ORIENTED_EDGE('',*,*,#15602,.F.);
#22364=ORIENTED_EDGE('',*,*,#15603,.F.);
#22365=ORIENTED_EDGE('',*,*,#15600,.T.);
#22366=ORIENTED_EDGE('',*,*,#15235,.T.);
#22367=ORIENTED_EDGE('',*,*,#15604,.F.);
#22368=ORIENTED_EDGE('',*,*,#15605,.T.);
#22369=ORIENTED_EDGE('',*,*,#15602,.T.);
#22370=ORIENTED_EDGE('',*,*,#15234,.T.);
#22371=ORIENTED_EDGE('',*,*,#15606,.F.);
#22372=ORIENTED_EDGE('',*,*,#15607,.F.);
#22373=ORIENTED_EDGE('',*,*,#15604,.T.);
#22374=ORIENTED_EDGE('',*,*,#15233,.T.);
#22375=ORIENTED_EDGE('',*,*,#15440,.F.);
#22376=ORIENTED_EDGE('',*,*,#15608,.T.);
#22377=ORIENTED_EDGE('',*,*,#15606,.T.);
#22378=ORIENTED_EDGE('',*,*,#15609,.T.);
#22379=ORIENTED_EDGE('',*,*,#15438,.T.);
#22380=ORIENTED_EDGE('',*,*,#15610,.F.);
#22381=ORIENTED_EDGE('',*,*,#15611,.F.);
#22382=ORIENTED_EDGE('',*,*,#15612,.T.);
#22383=ORIENTED_EDGE('',*,*,#15611,.T.);
#22384=ORIENTED_EDGE('',*,*,#15613,.F.);
#22385=ORIENTED_EDGE('',*,*,#15614,.F.);
#22386=ORIENTED_EDGE('',*,*,#15615,.T.);
#22387=ORIENTED_EDGE('',*,*,#15614,.T.);
#22388=ORIENTED_EDGE('',*,*,#15616,.F.);
#22389=ORIENTED_EDGE('',*,*,#15617,.F.);
#22390=ORIENTED_EDGE('',*,*,#15618,.T.);
#22391=ORIENTED_EDGE('',*,*,#15617,.T.);
#22392=ORIENTED_EDGE('',*,*,#15619,.F.);
#22393=ORIENTED_EDGE('',*,*,#15620,.F.);
#22394=ORIENTED_EDGE('',*,*,#15621,.T.);
#22395=ORIENTED_EDGE('',*,*,#15620,.T.);
#22396=ORIENTED_EDGE('',*,*,#15622,.F.);
#22397=ORIENTED_EDGE('',*,*,#15623,.F.);
#22398=ORIENTED_EDGE('',*,*,#15238,.T.);
#22399=ORIENTED_EDGE('',*,*,#15239,.T.);
#22400=ORIENTED_EDGE('',*,*,#15192,.T.);
#22401=ORIENTED_EDGE('',*,*,#15298,.T.);
#22402=ORIENTED_EDGE('',*,*,#15299,.T.);
#22403=ORIENTED_EDGE('',*,*,#15252,.T.);
#22404=ORIENTED_EDGE('',*,*,#15358,.T.);
#22405=ORIENTED_EDGE('',*,*,#15359,.T.);
#22406=ORIENTED_EDGE('',*,*,#15312,.T.);
#22407=ORIENTED_EDGE('',*,*,#15624,.F.);
#22408=ORIENTED_EDGE('',*,*,#15623,.T.);
#22409=ORIENTED_EDGE('',*,*,#15625,.F.);
#22410=ORIENTED_EDGE('',*,*,#15626,.F.);
#22411=ORIENTED_EDGE('',*,*,#15627,.T.);
#22412=ORIENTED_EDGE('',*,*,#15626,.T.);
#22413=ORIENTED_EDGE('',*,*,#15628,.F.);
#22414=ORIENTED_EDGE('',*,*,#15629,.F.);
#22415=ORIENTED_EDGE('',*,*,#15630,.T.);
#22416=ORIENTED_EDGE('',*,*,#15629,.T.);
#22417=ORIENTED_EDGE('',*,*,#15631,.F.);
#22418=ORIENTED_EDGE('',*,*,#15632,.F.);
#22419=ORIENTED_EDGE('',*,*,#15633,.T.);
#22420=ORIENTED_EDGE('',*,*,#15632,.T.);
#22421=ORIENTED_EDGE('',*,*,#15634,.F.);
#22422=ORIENTED_EDGE('',*,*,#15635,.F.);
#22423=ORIENTED_EDGE('',*,*,#15636,.T.);
#22424=ORIENTED_EDGE('',*,*,#15635,.T.);
#22425=ORIENTED_EDGE('',*,*,#15637,.F.);
#22426=ORIENTED_EDGE('',*,*,#15638,.F.);
#22427=ORIENTED_EDGE('',*,*,#15639,.T.);
#22428=ORIENTED_EDGE('',*,*,#15638,.T.);
#22429=ORIENTED_EDGE('',*,*,#15640,.F.);
#22430=ORIENTED_EDGE('',*,*,#15641,.F.);
#22431=ORIENTED_EDGE('',*,*,#15642,.T.);
#22432=ORIENTED_EDGE('',*,*,#15641,.T.);
#22433=ORIENTED_EDGE('',*,*,#15643,.F.);
#22434=ORIENTED_EDGE('',*,*,#15644,.F.);
#22435=ORIENTED_EDGE('',*,*,#15645,.T.);
#22436=ORIENTED_EDGE('',*,*,#15644,.T.);
#22437=ORIENTED_EDGE('',*,*,#15646,.F.);
#22438=ORIENTED_EDGE('',*,*,#15647,.F.);
#22439=ORIENTED_EDGE('',*,*,#15648,.T.);
#22440=ORIENTED_EDGE('',*,*,#15647,.T.);
#22441=ORIENTED_EDGE('',*,*,#15649,.F.);
#22442=ORIENTED_EDGE('',*,*,#15650,.F.);
#22443=ORIENTED_EDGE('',*,*,#15651,.T.);
#22444=ORIENTED_EDGE('',*,*,#15650,.T.);
#22445=ORIENTED_EDGE('',*,*,#15652,.F.);
#22446=ORIENTED_EDGE('',*,*,#15653,.F.);
#22447=ORIENTED_EDGE('',*,*,#15654,.F.);
#22448=ORIENTED_EDGE('',*,*,#15653,.T.);
#22449=ORIENTED_EDGE('',*,*,#15655,.F.);
#22450=ORIENTED_EDGE('',*,*,#15656,.F.);
#22451=ORIENTED_EDGE('',*,*,#15657,.T.);
#22452=ORIENTED_EDGE('',*,*,#15656,.T.);
#22453=ORIENTED_EDGE('',*,*,#15658,.F.);
#22454=ORIENTED_EDGE('',*,*,#15659,.F.);
#22455=ORIENTED_EDGE('',*,*,#15660,.T.);
#22456=ORIENTED_EDGE('',*,*,#15659,.T.);
#22457=ORIENTED_EDGE('',*,*,#15661,.F.);
#22458=ORIENTED_EDGE('',*,*,#15662,.F.);
#22459=ORIENTED_EDGE('',*,*,#15663,.T.);
#22460=ORIENTED_EDGE('',*,*,#15662,.T.);
#22461=ORIENTED_EDGE('',*,*,#15664,.F.);
#22462=ORIENTED_EDGE('',*,*,#15577,.F.);
#22463=ORIENTED_EDGE('',*,*,#15664,.T.);
#22464=ORIENTED_EDGE('',*,*,#15661,.T.);
#22465=ORIENTED_EDGE('',*,*,#15658,.T.);
#22466=ORIENTED_EDGE('',*,*,#15655,.T.);
#22467=ORIENTED_EDGE('',*,*,#15652,.T.);
#22468=ORIENTED_EDGE('',*,*,#15649,.T.);
#22469=ORIENTED_EDGE('',*,*,#15646,.T.);
#22470=ORIENTED_EDGE('',*,*,#15643,.T.);
#22471=ORIENTED_EDGE('',*,*,#15640,.T.);
#22472=ORIENTED_EDGE('',*,*,#15637,.T.);
#22473=ORIENTED_EDGE('',*,*,#15634,.T.);
#22474=ORIENTED_EDGE('',*,*,#15631,.T.);
#22475=ORIENTED_EDGE('',*,*,#15628,.T.);
#22476=ORIENTED_EDGE('',*,*,#15625,.T.);
#22477=ORIENTED_EDGE('',*,*,#15622,.T.);
#22478=ORIENTED_EDGE('',*,*,#15619,.T.);
#22479=ORIENTED_EDGE('',*,*,#15616,.T.);
#22480=ORIENTED_EDGE('',*,*,#15613,.T.);
#22481=ORIENTED_EDGE('',*,*,#15610,.T.);
#22482=ORIENTED_EDGE('',*,*,#15437,.T.);
#22483=ORIENTED_EDGE('',*,*,#15442,.T.);
#22484=ORIENTED_EDGE('',*,*,#15446,.T.);
#22485=ORIENTED_EDGE('',*,*,#15450,.T.);
#22486=ORIENTED_EDGE('',*,*,#15454,.T.);
#22487=ORIENTED_EDGE('',*,*,#15458,.T.);
#22488=ORIENTED_EDGE('',*,*,#15462,.T.);
#22489=ORIENTED_EDGE('',*,*,#15466,.T.);
#22490=ORIENTED_EDGE('',*,*,#15470,.T.);
#22491=ORIENTED_EDGE('',*,*,#15474,.T.);
#22492=ORIENTED_EDGE('',*,*,#15478,.T.);
#22493=ORIENTED_EDGE('',*,*,#15482,.T.);
#22494=ORIENTED_EDGE('',*,*,#15587,.T.);
#22495=ORIENTED_EDGE('',*,*,#15583,.T.);
#22496=ORIENTED_EDGE('',*,*,#15580,.T.);
#22497=ORIENTED_EDGE('',*,*,#15188,.T.);
#22498=ORIENTED_EDGE('',*,*,#15500,.F.);
#22499=ORIENTED_EDGE('',*,*,#15503,.F.);
#22500=ORIENTED_EDGE('',*,*,#15506,.F.);
#22501=ORIENTED_EDGE('',*,*,#15508,.F.);
#22502=ORIENTED_EDGE('',*,*,#15431,.F.);
#22503=ORIENTED_EDGE('',*,*,#15426,.F.);
#22504=ORIENTED_EDGE('',*,*,#15421,.F.);
#22505=ORIENTED_EDGE('',*,*,#15416,.F.);
#22506=ORIENTED_EDGE('',*,*,#15411,.F.);
#22507=ORIENTED_EDGE('',*,*,#15406,.F.);
#22508=ORIENTED_EDGE('',*,*,#15401,.F.);
#22509=ORIENTED_EDGE('',*,*,#15396,.F.);
#22510=ORIENTED_EDGE('',*,*,#15391,.F.);
#22511=ORIENTED_EDGE('',*,*,#15386,.F.);
#22512=ORIENTED_EDGE('',*,*,#15381,.F.);
#22513=ORIENTED_EDGE('',*,*,#15375,.F.);
#22514=ORIENTED_EDGE('',*,*,#15522,.F.);
#22515=ORIENTED_EDGE('',*,*,#15525,.F.);
#22516=ORIENTED_EDGE('',*,*,#15528,.F.);
#22517=ORIENTED_EDGE('',*,*,#15531,.F.);
#22518=ORIENTED_EDGE('',*,*,#15534,.F.);
#22519=ORIENTED_EDGE('',*,*,#15537,.F.);
#22520=ORIENTED_EDGE('',*,*,#15540,.F.);
#22521=ORIENTED_EDGE('',*,*,#15543,.F.);
#22522=ORIENTED_EDGE('',*,*,#15546,.F.);
#22523=ORIENTED_EDGE('',*,*,#15549,.F.);
#22524=ORIENTED_EDGE('',*,*,#15552,.F.);
#22525=ORIENTED_EDGE('',*,*,#15555,.F.);
#22526=ORIENTED_EDGE('',*,*,#15558,.F.);
#22527=ORIENTED_EDGE('',*,*,#15561,.F.);
#22528=ORIENTED_EDGE('',*,*,#15564,.F.);
#22529=ORIENTED_EDGE('',*,*,#15567,.F.);
#22530=ORIENTED_EDGE('',*,*,#15570,.F.);
#22531=ORIENTED_EDGE('',*,*,#15573,.F.);
#22532=ORIENTED_EDGE('',*,*,#15575,.F.);
#22533=ORIENTED_EDGE('',*,*,#15496,.F.);
#22534=ORIENTED_EDGE('',*,*,#15578,.T.);
#22535=ORIENTED_EDGE('',*,*,#15663,.F.);
#22536=ORIENTED_EDGE('',*,*,#15576,.T.);
#22537=ORIENTED_EDGE('',*,*,#15494,.F.);
#22538=ORIENTED_EDGE('',*,*,#15574,.T.);
#22539=ORIENTED_EDGE('',*,*,#15571,.T.);
#22540=ORIENTED_EDGE('',*,*,#15568,.T.);
#22541=ORIENTED_EDGE('',*,*,#15565,.F.);
#22542=ORIENTED_EDGE('',*,*,#15562,.T.);
#22543=ORIENTED_EDGE('',*,*,#15559,.T.);
#22544=ORIENTED_EDGE('',*,*,#15556,.T.);
#22545=ORIENTED_EDGE('',*,*,#15553,.T.);
#22546=ORIENTED_EDGE('',*,*,#15550,.T.);
#22547=ORIENTED_EDGE('',*,*,#15547,.T.);
#22548=ORIENTED_EDGE('',*,*,#15544,.T.);
#22549=ORIENTED_EDGE('',*,*,#15541,.T.);
#22550=ORIENTED_EDGE('',*,*,#15538,.T.);
#22551=ORIENTED_EDGE('',*,*,#15535,.F.);
#22552=ORIENTED_EDGE('',*,*,#15532,.T.);
#22553=ORIENTED_EDGE('',*,*,#15529,.T.);
#22554=ORIENTED_EDGE('',*,*,#15526,.T.);
#22555=ORIENTED_EDGE('',*,*,#15523,.T.);
#22556=ORIENTED_EDGE('',*,*,#15520,.T.);
#22557=ORIENTED_EDGE('',*,*,#15373,.T.);
#22558=ORIENTED_EDGE('',*,*,#15380,.T.);
#22559=ORIENTED_EDGE('',*,*,#15385,.F.);
#22560=ORIENTED_EDGE('',*,*,#15390,.T.);
#22561=ORIENTED_EDGE('',*,*,#15395,.F.);
#22562=ORIENTED_EDGE('',*,*,#15400,.T.);
#22563=ORIENTED_EDGE('',*,*,#15405,.F.);
#22564=ORIENTED_EDGE('',*,*,#15410,.T.);
#22565=ORIENTED_EDGE('',*,*,#15415,.F.);
#22566=ORIENTED_EDGE('',*,*,#15420,.T.);
#22567=ORIENTED_EDGE('',*,*,#15425,.F.);
#22568=ORIENTED_EDGE('',*,*,#15430,.T.);
#22569=ORIENTED_EDGE('',*,*,#15509,.T.);
#22570=ORIENTED_EDGE('',*,*,#15504,.T.);
#22571=ORIENTED_EDGE('',*,*,#15501,.T.);
#22572=ORIENTED_EDGE('',*,*,#15498,.T.);
#22573=ORIENTED_EDGE('',*,*,#15190,.F.);
#22574=ORIENTED_EDGE('',*,*,#15579,.F.);
#22575=ORIENTED_EDGE('',*,*,#15582,.F.);
#22576=ORIENTED_EDGE('',*,*,#15586,.F.);
#22577=ORIENTED_EDGE('',*,*,#15589,.F.);
#22578=ORIENTED_EDGE('',*,*,#15591,.T.);
#22579=ORIENTED_EDGE('',*,*,#15593,.F.);
#22580=ORIENTED_EDGE('',*,*,#15595,.T.);
#22581=ORIENTED_EDGE('',*,*,#15597,.F.);
#22582=ORIENTED_EDGE('',*,*,#15599,.T.);
#22583=ORIENTED_EDGE('',*,*,#15601,.F.);
#22584=ORIENTED_EDGE('',*,*,#15603,.T.);
#22585=ORIENTED_EDGE('',*,*,#15605,.F.);
#22586=ORIENTED_EDGE('',*,*,#15607,.T.);
#22587=ORIENTED_EDGE('',*,*,#15608,.F.);
#22588=ORIENTED_EDGE('',*,*,#15439,.F.);
#22589=ORIENTED_EDGE('',*,*,#15609,.F.);
#22590=ORIENTED_EDGE('',*,*,#15612,.F.);
#22591=ORIENTED_EDGE('',*,*,#15615,.F.);
#22592=ORIENTED_EDGE('',*,*,#15618,.F.);
#22593=ORIENTED_EDGE('',*,*,#15621,.F.);
#22594=ORIENTED_EDGE('',*,*,#15624,.T.);
#22595=ORIENTED_EDGE('',*,*,#15627,.F.);
#22596=ORIENTED_EDGE('',*,*,#15630,.F.);
#22597=ORIENTED_EDGE('',*,*,#15633,.F.);
#22598=ORIENTED_EDGE('',*,*,#15636,.F.);
#22599=ORIENTED_EDGE('',*,*,#15639,.F.);
#22600=ORIENTED_EDGE('',*,*,#15642,.F.);
#22601=ORIENTED_EDGE('',*,*,#15645,.F.);
#22602=ORIENTED_EDGE('',*,*,#15648,.F.);
#22603=ORIENTED_EDGE('',*,*,#15651,.F.);
#22604=ORIENTED_EDGE('',*,*,#15654,.T.);
#22605=ORIENTED_EDGE('',*,*,#15657,.F.);
#22606=ORIENTED_EDGE('',*,*,#15660,.F.);
#22607=ORIENTED_EDGE('',*,*,#15665,.T.);
#22608=ORIENTED_EDGE('',*,*,#15666,.T.);
#22609=ORIENTED_EDGE('',*,*,#15667,.T.);
#22610=ORIENTED_EDGE('',*,*,#15668,.T.);
#22611=ORIENTED_EDGE('',*,*,#15669,.T.);
#22612=ORIENTED_EDGE('',*,*,#15670,.T.);
#22613=ORIENTED_EDGE('',*,*,#15671,.T.);
#22614=ORIENTED_EDGE('',*,*,#15672,.T.);
#22615=ORIENTED_EDGE('',*,*,#15673,.T.);
#22616=ORIENTED_EDGE('',*,*,#15674,.T.);
#22617=ORIENTED_EDGE('',*,*,#15675,.T.);
#22618=ORIENTED_EDGE('',*,*,#15676,.F.);
#22619=ORIENTED_EDGE('',*,*,#15677,.F.);
#22620=ORIENTED_EDGE('',*,*,#15678,.F.);
#22621=ORIENTED_EDGE('',*,*,#15679,.F.);
#22622=ORIENTED_EDGE('',*,*,#15680,.F.);
#22623=ORIENTED_EDGE('',*,*,#15681,.F.);
#22624=ORIENTED_EDGE('',*,*,#15682,.F.);
#22625=ORIENTED_EDGE('',*,*,#15676,.T.);
#22626=ORIENTED_EDGE('',*,*,#15683,.T.);
#22627=ORIENTED_EDGE('',*,*,#15684,.T.);
#22628=ORIENTED_EDGE('',*,*,#15685,.T.);
#22629=ORIENTED_EDGE('',*,*,#15686,.F.);
#22630=ORIENTED_EDGE('',*,*,#15687,.F.);
#22631=ORIENTED_EDGE('',*,*,#15688,.T.);
#22632=ORIENTED_EDGE('',*,*,#15689,.F.);
#22633=ORIENTED_EDGE('',*,*,#15690,.F.);
#22634=ORIENTED_EDGE('',*,*,#15691,.F.);
#22635=ORIENTED_EDGE('',*,*,#15692,.F.);
#22636=ORIENTED_EDGE('',*,*,#15693,.T.);
#22637=ORIENTED_EDGE('',*,*,#15691,.T.);
#22638=ORIENTED_EDGE('',*,*,#15694,.T.);
#22639=ORIENTED_EDGE('',*,*,#15694,.F.);
#22640=ORIENTED_EDGE('',*,*,#15690,.T.);
#22641=ORIENTED_EDGE('',*,*,#15695,.F.);
#22642=ORIENTED_EDGE('',*,*,#15696,.T.);
#22643=ORIENTED_EDGE('',*,*,#15692,.T.);
#22644=ORIENTED_EDGE('',*,*,#15696,.F.);
#22645=ORIENTED_EDGE('',*,*,#15697,.F.);
#22646=ORIENTED_EDGE('',*,*,#15698,.F.);
#22647=ORIENTED_EDGE('',*,*,#15699,.F.);
#22648=ORIENTED_EDGE('',*,*,#15700,.F.);
#22649=ORIENTED_EDGE('',*,*,#15701,.F.);
#22650=ORIENTED_EDGE('',*,*,#15702,.F.);
#22651=ORIENTED_EDGE('',*,*,#15703,.F.);
#22652=ORIENTED_EDGE('',*,*,#15674,.F.);
#22653=ORIENTED_EDGE('',*,*,#15704,.T.);
#22654=ORIENTED_EDGE('',*,*,#15705,.F.);
#22655=ORIENTED_EDGE('',*,*,#15706,.F.);
#22656=ORIENTED_EDGE('',*,*,#15707,.F.);
#22657=ORIENTED_EDGE('',*,*,#15708,.F.);
#22658=ORIENTED_EDGE('',*,*,#15709,.F.);
#22659=ORIENTED_EDGE('',*,*,#15710,.F.);
#22660=ORIENTED_EDGE('',*,*,#15711,.F.);
#22661=ORIENTED_EDGE('',*,*,#15712,.F.);
#22662=ORIENTED_EDGE('',*,*,#15713,.F.);
#22663=ORIENTED_EDGE('',*,*,#15714,.F.);
#22664=ORIENTED_EDGE('',*,*,#15715,.F.);
#22665=ORIENTED_EDGE('',*,*,#15704,.F.);
#22666=ORIENTED_EDGE('',*,*,#15673,.F.);
#22667=ORIENTED_EDGE('',*,*,#15682,.T.);
#22668=ORIENTED_EDGE('',*,*,#15716,.F.);
#22669=ORIENTED_EDGE('',*,*,#15697,.T.);
#22670=ORIENTED_EDGE('',*,*,#15695,.T.);
#22671=ORIENTED_EDGE('',*,*,#15689,.T.);
#22672=ORIENTED_EDGE('',*,*,#15717,.T.);
#22673=ORIENTED_EDGE('',*,*,#15700,.T.);
#22674=ORIENTED_EDGE('',*,*,#15718,.T.);
#22675=ORIENTED_EDGE('',*,*,#15686,.T.);
#22676=ORIENTED_EDGE('',*,*,#15719,.F.);
#22677=ORIENTED_EDGE('',*,*,#15720,.F.);
#22678=ORIENTED_EDGE('',*,*,#15721,.F.);
#22679=ORIENTED_EDGE('',*,*,#15722,.F.);
#22680=ORIENTED_EDGE('',*,*,#15723,.F.);
#22681=ORIENTED_EDGE('',*,*,#15718,.F.);
#22682=ORIENTED_EDGE('',*,*,#15699,.T.);
#22683=ORIENTED_EDGE('',*,*,#15724,.F.);
#22684=ORIENTED_EDGE('',*,*,#15687,.T.);
#22685=ORIENTED_EDGE('',*,*,#15701,.T.);
#22686=ORIENTED_EDGE('',*,*,#15719,.T.);
#22687=ORIENTED_EDGE('',*,*,#15685,.F.);
#22688=ORIENTED_EDGE('',*,*,#15725,.T.);
#22689=ORIENTED_EDGE('',*,*,#15675,.F.);
#22690=ORIENTED_EDGE('',*,*,#15703,.T.);
#22691=ORIENTED_EDGE('',*,*,#15726,.F.);
#22692=ORIENTED_EDGE('',*,*,#15683,.F.);
#22693=ORIENTED_EDGE('',*,*,#15693,.F.);
#22694=ORIENTED_EDGE('',*,*,#15715,.T.);
#22695=ORIENTED_EDGE('',*,*,#15727,.T.);
#22696=ORIENTED_EDGE('',*,*,#15669,.F.);
#22697=ORIENTED_EDGE('',*,*,#15728,.T.);
#22698=ORIENTED_EDGE('',*,*,#15677,.T.);
#22699=ORIENTED_EDGE('',*,*,#15716,.T.);
#22700=ORIENTED_EDGE('',*,*,#15681,.T.);
#22701=ORIENTED_EDGE('',*,*,#15729,.T.);
#22702=ORIENTED_EDGE('',*,*,#15671,.F.);
#22703=ORIENTED_EDGE('',*,*,#15667,.F.);
#22704=ORIENTED_EDGE('',*,*,#15730,.T.);
#22705=ORIENTED_EDGE('',*,*,#15705,.T.);
#22706=ORIENTED_EDGE('',*,*,#15720,.T.);
#22707=ORIENTED_EDGE('',*,*,#15731,.T.);
#22708=ORIENTED_EDGE('',*,*,#15732,.F.);
#22709=ORIENTED_EDGE('',*,*,#15733,.F.);
#22710=ORIENTED_EDGE('',*,*,#15721,.T.);
#22711=ORIENTED_EDGE('',*,*,#15733,.T.);
#22712=ORIENTED_EDGE('',*,*,#15734,.F.);
#22713=ORIENTED_EDGE('',*,*,#15735,.F.);
#22714=ORIENTED_EDGE('',*,*,#15722,.T.);
#22715=ORIENTED_EDGE('',*,*,#15735,.T.);
#22716=ORIENTED_EDGE('',*,*,#15736,.F.);
#22717=ORIENTED_EDGE('',*,*,#15737,.F.);
#22718=ORIENTED_EDGE('',*,*,#15723,.T.);
#22719=ORIENTED_EDGE('',*,*,#15737,.T.);
#22720=ORIENTED_EDGE('',*,*,#15738,.F.);
#22721=ORIENTED_EDGE('',*,*,#15731,.F.);
#22722=ORIENTED_EDGE('',*,*,#15738,.T.);
#22723=ORIENTED_EDGE('',*,*,#15736,.T.);
#22724=ORIENTED_EDGE('',*,*,#15734,.T.);
#22725=ORIENTED_EDGE('',*,*,#15732,.T.);
#22726=ORIENTED_EDGE('',*,*,#15739,.F.);
#22727=ORIENTED_EDGE('',*,*,#15740,.F.);
#22728=ORIENTED_EDGE('',*,*,#15741,.F.);
#22729=ORIENTED_EDGE('',*,*,#15742,.T.);
#22730=ORIENTED_EDGE('',*,*,#15743,.F.);
#22731=ORIENTED_EDGE('',*,*,#15744,.F.);
#22732=ORIENTED_EDGE('',*,*,#15745,.F.);
#22733=ORIENTED_EDGE('',*,*,#15746,.T.);
#22734=ORIENTED_EDGE('',*,*,#15747,.T.);
#22735=ORIENTED_EDGE('',*,*,#15748,.F.);
#22736=ORIENTED_EDGE('',*,*,#15742,.F.);
#22737=ORIENTED_EDGE('',*,*,#15749,.T.);
#22738=ORIENTED_EDGE('',*,*,#15711,.T.);
#22739=ORIENTED_EDGE('',*,*,#15750,.F.);
#22740=ORIENTED_EDGE('',*,*,#15741,.T.);
#22741=ORIENTED_EDGE('',*,*,#15751,.T.);
#22742=ORIENTED_EDGE('',*,*,#15712,.T.);
#22743=ORIENTED_EDGE('',*,*,#15749,.F.);
#22744=ORIENTED_EDGE('',*,*,#15740,.T.);
#22745=ORIENTED_EDGE('',*,*,#15752,.T.);
#22746=ORIENTED_EDGE('',*,*,#15713,.T.);
#22747=ORIENTED_EDGE('',*,*,#15751,.F.);
#22748=ORIENTED_EDGE('',*,*,#15688,.F.);
#22749=ORIENTED_EDGE('',*,*,#15724,.T.);
#22750=ORIENTED_EDGE('',*,*,#15698,.T.);
#22751=ORIENTED_EDGE('',*,*,#15717,.F.);
#22752=ORIENTED_EDGE('',*,*,#15684,.F.);
#22753=ORIENTED_EDGE('',*,*,#15726,.T.);
#22754=ORIENTED_EDGE('',*,*,#15702,.T.);
#22755=ORIENTED_EDGE('',*,*,#15725,.F.);
#22756=ORIENTED_EDGE('',*,*,#15748,.T.);
#22757=ORIENTED_EDGE('',*,*,#15753,.T.);
#22758=ORIENTED_EDGE('',*,*,#15707,.T.);
#22759=ORIENTED_EDGE('',*,*,#15754,.F.);
#22760=ORIENTED_EDGE('',*,*,#15747,.F.);
#22761=ORIENTED_EDGE('',*,*,#15755,.T.);
#22762=ORIENTED_EDGE('',*,*,#15708,.T.);
#22763=ORIENTED_EDGE('',*,*,#15753,.F.);
#22764=ORIENTED_EDGE('',*,*,#15746,.F.);
#22765=ORIENTED_EDGE('',*,*,#15756,.T.);
#22766=ORIENTED_EDGE('',*,*,#15709,.T.);
#22767=ORIENTED_EDGE('',*,*,#15755,.F.);
#22768=ORIENTED_EDGE('',*,*,#15757,.F.);
#22769=ORIENTED_EDGE('',*,*,#15758,.F.);
#22770=ORIENTED_EDGE('',*,*,#15759,.F.);
#22771=ORIENTED_EDGE('',*,*,#15760,.F.);
#22772=ORIENTED_EDGE('',*,*,#15761,.F.);
#22773=ORIENTED_EDGE('',*,*,#15762,.F.);
#22774=ORIENTED_EDGE('',*,*,#15763,.F.);
#22775=ORIENTED_EDGE('',*,*,#15764,.F.);
#22776=ORIENTED_EDGE('',*,*,#15760,.T.);
#22777=ORIENTED_EDGE('',*,*,#15765,.T.);
#22778=ORIENTED_EDGE('',*,*,#15766,.F.);
#22779=ORIENTED_EDGE('',*,*,#15767,.T.);
#22780=ORIENTED_EDGE('',*,*,#15678,.T.);
#22781=ORIENTED_EDGE('',*,*,#15728,.F.);
#22782=ORIENTED_EDGE('',*,*,#15668,.F.);
#22783=ORIENTED_EDGE('',*,*,#15768,.F.);
#22784=ORIENTED_EDGE('',*,*,#15769,.F.);
#22785=ORIENTED_EDGE('',*,*,#15770,.T.);
#22786=ORIENTED_EDGE('',*,*,#15771,.F.);
#22787=ORIENTED_EDGE('',*,*,#15772,.F.);
#22788=ORIENTED_EDGE('',*,*,#15773,.T.);
#22789=ORIENTED_EDGE('',*,*,#15774,.T.);
#22790=ORIENTED_EDGE('',*,*,#15775,.T.);
#22791=ORIENTED_EDGE('',*,*,#15776,.T.);
#22792=ORIENTED_EDGE('',*,*,#15777,.F.);
#22793=ORIENTED_EDGE('',*,*,#15778,.T.);
#22794=ORIENTED_EDGE('',*,*,#15779,.T.);
#22795=ORIENTED_EDGE('',*,*,#15780,.F.);
#22796=ORIENTED_EDGE('',*,*,#15781,.F.);
#22797=ORIENTED_EDGE('',*,*,#15782,.F.);
#22798=ORIENTED_EDGE('',*,*,#15770,.F.);
#22799=ORIENTED_EDGE('',*,*,#15783,.T.);
#22800=ORIENTED_EDGE('',*,*,#15784,.T.);
#22801=ORIENTED_EDGE('',*,*,#15785,.T.);
#22802=ORIENTED_EDGE('',*,*,#15786,.T.);
#22803=ORIENTED_EDGE('',*,*,#15766,.T.);
#22804=ORIENTED_EDGE('',*,*,#15787,.T.);
#22805=ORIENTED_EDGE('',*,*,#15764,.T.);
#22806=ORIENTED_EDGE('',*,*,#15757,.T.);
#22807=ORIENTED_EDGE('',*,*,#15788,.T.);
#22808=ORIENTED_EDGE('',*,*,#15665,.F.);
#22809=ORIENTED_EDGE('',*,*,#15672,.F.);
#22810=ORIENTED_EDGE('',*,*,#15729,.F.);
#22811=ORIENTED_EDGE('',*,*,#15680,.T.);
#22812=ORIENTED_EDGE('',*,*,#15789,.F.);
#22813=ORIENTED_EDGE('',*,*,#15785,.F.);
#22814=ORIENTED_EDGE('',*,*,#15790,.T.);
#22815=ORIENTED_EDGE('',*,*,#15791,.F.);
#22816=ORIENTED_EDGE('',*,*,#15774,.F.);
#22817=ORIENTED_EDGE('',*,*,#15792,.F.);
#22818=ORIENTED_EDGE('',*,*,#15791,.T.);
#22819=ORIENTED_EDGE('',*,*,#15793,.F.);
#22820=ORIENTED_EDGE('',*,*,#15794,.T.);
#22821=ORIENTED_EDGE('',*,*,#15775,.F.);
#22822=ORIENTED_EDGE('',*,*,#15790,.F.);
#22823=ORIENTED_EDGE('',*,*,#15795,.T.);
#22824=ORIENTED_EDGE('',*,*,#15796,.T.);
#22825=ORIENTED_EDGE('',*,*,#15797,.T.);
#22826=ORIENTED_EDGE('',*,*,#15798,.T.);
#22827=ORIENTED_EDGE('',*,*,#15799,.T.);
#22828=ORIENTED_EDGE('',*,*,#15800,.T.);
#22829=ORIENTED_EDGE('',*,*,#15801,.T.);
#22830=ORIENTED_EDGE('',*,*,#15802,.T.);
#22831=ORIENTED_EDGE('',*,*,#15803,.T.);
#22832=ORIENTED_EDGE('',*,*,#15804,.T.);
#22833=ORIENTED_EDGE('',*,*,#15805,.T.);
#22834=ORIENTED_EDGE('',*,*,#15806,.F.);
#22835=ORIENTED_EDGE('',*,*,#15772,.T.);
#22836=ORIENTED_EDGE('',*,*,#15807,.T.);
#22837=ORIENTED_EDGE('',*,*,#15808,.T.);
#22838=ORIENTED_EDGE('',*,*,#15809,.T.);
#22839=ORIENTED_EDGE('',*,*,#15810,.T.);
#22840=ORIENTED_EDGE('',*,*,#15811,.T.);
#22841=ORIENTED_EDGE('',*,*,#15812,.T.);
#22842=ORIENTED_EDGE('',*,*,#15813,.T.);
#22843=ORIENTED_EDGE('',*,*,#15793,.T.);
#22844=ORIENTED_EDGE('',*,*,#15761,.T.);
#22845=ORIENTED_EDGE('',*,*,#15768,.T.);
#22846=ORIENTED_EDGE('',*,*,#15670,.F.);
#22847=ORIENTED_EDGE('',*,*,#15727,.F.);
#22848=ORIENTED_EDGE('',*,*,#15714,.T.);
#22849=ORIENTED_EDGE('',*,*,#15752,.F.);
#22850=ORIENTED_EDGE('',*,*,#15814,.F.);
#22851=ORIENTED_EDGE('',*,*,#15815,.T.);
#22852=ORIENTED_EDGE('',*,*,#15796,.F.);
#22853=ORIENTED_EDGE('',*,*,#15816,.T.);
#22854=ORIENTED_EDGE('',*,*,#15806,.T.);
#22855=ORIENTED_EDGE('',*,*,#15817,.T.);
#22856=ORIENTED_EDGE('',*,*,#15783,.F.);
#22857=ORIENTED_EDGE('',*,*,#15769,.T.);
#22858=ORIENTED_EDGE('',*,*,#15813,.F.);
#22859=ORIENTED_EDGE('',*,*,#15818,.F.);
#22860=ORIENTED_EDGE('',*,*,#15776,.F.);
#22861=ORIENTED_EDGE('',*,*,#15794,.F.);
#22862=ORIENTED_EDGE('',*,*,#15810,.F.);
#22863=ORIENTED_EDGE('',*,*,#15819,.T.);
#22864=ORIENTED_EDGE('',*,*,#15779,.F.);
#22865=ORIENTED_EDGE('',*,*,#15820,.F.);
#22866=ORIENTED_EDGE('',*,*,#15821,.T.);
#22867=ORIENTED_EDGE('',*,*,#15822,.T.);
#22868=ORIENTED_EDGE('',*,*,#15823,.T.);
#22869=ORIENTED_EDGE('',*,*,#15824,.T.);
#22870=ORIENTED_EDGE('',*,*,#15820,.T.);
#22871=ORIENTED_EDGE('',*,*,#15778,.F.);
#22872=ORIENTED_EDGE('',*,*,#15825,.T.);
#22873=ORIENTED_EDGE('',*,*,#15811,.F.);
#22874=ORIENTED_EDGE('',*,*,#15809,.F.);
#22875=ORIENTED_EDGE('',*,*,#15826,.F.);
#22876=ORIENTED_EDGE('',*,*,#15780,.T.);
#22877=ORIENTED_EDGE('',*,*,#15819,.F.);
#22878=ORIENTED_EDGE('',*,*,#15771,.T.);
#22879=ORIENTED_EDGE('',*,*,#15782,.T.);
#22880=ORIENTED_EDGE('',*,*,#15827,.T.);
#22881=ORIENTED_EDGE('',*,*,#15807,.F.);
#22882=ORIENTED_EDGE('',*,*,#15792,.T.);
#22883=ORIENTED_EDGE('',*,*,#15773,.F.);
#22884=ORIENTED_EDGE('',*,*,#15765,.F.);
#22885=ORIENTED_EDGE('',*,*,#15762,.T.);
#22886=ORIENTED_EDGE('',*,*,#15816,.F.);
#22887=ORIENTED_EDGE('',*,*,#15795,.F.);
#22888=ORIENTED_EDGE('',*,*,#15817,.F.);
#22889=ORIENTED_EDGE('',*,*,#15805,.F.);
#22890=ORIENTED_EDGE('',*,*,#15828,.F.);
#22891=ORIENTED_EDGE('',*,*,#15758,.T.);
#22892=ORIENTED_EDGE('',*,*,#15763,.T.);
#22893=ORIENTED_EDGE('',*,*,#15787,.F.);
#22894=ORIENTED_EDGE('',*,*,#15784,.F.);
#22895=ORIENTED_EDGE('',*,*,#15821,.F.);
#22896=ORIENTED_EDGE('',*,*,#15829,.T.);
#22897=ORIENTED_EDGE('',*,*,#15830,.T.);
#22898=ORIENTED_EDGE('',*,*,#15831,.F.);
#22899=ORIENTED_EDGE('',*,*,#15824,.F.);
#22900=ORIENTED_EDGE('',*,*,#15832,.T.);
#22901=ORIENTED_EDGE('',*,*,#15833,.T.);
#22902=ORIENTED_EDGE('',*,*,#15829,.F.);
#22903=ORIENTED_EDGE('',*,*,#15823,.F.);
#22904=ORIENTED_EDGE('',*,*,#15834,.T.);
#22905=ORIENTED_EDGE('',*,*,#15835,.T.);
#22906=ORIENTED_EDGE('',*,*,#15832,.F.);
#22907=ORIENTED_EDGE('',*,*,#15822,.F.);
#22908=ORIENTED_EDGE('',*,*,#15831,.T.);
#22909=ORIENTED_EDGE('',*,*,#15836,.T.);
#22910=ORIENTED_EDGE('',*,*,#15834,.F.);
#22911=ORIENTED_EDGE('',*,*,#15836,.F.);
#22912=ORIENTED_EDGE('',*,*,#15830,.F.);
#22913=ORIENTED_EDGE('',*,*,#15833,.F.);
#22914=ORIENTED_EDGE('',*,*,#15835,.F.);
#22915=ORIENTED_EDGE('',*,*,#15786,.F.);
#22916=ORIENTED_EDGE('',*,*,#15789,.T.);
#22917=ORIENTED_EDGE('',*,*,#15679,.T.);
#22918=ORIENTED_EDGE('',*,*,#15767,.F.);
#22919=ORIENTED_EDGE('',*,*,#15837,.F.);
#22920=ORIENTED_EDGE('',*,*,#15814,.T.);
#22921=ORIENTED_EDGE('',*,*,#15739,.T.);
#22922=ORIENTED_EDGE('',*,*,#15838,.T.);
#22923=ORIENTED_EDGE('',*,*,#15839,.F.);
#22924=ORIENTED_EDGE('',*,*,#15840,.F.);
#22925=ORIENTED_EDGE('',*,*,#15744,.T.);
#22926=ORIENTED_EDGE('',*,*,#15841,.F.);
#22927=ORIENTED_EDGE('',*,*,#15837,.T.);
#22928=ORIENTED_EDGE('',*,*,#15842,.T.);
#22929=ORIENTED_EDGE('',*,*,#15843,.F.);
#22930=ORIENTED_EDGE('',*,*,#15844,.T.);
#22931=ORIENTED_EDGE('',*,*,#15845,.T.);
#22932=ORIENTED_EDGE('',*,*,#15839,.T.);
#22933=ORIENTED_EDGE('',*,*,#15846,.T.);
#22934=ORIENTED_EDGE('',*,*,#15847,.F.);
#22935=ORIENTED_EDGE('',*,*,#15848,.F.);
#22936=ORIENTED_EDGE('',*,*,#15849,.T.);
#22937=ORIENTED_EDGE('',*,*,#15828,.T.);
#22938=ORIENTED_EDGE('',*,*,#15804,.F.);
#22939=ORIENTED_EDGE('',*,*,#15850,.F.);
#22940=ORIENTED_EDGE('',*,*,#15841,.T.);
#22941=ORIENTED_EDGE('',*,*,#15754,.T.);
#22942=ORIENTED_EDGE('',*,*,#15706,.T.);
#22943=ORIENTED_EDGE('',*,*,#15730,.F.);
#22944=ORIENTED_EDGE('',*,*,#15666,.F.);
#22945=ORIENTED_EDGE('',*,*,#15788,.F.);
#22946=ORIENTED_EDGE('',*,*,#15759,.T.);
#22947=ORIENTED_EDGE('',*,*,#15851,.T.);
#22948=ORIENTED_EDGE('',*,*,#15800,.F.);
#22949=ORIENTED_EDGE('',*,*,#15852,.F.);
#22950=ORIENTED_EDGE('',*,*,#15842,.F.);
#22951=ORIENTED_EDGE('',*,*,#15838,.F.);
#22952=ORIENTED_EDGE('',*,*,#15743,.T.);
#22953=ORIENTED_EDGE('',*,*,#15750,.T.);
#22954=ORIENTED_EDGE('',*,*,#15710,.T.);
#22955=ORIENTED_EDGE('',*,*,#15756,.F.);
#22956=ORIENTED_EDGE('',*,*,#15745,.T.);
#22957=ORIENTED_EDGE('',*,*,#15840,.T.);
#22958=ORIENTED_EDGE('',*,*,#15849,.F.);
#22959=ORIENTED_EDGE('',*,*,#15843,.T.);
#22960=ORIENTED_EDGE('',*,*,#15852,.T.);
#22961=ORIENTED_EDGE('',*,*,#15799,.F.);
#22962=ORIENTED_EDGE('',*,*,#15853,.F.);
#22963=ORIENTED_EDGE('',*,*,#15844,.F.);
#22964=ORIENTED_EDGE('',*,*,#15853,.T.);
#22965=ORIENTED_EDGE('',*,*,#15798,.F.);
#22966=ORIENTED_EDGE('',*,*,#15854,.F.);
#22967=ORIENTED_EDGE('',*,*,#15845,.F.);
#22968=ORIENTED_EDGE('',*,*,#15854,.T.);
#22969=ORIENTED_EDGE('',*,*,#15797,.F.);
#22970=ORIENTED_EDGE('',*,*,#15815,.F.);
#22971=ORIENTED_EDGE('',*,*,#15777,.T.);
#22972=ORIENTED_EDGE('',*,*,#15818,.T.);
#22973=ORIENTED_EDGE('',*,*,#15812,.F.);
#22974=ORIENTED_EDGE('',*,*,#15825,.F.);
#22975=ORIENTED_EDGE('',*,*,#15781,.T.);
#22976=ORIENTED_EDGE('',*,*,#15826,.T.);
#22977=ORIENTED_EDGE('',*,*,#15808,.F.);
#22978=ORIENTED_EDGE('',*,*,#15827,.F.);
#22979=ORIENTED_EDGE('',*,*,#15846,.F.);
#22980=ORIENTED_EDGE('',*,*,#15850,.T.);
#22981=ORIENTED_EDGE('',*,*,#15803,.F.);
#22982=ORIENTED_EDGE('',*,*,#15855,.F.);
#22983=ORIENTED_EDGE('',*,*,#15847,.T.);
#22984=ORIENTED_EDGE('',*,*,#15855,.T.);
#22985=ORIENTED_EDGE('',*,*,#15802,.F.);
#22986=ORIENTED_EDGE('',*,*,#15856,.F.);
#22987=ORIENTED_EDGE('',*,*,#15848,.T.);
#22988=ORIENTED_EDGE('',*,*,#15856,.T.);
#22989=ORIENTED_EDGE('',*,*,#15801,.F.);
#22990=ORIENTED_EDGE('',*,*,#15851,.F.);
#22991=ORIENTED_EDGE('',*,*,#15857,.T.);
#22992=ORIENTED_EDGE('',*,*,#15858,.T.);
#22993=ORIENTED_EDGE('',*,*,#15859,.F.);
#22994=ORIENTED_EDGE('',*,*,#15858,.F.);
#22995=ORIENTED_EDGE('',*,*,#15860,.T.);
#22996=ORIENTED_EDGE('',*,*,#15861,.T.);
#22997=ORIENTED_EDGE('',*,*,#15862,.F.);
#22998=ORIENTED_EDGE('',*,*,#15863,.F.);
#22999=ORIENTED_EDGE('',*,*,#15864,.F.);
#23000=ORIENTED_EDGE('',*,*,#15863,.T.);
#23001=ORIENTED_EDGE('',*,*,#15865,.F.);
#23002=ORIENTED_EDGE('',*,*,#15866,.F.);
#23003=ORIENTED_EDGE('',*,*,#15867,.T.);
#23004=ORIENTED_EDGE('',*,*,#15866,.T.);
#23005=ORIENTED_EDGE('',*,*,#15868,.F.);
#23006=ORIENTED_EDGE('',*,*,#15869,.F.);
#23007=ORIENTED_EDGE('',*,*,#15870,.T.);
#23008=ORIENTED_EDGE('',*,*,#15869,.T.);
#23009=ORIENTED_EDGE('',*,*,#15871,.F.);
#23010=ORIENTED_EDGE('',*,*,#15872,.F.);
#23011=ORIENTED_EDGE('',*,*,#15873,.F.);
#23012=ORIENTED_EDGE('',*,*,#15872,.T.);
#23013=ORIENTED_EDGE('',*,*,#15874,.F.);
#23014=ORIENTED_EDGE('',*,*,#15875,.F.);
#23015=ORIENTED_EDGE('',*,*,#15876,.T.);
#23016=ORIENTED_EDGE('',*,*,#15875,.T.);
#23017=ORIENTED_EDGE('',*,*,#15877,.F.);
#23018=ORIENTED_EDGE('',*,*,#15878,.F.);
#23019=ORIENTED_EDGE('',*,*,#15879,.T.);
#23020=ORIENTED_EDGE('',*,*,#15878,.T.);
#23021=ORIENTED_EDGE('',*,*,#15880,.F.);
#23022=ORIENTED_EDGE('',*,*,#15881,.F.);
#23023=ORIENTED_EDGE('',*,*,#15882,.F.);
#23024=ORIENTED_EDGE('',*,*,#15881,.T.);
#23025=ORIENTED_EDGE('',*,*,#15883,.F.);
#23026=ORIENTED_EDGE('',*,*,#15884,.F.);
#23027=ORIENTED_EDGE('',*,*,#15885,.F.);
#23028=ORIENTED_EDGE('',*,*,#15884,.T.);
#23029=ORIENTED_EDGE('',*,*,#15886,.F.);
#23030=ORIENTED_EDGE('',*,*,#15887,.F.);
#23031=ORIENTED_EDGE('',*,*,#15888,.T.);
#23032=ORIENTED_EDGE('',*,*,#15887,.T.);
#23033=ORIENTED_EDGE('',*,*,#15889,.F.);
#23034=ORIENTED_EDGE('',*,*,#15890,.F.);
#23035=ORIENTED_EDGE('',*,*,#15891,.F.);
#23036=ORIENTED_EDGE('',*,*,#15890,.T.);
#23037=ORIENTED_EDGE('',*,*,#15892,.F.);
#23038=ORIENTED_EDGE('',*,*,#15893,.F.);
#23039=ORIENTED_EDGE('',*,*,#15894,.T.);
#23040=ORIENTED_EDGE('',*,*,#15893,.T.);
#23041=ORIENTED_EDGE('',*,*,#15895,.F.);
#23042=ORIENTED_EDGE('',*,*,#15896,.F.);
#23043=ORIENTED_EDGE('',*,*,#15897,.T.);
#23044=ORIENTED_EDGE('',*,*,#15896,.T.);
#23045=ORIENTED_EDGE('',*,*,#15898,.F.);
#23046=ORIENTED_EDGE('',*,*,#15899,.F.);
#23047=ORIENTED_EDGE('',*,*,#15900,.F.);
#23048=ORIENTED_EDGE('',*,*,#15899,.T.);
#23049=ORIENTED_EDGE('',*,*,#15901,.F.);
#23050=ORIENTED_EDGE('',*,*,#15902,.F.);
#23051=ORIENTED_EDGE('',*,*,#15903,.F.);
#23052=ORIENTED_EDGE('',*,*,#15902,.T.);
#23053=ORIENTED_EDGE('',*,*,#15904,.F.);
#23054=ORIENTED_EDGE('',*,*,#15905,.F.);
#23055=ORIENTED_EDGE('',*,*,#15906,.F.);
#23056=ORIENTED_EDGE('',*,*,#15905,.T.);
#23057=ORIENTED_EDGE('',*,*,#15907,.F.);
#23058=ORIENTED_EDGE('',*,*,#15908,.F.);
#23059=ORIENTED_EDGE('',*,*,#15909,.F.);
#23060=ORIENTED_EDGE('',*,*,#15908,.T.);
#23061=ORIENTED_EDGE('',*,*,#15910,.F.);
#23062=ORIENTED_EDGE('',*,*,#15911,.F.);
#23063=ORIENTED_EDGE('',*,*,#15912,.T.);
#23064=ORIENTED_EDGE('',*,*,#15911,.T.);
#23065=ORIENTED_EDGE('',*,*,#15913,.F.);
#23066=ORIENTED_EDGE('',*,*,#15914,.F.);
#23067=ORIENTED_EDGE('',*,*,#15915,.F.);
#23068=ORIENTED_EDGE('',*,*,#15914,.T.);
#23069=ORIENTED_EDGE('',*,*,#15916,.F.);
#23070=ORIENTED_EDGE('',*,*,#15917,.F.);
#23071=ORIENTED_EDGE('',*,*,#15918,.T.);
#23072=ORIENTED_EDGE('',*,*,#15917,.T.);
#23073=ORIENTED_EDGE('',*,*,#15919,.F.);
#23074=ORIENTED_EDGE('',*,*,#15920,.F.);
#23075=ORIENTED_EDGE('',*,*,#15921,.F.);
#23076=ORIENTED_EDGE('',*,*,#15920,.T.);
#23077=ORIENTED_EDGE('',*,*,#15922,.F.);
#23078=ORIENTED_EDGE('',*,*,#15923,.F.);
#23079=ORIENTED_EDGE('',*,*,#15924,.F.);
#23080=ORIENTED_EDGE('',*,*,#15923,.T.);
#23081=ORIENTED_EDGE('',*,*,#15925,.F.);
#23082=ORIENTED_EDGE('',*,*,#15926,.F.);
#23083=ORIENTED_EDGE('',*,*,#15927,.F.);
#23084=ORIENTED_EDGE('',*,*,#15926,.T.);
#23085=ORIENTED_EDGE('',*,*,#15928,.F.);
#23086=ORIENTED_EDGE('',*,*,#15929,.F.);
#23087=ORIENTED_EDGE('',*,*,#15930,.F.);
#23088=ORIENTED_EDGE('',*,*,#15929,.T.);
#23089=ORIENTED_EDGE('',*,*,#15931,.F.);
#23090=ORIENTED_EDGE('',*,*,#15932,.F.);
#23091=ORIENTED_EDGE('',*,*,#15933,.F.);
#23092=ORIENTED_EDGE('',*,*,#15932,.T.);
#23093=ORIENTED_EDGE('',*,*,#15934,.F.);
#23094=ORIENTED_EDGE('',*,*,#15935,.F.);
#23095=ORIENTED_EDGE('',*,*,#15936,.F.);
#23096=ORIENTED_EDGE('',*,*,#15935,.T.);
#23097=ORIENTED_EDGE('',*,*,#15937,.F.);
#23098=ORIENTED_EDGE('',*,*,#15938,.F.);
#23099=ORIENTED_EDGE('',*,*,#15939,.T.);
#23100=ORIENTED_EDGE('',*,*,#15938,.T.);
#23101=ORIENTED_EDGE('',*,*,#15940,.F.);
#23102=ORIENTED_EDGE('',*,*,#15941,.F.);
#23103=ORIENTED_EDGE('',*,*,#15942,.F.);
#23104=ORIENTED_EDGE('',*,*,#15941,.T.);
#23105=ORIENTED_EDGE('',*,*,#15943,.F.);
#23106=ORIENTED_EDGE('',*,*,#15944,.F.);
#23107=ORIENTED_EDGE('',*,*,#15945,.T.);
#23108=ORIENTED_EDGE('',*,*,#15944,.T.);
#23109=ORIENTED_EDGE('',*,*,#15946,.F.);
#23110=ORIENTED_EDGE('',*,*,#15947,.F.);
#23111=ORIENTED_EDGE('',*,*,#15948,.F.);
#23112=ORIENTED_EDGE('',*,*,#15947,.T.);
#23113=ORIENTED_EDGE('',*,*,#15949,.F.);
#23114=ORIENTED_EDGE('',*,*,#15950,.F.);
#23115=ORIENTED_EDGE('',*,*,#15951,.T.);
#23116=ORIENTED_EDGE('',*,*,#15950,.T.);
#23117=ORIENTED_EDGE('',*,*,#15952,.F.);
#23118=ORIENTED_EDGE('',*,*,#15953,.F.);
#23119=ORIENTED_EDGE('',*,*,#15954,.T.);
#23120=ORIENTED_EDGE('',*,*,#15953,.T.);
#23121=ORIENTED_EDGE('',*,*,#15955,.F.);
#23122=ORIENTED_EDGE('',*,*,#15956,.F.);
#23123=ORIENTED_EDGE('',*,*,#15957,.T.);
#23124=ORIENTED_EDGE('',*,*,#15956,.T.);
#23125=ORIENTED_EDGE('',*,*,#15958,.F.);
#23126=ORIENTED_EDGE('',*,*,#15959,.F.);
#23127=ORIENTED_EDGE('',*,*,#15960,.T.);
#23128=ORIENTED_EDGE('',*,*,#15959,.T.);
#23129=ORIENTED_EDGE('',*,*,#15961,.F.);
#23130=ORIENTED_EDGE('',*,*,#15962,.F.);
#23131=ORIENTED_EDGE('',*,*,#15963,.T.);
#23132=ORIENTED_EDGE('',*,*,#15962,.T.);
#23133=ORIENTED_EDGE('',*,*,#15964,.F.);
#23134=ORIENTED_EDGE('',*,*,#15965,.F.);
#23135=ORIENTED_EDGE('',*,*,#15966,.T.);
#23136=ORIENTED_EDGE('',*,*,#15965,.T.);
#23137=ORIENTED_EDGE('',*,*,#15967,.F.);
#23138=ORIENTED_EDGE('',*,*,#15968,.F.);
#23139=ORIENTED_EDGE('',*,*,#15969,.T.);
#23140=ORIENTED_EDGE('',*,*,#15968,.T.);
#23141=ORIENTED_EDGE('',*,*,#15970,.F.);
#23142=ORIENTED_EDGE('',*,*,#15971,.F.);
#23143=ORIENTED_EDGE('',*,*,#15972,.F.);
#23144=ORIENTED_EDGE('',*,*,#15971,.T.);
#23145=ORIENTED_EDGE('',*,*,#15973,.F.);
#23146=ORIENTED_EDGE('',*,*,#15974,.F.);
#23147=ORIENTED_EDGE('',*,*,#15975,.T.);
#23148=ORIENTED_EDGE('',*,*,#15974,.T.);
#23149=ORIENTED_EDGE('',*,*,#15976,.F.);
#23150=ORIENTED_EDGE('',*,*,#15977,.F.);
#23151=ORIENTED_EDGE('',*,*,#15978,.T.);
#23152=ORIENTED_EDGE('',*,*,#15977,.T.);
#23153=ORIENTED_EDGE('',*,*,#15979,.F.);
#23154=ORIENTED_EDGE('',*,*,#15980,.F.);
#23155=ORIENTED_EDGE('',*,*,#15981,.F.);
#23156=ORIENTED_EDGE('',*,*,#15980,.T.);
#23157=ORIENTED_EDGE('',*,*,#15982,.F.);
#23158=ORIENTED_EDGE('',*,*,#15983,.F.);
#23159=ORIENTED_EDGE('',*,*,#15984,.T.);
#23160=ORIENTED_EDGE('',*,*,#15983,.T.);
#23161=ORIENTED_EDGE('',*,*,#15985,.F.);
#23162=ORIENTED_EDGE('',*,*,#15986,.F.);
#23163=ORIENTED_EDGE('',*,*,#15987,.F.);
#23164=ORIENTED_EDGE('',*,*,#15986,.T.);
#23165=ORIENTED_EDGE('',*,*,#15988,.F.);
#23166=ORIENTED_EDGE('',*,*,#15989,.F.);
#23167=ORIENTED_EDGE('',*,*,#15990,.T.);
#23168=ORIENTED_EDGE('',*,*,#15989,.T.);
#23169=ORIENTED_EDGE('',*,*,#15991,.F.);
#23170=ORIENTED_EDGE('',*,*,#15992,.F.);
#23171=ORIENTED_EDGE('',*,*,#15993,.T.);
#23172=ORIENTED_EDGE('',*,*,#15992,.T.);
#23173=ORIENTED_EDGE('',*,*,#15994,.F.);
#23174=ORIENTED_EDGE('',*,*,#15995,.F.);
#23175=ORIENTED_EDGE('',*,*,#15996,.T.);
#23176=ORIENTED_EDGE('',*,*,#15995,.T.);
#23177=ORIENTED_EDGE('',*,*,#15997,.F.);
#23178=ORIENTED_EDGE('',*,*,#15998,.F.);
#23179=ORIENTED_EDGE('',*,*,#15999,.T.);
#23180=ORIENTED_EDGE('',*,*,#15998,.T.);
#23181=ORIENTED_EDGE('',*,*,#16000,.F.);
#23182=ORIENTED_EDGE('',*,*,#16001,.F.);
#23183=ORIENTED_EDGE('',*,*,#16002,.T.);
#23184=ORIENTED_EDGE('',*,*,#16001,.T.);
#23185=ORIENTED_EDGE('',*,*,#16003,.F.);
#23186=ORIENTED_EDGE('',*,*,#16004,.F.);
#23187=ORIENTED_EDGE('',*,*,#16005,.T.);
#23188=ORIENTED_EDGE('',*,*,#16004,.T.);
#23189=ORIENTED_EDGE('',*,*,#16006,.F.);
#23190=ORIENTED_EDGE('',*,*,#16007,.F.);
#23191=ORIENTED_EDGE('',*,*,#16008,.F.);
#23192=ORIENTED_EDGE('',*,*,#16007,.T.);
#23193=ORIENTED_EDGE('',*,*,#16009,.F.);
#23194=ORIENTED_EDGE('',*,*,#16010,.F.);
#23195=ORIENTED_EDGE('',*,*,#16011,.F.);
#23196=ORIENTED_EDGE('',*,*,#16010,.T.);
#23197=ORIENTED_EDGE('',*,*,#16012,.F.);
#23198=ORIENTED_EDGE('',*,*,#16013,.F.);
#23199=ORIENTED_EDGE('',*,*,#16014,.F.);
#23200=ORIENTED_EDGE('',*,*,#16013,.T.);
#23201=ORIENTED_EDGE('',*,*,#16015,.F.);
#23202=ORIENTED_EDGE('',*,*,#16016,.F.);
#23203=ORIENTED_EDGE('',*,*,#16017,.T.);
#23204=ORIENTED_EDGE('',*,*,#16016,.T.);
#23205=ORIENTED_EDGE('',*,*,#16018,.F.);
#23206=ORIENTED_EDGE('',*,*,#16019,.F.);
#23207=ORIENTED_EDGE('',*,*,#16020,.F.);
#23208=ORIENTED_EDGE('',*,*,#16019,.T.);
#23209=ORIENTED_EDGE('',*,*,#16021,.F.);
#23210=ORIENTED_EDGE('',*,*,#16022,.F.);
#23211=ORIENTED_EDGE('',*,*,#16023,.F.);
#23212=ORIENTED_EDGE('',*,*,#16022,.T.);
#23213=ORIENTED_EDGE('',*,*,#16024,.F.);
#23214=ORIENTED_EDGE('',*,*,#16025,.F.);
#23215=ORIENTED_EDGE('',*,*,#16026,.T.);
#23216=ORIENTED_EDGE('',*,*,#16025,.T.);
#23217=ORIENTED_EDGE('',*,*,#16027,.F.);
#23218=ORIENTED_EDGE('',*,*,#16028,.F.);
#23219=ORIENTED_EDGE('',*,*,#16029,.F.);
#23220=ORIENTED_EDGE('',*,*,#16028,.T.);
#23221=ORIENTED_EDGE('',*,*,#16030,.F.);
#23222=ORIENTED_EDGE('',*,*,#16031,.F.);
#23223=ORIENTED_EDGE('',*,*,#16032,.T.);
#23224=ORIENTED_EDGE('',*,*,#16031,.T.);
#23225=ORIENTED_EDGE('',*,*,#16033,.F.);
#23226=ORIENTED_EDGE('',*,*,#16034,.F.);
#23227=ORIENTED_EDGE('',*,*,#16035,.T.);
#23228=ORIENTED_EDGE('',*,*,#16034,.T.);
#23229=ORIENTED_EDGE('',*,*,#16036,.F.);
#23230=ORIENTED_EDGE('',*,*,#16037,.F.);
#23231=ORIENTED_EDGE('',*,*,#16038,.F.);
#23232=ORIENTED_EDGE('',*,*,#16037,.T.);
#23233=ORIENTED_EDGE('',*,*,#16039,.F.);
#23234=ORIENTED_EDGE('',*,*,#16040,.F.);
#23235=ORIENTED_EDGE('',*,*,#16041,.F.);
#23236=ORIENTED_EDGE('',*,*,#16040,.T.);
#23237=ORIENTED_EDGE('',*,*,#16042,.F.);
#23238=ORIENTED_EDGE('',*,*,#16043,.F.);
#23239=ORIENTED_EDGE('',*,*,#16044,.F.);
#23240=ORIENTED_EDGE('',*,*,#16043,.T.);
#23241=ORIENTED_EDGE('',*,*,#16045,.F.);
#23242=ORIENTED_EDGE('',*,*,#16046,.F.);
#23243=ORIENTED_EDGE('',*,*,#16047,.F.);
#23244=ORIENTED_EDGE('',*,*,#16046,.T.);
#23245=ORIENTED_EDGE('',*,*,#16048,.F.);
#23246=ORIENTED_EDGE('',*,*,#16049,.F.);
#23247=ORIENTED_EDGE('',*,*,#16050,.T.);
#23248=ORIENTED_EDGE('',*,*,#16049,.T.);
#23249=ORIENTED_EDGE('',*,*,#16051,.F.);
#23250=ORIENTED_EDGE('',*,*,#16052,.F.);
#23251=ORIENTED_EDGE('',*,*,#16053,.F.);
#23252=ORIENTED_EDGE('',*,*,#16052,.T.);
#23253=ORIENTED_EDGE('',*,*,#16054,.F.);
#23254=ORIENTED_EDGE('',*,*,#16055,.F.);
#23255=ORIENTED_EDGE('',*,*,#16056,.T.);
#23256=ORIENTED_EDGE('',*,*,#16055,.T.);
#23257=ORIENTED_EDGE('',*,*,#16057,.F.);
#23258=ORIENTED_EDGE('',*,*,#16058,.F.);
#23259=ORIENTED_EDGE('',*,*,#16059,.F.);
#23260=ORIENTED_EDGE('',*,*,#16058,.T.);
#23261=ORIENTED_EDGE('',*,*,#16060,.F.);
#23262=ORIENTED_EDGE('',*,*,#16061,.F.);
#23263=ORIENTED_EDGE('',*,*,#16062,.F.);
#23264=ORIENTED_EDGE('',*,*,#16061,.T.);
#23265=ORIENTED_EDGE('',*,*,#16063,.F.);
#23266=ORIENTED_EDGE('',*,*,#16064,.F.);
#23267=ORIENTED_EDGE('',*,*,#16065,.F.);
#23268=ORIENTED_EDGE('',*,*,#16064,.T.);
#23269=ORIENTED_EDGE('',*,*,#16066,.F.);
#23270=ORIENTED_EDGE('',*,*,#16067,.F.);
#23271=ORIENTED_EDGE('',*,*,#16068,.F.);
#23272=ORIENTED_EDGE('',*,*,#16067,.T.);
#23273=ORIENTED_EDGE('',*,*,#16069,.F.);
#23274=ORIENTED_EDGE('',*,*,#16070,.F.);
#23275=ORIENTED_EDGE('',*,*,#16071,.F.);
#23276=ORIENTED_EDGE('',*,*,#16070,.T.);
#23277=ORIENTED_EDGE('',*,*,#16072,.F.);
#23278=ORIENTED_EDGE('',*,*,#16073,.F.);
#23279=ORIENTED_EDGE('',*,*,#16074,.F.);
#23280=ORIENTED_EDGE('',*,*,#16073,.T.);
#23281=ORIENTED_EDGE('',*,*,#16075,.F.);
#23282=ORIENTED_EDGE('',*,*,#16076,.F.);
#23283=ORIENTED_EDGE('',*,*,#16077,.F.);
#23284=ORIENTED_EDGE('',*,*,#16076,.T.);
#23285=ORIENTED_EDGE('',*,*,#16078,.F.);
#23286=ORIENTED_EDGE('',*,*,#16079,.F.);
#23287=ORIENTED_EDGE('',*,*,#16080,.F.);
#23288=ORIENTED_EDGE('',*,*,#16079,.T.);
#23289=ORIENTED_EDGE('',*,*,#16081,.F.);
#23290=ORIENTED_EDGE('',*,*,#16082,.F.);
#23291=ORIENTED_EDGE('',*,*,#16083,.T.);
#23292=ORIENTED_EDGE('',*,*,#16082,.T.);
#23293=ORIENTED_EDGE('',*,*,#16084,.F.);
#23294=ORIENTED_EDGE('',*,*,#16085,.F.);
#23295=ORIENTED_EDGE('',*,*,#16086,.F.);
#23296=ORIENTED_EDGE('',*,*,#16085,.T.);
#23297=ORIENTED_EDGE('',*,*,#16087,.F.);
#23298=ORIENTED_EDGE('',*,*,#16088,.F.);
#23299=ORIENTED_EDGE('',*,*,#16089,.T.);
#23300=ORIENTED_EDGE('',*,*,#16088,.T.);
#23301=ORIENTED_EDGE('',*,*,#16090,.F.);
#23302=ORIENTED_EDGE('',*,*,#16091,.F.);
#23303=ORIENTED_EDGE('',*,*,#16092,.T.);
#23304=ORIENTED_EDGE('',*,*,#16091,.T.);
#23305=ORIENTED_EDGE('',*,*,#16093,.F.);
#23306=ORIENTED_EDGE('',*,*,#16094,.F.);
#23307=ORIENTED_EDGE('',*,*,#16095,.T.);
#23308=ORIENTED_EDGE('',*,*,#16094,.T.);
#23309=ORIENTED_EDGE('',*,*,#16096,.F.);
#23310=ORIENTED_EDGE('',*,*,#16097,.F.);
#23311=ORIENTED_EDGE('',*,*,#16098,.T.);
#23312=ORIENTED_EDGE('',*,*,#16097,.T.);
#23313=ORIENTED_EDGE('',*,*,#16099,.F.);
#23314=ORIENTED_EDGE('',*,*,#16100,.F.);
#23315=ORIENTED_EDGE('',*,*,#16101,.T.);
#23316=ORIENTED_EDGE('',*,*,#16100,.T.);
#23317=ORIENTED_EDGE('',*,*,#16102,.F.);
#23318=ORIENTED_EDGE('',*,*,#16103,.F.);
#23319=ORIENTED_EDGE('',*,*,#16104,.T.);
#23320=ORIENTED_EDGE('',*,*,#16103,.T.);
#23321=ORIENTED_EDGE('',*,*,#16105,.F.);
#23322=ORIENTED_EDGE('',*,*,#16106,.F.);
#23323=ORIENTED_EDGE('',*,*,#16107,.T.);
#23324=ORIENTED_EDGE('',*,*,#16106,.T.);
#23325=ORIENTED_EDGE('',*,*,#16108,.F.);
#23326=ORIENTED_EDGE('',*,*,#16109,.F.);
#23327=ORIENTED_EDGE('',*,*,#16110,.F.);
#23328=ORIENTED_EDGE('',*,*,#16109,.T.);
#23329=ORIENTED_EDGE('',*,*,#16111,.F.);
#23330=ORIENTED_EDGE('',*,*,#16112,.F.);
#23331=ORIENTED_EDGE('',*,*,#16113,.T.);
#23332=ORIENTED_EDGE('',*,*,#16112,.T.);
#23333=ORIENTED_EDGE('',*,*,#16114,.F.);
#23334=ORIENTED_EDGE('',*,*,#16115,.F.);
#23335=ORIENTED_EDGE('',*,*,#16116,.T.);
#23336=ORIENTED_EDGE('',*,*,#16115,.T.);
#23337=ORIENTED_EDGE('',*,*,#16117,.F.);
#23338=ORIENTED_EDGE('',*,*,#16118,.F.);
#23339=ORIENTED_EDGE('',*,*,#16119,.F.);
#23340=ORIENTED_EDGE('',*,*,#16118,.T.);
#23341=ORIENTED_EDGE('',*,*,#16120,.F.);
#23342=ORIENTED_EDGE('',*,*,#16121,.F.);
#23343=ORIENTED_EDGE('',*,*,#16122,.T.);
#23344=ORIENTED_EDGE('',*,*,#16121,.T.);
#23345=ORIENTED_EDGE('',*,*,#16123,.F.);
#23346=ORIENTED_EDGE('',*,*,#16124,.F.);
#23347=ORIENTED_EDGE('',*,*,#16125,.F.);
#23348=ORIENTED_EDGE('',*,*,#16124,.T.);
#23349=ORIENTED_EDGE('',*,*,#16126,.F.);
#23350=ORIENTED_EDGE('',*,*,#16127,.F.);
#23351=ORIENTED_EDGE('',*,*,#16128,.T.);
#23352=ORIENTED_EDGE('',*,*,#16127,.T.);
#23353=ORIENTED_EDGE('',*,*,#16129,.F.);
#23354=ORIENTED_EDGE('',*,*,#16130,.F.);
#23355=ORIENTED_EDGE('',*,*,#16131,.T.);
#23356=ORIENTED_EDGE('',*,*,#16130,.T.);
#23357=ORIENTED_EDGE('',*,*,#16132,.F.);
#23358=ORIENTED_EDGE('',*,*,#16133,.F.);
#23359=ORIENTED_EDGE('',*,*,#16134,.T.);
#23360=ORIENTED_EDGE('',*,*,#16133,.T.);
#23361=ORIENTED_EDGE('',*,*,#16135,.F.);
#23362=ORIENTED_EDGE('',*,*,#15861,.F.);
#23363=ORIENTED_EDGE('',*,*,#16135,.T.);
#23364=ORIENTED_EDGE('',*,*,#16132,.T.);
#23365=ORIENTED_EDGE('',*,*,#16129,.T.);
#23366=ORIENTED_EDGE('',*,*,#16126,.T.);
#23367=ORIENTED_EDGE('',*,*,#16123,.T.);
#23368=ORIENTED_EDGE('',*,*,#16120,.T.);
#23369=ORIENTED_EDGE('',*,*,#16117,.T.);
#23370=ORIENTED_EDGE('',*,*,#16114,.T.);
#23371=ORIENTED_EDGE('',*,*,#16111,.T.);
#23372=ORIENTED_EDGE('',*,*,#16108,.T.);
#23373=ORIENTED_EDGE('',*,*,#16105,.T.);
#23374=ORIENTED_EDGE('',*,*,#16102,.T.);
#23375=ORIENTED_EDGE('',*,*,#16099,.T.);
#23376=ORIENTED_EDGE('',*,*,#16096,.T.);
#23377=ORIENTED_EDGE('',*,*,#16093,.T.);
#23378=ORIENTED_EDGE('',*,*,#16090,.T.);
#23379=ORIENTED_EDGE('',*,*,#16087,.T.);
#23380=ORIENTED_EDGE('',*,*,#16084,.T.);
#23381=ORIENTED_EDGE('',*,*,#16081,.T.);
#23382=ORIENTED_EDGE('',*,*,#16078,.T.);
#23383=ORIENTED_EDGE('',*,*,#16075,.T.);
#23384=ORIENTED_EDGE('',*,*,#16072,.T.);
#23385=ORIENTED_EDGE('',*,*,#16069,.T.);
#23386=ORIENTED_EDGE('',*,*,#16066,.T.);
#23387=ORIENTED_EDGE('',*,*,#16063,.T.);
#23388=ORIENTED_EDGE('',*,*,#16060,.T.);
#23389=ORIENTED_EDGE('',*,*,#16057,.T.);
#23390=ORIENTED_EDGE('',*,*,#16054,.T.);
#23391=ORIENTED_EDGE('',*,*,#16051,.T.);
#23392=ORIENTED_EDGE('',*,*,#16048,.T.);
#23393=ORIENTED_EDGE('',*,*,#16045,.T.);
#23394=ORIENTED_EDGE('',*,*,#16042,.T.);
#23395=ORIENTED_EDGE('',*,*,#16039,.T.);
#23396=ORIENTED_EDGE('',*,*,#16036,.T.);
#23397=ORIENTED_EDGE('',*,*,#16033,.T.);
#23398=ORIENTED_EDGE('',*,*,#16030,.T.);
#23399=ORIENTED_EDGE('',*,*,#16027,.T.);
#23400=ORIENTED_EDGE('',*,*,#16024,.T.);
#23401=ORIENTED_EDGE('',*,*,#16021,.T.);
#23402=ORIENTED_EDGE('',*,*,#16018,.T.);
#23403=ORIENTED_EDGE('',*,*,#16015,.T.);
#23404=ORIENTED_EDGE('',*,*,#16012,.T.);
#23405=ORIENTED_EDGE('',*,*,#16009,.T.);
#23406=ORIENTED_EDGE('',*,*,#16006,.T.);
#23407=ORIENTED_EDGE('',*,*,#16003,.T.);
#23408=ORIENTED_EDGE('',*,*,#16000,.T.);
#23409=ORIENTED_EDGE('',*,*,#15997,.T.);
#23410=ORIENTED_EDGE('',*,*,#15994,.T.);
#23411=ORIENTED_EDGE('',*,*,#15991,.T.);
#23412=ORIENTED_EDGE('',*,*,#15988,.T.);
#23413=ORIENTED_EDGE('',*,*,#15985,.T.);
#23414=ORIENTED_EDGE('',*,*,#15982,.T.);
#23415=ORIENTED_EDGE('',*,*,#15979,.T.);
#23416=ORIENTED_EDGE('',*,*,#15976,.T.);
#23417=ORIENTED_EDGE('',*,*,#15973,.T.);
#23418=ORIENTED_EDGE('',*,*,#15970,.T.);
#23419=ORIENTED_EDGE('',*,*,#15967,.T.);
#23420=ORIENTED_EDGE('',*,*,#15964,.T.);
#23421=ORIENTED_EDGE('',*,*,#15961,.T.);
#23422=ORIENTED_EDGE('',*,*,#15958,.T.);
#23423=ORIENTED_EDGE('',*,*,#15955,.T.);
#23424=ORIENTED_EDGE('',*,*,#15952,.T.);
#23425=ORIENTED_EDGE('',*,*,#15949,.T.);
#23426=ORIENTED_EDGE('',*,*,#15946,.T.);
#23427=ORIENTED_EDGE('',*,*,#15943,.T.);
#23428=ORIENTED_EDGE('',*,*,#15940,.T.);
#23429=ORIENTED_EDGE('',*,*,#15937,.T.);
#23430=ORIENTED_EDGE('',*,*,#15934,.T.);
#23431=ORIENTED_EDGE('',*,*,#15931,.T.);
#23432=ORIENTED_EDGE('',*,*,#15928,.T.);
#23433=ORIENTED_EDGE('',*,*,#15925,.T.);
#23434=ORIENTED_EDGE('',*,*,#15922,.T.);
#23435=ORIENTED_EDGE('',*,*,#15919,.T.);
#23436=ORIENTED_EDGE('',*,*,#15916,.T.);
#23437=ORIENTED_EDGE('',*,*,#15913,.T.);
#23438=ORIENTED_EDGE('',*,*,#15910,.T.);
#23439=ORIENTED_EDGE('',*,*,#15907,.T.);
#23440=ORIENTED_EDGE('',*,*,#15904,.T.);
#23441=ORIENTED_EDGE('',*,*,#15901,.T.);
#23442=ORIENTED_EDGE('',*,*,#15898,.T.);
#23443=ORIENTED_EDGE('',*,*,#15895,.T.);
#23444=ORIENTED_EDGE('',*,*,#15892,.T.);
#23445=ORIENTED_EDGE('',*,*,#15889,.T.);
#23446=ORIENTED_EDGE('',*,*,#15886,.T.);
#23447=ORIENTED_EDGE('',*,*,#15883,.T.);
#23448=ORIENTED_EDGE('',*,*,#15880,.T.);
#23449=ORIENTED_EDGE('',*,*,#15877,.T.);
#23450=ORIENTED_EDGE('',*,*,#15874,.T.);
#23451=ORIENTED_EDGE('',*,*,#15871,.T.);
#23452=ORIENTED_EDGE('',*,*,#15868,.T.);
#23453=ORIENTED_EDGE('',*,*,#15865,.T.);
#23454=ORIENTED_EDGE('',*,*,#15862,.T.);
#23455=ORIENTED_EDGE('',*,*,#15859,.T.);
#23456=ORIENTED_EDGE('',*,*,#16134,.F.);
#23457=ORIENTED_EDGE('',*,*,#15860,.F.);
#23458=ORIENTED_EDGE('',*,*,#15864,.T.);
#23459=ORIENTED_EDGE('',*,*,#15867,.F.);
#23460=ORIENTED_EDGE('',*,*,#15870,.F.);
#23461=ORIENTED_EDGE('',*,*,#15873,.T.);
#23462=ORIENTED_EDGE('',*,*,#15876,.F.);
#23463=ORIENTED_EDGE('',*,*,#15879,.F.);
#23464=ORIENTED_EDGE('',*,*,#15882,.T.);
#23465=ORIENTED_EDGE('',*,*,#15885,.T.);
#23466=ORIENTED_EDGE('',*,*,#15888,.F.);
#23467=ORIENTED_EDGE('',*,*,#15891,.T.);
#23468=ORIENTED_EDGE('',*,*,#15894,.F.);
#23469=ORIENTED_EDGE('',*,*,#15897,.F.);
#23470=ORIENTED_EDGE('',*,*,#15900,.T.);
#23471=ORIENTED_EDGE('',*,*,#15903,.T.);
#23472=ORIENTED_EDGE('',*,*,#15906,.T.);
#23473=ORIENTED_EDGE('',*,*,#15909,.T.);
#23474=ORIENTED_EDGE('',*,*,#15912,.F.);
#23475=ORIENTED_EDGE('',*,*,#15915,.T.);
#23476=ORIENTED_EDGE('',*,*,#15918,.F.);
#23477=ORIENTED_EDGE('',*,*,#15921,.T.);
#23478=ORIENTED_EDGE('',*,*,#15924,.T.);
#23479=ORIENTED_EDGE('',*,*,#15927,.T.);
#23480=ORIENTED_EDGE('',*,*,#15930,.T.);
#23481=ORIENTED_EDGE('',*,*,#15933,.T.);
#23482=ORIENTED_EDGE('',*,*,#15936,.T.);
#23483=ORIENTED_EDGE('',*,*,#15939,.F.);
#23484=ORIENTED_EDGE('',*,*,#15942,.T.);
#23485=ORIENTED_EDGE('',*,*,#15945,.F.);
#23486=ORIENTED_EDGE('',*,*,#15948,.T.);
#23487=ORIENTED_EDGE('',*,*,#15951,.F.);
#23488=ORIENTED_EDGE('',*,*,#15954,.F.);
#23489=ORIENTED_EDGE('',*,*,#15957,.F.);
#23490=ORIENTED_EDGE('',*,*,#15960,.F.);
#23491=ORIENTED_EDGE('',*,*,#15963,.F.);
#23492=ORIENTED_EDGE('',*,*,#15966,.F.);
#23493=ORIENTED_EDGE('',*,*,#15969,.F.);
#23494=ORIENTED_EDGE('',*,*,#15972,.T.);
#23495=ORIENTED_EDGE('',*,*,#15975,.F.);
#23496=ORIENTED_EDGE('',*,*,#15978,.F.);
#23497=ORIENTED_EDGE('',*,*,#15981,.T.);
#23498=ORIENTED_EDGE('',*,*,#15984,.F.);
#23499=ORIENTED_EDGE('',*,*,#15987,.T.);
#23500=ORIENTED_EDGE('',*,*,#15990,.F.);
#23501=ORIENTED_EDGE('',*,*,#15993,.F.);
#23502=ORIENTED_EDGE('',*,*,#15996,.F.);
#23503=ORIENTED_EDGE('',*,*,#15999,.F.);
#23504=ORIENTED_EDGE('',*,*,#16002,.F.);
#23505=ORIENTED_EDGE('',*,*,#16005,.F.);
#23506=ORIENTED_EDGE('',*,*,#16008,.T.);
#23507=ORIENTED_EDGE('',*,*,#16011,.T.);
#23508=ORIENTED_EDGE('',*,*,#16014,.T.);
#23509=ORIENTED_EDGE('',*,*,#16017,.F.);
#23510=ORIENTED_EDGE('',*,*,#16020,.T.);
#23511=ORIENTED_EDGE('',*,*,#16023,.T.);
#23512=ORIENTED_EDGE('',*,*,#16026,.F.);
#23513=ORIENTED_EDGE('',*,*,#16029,.T.);
#23514=ORIENTED_EDGE('',*,*,#16032,.F.);
#23515=ORIENTED_EDGE('',*,*,#16035,.F.);
#23516=ORIENTED_EDGE('',*,*,#16038,.T.);
#23517=ORIENTED_EDGE('',*,*,#16041,.T.);
#23518=ORIENTED_EDGE('',*,*,#16044,.T.);
#23519=ORIENTED_EDGE('',*,*,#16047,.T.);
#23520=ORIENTED_EDGE('',*,*,#16050,.F.);
#23521=ORIENTED_EDGE('',*,*,#16053,.T.);
#23522=ORIENTED_EDGE('',*,*,#16056,.F.);
#23523=ORIENTED_EDGE('',*,*,#16059,.T.);
#23524=ORIENTED_EDGE('',*,*,#16062,.T.);
#23525=ORIENTED_EDGE('',*,*,#16065,.T.);
#23526=ORIENTED_EDGE('',*,*,#16068,.T.);
#23527=ORIENTED_EDGE('',*,*,#16071,.T.);
#23528=ORIENTED_EDGE('',*,*,#16074,.T.);
#23529=ORIENTED_EDGE('',*,*,#16077,.T.);
#23530=ORIENTED_EDGE('',*,*,#16080,.T.);
#23531=ORIENTED_EDGE('',*,*,#16083,.F.);
#23532=ORIENTED_EDGE('',*,*,#16086,.T.);
#23533=ORIENTED_EDGE('',*,*,#16089,.F.);
#23534=ORIENTED_EDGE('',*,*,#16092,.F.);
#23535=ORIENTED_EDGE('',*,*,#16095,.F.);
#23536=ORIENTED_EDGE('',*,*,#16098,.F.);
#23537=ORIENTED_EDGE('',*,*,#16101,.F.);
#23538=ORIENTED_EDGE('',*,*,#16104,.F.);
#23539=ORIENTED_EDGE('',*,*,#16107,.F.);
#23540=ORIENTED_EDGE('',*,*,#16110,.T.);
#23541=ORIENTED_EDGE('',*,*,#16113,.F.);
#23542=ORIENTED_EDGE('',*,*,#16116,.F.);
#23543=ORIENTED_EDGE('',*,*,#16119,.T.);
#23544=ORIENTED_EDGE('',*,*,#16122,.F.);
#23545=ORIENTED_EDGE('',*,*,#16125,.T.);
#23546=ORIENTED_EDGE('',*,*,#16128,.F.);
#23547=ORIENTED_EDGE('',*,*,#16131,.F.);
#23548=ORIENTED_EDGE('',*,*,#15857,.F.);
#23549=ORIENTED_EDGE('',*,*,#16136,.F.);
#23550=ORIENTED_EDGE('',*,*,#16137,.F.);
#23551=ORIENTED_EDGE('',*,*,#16138,.T.);
#23552=ORIENTED_EDGE('',*,*,#16139,.T.);
#23553=ORIENTED_EDGE('',*,*,#16140,.F.);
#23554=ORIENTED_EDGE('',*,*,#16141,.F.);
#23555=ORIENTED_EDGE('',*,*,#16142,.F.);
#23556=ORIENTED_EDGE('',*,*,#16136,.T.);
#23557=ORIENTED_EDGE('',*,*,#16143,.T.);
#23558=ORIENTED_EDGE('',*,*,#16144,.T.);
#23559=ORIENTED_EDGE('',*,*,#16145,.F.);
#23560=ORIENTED_EDGE('',*,*,#16146,.F.);
#23561=ORIENTED_EDGE('',*,*,#16147,.F.);
#23562=ORIENTED_EDGE('',*,*,#16140,.T.);
#23563=ORIENTED_EDGE('',*,*,#16148,.T.);
#23564=ORIENTED_EDGE('',*,*,#16149,.T.);
#23565=ORIENTED_EDGE('',*,*,#16150,.F.);
#23566=ORIENTED_EDGE('',*,*,#16151,.F.);
#23567=ORIENTED_EDGE('',*,*,#16152,.F.);
#23568=ORIENTED_EDGE('',*,*,#16145,.T.);
#23569=ORIENTED_EDGE('',*,*,#16153,.T.);
#23570=ORIENTED_EDGE('',*,*,#16154,.T.);
#23571=ORIENTED_EDGE('',*,*,#16155,.F.);
#23572=ORIENTED_EDGE('',*,*,#16156,.F.);
#23573=ORIENTED_EDGE('',*,*,#16157,.T.);
#23574=ORIENTED_EDGE('',*,*,#16158,.T.);
#23575=ORIENTED_EDGE('',*,*,#16159,.F.);
#23576=ORIENTED_EDGE('',*,*,#16160,.F.);
#23577=ORIENTED_EDGE('',*,*,#16161,.F.);
#23578=ORIENTED_EDGE('',*,*,#16155,.T.);
#23579=ORIENTED_EDGE('',*,*,#16162,.T.);
#23580=ORIENTED_EDGE('',*,*,#16163,.T.);
#23581=ORIENTED_EDGE('',*,*,#16164,.F.);
#23582=ORIENTED_EDGE('',*,*,#16165,.F.);
#23583=ORIENTED_EDGE('',*,*,#16166,.F.);
#23584=ORIENTED_EDGE('',*,*,#16159,.T.);
#23585=ORIENTED_EDGE('',*,*,#16167,.T.);
#23586=ORIENTED_EDGE('',*,*,#16168,.T.);
#23587=ORIENTED_EDGE('',*,*,#16169,.F.);
#23588=ORIENTED_EDGE('',*,*,#16170,.F.);
#23589=ORIENTED_EDGE('',*,*,#16171,.F.);
#23590=ORIENTED_EDGE('',*,*,#16164,.T.);
#23591=ORIENTED_EDGE('',*,*,#16172,.T.);
#23592=ORIENTED_EDGE('',*,*,#16173,.T.);
#23593=ORIENTED_EDGE('',*,*,#16174,.F.);
#23594=ORIENTED_EDGE('',*,*,#16175,.F.);
#23595=ORIENTED_EDGE('',*,*,#16176,.F.);
#23596=ORIENTED_EDGE('',*,*,#16177,.T.);
#23597=ORIENTED_EDGE('',*,*,#16178,.T.);
#23598=ORIENTED_EDGE('',*,*,#16179,.T.);
#23599=ORIENTED_EDGE('',*,*,#16180,.F.);
#23600=ORIENTED_EDGE('',*,*,#16181,.F.);
#23601=ORIENTED_EDGE('',*,*,#16182,.F.);
#23602=ORIENTED_EDGE('',*,*,#16174,.T.);
#23603=ORIENTED_EDGE('',*,*,#16183,.T.);
#23604=ORIENTED_EDGE('',*,*,#16184,.T.);
#23605=ORIENTED_EDGE('',*,*,#16185,.F.);
#23606=ORIENTED_EDGE('',*,*,#16186,.F.);
#23607=ORIENTED_EDGE('',*,*,#16187,.F.);
#23608=ORIENTED_EDGE('',*,*,#16180,.T.);
#23609=ORIENTED_EDGE('',*,*,#16188,.T.);
#23610=ORIENTED_EDGE('',*,*,#16189,.T.);
#23611=ORIENTED_EDGE('',*,*,#16190,.F.);
#23612=ORIENTED_EDGE('',*,*,#16191,.F.);
#23613=ORIENTED_EDGE('',*,*,#16192,.F.);
#23614=ORIENTED_EDGE('',*,*,#16185,.T.);
#23615=ORIENTED_EDGE('',*,*,#16193,.T.);
#23616=ORIENTED_EDGE('',*,*,#16194,.T.);
#23617=ORIENTED_EDGE('',*,*,#16195,.F.);
#23618=ORIENTED_EDGE('',*,*,#16196,.F.);
#23619=ORIENTED_EDGE('',*,*,#16197,.F.);
#23620=ORIENTED_EDGE('',*,*,#16190,.T.);
#23621=ORIENTED_EDGE('',*,*,#16198,.T.);
#23622=ORIENTED_EDGE('',*,*,#16199,.T.);
#23623=ORIENTED_EDGE('',*,*,#16200,.F.);
#23624=ORIENTED_EDGE('',*,*,#16201,.F.);
#23625=ORIENTED_EDGE('',*,*,#16202,.F.);
#23626=ORIENTED_EDGE('',*,*,#16195,.T.);
#23627=ORIENTED_EDGE('',*,*,#16203,.T.);
#23628=ORIENTED_EDGE('',*,*,#16204,.T.);
#23629=ORIENTED_EDGE('',*,*,#16205,.F.);
#23630=ORIENTED_EDGE('',*,*,#16206,.F.);
#23631=ORIENTED_EDGE('',*,*,#16207,.F.);
#23632=ORIENTED_EDGE('',*,*,#16200,.T.);
#23633=ORIENTED_EDGE('',*,*,#16208,.T.);
#23634=ORIENTED_EDGE('',*,*,#16209,.T.);
#23635=ORIENTED_EDGE('',*,*,#16210,.F.);
#23636=ORIENTED_EDGE('',*,*,#16211,.F.);
#23637=ORIENTED_EDGE('',*,*,#16212,.F.);
#23638=ORIENTED_EDGE('',*,*,#16205,.T.);
#23639=ORIENTED_EDGE('',*,*,#16213,.T.);
#23640=ORIENTED_EDGE('',*,*,#16214,.T.);
#23641=ORIENTED_EDGE('',*,*,#16215,.F.);
#23642=ORIENTED_EDGE('',*,*,#16216,.F.);
#23643=ORIENTED_EDGE('',*,*,#16217,.F.);
#23644=ORIENTED_EDGE('',*,*,#16210,.T.);
#23645=ORIENTED_EDGE('',*,*,#16218,.T.);
#23646=ORIENTED_EDGE('',*,*,#16219,.T.);
#23647=ORIENTED_EDGE('',*,*,#16220,.F.);
#23648=ORIENTED_EDGE('',*,*,#16221,.F.);
#23649=ORIENTED_EDGE('',*,*,#16222,.F.);
#23650=ORIENTED_EDGE('',*,*,#16215,.T.);
#23651=ORIENTED_EDGE('',*,*,#16223,.T.);
#23652=ORIENTED_EDGE('',*,*,#16224,.T.);
#23653=ORIENTED_EDGE('',*,*,#16225,.F.);
#23654=ORIENTED_EDGE('',*,*,#16226,.F.);
#23655=ORIENTED_EDGE('',*,*,#16227,.F.);
#23656=ORIENTED_EDGE('',*,*,#16220,.T.);
#23657=ORIENTED_EDGE('',*,*,#16228,.T.);
#23658=ORIENTED_EDGE('',*,*,#16229,.T.);
#23659=ORIENTED_EDGE('',*,*,#16230,.F.);
#23660=ORIENTED_EDGE('',*,*,#16231,.F.);
#23661=ORIENTED_EDGE('',*,*,#16232,.F.);
#23662=ORIENTED_EDGE('',*,*,#16225,.T.);
#23663=ORIENTED_EDGE('',*,*,#16233,.T.);
#23664=ORIENTED_EDGE('',*,*,#16234,.T.);
#23665=ORIENTED_EDGE('',*,*,#16235,.F.);
#23666=ORIENTED_EDGE('',*,*,#16236,.F.);
#23667=ORIENTED_EDGE('',*,*,#16237,.F.);
#23668=ORIENTED_EDGE('',*,*,#16230,.T.);
#23669=ORIENTED_EDGE('',*,*,#16238,.T.);
#23670=ORIENTED_EDGE('',*,*,#16239,.T.);
#23671=ORIENTED_EDGE('',*,*,#16240,.F.);
#23672=ORIENTED_EDGE('',*,*,#16241,.F.);
#23673=ORIENTED_EDGE('',*,*,#16242,.F.);
#23674=ORIENTED_EDGE('',*,*,#16235,.T.);
#23675=ORIENTED_EDGE('',*,*,#16243,.T.);
#23676=ORIENTED_EDGE('',*,*,#16244,.T.);
#23677=ORIENTED_EDGE('',*,*,#16245,.F.);
#23678=ORIENTED_EDGE('',*,*,#16246,.F.);
#23679=ORIENTED_EDGE('',*,*,#16247,.F.);
#23680=ORIENTED_EDGE('',*,*,#16240,.T.);
#23681=ORIENTED_EDGE('',*,*,#16248,.T.);
#23682=ORIENTED_EDGE('',*,*,#16249,.T.);
#23683=ORIENTED_EDGE('',*,*,#16250,.F.);
#23684=ORIENTED_EDGE('',*,*,#16251,.F.);
#23685=ORIENTED_EDGE('',*,*,#16252,.F.);
#23686=ORIENTED_EDGE('',*,*,#16245,.T.);
#23687=ORIENTED_EDGE('',*,*,#16253,.T.);
#23688=ORIENTED_EDGE('',*,*,#16254,.T.);
#23689=ORIENTED_EDGE('',*,*,#16255,.F.);
#23690=ORIENTED_EDGE('',*,*,#16256,.F.);
#23691=ORIENTED_EDGE('',*,*,#16257,.F.);
#23692=ORIENTED_EDGE('',*,*,#16250,.T.);
#23693=ORIENTED_EDGE('',*,*,#16258,.T.);
#23694=ORIENTED_EDGE('',*,*,#16259,.T.);
#23695=ORIENTED_EDGE('',*,*,#16260,.F.);
#23696=ORIENTED_EDGE('',*,*,#16261,.F.);
#23697=ORIENTED_EDGE('',*,*,#16262,.F.);
#23698=ORIENTED_EDGE('',*,*,#16255,.T.);
#23699=ORIENTED_EDGE('',*,*,#16263,.T.);
#23700=ORIENTED_EDGE('',*,*,#16264,.T.);
#23701=ORIENTED_EDGE('',*,*,#16265,.F.);
#23702=ORIENTED_EDGE('',*,*,#16266,.F.);
#23703=ORIENTED_EDGE('',*,*,#16267,.F.);
#23704=ORIENTED_EDGE('',*,*,#16260,.T.);
#23705=ORIENTED_EDGE('',*,*,#16268,.T.);
#23706=ORIENTED_EDGE('',*,*,#16269,.T.);
#23707=ORIENTED_EDGE('',*,*,#16270,.F.);
#23708=ORIENTED_EDGE('',*,*,#16271,.F.);
#23709=ORIENTED_EDGE('',*,*,#16272,.F.);
#23710=ORIENTED_EDGE('',*,*,#16265,.T.);
#23711=ORIENTED_EDGE('',*,*,#16273,.T.);
#23712=ORIENTED_EDGE('',*,*,#16274,.T.);
#23713=ORIENTED_EDGE('',*,*,#16275,.F.);
#23714=ORIENTED_EDGE('',*,*,#16276,.F.);
#23715=ORIENTED_EDGE('',*,*,#16277,.F.);
#23716=ORIENTED_EDGE('',*,*,#16270,.T.);
#23717=ORIENTED_EDGE('',*,*,#16278,.T.);
#23718=ORIENTED_EDGE('',*,*,#16279,.T.);
#23719=ORIENTED_EDGE('',*,*,#16280,.F.);
#23720=ORIENTED_EDGE('',*,*,#16281,.F.);
#23721=ORIENTED_EDGE('',*,*,#16282,.F.);
#23722=ORIENTED_EDGE('',*,*,#16275,.T.);
#23723=ORIENTED_EDGE('',*,*,#16283,.T.);
#23724=ORIENTED_EDGE('',*,*,#16284,.T.);
#23725=ORIENTED_EDGE('',*,*,#16285,.F.);
#23726=ORIENTED_EDGE('',*,*,#16286,.F.);
#23727=ORIENTED_EDGE('',*,*,#16287,.F.);
#23728=ORIENTED_EDGE('',*,*,#16280,.T.);
#23729=ORIENTED_EDGE('',*,*,#16288,.T.);
#23730=ORIENTED_EDGE('',*,*,#16289,.T.);
#23731=ORIENTED_EDGE('',*,*,#16290,.F.);
#23732=ORIENTED_EDGE('',*,*,#16291,.F.);
#23733=ORIENTED_EDGE('',*,*,#16292,.F.);
#23734=ORIENTED_EDGE('',*,*,#16285,.T.);
#23735=ORIENTED_EDGE('',*,*,#16293,.T.);
#23736=ORIENTED_EDGE('',*,*,#16294,.T.);
#23737=ORIENTED_EDGE('',*,*,#16295,.F.);
#23738=ORIENTED_EDGE('',*,*,#16296,.F.);
#23739=ORIENTED_EDGE('',*,*,#16297,.F.);
#23740=ORIENTED_EDGE('',*,*,#16290,.T.);
#23741=ORIENTED_EDGE('',*,*,#16298,.T.);
#23742=ORIENTED_EDGE('',*,*,#16299,.T.);
#23743=ORIENTED_EDGE('',*,*,#16300,.F.);
#23744=ORIENTED_EDGE('',*,*,#16301,.F.);
#23745=ORIENTED_EDGE('',*,*,#16302,.F.);
#23746=ORIENTED_EDGE('',*,*,#16295,.T.);
#23747=ORIENTED_EDGE('',*,*,#16303,.T.);
#23748=ORIENTED_EDGE('',*,*,#16304,.T.);
#23749=ORIENTED_EDGE('',*,*,#16305,.F.);
#23750=ORIENTED_EDGE('',*,*,#16306,.F.);
#23751=ORIENTED_EDGE('',*,*,#16307,.F.);
#23752=ORIENTED_EDGE('',*,*,#16300,.T.);
#23753=ORIENTED_EDGE('',*,*,#16308,.T.);
#23754=ORIENTED_EDGE('',*,*,#16309,.T.);
#23755=ORIENTED_EDGE('',*,*,#16310,.F.);
#23756=ORIENTED_EDGE('',*,*,#16311,.F.);
#23757=ORIENTED_EDGE('',*,*,#16312,.F.);
#23758=ORIENTED_EDGE('',*,*,#16313,.T.);
#23759=ORIENTED_EDGE('',*,*,#16314,.T.);
#23760=ORIENTED_EDGE('',*,*,#16315,.T.);
#23761=ORIENTED_EDGE('',*,*,#16316,.F.);
#23762=ORIENTED_EDGE('',*,*,#16317,.F.);
#23763=ORIENTED_EDGE('',*,*,#16318,.F.);
#23764=ORIENTED_EDGE('',*,*,#16310,.T.);
#23765=ORIENTED_EDGE('',*,*,#16319,.T.);
#23766=ORIENTED_EDGE('',*,*,#16320,.T.);
#23767=ORIENTED_EDGE('',*,*,#16321,.F.);
#23768=ORIENTED_EDGE('',*,*,#16322,.F.);
#23769=ORIENTED_EDGE('',*,*,#16323,.F.);
#23770=ORIENTED_EDGE('',*,*,#16316,.T.);
#23771=ORIENTED_EDGE('',*,*,#16324,.T.);
#23772=ORIENTED_EDGE('',*,*,#16325,.T.);
#23773=ORIENTED_EDGE('',*,*,#16326,.F.);
#23774=ORIENTED_EDGE('',*,*,#16327,.F.);
#23775=ORIENTED_EDGE('',*,*,#16328,.F.);
#23776=ORIENTED_EDGE('',*,*,#16321,.T.);
#23777=ORIENTED_EDGE('',*,*,#16329,.T.);
#23778=ORIENTED_EDGE('',*,*,#16330,.T.);
#23779=ORIENTED_EDGE('',*,*,#16331,.F.);
#23780=ORIENTED_EDGE('',*,*,#16332,.F.);
#23781=ORIENTED_EDGE('',*,*,#16333,.F.);
#23782=ORIENTED_EDGE('',*,*,#16326,.T.);
#23783=ORIENTED_EDGE('',*,*,#16334,.T.);
#23784=ORIENTED_EDGE('',*,*,#16335,.T.);
#23785=ORIENTED_EDGE('',*,*,#16336,.F.);
#23786=ORIENTED_EDGE('',*,*,#16337,.F.);
#23787=ORIENTED_EDGE('',*,*,#16338,.F.);
#23788=ORIENTED_EDGE('',*,*,#16331,.T.);
#23789=ORIENTED_EDGE('',*,*,#16339,.T.);
#23790=ORIENTED_EDGE('',*,*,#16340,.T.);
#23791=ORIENTED_EDGE('',*,*,#16341,.F.);
#23792=ORIENTED_EDGE('',*,*,#16342,.F.);
#23793=ORIENTED_EDGE('',*,*,#16343,.F.);
#23794=ORIENTED_EDGE('',*,*,#16336,.T.);
#23795=ORIENTED_EDGE('',*,*,#16344,.T.);
#23796=ORIENTED_EDGE('',*,*,#16345,.T.);
#23797=ORIENTED_EDGE('',*,*,#16346,.F.);
#23798=ORIENTED_EDGE('',*,*,#16347,.F.);
#23799=ORIENTED_EDGE('',*,*,#16348,.F.);
#23800=ORIENTED_EDGE('',*,*,#16341,.T.);
#23801=ORIENTED_EDGE('',*,*,#16349,.T.);
#23802=ORIENTED_EDGE('',*,*,#16350,.T.);
#23803=ORIENTED_EDGE('',*,*,#16351,.F.);
#23804=ORIENTED_EDGE('',*,*,#16352,.F.);
#23805=ORIENTED_EDGE('',*,*,#16353,.F.);
#23806=ORIENTED_EDGE('',*,*,#16346,.T.);
#23807=ORIENTED_EDGE('',*,*,#16354,.T.);
#23808=ORIENTED_EDGE('',*,*,#16355,.T.);
#23809=ORIENTED_EDGE('',*,*,#16356,.F.);
#23810=ORIENTED_EDGE('',*,*,#16357,.F.);
#23811=ORIENTED_EDGE('',*,*,#16358,.F.);
#23812=ORIENTED_EDGE('',*,*,#16351,.T.);
#23813=ORIENTED_EDGE('',*,*,#16359,.T.);
#23814=ORIENTED_EDGE('',*,*,#16360,.T.);
#23815=ORIENTED_EDGE('',*,*,#16361,.F.);
#23816=ORIENTED_EDGE('',*,*,#16362,.F.);
#23817=ORIENTED_EDGE('',*,*,#16363,.F.);
#23818=ORIENTED_EDGE('',*,*,#16356,.T.);
#23819=ORIENTED_EDGE('',*,*,#16364,.T.);
#23820=ORIENTED_EDGE('',*,*,#16365,.T.);
#23821=ORIENTED_EDGE('',*,*,#16366,.F.);
#23822=ORIENTED_EDGE('',*,*,#16367,.F.);
#23823=ORIENTED_EDGE('',*,*,#16368,.F.);
#23824=ORIENTED_EDGE('',*,*,#16361,.T.);
#23825=ORIENTED_EDGE('',*,*,#16369,.T.);
#23826=ORIENTED_EDGE('',*,*,#16370,.T.);
#23827=ORIENTED_EDGE('',*,*,#16371,.F.);
#23828=ORIENTED_EDGE('',*,*,#16372,.F.);
#23829=ORIENTED_EDGE('',*,*,#16373,.F.);
#23830=ORIENTED_EDGE('',*,*,#16366,.T.);
#23831=ORIENTED_EDGE('',*,*,#16374,.T.);
#23832=ORIENTED_EDGE('',*,*,#16375,.T.);
#23833=ORIENTED_EDGE('',*,*,#16376,.F.);
#23834=ORIENTED_EDGE('',*,*,#16377,.F.);
#23835=ORIENTED_EDGE('',*,*,#16378,.F.);
#23836=ORIENTED_EDGE('',*,*,#16371,.T.);
#23837=ORIENTED_EDGE('',*,*,#16379,.T.);
#23838=ORIENTED_EDGE('',*,*,#16380,.T.);
#23839=ORIENTED_EDGE('',*,*,#16381,.F.);
#23840=ORIENTED_EDGE('',*,*,#16382,.F.);
#23841=ORIENTED_EDGE('',*,*,#16383,.F.);
#23842=ORIENTED_EDGE('',*,*,#16376,.T.);
#23843=ORIENTED_EDGE('',*,*,#16384,.T.);
#23844=ORIENTED_EDGE('',*,*,#16385,.T.);
#23845=ORIENTED_EDGE('',*,*,#16386,.F.);
#23846=ORIENTED_EDGE('',*,*,#16387,.F.);
#23847=ORIENTED_EDGE('',*,*,#16388,.F.);
#23848=ORIENTED_EDGE('',*,*,#16381,.T.);
#23849=ORIENTED_EDGE('',*,*,#16389,.T.);
#23850=ORIENTED_EDGE('',*,*,#16390,.T.);
#23851=ORIENTED_EDGE('',*,*,#16391,.F.);
#23852=ORIENTED_EDGE('',*,*,#16392,.F.);
#23853=ORIENTED_EDGE('',*,*,#16393,.F.);
#23854=ORIENTED_EDGE('',*,*,#16386,.T.);
#23855=ORIENTED_EDGE('',*,*,#16394,.T.);
#23856=ORIENTED_EDGE('',*,*,#16395,.T.);
#23857=ORIENTED_EDGE('',*,*,#16396,.F.);
#23858=ORIENTED_EDGE('',*,*,#16397,.F.);
#23859=ORIENTED_EDGE('',*,*,#16398,.F.);
#23860=ORIENTED_EDGE('',*,*,#16391,.T.);
#23861=ORIENTED_EDGE('',*,*,#16399,.T.);
#23862=ORIENTED_EDGE('',*,*,#16400,.T.);
#23863=ORIENTED_EDGE('',*,*,#16401,.F.);
#23864=ORIENTED_EDGE('',*,*,#16402,.F.);
#23865=ORIENTED_EDGE('',*,*,#16403,.F.);
#23866=ORIENTED_EDGE('',*,*,#16396,.T.);
#23867=ORIENTED_EDGE('',*,*,#16404,.T.);
#23868=ORIENTED_EDGE('',*,*,#16405,.T.);
#23869=ORIENTED_EDGE('',*,*,#16406,.F.);
#23870=ORIENTED_EDGE('',*,*,#16407,.F.);
#23871=ORIENTED_EDGE('',*,*,#16408,.F.);
#23872=ORIENTED_EDGE('',*,*,#16401,.T.);
#23873=ORIENTED_EDGE('',*,*,#16409,.T.);
#23874=ORIENTED_EDGE('',*,*,#16410,.T.);
#23875=ORIENTED_EDGE('',*,*,#16411,.F.);
#23876=ORIENTED_EDGE('',*,*,#16412,.F.);
#23877=ORIENTED_EDGE('',*,*,#16413,.F.);
#23878=ORIENTED_EDGE('',*,*,#16406,.T.);
#23879=ORIENTED_EDGE('',*,*,#16414,.T.);
#23880=ORIENTED_EDGE('',*,*,#16415,.T.);
#23881=ORIENTED_EDGE('',*,*,#16416,.F.);
#23882=ORIENTED_EDGE('',*,*,#16417,.F.);
#23883=ORIENTED_EDGE('',*,*,#16418,.F.);
#23884=ORIENTED_EDGE('',*,*,#16411,.T.);
#23885=ORIENTED_EDGE('',*,*,#16419,.T.);
#23886=ORIENTED_EDGE('',*,*,#16420,.T.);
#23887=ORIENTED_EDGE('',*,*,#16421,.F.);
#23888=ORIENTED_EDGE('',*,*,#16422,.F.);
#23889=ORIENTED_EDGE('',*,*,#16423,.F.);
#23890=ORIENTED_EDGE('',*,*,#16416,.T.);
#23891=ORIENTED_EDGE('',*,*,#16424,.T.);
#23892=ORIENTED_EDGE('',*,*,#16425,.T.);
#23893=ORIENTED_EDGE('',*,*,#16426,.F.);
#23894=ORIENTED_EDGE('',*,*,#16427,.F.);
#23895=ORIENTED_EDGE('',*,*,#16428,.F.);
#23896=ORIENTED_EDGE('',*,*,#16421,.T.);
#23897=ORIENTED_EDGE('',*,*,#16429,.T.);
#23898=ORIENTED_EDGE('',*,*,#16430,.T.);
#23899=ORIENTED_EDGE('',*,*,#16431,.F.);
#23900=ORIENTED_EDGE('',*,*,#16432,.F.);
#23901=ORIENTED_EDGE('',*,*,#16433,.F.);
#23902=ORIENTED_EDGE('',*,*,#16426,.T.);
#23903=ORIENTED_EDGE('',*,*,#16434,.T.);
#23904=ORIENTED_EDGE('',*,*,#16435,.T.);
#23905=ORIENTED_EDGE('',*,*,#16436,.F.);
#23906=ORIENTED_EDGE('',*,*,#16437,.F.);
#23907=ORIENTED_EDGE('',*,*,#16438,.F.);
#23908=ORIENTED_EDGE('',*,*,#16431,.T.);
#23909=ORIENTED_EDGE('',*,*,#16439,.T.);
#23910=ORIENTED_EDGE('',*,*,#16440,.T.);
#23911=ORIENTED_EDGE('',*,*,#16441,.F.);
#23912=ORIENTED_EDGE('',*,*,#16442,.F.);
#23913=ORIENTED_EDGE('',*,*,#16443,.F.);
#23914=ORIENTED_EDGE('',*,*,#16436,.T.);
#23915=ORIENTED_EDGE('',*,*,#16444,.T.);
#23916=ORIENTED_EDGE('',*,*,#16445,.T.);
#23917=ORIENTED_EDGE('',*,*,#16446,.F.);
#23918=ORIENTED_EDGE('',*,*,#16447,.F.);
#23919=ORIENTED_EDGE('',*,*,#16448,.F.);
#23920=ORIENTED_EDGE('',*,*,#16449,.T.);
#23921=ORIENTED_EDGE('',*,*,#16450,.T.);
#23922=ORIENTED_EDGE('',*,*,#16451,.T.);
#23923=ORIENTED_EDGE('',*,*,#16452,.F.);
#23924=ORIENTED_EDGE('',*,*,#16453,.F.);
#23925=ORIENTED_EDGE('',*,*,#16454,.F.);
#23926=ORIENTED_EDGE('',*,*,#16446,.T.);
#23927=ORIENTED_EDGE('',*,*,#16455,.T.);
#23928=ORIENTED_EDGE('',*,*,#16456,.T.);
#23929=ORIENTED_EDGE('',*,*,#16457,.F.);
#23930=ORIENTED_EDGE('',*,*,#16458,.F.);
#23931=ORIENTED_EDGE('',*,*,#16459,.F.);
#23932=ORIENTED_EDGE('',*,*,#16452,.T.);
#23933=ORIENTED_EDGE('',*,*,#16460,.T.);
#23934=ORIENTED_EDGE('',*,*,#16461,.T.);
#23935=ORIENTED_EDGE('',*,*,#16462,.F.);
#23936=ORIENTED_EDGE('',*,*,#16463,.F.);
#23937=ORIENTED_EDGE('',*,*,#16464,.F.);
#23938=ORIENTED_EDGE('',*,*,#16457,.T.);
#23939=ORIENTED_EDGE('',*,*,#16465,.T.);
#23940=ORIENTED_EDGE('',*,*,#16466,.T.);
#23941=ORIENTED_EDGE('',*,*,#16467,.F.);
#23942=ORIENTED_EDGE('',*,*,#16468,.F.);
#23943=ORIENTED_EDGE('',*,*,#16469,.F.);
#23944=ORIENTED_EDGE('',*,*,#16462,.T.);
#23945=ORIENTED_EDGE('',*,*,#16470,.T.);
#23946=ORIENTED_EDGE('',*,*,#16471,.T.);
#23947=ORIENTED_EDGE('',*,*,#16472,.F.);
#23948=ORIENTED_EDGE('',*,*,#16473,.F.);
#23949=ORIENTED_EDGE('',*,*,#16474,.F.);
#23950=ORIENTED_EDGE('',*,*,#16467,.T.);
#23951=ORIENTED_EDGE('',*,*,#16475,.T.);
#23952=ORIENTED_EDGE('',*,*,#16476,.T.);
#23953=ORIENTED_EDGE('',*,*,#16477,.F.);
#23954=ORIENTED_EDGE('',*,*,#16478,.F.);
#23955=ORIENTED_EDGE('',*,*,#16479,.F.);
#23956=ORIENTED_EDGE('',*,*,#16472,.T.);
#23957=ORIENTED_EDGE('',*,*,#16480,.T.);
#23958=ORIENTED_EDGE('',*,*,#16481,.T.);
#23959=ORIENTED_EDGE('',*,*,#16482,.F.);
#23960=ORIENTED_EDGE('',*,*,#16483,.F.);
#23961=ORIENTED_EDGE('',*,*,#16484,.F.);
#23962=ORIENTED_EDGE('',*,*,#16477,.T.);
#23963=ORIENTED_EDGE('',*,*,#16485,.T.);
#23964=ORIENTED_EDGE('',*,*,#16486,.T.);
#23965=ORIENTED_EDGE('',*,*,#16487,.F.);
#23966=ORIENTED_EDGE('',*,*,#16488,.F.);
#23967=ORIENTED_EDGE('',*,*,#16489,.F.);
#23968=ORIENTED_EDGE('',*,*,#16482,.T.);
#23969=ORIENTED_EDGE('',*,*,#16490,.T.);
#23970=ORIENTED_EDGE('',*,*,#16491,.T.);
#23971=ORIENTED_EDGE('',*,*,#16492,.F.);
#23972=ORIENTED_EDGE('',*,*,#16493,.F.);
#23973=ORIENTED_EDGE('',*,*,#16494,.F.);
#23974=ORIENTED_EDGE('',*,*,#16487,.T.);
#23975=ORIENTED_EDGE('',*,*,#16495,.T.);
#23976=ORIENTED_EDGE('',*,*,#16496,.T.);
#23977=ORIENTED_EDGE('',*,*,#16497,.F.);
#23978=ORIENTED_EDGE('',*,*,#16498,.F.);
#23979=ORIENTED_EDGE('',*,*,#16499,.F.);
#23980=ORIENTED_EDGE('',*,*,#16492,.T.);
#23981=ORIENTED_EDGE('',*,*,#16500,.T.);
#23982=ORIENTED_EDGE('',*,*,#16501,.T.);
#23983=ORIENTED_EDGE('',*,*,#16502,.F.);
#23984=ORIENTED_EDGE('',*,*,#16503,.F.);
#23985=ORIENTED_EDGE('',*,*,#16504,.F.);
#23986=ORIENTED_EDGE('',*,*,#16497,.T.);
#23987=ORIENTED_EDGE('',*,*,#16505,.T.);
#23988=ORIENTED_EDGE('',*,*,#16506,.T.);
#23989=ORIENTED_EDGE('',*,*,#16507,.F.);
#23990=ORIENTED_EDGE('',*,*,#16508,.F.);
#23991=ORIENTED_EDGE('',*,*,#16509,.F.);
#23992=ORIENTED_EDGE('',*,*,#16502,.T.);
#23993=ORIENTED_EDGE('',*,*,#16510,.T.);
#23994=ORIENTED_EDGE('',*,*,#16511,.T.);
#23995=ORIENTED_EDGE('',*,*,#16512,.F.);
#23996=ORIENTED_EDGE('',*,*,#16513,.F.);
#23997=ORIENTED_EDGE('',*,*,#16514,.F.);
#23998=ORIENTED_EDGE('',*,*,#16507,.T.);
#23999=ORIENTED_EDGE('',*,*,#16515,.T.);
#24000=ORIENTED_EDGE('',*,*,#16516,.T.);
#24001=ORIENTED_EDGE('',*,*,#16517,.F.);
#24002=ORIENTED_EDGE('',*,*,#16518,.F.);
#24003=ORIENTED_EDGE('',*,*,#16519,.F.);
#24004=ORIENTED_EDGE('',*,*,#16512,.T.);
#24005=ORIENTED_EDGE('',*,*,#16520,.T.);
#24006=ORIENTED_EDGE('',*,*,#16521,.T.);
#24007=ORIENTED_EDGE('',*,*,#16522,.F.);
#24008=ORIENTED_EDGE('',*,*,#16523,.F.);
#24009=ORIENTED_EDGE('',*,*,#16524,.F.);
#24010=ORIENTED_EDGE('',*,*,#16517,.T.);
#24011=ORIENTED_EDGE('',*,*,#16525,.T.);
#24012=ORIENTED_EDGE('',*,*,#16526,.T.);
#24013=ORIENTED_EDGE('',*,*,#16527,.F.);
#24014=ORIENTED_EDGE('',*,*,#16528,.F.);
#24015=ORIENTED_EDGE('',*,*,#16529,.F.);
#24016=ORIENTED_EDGE('',*,*,#16522,.T.);
#24017=ORIENTED_EDGE('',*,*,#16530,.T.);
#24018=ORIENTED_EDGE('',*,*,#16531,.T.);
#24019=ORIENTED_EDGE('',*,*,#16532,.F.);
#24020=ORIENTED_EDGE('',*,*,#16533,.F.);
#24021=ORIENTED_EDGE('',*,*,#16534,.F.);
#24022=ORIENTED_EDGE('',*,*,#16527,.T.);
#24023=ORIENTED_EDGE('',*,*,#16535,.T.);
#24024=ORIENTED_EDGE('',*,*,#16536,.T.);
#24025=ORIENTED_EDGE('',*,*,#16537,.F.);
#24026=ORIENTED_EDGE('',*,*,#16538,.F.);
#24027=ORIENTED_EDGE('',*,*,#16539,.F.);
#24028=ORIENTED_EDGE('',*,*,#16532,.T.);
#24029=ORIENTED_EDGE('',*,*,#16540,.T.);
#24030=ORIENTED_EDGE('',*,*,#16541,.T.);
#24031=ORIENTED_EDGE('',*,*,#16542,.F.);
#24032=ORIENTED_EDGE('',*,*,#16543,.F.);
#24033=ORIENTED_EDGE('',*,*,#16544,.F.);
#24034=ORIENTED_EDGE('',*,*,#16537,.T.);
#24035=ORIENTED_EDGE('',*,*,#16545,.T.);
#24036=ORIENTED_EDGE('',*,*,#16546,.T.);
#24037=ORIENTED_EDGE('',*,*,#16547,.F.);
#24038=ORIENTED_EDGE('',*,*,#16548,.F.);
#24039=ORIENTED_EDGE('',*,*,#16549,.F.);
#24040=ORIENTED_EDGE('',*,*,#16542,.T.);
#24041=ORIENTED_EDGE('',*,*,#16550,.T.);
#24042=ORIENTED_EDGE('',*,*,#16551,.T.);
#24043=ORIENTED_EDGE('',*,*,#16552,.F.);
#24044=ORIENTED_EDGE('',*,*,#16553,.F.);
#24045=ORIENTED_EDGE('',*,*,#16554,.F.);
#24046=ORIENTED_EDGE('',*,*,#16547,.T.);
#24047=ORIENTED_EDGE('',*,*,#16555,.T.);
#24048=ORIENTED_EDGE('',*,*,#16556,.T.);
#24049=ORIENTED_EDGE('',*,*,#16557,.F.);
#24050=ORIENTED_EDGE('',*,*,#16558,.F.);
#24051=ORIENTED_EDGE('',*,*,#16559,.F.);
#24052=ORIENTED_EDGE('',*,*,#16552,.T.);
#24053=ORIENTED_EDGE('',*,*,#16560,.T.);
#24054=ORIENTED_EDGE('',*,*,#16561,.T.);
#24055=ORIENTED_EDGE('',*,*,#16562,.F.);
#24056=ORIENTED_EDGE('',*,*,#16563,.F.);
#24057=ORIENTED_EDGE('',*,*,#16564,.F.);
#24058=ORIENTED_EDGE('',*,*,#16557,.T.);
#24059=ORIENTED_EDGE('',*,*,#16565,.T.);
#24060=ORIENTED_EDGE('',*,*,#16566,.T.);
#24061=ORIENTED_EDGE('',*,*,#16567,.F.);
#24062=ORIENTED_EDGE('',*,*,#16568,.F.);
#24063=ORIENTED_EDGE('',*,*,#16569,.F.);
#24064=ORIENTED_EDGE('',*,*,#16562,.T.);
#24065=ORIENTED_EDGE('',*,*,#16570,.T.);
#24066=ORIENTED_EDGE('',*,*,#16571,.T.);
#24067=ORIENTED_EDGE('',*,*,#16572,.F.);
#24068=ORIENTED_EDGE('',*,*,#16573,.F.);
#24069=ORIENTED_EDGE('',*,*,#16574,.F.);
#24070=ORIENTED_EDGE('',*,*,#16567,.T.);
#24071=ORIENTED_EDGE('',*,*,#16575,.T.);
#24072=ORIENTED_EDGE('',*,*,#16576,.T.);
#24073=ORIENTED_EDGE('',*,*,#16577,.F.);
#24074=ORIENTED_EDGE('',*,*,#16578,.F.);
#24075=ORIENTED_EDGE('',*,*,#16579,.F.);
#24076=ORIENTED_EDGE('',*,*,#16572,.T.);
#24077=ORIENTED_EDGE('',*,*,#16580,.T.);
#24078=ORIENTED_EDGE('',*,*,#16581,.T.);
#24079=ORIENTED_EDGE('',*,*,#16582,.F.);
#24080=ORIENTED_EDGE('',*,*,#16583,.F.);
#24081=ORIENTED_EDGE('',*,*,#16584,.F.);
#24082=ORIENTED_EDGE('',*,*,#16585,.T.);
#24083=ORIENTED_EDGE('',*,*,#16586,.T.);
#24084=ORIENTED_EDGE('',*,*,#16587,.T.);
#24085=ORIENTED_EDGE('',*,*,#16588,.F.);
#24086=ORIENTED_EDGE('',*,*,#16589,.F.);
#24087=ORIENTED_EDGE('',*,*,#16590,.F.);
#24088=ORIENTED_EDGE('',*,*,#16582,.T.);
#24089=ORIENTED_EDGE('',*,*,#16591,.T.);
#24090=ORIENTED_EDGE('',*,*,#16592,.T.);
#24091=ORIENTED_EDGE('',*,*,#16593,.F.);
#24092=ORIENTED_EDGE('',*,*,#16594,.F.);
#24093=ORIENTED_EDGE('',*,*,#16595,.F.);
#24094=ORIENTED_EDGE('',*,*,#16588,.T.);
#24095=ORIENTED_EDGE('',*,*,#16596,.T.);
#24096=ORIENTED_EDGE('',*,*,#16597,.T.);
#24097=ORIENTED_EDGE('',*,*,#16598,.F.);
#24098=ORIENTED_EDGE('',*,*,#16599,.F.);
#24099=ORIENTED_EDGE('',*,*,#16600,.F.);
#24100=ORIENTED_EDGE('',*,*,#16593,.T.);
#24101=ORIENTED_EDGE('',*,*,#16601,.T.);
#24102=ORIENTED_EDGE('',*,*,#16602,.T.);
#24103=ORIENTED_EDGE('',*,*,#16603,.F.);
#24104=ORIENTED_EDGE('',*,*,#16604,.F.);
#24105=ORIENTED_EDGE('',*,*,#16605,.F.);
#24106=ORIENTED_EDGE('',*,*,#16598,.T.);
#24107=ORIENTED_EDGE('',*,*,#16606,.T.);
#24108=ORIENTED_EDGE('',*,*,#16607,.T.);
#24109=ORIENTED_EDGE('',*,*,#16608,.F.);
#24110=ORIENTED_EDGE('',*,*,#16609,.F.);
#24111=ORIENTED_EDGE('',*,*,#16610,.F.);
#24112=ORIENTED_EDGE('',*,*,#16603,.T.);
#24113=ORIENTED_EDGE('',*,*,#16611,.T.);
#24114=ORIENTED_EDGE('',*,*,#16612,.T.);
#24115=ORIENTED_EDGE('',*,*,#16613,.F.);
#24116=ORIENTED_EDGE('',*,*,#16614,.F.);
#24117=ORIENTED_EDGE('',*,*,#16615,.F.);
#24118=ORIENTED_EDGE('',*,*,#16608,.T.);
#24119=ORIENTED_EDGE('',*,*,#16616,.T.);
#24120=ORIENTED_EDGE('',*,*,#16617,.T.);
#24121=ORIENTED_EDGE('',*,*,#16618,.F.);
#24122=ORIENTED_EDGE('',*,*,#16619,.F.);
#24123=ORIENTED_EDGE('',*,*,#16620,.F.);
#24124=ORIENTED_EDGE('',*,*,#16613,.T.);
#24125=ORIENTED_EDGE('',*,*,#16621,.T.);
#24126=ORIENTED_EDGE('',*,*,#16622,.T.);
#24127=ORIENTED_EDGE('',*,*,#16623,.F.);
#24128=ORIENTED_EDGE('',*,*,#16624,.F.);
#24129=ORIENTED_EDGE('',*,*,#16625,.F.);
#24130=ORIENTED_EDGE('',*,*,#16618,.T.);
#24131=ORIENTED_EDGE('',*,*,#16626,.T.);
#24132=ORIENTED_EDGE('',*,*,#16627,.T.);
#24133=ORIENTED_EDGE('',*,*,#16628,.F.);
#24134=ORIENTED_EDGE('',*,*,#16629,.F.);
#24135=ORIENTED_EDGE('',*,*,#16630,.F.);
#24136=ORIENTED_EDGE('',*,*,#16623,.T.);
#24137=ORIENTED_EDGE('',*,*,#16631,.T.);
#24138=ORIENTED_EDGE('',*,*,#16632,.T.);
#24139=ORIENTED_EDGE('',*,*,#16633,.F.);
#24140=ORIENTED_EDGE('',*,*,#16634,.F.);
#24141=ORIENTED_EDGE('',*,*,#16635,.F.);
#24142=ORIENTED_EDGE('',*,*,#16628,.T.);
#24143=ORIENTED_EDGE('',*,*,#16636,.T.);
#24144=ORIENTED_EDGE('',*,*,#16637,.T.);
#24145=ORIENTED_EDGE('',*,*,#16638,.F.);
#24146=ORIENTED_EDGE('',*,*,#16639,.F.);
#24147=ORIENTED_EDGE('',*,*,#16640,.F.);
#24148=ORIENTED_EDGE('',*,*,#16633,.T.);
#24149=ORIENTED_EDGE('',*,*,#16641,.T.);
#24150=ORIENTED_EDGE('',*,*,#16642,.T.);
#24151=ORIENTED_EDGE('',*,*,#16643,.F.);
#24152=ORIENTED_EDGE('',*,*,#16644,.F.);
#24153=ORIENTED_EDGE('',*,*,#16645,.F.);
#24154=ORIENTED_EDGE('',*,*,#16638,.T.);
#24155=ORIENTED_EDGE('',*,*,#16646,.T.);
#24156=ORIENTED_EDGE('',*,*,#16647,.T.);
#24157=ORIENTED_EDGE('',*,*,#16648,.F.);
#24158=ORIENTED_EDGE('',*,*,#16649,.F.);
#24159=ORIENTED_EDGE('',*,*,#16650,.F.);
#24160=ORIENTED_EDGE('',*,*,#16643,.T.);
#24161=ORIENTED_EDGE('',*,*,#16651,.T.);
#24162=ORIENTED_EDGE('',*,*,#16652,.T.);
#24163=ORIENTED_EDGE('',*,*,#16653,.F.);
#24164=ORIENTED_EDGE('',*,*,#16654,.F.);
#24165=ORIENTED_EDGE('',*,*,#16655,.F.);
#24166=ORIENTED_EDGE('',*,*,#16648,.T.);
#24167=ORIENTED_EDGE('',*,*,#16656,.T.);
#24168=ORIENTED_EDGE('',*,*,#16657,.T.);
#24169=ORIENTED_EDGE('',*,*,#16658,.F.);
#24170=ORIENTED_EDGE('',*,*,#16659,.F.);
#24171=ORIENTED_EDGE('',*,*,#16660,.F.);
#24172=ORIENTED_EDGE('',*,*,#16653,.T.);
#24173=ORIENTED_EDGE('',*,*,#16661,.T.);
#24174=ORIENTED_EDGE('',*,*,#16662,.T.);
#24175=ORIENTED_EDGE('',*,*,#16663,.F.);
#24176=ORIENTED_EDGE('',*,*,#16664,.F.);
#24177=ORIENTED_EDGE('',*,*,#16665,.F.);
#24178=ORIENTED_EDGE('',*,*,#16658,.T.);
#24179=ORIENTED_EDGE('',*,*,#16666,.T.);
#24180=ORIENTED_EDGE('',*,*,#16667,.T.);
#24181=ORIENTED_EDGE('',*,*,#16668,.F.);
#24182=ORIENTED_EDGE('',*,*,#16669,.F.);
#24183=ORIENTED_EDGE('',*,*,#16670,.F.);
#24184=ORIENTED_EDGE('',*,*,#16663,.T.);
#24185=ORIENTED_EDGE('',*,*,#16671,.T.);
#24186=ORIENTED_EDGE('',*,*,#16672,.T.);
#24187=ORIENTED_EDGE('',*,*,#16673,.F.);
#24188=ORIENTED_EDGE('',*,*,#16674,.F.);
#24189=ORIENTED_EDGE('',*,*,#16675,.F.);
#24190=ORIENTED_EDGE('',*,*,#16668,.T.);
#24191=ORIENTED_EDGE('',*,*,#16676,.T.);
#24192=ORIENTED_EDGE('',*,*,#16677,.T.);
#24193=ORIENTED_EDGE('',*,*,#16678,.F.);
#24194=ORIENTED_EDGE('',*,*,#16679,.F.);
#24195=ORIENTED_EDGE('',*,*,#16680,.F.);
#24196=ORIENTED_EDGE('',*,*,#16673,.T.);
#24197=ORIENTED_EDGE('',*,*,#16681,.T.);
#24198=ORIENTED_EDGE('',*,*,#16682,.T.);
#24199=ORIENTED_EDGE('',*,*,#16683,.F.);
#24200=ORIENTED_EDGE('',*,*,#16684,.F.);
#24201=ORIENTED_EDGE('',*,*,#16685,.F.);
#24202=ORIENTED_EDGE('',*,*,#16678,.T.);
#24203=ORIENTED_EDGE('',*,*,#16686,.T.);
#24204=ORIENTED_EDGE('',*,*,#16687,.T.);
#24205=ORIENTED_EDGE('',*,*,#16688,.F.);
#24206=ORIENTED_EDGE('',*,*,#16689,.F.);
#24207=ORIENTED_EDGE('',*,*,#16690,.F.);
#24208=ORIENTED_EDGE('',*,*,#16683,.T.);
#24209=ORIENTED_EDGE('',*,*,#16691,.T.);
#24210=ORIENTED_EDGE('',*,*,#16692,.T.);
#24211=ORIENTED_EDGE('',*,*,#16693,.F.);
#24212=ORIENTED_EDGE('',*,*,#16694,.F.);
#24213=ORIENTED_EDGE('',*,*,#16695,.F.);
#24214=ORIENTED_EDGE('',*,*,#16688,.T.);
#24215=ORIENTED_EDGE('',*,*,#16696,.T.);
#24216=ORIENTED_EDGE('',*,*,#16697,.T.);
#24217=ORIENTED_EDGE('',*,*,#16698,.F.);
#24218=ORIENTED_EDGE('',*,*,#16699,.F.);
#24219=ORIENTED_EDGE('',*,*,#16700,.F.);
#24220=ORIENTED_EDGE('',*,*,#16693,.T.);
#24221=ORIENTED_EDGE('',*,*,#16701,.T.);
#24222=ORIENTED_EDGE('',*,*,#16702,.T.);
#24223=ORIENTED_EDGE('',*,*,#16703,.F.);
#24224=ORIENTED_EDGE('',*,*,#16704,.F.);
#24225=ORIENTED_EDGE('',*,*,#16705,.F.);
#24226=ORIENTED_EDGE('',*,*,#16698,.T.);
#24227=ORIENTED_EDGE('',*,*,#16706,.T.);
#24228=ORIENTED_EDGE('',*,*,#16707,.T.);
#24229=ORIENTED_EDGE('',*,*,#16708,.F.);
#24230=ORIENTED_EDGE('',*,*,#16709,.F.);
#24231=ORIENTED_EDGE('',*,*,#16710,.F.);
#24232=ORIENTED_EDGE('',*,*,#16703,.T.);
#24233=ORIENTED_EDGE('',*,*,#16711,.T.);
#24234=ORIENTED_EDGE('',*,*,#16712,.T.);
#24235=ORIENTED_EDGE('',*,*,#16713,.F.);
#24236=ORIENTED_EDGE('',*,*,#16714,.F.);
#24237=ORIENTED_EDGE('',*,*,#16715,.F.);
#24238=ORIENTED_EDGE('',*,*,#16708,.T.);
#24239=ORIENTED_EDGE('',*,*,#16716,.T.);
#24240=ORIENTED_EDGE('',*,*,#16717,.T.);
#24241=ORIENTED_EDGE('',*,*,#16718,.F.);
#24242=ORIENTED_EDGE('',*,*,#16719,.F.);
#24243=ORIENTED_EDGE('',*,*,#16720,.T.);
#24244=ORIENTED_EDGE('',*,*,#16721,.F.);
#24245=ORIENTED_EDGE('',*,*,#16722,.F.);
#24246=ORIENTED_EDGE('',*,*,#16718,.T.);
#24247=ORIENTED_EDGE('',*,*,#16723,.T.);
#24248=ORIENTED_EDGE('',*,*,#16724,.F.);
#24249=ORIENTED_EDGE('',*,*,#16725,.F.);
#24250=ORIENTED_EDGE('',*,*,#16726,.F.);
#24251=ORIENTED_EDGE('',*,*,#16721,.T.);
#24252=ORIENTED_EDGE('',*,*,#16727,.F.);
#24253=ORIENTED_EDGE('',*,*,#16728,.F.);
#24254=ORIENTED_EDGE('',*,*,#16729,.F.);
#24255=ORIENTED_EDGE('',*,*,#16725,.T.);
#24256=ORIENTED_EDGE('',*,*,#16730,.F.);
#24257=ORIENTED_EDGE('',*,*,#16731,.F.);
#24258=ORIENTED_EDGE('',*,*,#16732,.F.);
#24259=ORIENTED_EDGE('',*,*,#16733,.F.);
#24260=ORIENTED_EDGE('',*,*,#16734,.F.);
#24261=ORIENTED_EDGE('',*,*,#16735,.F.);
#24262=ORIENTED_EDGE('',*,*,#16736,.F.);
#24263=ORIENTED_EDGE('',*,*,#16731,.T.);
#24264=ORIENTED_EDGE('',*,*,#16737,.F.);
#24265=ORIENTED_EDGE('',*,*,#16738,.F.);
#24266=ORIENTED_EDGE('',*,*,#16739,.F.);
#24267=ORIENTED_EDGE('',*,*,#16735,.T.);
#24268=ORIENTED_EDGE('',*,*,#16740,.F.);
#24269=ORIENTED_EDGE('',*,*,#16741,.F.);
#24270=ORIENTED_EDGE('',*,*,#16742,.F.);
#24271=ORIENTED_EDGE('',*,*,#16743,.F.);
#24272=ORIENTED_EDGE('',*,*,#16738,.T.);
#24273=ORIENTED_EDGE('',*,*,#16744,.F.);
#24274=ORIENTED_EDGE('',*,*,#16745,.F.);
#24275=ORIENTED_EDGE('',*,*,#16746,.F.);
#24276=ORIENTED_EDGE('',*,*,#16747,.F.);
#24277=ORIENTED_EDGE('',*,*,#16748,.T.);
#24278=ORIENTED_EDGE('',*,*,#16749,.F.);
#24279=ORIENTED_EDGE('',*,*,#16750,.F.);
#24280=ORIENTED_EDGE('',*,*,#16751,.F.);
#24281=ORIENTED_EDGE('',*,*,#16752,.F.);
#24282=ORIENTED_EDGE('',*,*,#16753,.F.);
#24283=ORIENTED_EDGE('',*,*,#16745,.T.);
#24284=ORIENTED_EDGE('',*,*,#16754,.F.);
#24285=ORIENTED_EDGE('',*,*,#16755,.F.);
#24286=ORIENTED_EDGE('',*,*,#16756,.F.);
#24287=ORIENTED_EDGE('',*,*,#16751,.T.);
#24288=ORIENTED_EDGE('',*,*,#16757,.F.);
#24289=ORIENTED_EDGE('',*,*,#16758,.F.);
#24290=ORIENTED_EDGE('',*,*,#16759,.F.);
#24291=ORIENTED_EDGE('',*,*,#16760,.F.);
#24292=ORIENTED_EDGE('',*,*,#16761,.F.);
#24293=ORIENTED_EDGE('',*,*,#16755,.T.);
#24294=ORIENTED_EDGE('',*,*,#16762,.F.);
#24295=ORIENTED_EDGE('',*,*,#16763,.F.);
#24296=ORIENTED_EDGE('',*,*,#16764,.F.);
#24297=ORIENTED_EDGE('',*,*,#16765,.F.);
#24298=ORIENTED_EDGE('',*,*,#16759,.T.);
#24299=ORIENTED_EDGE('',*,*,#16766,.F.);
#24300=ORIENTED_EDGE('',*,*,#16767,.F.);
#24301=ORIENTED_EDGE('',*,*,#16768,.F.);
#24302=ORIENTED_EDGE('',*,*,#16769,.F.);
#24303=ORIENTED_EDGE('',*,*,#16764,.T.);
#24304=ORIENTED_EDGE('',*,*,#16770,.F.);
#24305=ORIENTED_EDGE('',*,*,#16771,.F.);
#24306=ORIENTED_EDGE('',*,*,#16772,.F.);
#24307=ORIENTED_EDGE('',*,*,#16773,.F.);
#24308=ORIENTED_EDGE('',*,*,#16767,.T.);
#24309=ORIENTED_EDGE('',*,*,#16774,.F.);
#24310=ORIENTED_EDGE('',*,*,#16775,.F.);
#24311=ORIENTED_EDGE('',*,*,#16776,.F.);
#24312=ORIENTED_EDGE('',*,*,#16777,.F.);
#24313=ORIENTED_EDGE('',*,*,#16772,.T.);
#24314=ORIENTED_EDGE('',*,*,#16778,.F.);
#24315=ORIENTED_EDGE('',*,*,#16779,.F.);
#24316=ORIENTED_EDGE('',*,*,#16780,.F.);
#24317=ORIENTED_EDGE('',*,*,#16781,.F.);
#24318=ORIENTED_EDGE('',*,*,#16775,.T.);
#24319=ORIENTED_EDGE('',*,*,#16782,.F.);
#24320=ORIENTED_EDGE('',*,*,#16783,.F.);
#24321=ORIENTED_EDGE('',*,*,#16784,.F.);
#24322=ORIENTED_EDGE('',*,*,#16785,.F.);
#24323=ORIENTED_EDGE('',*,*,#16786,.F.);
#24324=ORIENTED_EDGE('',*,*,#16780,.T.);
#24325=ORIENTED_EDGE('',*,*,#16787,.F.);
#24326=ORIENTED_EDGE('',*,*,#16788,.F.);
#24327=ORIENTED_EDGE('',*,*,#16789,.F.);
#24328=ORIENTED_EDGE('',*,*,#16790,.F.);
#24329=ORIENTED_EDGE('',*,*,#16784,.T.);
#24330=ORIENTED_EDGE('',*,*,#16791,.F.);
#24331=ORIENTED_EDGE('',*,*,#16792,.F.);
#24332=ORIENTED_EDGE('',*,*,#16793,.F.);
#24333=ORIENTED_EDGE('',*,*,#16794,.F.);
#24334=ORIENTED_EDGE('',*,*,#16789,.T.);
#24335=ORIENTED_EDGE('',*,*,#16795,.F.);
#24336=ORIENTED_EDGE('',*,*,#16796,.F.);
#24337=ORIENTED_EDGE('',*,*,#16797,.F.);
#24338=ORIENTED_EDGE('',*,*,#16798,.F.);
#24339=ORIENTED_EDGE('',*,*,#16799,.F.);
#24340=ORIENTED_EDGE('',*,*,#16792,.T.);
#24341=ORIENTED_EDGE('',*,*,#16800,.F.);
#24342=ORIENTED_EDGE('',*,*,#16801,.F.);
#24343=ORIENTED_EDGE('',*,*,#16802,.F.);
#24344=ORIENTED_EDGE('',*,*,#16803,.F.);
#24345=ORIENTED_EDGE('',*,*,#16797,.T.);
#24346=ORIENTED_EDGE('',*,*,#16804,.F.);
#24347=ORIENTED_EDGE('',*,*,#16805,.F.);
#24348=ORIENTED_EDGE('',*,*,#16806,.F.);
#24349=ORIENTED_EDGE('',*,*,#16807,.F.);
#24350=ORIENTED_EDGE('',*,*,#16801,.T.);
#24351=ORIENTED_EDGE('',*,*,#16808,.F.);
#24352=ORIENTED_EDGE('',*,*,#16809,.F.);
#24353=ORIENTED_EDGE('',*,*,#16810,.F.);
#24354=ORIENTED_EDGE('',*,*,#16811,.F.);
#24355=ORIENTED_EDGE('',*,*,#16812,.F.);
#24356=ORIENTED_EDGE('',*,*,#16806,.T.);
#24357=ORIENTED_EDGE('',*,*,#16813,.F.);
#24358=ORIENTED_EDGE('',*,*,#16814,.F.);
#24359=ORIENTED_EDGE('',*,*,#16815,.F.);
#24360=ORIENTED_EDGE('',*,*,#16816,.F.);
#24361=ORIENTED_EDGE('',*,*,#16810,.T.);
#24362=ORIENTED_EDGE('',*,*,#16817,.F.);
#24363=ORIENTED_EDGE('',*,*,#16818,.F.);
#24364=ORIENTED_EDGE('',*,*,#16819,.F.);
#24365=ORIENTED_EDGE('',*,*,#16820,.F.);
#24366=ORIENTED_EDGE('',*,*,#16815,.T.);
#24367=ORIENTED_EDGE('',*,*,#16821,.F.);
#24368=ORIENTED_EDGE('',*,*,#16822,.F.);
#24369=ORIENTED_EDGE('',*,*,#16823,.F.);
#24370=ORIENTED_EDGE('',*,*,#16824,.F.);
#24371=ORIENTED_EDGE('',*,*,#16825,.F.);
#24372=ORIENTED_EDGE('',*,*,#16818,.T.);
#24373=ORIENTED_EDGE('',*,*,#16826,.F.);
#24374=ORIENTED_EDGE('',*,*,#16827,.F.);
#24375=ORIENTED_EDGE('',*,*,#16828,.F.);
#24376=ORIENTED_EDGE('',*,*,#16829,.F.);
#24377=ORIENTED_EDGE('',*,*,#16823,.T.);
#24378=ORIENTED_EDGE('',*,*,#16830,.F.);
#24379=ORIENTED_EDGE('',*,*,#16831,.F.);
#24380=ORIENTED_EDGE('',*,*,#16832,.F.);
#24381=ORIENTED_EDGE('',*,*,#16833,.F.);
#24382=ORIENTED_EDGE('',*,*,#16827,.T.);
#24383=ORIENTED_EDGE('',*,*,#16834,.F.);
#24384=ORIENTED_EDGE('',*,*,#16835,.F.);
#24385=ORIENTED_EDGE('',*,*,#16836,.F.);
#24386=ORIENTED_EDGE('',*,*,#16837,.F.);
#24387=ORIENTED_EDGE('',*,*,#16832,.T.);
#24388=ORIENTED_EDGE('',*,*,#16838,.F.);
#24389=ORIENTED_EDGE('',*,*,#16839,.F.);
#24390=ORIENTED_EDGE('',*,*,#16840,.F.);
#24391=ORIENTED_EDGE('',*,*,#16841,.F.);
#24392=ORIENTED_EDGE('',*,*,#16835,.T.);
#24393=ORIENTED_EDGE('',*,*,#16842,.F.);
#24394=ORIENTED_EDGE('',*,*,#16843,.F.);
#24395=ORIENTED_EDGE('',*,*,#16844,.F.);
#24396=ORIENTED_EDGE('',*,*,#16845,.F.);
#24397=ORIENTED_EDGE('',*,*,#16840,.T.);
#24398=ORIENTED_EDGE('',*,*,#16846,.F.);
#24399=ORIENTED_EDGE('',*,*,#16847,.F.);
#24400=ORIENTED_EDGE('',*,*,#16848,.F.);
#24401=ORIENTED_EDGE('',*,*,#16849,.F.);
#24402=ORIENTED_EDGE('',*,*,#16850,.F.);
#24403=ORIENTED_EDGE('',*,*,#16843,.T.);
#24404=ORIENTED_EDGE('',*,*,#16851,.F.);
#24405=ORIENTED_EDGE('',*,*,#16852,.F.);
#24406=ORIENTED_EDGE('',*,*,#16853,.F.);
#24407=ORIENTED_EDGE('',*,*,#16848,.T.);
#24408=ORIENTED_EDGE('',*,*,#16854,.F.);
#24409=ORIENTED_EDGE('',*,*,#16855,.F.);
#24410=ORIENTED_EDGE('',*,*,#16856,.F.);
#24411=ORIENTED_EDGE('',*,*,#16857,.F.);
#24412=ORIENTED_EDGE('',*,*,#16858,.F.);
#24413=ORIENTED_EDGE('',*,*,#16852,.T.);
#24414=ORIENTED_EDGE('',*,*,#16859,.F.);
#24415=ORIENTED_EDGE('',*,*,#16860,.F.);
#24416=ORIENTED_EDGE('',*,*,#16861,.F.);
#24417=ORIENTED_EDGE('',*,*,#16862,.F.);
#24418=ORIENTED_EDGE('',*,*,#16863,.F.);
#24419=ORIENTED_EDGE('',*,*,#16864,.T.);
#24420=ORIENTED_EDGE('',*,*,#16865,.F.);
#24421=ORIENTED_EDGE('',*,*,#16866,.F.);
#24422=ORIENTED_EDGE('',*,*,#16867,.F.);
#24423=ORIENTED_EDGE('',*,*,#16868,.F.);
#24424=ORIENTED_EDGE('',*,*,#16869,.F.);
#24425=ORIENTED_EDGE('',*,*,#16861,.T.);
#24426=ORIENTED_EDGE('',*,*,#16870,.F.);
#24427=ORIENTED_EDGE('',*,*,#16871,.F.);
#24428=ORIENTED_EDGE('',*,*,#16872,.F.);
#24429=ORIENTED_EDGE('',*,*,#16867,.T.);
#24430=ORIENTED_EDGE('',*,*,#16873,.F.);
#24431=ORIENTED_EDGE('',*,*,#16874,.F.);
#24432=ORIENTED_EDGE('',*,*,#16875,.F.);
#24433=ORIENTED_EDGE('',*,*,#16876,.F.);
#24434=ORIENTED_EDGE('',*,*,#16877,.F.);
#24435=ORIENTED_EDGE('',*,*,#16871,.T.);
#24436=ORIENTED_EDGE('',*,*,#16878,.F.);
#24437=ORIENTED_EDGE('',*,*,#16879,.F.);
#24438=ORIENTED_EDGE('',*,*,#16880,.F.);
#24439=ORIENTED_EDGE('',*,*,#16881,.F.);
#24440=ORIENTED_EDGE('',*,*,#16875,.T.);
#24441=ORIENTED_EDGE('',*,*,#16882,.F.);
#24442=ORIENTED_EDGE('',*,*,#16883,.F.);
#24443=ORIENTED_EDGE('',*,*,#16884,.F.);
#24444=ORIENTED_EDGE('',*,*,#16885,.F.);
#24445=ORIENTED_EDGE('',*,*,#16880,.T.);
#24446=ORIENTED_EDGE('',*,*,#16886,.F.);
#24447=ORIENTED_EDGE('',*,*,#16887,.F.);
#24448=ORIENTED_EDGE('',*,*,#16888,.F.);
#24449=ORIENTED_EDGE('',*,*,#16889,.F.);
#24450=ORIENTED_EDGE('',*,*,#16883,.T.);
#24451=ORIENTED_EDGE('',*,*,#16890,.F.);
#24452=ORIENTED_EDGE('',*,*,#16891,.F.);
#24453=ORIENTED_EDGE('',*,*,#16892,.F.);
#24454=ORIENTED_EDGE('',*,*,#16893,.F.);
#24455=ORIENTED_EDGE('',*,*,#16888,.T.);
#24456=ORIENTED_EDGE('',*,*,#16894,.F.);
#24457=ORIENTED_EDGE('',*,*,#16895,.F.);
#24458=ORIENTED_EDGE('',*,*,#16896,.F.);
#24459=ORIENTED_EDGE('',*,*,#16897,.F.);
#24460=ORIENTED_EDGE('',*,*,#16891,.T.);
#24461=ORIENTED_EDGE('',*,*,#16898,.F.);
#24462=ORIENTED_EDGE('',*,*,#16899,.F.);
#24463=ORIENTED_EDGE('',*,*,#16900,.F.);
#24464=ORIENTED_EDGE('',*,*,#16901,.F.);
#24465=ORIENTED_EDGE('',*,*,#16902,.F.);
#24466=ORIENTED_EDGE('',*,*,#16896,.T.);
#24467=ORIENTED_EDGE('',*,*,#16903,.F.);
#24468=ORIENTED_EDGE('',*,*,#16904,.F.);
#24469=ORIENTED_EDGE('',*,*,#16905,.F.);
#24470=ORIENTED_EDGE('',*,*,#16906,.F.);
#24471=ORIENTED_EDGE('',*,*,#16900,.T.);
#24472=ORIENTED_EDGE('',*,*,#16907,.F.);
#24473=ORIENTED_EDGE('',*,*,#16908,.F.);
#24474=ORIENTED_EDGE('',*,*,#16909,.F.);
#24475=ORIENTED_EDGE('',*,*,#16910,.F.);
#24476=ORIENTED_EDGE('',*,*,#16905,.T.);
#24477=ORIENTED_EDGE('',*,*,#16911,.F.);
#24478=ORIENTED_EDGE('',*,*,#16912,.F.);
#24479=ORIENTED_EDGE('',*,*,#16913,.F.);
#24480=ORIENTED_EDGE('',*,*,#16914,.F.);
#24481=ORIENTED_EDGE('',*,*,#16915,.F.);
#24482=ORIENTED_EDGE('',*,*,#16908,.T.);
#24483=ORIENTED_EDGE('',*,*,#16916,.F.);
#24484=ORIENTED_EDGE('',*,*,#16917,.F.);
#24485=ORIENTED_EDGE('',*,*,#16918,.F.);
#24486=ORIENTED_EDGE('',*,*,#16919,.F.);
#24487=ORIENTED_EDGE('',*,*,#16913,.T.);
#24488=ORIENTED_EDGE('',*,*,#16920,.F.);
#24489=ORIENTED_EDGE('',*,*,#16921,.F.);
#24490=ORIENTED_EDGE('',*,*,#16922,.F.);
#24491=ORIENTED_EDGE('',*,*,#16923,.F.);
#24492=ORIENTED_EDGE('',*,*,#16917,.T.);
#24493=ORIENTED_EDGE('',*,*,#16924,.F.);
#24494=ORIENTED_EDGE('',*,*,#16925,.F.);
#24495=ORIENTED_EDGE('',*,*,#16926,.F.);
#24496=ORIENTED_EDGE('',*,*,#16927,.F.);
#24497=ORIENTED_EDGE('',*,*,#16928,.F.);
#24498=ORIENTED_EDGE('',*,*,#16922,.T.);
#24499=ORIENTED_EDGE('',*,*,#16929,.F.);
#24500=ORIENTED_EDGE('',*,*,#16930,.F.);
#24501=ORIENTED_EDGE('',*,*,#16931,.F.);
#24502=ORIENTED_EDGE('',*,*,#16932,.F.);
#24503=ORIENTED_EDGE('',*,*,#16926,.T.);
#24504=ORIENTED_EDGE('',*,*,#16933,.F.);
#24505=ORIENTED_EDGE('',*,*,#16934,.F.);
#24506=ORIENTED_EDGE('',*,*,#16935,.F.);
#24507=ORIENTED_EDGE('',*,*,#16936,.F.);
#24508=ORIENTED_EDGE('',*,*,#16931,.T.);
#24509=ORIENTED_EDGE('',*,*,#16937,.F.);
#24510=ORIENTED_EDGE('',*,*,#16938,.F.);
#24511=ORIENTED_EDGE('',*,*,#16939,.F.);
#24512=ORIENTED_EDGE('',*,*,#16940,.F.);
#24513=ORIENTED_EDGE('',*,*,#16941,.F.);
#24514=ORIENTED_EDGE('',*,*,#16934,.T.);
#24515=ORIENTED_EDGE('',*,*,#16942,.F.);
#24516=ORIENTED_EDGE('',*,*,#16943,.F.);
#24517=ORIENTED_EDGE('',*,*,#16944,.F.);
#24518=ORIENTED_EDGE('',*,*,#16945,.F.);
#24519=ORIENTED_EDGE('',*,*,#16939,.T.);
#24520=ORIENTED_EDGE('',*,*,#16946,.F.);
#24521=ORIENTED_EDGE('',*,*,#16947,.F.);
#24522=ORIENTED_EDGE('',*,*,#16948,.F.);
#24523=ORIENTED_EDGE('',*,*,#16949,.F.);
#24524=ORIENTED_EDGE('',*,*,#16943,.T.);
#24525=ORIENTED_EDGE('',*,*,#16950,.F.);
#24526=ORIENTED_EDGE('',*,*,#16951,.F.);
#24527=ORIENTED_EDGE('',*,*,#16952,.F.);
#24528=ORIENTED_EDGE('',*,*,#16953,.F.);
#24529=ORIENTED_EDGE('',*,*,#16948,.T.);
#24530=ORIENTED_EDGE('',*,*,#16954,.F.);
#24531=ORIENTED_EDGE('',*,*,#16955,.F.);
#24532=ORIENTED_EDGE('',*,*,#16956,.F.);
#24533=ORIENTED_EDGE('',*,*,#16957,.F.);
#24534=ORIENTED_EDGE('',*,*,#16951,.T.);
#24535=ORIENTED_EDGE('',*,*,#16958,.F.);
#24536=ORIENTED_EDGE('',*,*,#16959,.F.);
#24537=ORIENTED_EDGE('',*,*,#16960,.F.);
#24538=ORIENTED_EDGE('',*,*,#16961,.F.);
#24539=ORIENTED_EDGE('',*,*,#16956,.T.);
#24540=ORIENTED_EDGE('',*,*,#16962,.F.);
#24541=ORIENTED_EDGE('',*,*,#16963,.F.);
#24542=ORIENTED_EDGE('',*,*,#16964,.F.);
#24543=ORIENTED_EDGE('',*,*,#16965,.F.);
#24544=ORIENTED_EDGE('',*,*,#16966,.F.);
#24545=ORIENTED_EDGE('',*,*,#16959,.T.);
#24546=ORIENTED_EDGE('',*,*,#16967,.F.);
#24547=ORIENTED_EDGE('',*,*,#16968,.F.);
#24548=ORIENTED_EDGE('',*,*,#16969,.F.);
#24549=ORIENTED_EDGE('',*,*,#16964,.T.);
#24550=ORIENTED_EDGE('',*,*,#16970,.F.);
#24551=ORIENTED_EDGE('',*,*,#16971,.F.);
#24552=ORIENTED_EDGE('',*,*,#16972,.F.);
#24553=ORIENTED_EDGE('',*,*,#16973,.F.);
#24554=ORIENTED_EDGE('',*,*,#16974,.F.);
#24555=ORIENTED_EDGE('',*,*,#16968,.T.);
#24556=ORIENTED_EDGE('',*,*,#16975,.F.);
#24557=ORIENTED_EDGE('',*,*,#16976,.F.);
#24558=ORIENTED_EDGE('',*,*,#16977,.F.);
#24559=ORIENTED_EDGE('',*,*,#16978,.F.);
#24560=ORIENTED_EDGE('',*,*,#16979,.F.);
#24561=ORIENTED_EDGE('',*,*,#16980,.T.);
#24562=ORIENTED_EDGE('',*,*,#16981,.F.);
#24563=ORIENTED_EDGE('',*,*,#16982,.F.);
#24564=ORIENTED_EDGE('',*,*,#16983,.F.);
#24565=ORIENTED_EDGE('',*,*,#16984,.F.);
#24566=ORIENTED_EDGE('',*,*,#16985,.F.);
#24567=ORIENTED_EDGE('',*,*,#16977,.T.);
#24568=ORIENTED_EDGE('',*,*,#16986,.F.);
#24569=ORIENTED_EDGE('',*,*,#16987,.F.);
#24570=ORIENTED_EDGE('',*,*,#16988,.F.);
#24571=ORIENTED_EDGE('',*,*,#16983,.T.);
#24572=ORIENTED_EDGE('',*,*,#16989,.F.);
#24573=ORIENTED_EDGE('',*,*,#16990,.F.);
#24574=ORIENTED_EDGE('',*,*,#16991,.F.);
#24575=ORIENTED_EDGE('',*,*,#16992,.F.);
#24576=ORIENTED_EDGE('',*,*,#16993,.F.);
#24577=ORIENTED_EDGE('',*,*,#16987,.T.);
#24578=ORIENTED_EDGE('',*,*,#16994,.F.);
#24579=ORIENTED_EDGE('',*,*,#16995,.F.);
#24580=ORIENTED_EDGE('',*,*,#16996,.F.);
#24581=ORIENTED_EDGE('',*,*,#16997,.F.);
#24582=ORIENTED_EDGE('',*,*,#16991,.T.);
#24583=ORIENTED_EDGE('',*,*,#16998,.F.);
#24584=ORIENTED_EDGE('',*,*,#16999,.F.);
#24585=ORIENTED_EDGE('',*,*,#17000,.F.);
#24586=ORIENTED_EDGE('',*,*,#17001,.F.);
#24587=ORIENTED_EDGE('',*,*,#16996,.T.);
#24588=ORIENTED_EDGE('',*,*,#17002,.F.);
#24589=ORIENTED_EDGE('',*,*,#17003,.F.);
#24590=ORIENTED_EDGE('',*,*,#17004,.F.);
#24591=ORIENTED_EDGE('',*,*,#17005,.F.);
#24592=ORIENTED_EDGE('',*,*,#16999,.T.);
#24593=ORIENTED_EDGE('',*,*,#17006,.F.);
#24594=ORIENTED_EDGE('',*,*,#17007,.F.);
#24595=ORIENTED_EDGE('',*,*,#17008,.F.);
#24596=ORIENTED_EDGE('',*,*,#17009,.F.);
#24597=ORIENTED_EDGE('',*,*,#17004,.T.);
#24598=ORIENTED_EDGE('',*,*,#17010,.F.);
#24599=ORIENTED_EDGE('',*,*,#17011,.F.);
#24600=ORIENTED_EDGE('',*,*,#17012,.F.);
#24601=ORIENTED_EDGE('',*,*,#17013,.F.);
#24602=ORIENTED_EDGE('',*,*,#17007,.T.);
#24603=ORIENTED_EDGE('',*,*,#17014,.F.);
#24604=ORIENTED_EDGE('',*,*,#17015,.F.);
#24605=ORIENTED_EDGE('',*,*,#17016,.F.);
#24606=ORIENTED_EDGE('',*,*,#17017,.F.);
#24607=ORIENTED_EDGE('',*,*,#17018,.F.);
#24608=ORIENTED_EDGE('',*,*,#17012,.T.);
#24609=ORIENTED_EDGE('',*,*,#17019,.F.);
#24610=ORIENTED_EDGE('',*,*,#17020,.F.);
#24611=ORIENTED_EDGE('',*,*,#17021,.F.);
#24612=ORIENTED_EDGE('',*,*,#17022,.F.);
#24613=ORIENTED_EDGE('',*,*,#17016,.T.);
#24614=ORIENTED_EDGE('',*,*,#17023,.F.);
#24615=ORIENTED_EDGE('',*,*,#17024,.F.);
#24616=ORIENTED_EDGE('',*,*,#17025,.F.);
#24617=ORIENTED_EDGE('',*,*,#17026,.F.);
#24618=ORIENTED_EDGE('',*,*,#17021,.T.);
#24619=ORIENTED_EDGE('',*,*,#17027,.F.);
#24620=ORIENTED_EDGE('',*,*,#17028,.F.);
#24621=ORIENTED_EDGE('',*,*,#17029,.F.);
#24622=ORIENTED_EDGE('',*,*,#17030,.F.);
#24623=ORIENTED_EDGE('',*,*,#17031,.F.);
#24624=ORIENTED_EDGE('',*,*,#17024,.T.);
#24625=ORIENTED_EDGE('',*,*,#17032,.F.);
#24626=ORIENTED_EDGE('',*,*,#17033,.F.);
#24627=ORIENTED_EDGE('',*,*,#17034,.F.);
#24628=ORIENTED_EDGE('',*,*,#17035,.F.);
#24629=ORIENTED_EDGE('',*,*,#17029,.T.);
#24630=ORIENTED_EDGE('',*,*,#17036,.F.);
#24631=ORIENTED_EDGE('',*,*,#17037,.F.);
#24632=ORIENTED_EDGE('',*,*,#17038,.F.);
#24633=ORIENTED_EDGE('',*,*,#17039,.F.);
#24634=ORIENTED_EDGE('',*,*,#17033,.T.);
#24635=ORIENTED_EDGE('',*,*,#17040,.F.);
#24636=ORIENTED_EDGE('',*,*,#17041,.F.);
#24637=ORIENTED_EDGE('',*,*,#17042,.F.);
#24638=ORIENTED_EDGE('',*,*,#17043,.F.);
#24639=ORIENTED_EDGE('',*,*,#17044,.F.);
#24640=ORIENTED_EDGE('',*,*,#17038,.T.);
#24641=ORIENTED_EDGE('',*,*,#17045,.F.);
#24642=ORIENTED_EDGE('',*,*,#17046,.F.);
#24643=ORIENTED_EDGE('',*,*,#17047,.F.);
#24644=ORIENTED_EDGE('',*,*,#17048,.F.);
#24645=ORIENTED_EDGE('',*,*,#17042,.T.);
#24646=ORIENTED_EDGE('',*,*,#17049,.F.);
#24647=ORIENTED_EDGE('',*,*,#17050,.F.);
#24648=ORIENTED_EDGE('',*,*,#17051,.F.);
#24649=ORIENTED_EDGE('',*,*,#17052,.F.);
#24650=ORIENTED_EDGE('',*,*,#17047,.T.);
#24651=ORIENTED_EDGE('',*,*,#17053,.F.);
#24652=ORIENTED_EDGE('',*,*,#17054,.F.);
#24653=ORIENTED_EDGE('',*,*,#17055,.F.);
#24654=ORIENTED_EDGE('',*,*,#17056,.F.);
#24655=ORIENTED_EDGE('',*,*,#17057,.F.);
#24656=ORIENTED_EDGE('',*,*,#17050,.T.);
#24657=ORIENTED_EDGE('',*,*,#17058,.F.);
#24658=ORIENTED_EDGE('',*,*,#17059,.F.);
#24659=ORIENTED_EDGE('',*,*,#17060,.F.);
#24660=ORIENTED_EDGE('',*,*,#17061,.F.);
#24661=ORIENTED_EDGE('',*,*,#17055,.T.);
#24662=ORIENTED_EDGE('',*,*,#17062,.F.);
#24663=ORIENTED_EDGE('',*,*,#17063,.F.);
#24664=ORIENTED_EDGE('',*,*,#17064,.F.);
#24665=ORIENTED_EDGE('',*,*,#17065,.F.);
#24666=ORIENTED_EDGE('',*,*,#17059,.T.);
#24667=ORIENTED_EDGE('',*,*,#17066,.F.);
#24668=ORIENTED_EDGE('',*,*,#17067,.F.);
#24669=ORIENTED_EDGE('',*,*,#17068,.F.);
#24670=ORIENTED_EDGE('',*,*,#17069,.F.);
#24671=ORIENTED_EDGE('',*,*,#17064,.T.);
#24672=ORIENTED_EDGE('',*,*,#17070,.F.);
#24673=ORIENTED_EDGE('',*,*,#17071,.F.);
#24674=ORIENTED_EDGE('',*,*,#17072,.F.);
#24675=ORIENTED_EDGE('',*,*,#17073,.F.);
#24676=ORIENTED_EDGE('',*,*,#17067,.T.);
#24677=ORIENTED_EDGE('',*,*,#17074,.F.);
#24678=ORIENTED_EDGE('',*,*,#17075,.F.);
#24679=ORIENTED_EDGE('',*,*,#17076,.F.);
#24680=ORIENTED_EDGE('',*,*,#17077,.F.);
#24681=ORIENTED_EDGE('',*,*,#17072,.T.);
#24682=ORIENTED_EDGE('',*,*,#17078,.F.);
#24683=ORIENTED_EDGE('',*,*,#17079,.F.);
#24684=ORIENTED_EDGE('',*,*,#17080,.F.);
#24685=ORIENTED_EDGE('',*,*,#17081,.F.);
#24686=ORIENTED_EDGE('',*,*,#17082,.F.);
#24687=ORIENTED_EDGE('',*,*,#17075,.T.);
#24688=ORIENTED_EDGE('',*,*,#17083,.F.);
#24689=ORIENTED_EDGE('',*,*,#17084,.F.);
#24690=ORIENTED_EDGE('',*,*,#17085,.F.);
#24691=ORIENTED_EDGE('',*,*,#17080,.T.);
#24692=ORIENTED_EDGE('',*,*,#17086,.F.);
#24693=ORIENTED_EDGE('',*,*,#17087,.F.);
#24694=ORIENTED_EDGE('',*,*,#17088,.F.);
#24695=ORIENTED_EDGE('',*,*,#17089,.F.);
#24696=ORIENTED_EDGE('',*,*,#17090,.F.);
#24697=ORIENTED_EDGE('',*,*,#17084,.T.);
#24698=ORIENTED_EDGE('',*,*,#17091,.F.);
#24699=ORIENTED_EDGE('',*,*,#17092,.F.);
#24700=ORIENTED_EDGE('',*,*,#17093,.F.);
#24701=ORIENTED_EDGE('',*,*,#17094,.F.);
#24702=ORIENTED_EDGE('',*,*,#17095,.F.);
#24703=ORIENTED_EDGE('',*,*,#17096,.T.);
#24704=ORIENTED_EDGE('',*,*,#17097,.F.);
#24705=ORIENTED_EDGE('',*,*,#17098,.F.);
#24706=ORIENTED_EDGE('',*,*,#17099,.F.);
#24707=ORIENTED_EDGE('',*,*,#17100,.F.);
#24708=ORIENTED_EDGE('',*,*,#17101,.F.);
#24709=ORIENTED_EDGE('',*,*,#17093,.T.);
#24710=ORIENTED_EDGE('',*,*,#17102,.F.);
#24711=ORIENTED_EDGE('',*,*,#17103,.F.);
#24712=ORIENTED_EDGE('',*,*,#17104,.F.);
#24713=ORIENTED_EDGE('',*,*,#17099,.T.);
#24714=ORIENTED_EDGE('',*,*,#17105,.F.);
#24715=ORIENTED_EDGE('',*,*,#17106,.F.);
#24716=ORIENTED_EDGE('',*,*,#17107,.F.);
#24717=ORIENTED_EDGE('',*,*,#17108,.F.);
#24718=ORIENTED_EDGE('',*,*,#17109,.F.);
#24719=ORIENTED_EDGE('',*,*,#17103,.T.);
#24720=ORIENTED_EDGE('',*,*,#17110,.F.);
#24721=ORIENTED_EDGE('',*,*,#17111,.F.);
#24722=ORIENTED_EDGE('',*,*,#17112,.F.);
#24723=ORIENTED_EDGE('',*,*,#17113,.F.);
#24724=ORIENTED_EDGE('',*,*,#17107,.T.);
#24725=ORIENTED_EDGE('',*,*,#17114,.F.);
#24726=ORIENTED_EDGE('',*,*,#17115,.F.);
#24727=ORIENTED_EDGE('',*,*,#17116,.F.);
#24728=ORIENTED_EDGE('',*,*,#17117,.F.);
#24729=ORIENTED_EDGE('',*,*,#17112,.T.);
#24730=ORIENTED_EDGE('',*,*,#17118,.F.);
#24731=ORIENTED_EDGE('',*,*,#17119,.F.);
#24732=ORIENTED_EDGE('',*,*,#17120,.F.);
#24733=ORIENTED_EDGE('',*,*,#17121,.F.);
#24734=ORIENTED_EDGE('',*,*,#17115,.T.);
#24735=ORIENTED_EDGE('',*,*,#17122,.F.);
#24736=ORIENTED_EDGE('',*,*,#17123,.F.);
#24737=ORIENTED_EDGE('',*,*,#17124,.F.);
#24738=ORIENTED_EDGE('',*,*,#17125,.F.);
#24739=ORIENTED_EDGE('',*,*,#17120,.T.);
#24740=ORIENTED_EDGE('',*,*,#17126,.F.);
#24741=ORIENTED_EDGE('',*,*,#17127,.F.);
#24742=ORIENTED_EDGE('',*,*,#17128,.F.);
#24743=ORIENTED_EDGE('',*,*,#17129,.F.);
#24744=ORIENTED_EDGE('',*,*,#17123,.T.);
#24745=ORIENTED_EDGE('',*,*,#17130,.F.);
#24746=ORIENTED_EDGE('',*,*,#17131,.F.);
#24747=ORIENTED_EDGE('',*,*,#17132,.F.);
#24748=ORIENTED_EDGE('',*,*,#17133,.F.);
#24749=ORIENTED_EDGE('',*,*,#17134,.F.);
#24750=ORIENTED_EDGE('',*,*,#17128,.T.);
#24751=ORIENTED_EDGE('',*,*,#17135,.F.);
#24752=ORIENTED_EDGE('',*,*,#17136,.F.);
#24753=ORIENTED_EDGE('',*,*,#17137,.F.);
#24754=ORIENTED_EDGE('',*,*,#17138,.F.);
#24755=ORIENTED_EDGE('',*,*,#17132,.T.);
#24756=ORIENTED_EDGE('',*,*,#17139,.F.);
#24757=ORIENTED_EDGE('',*,*,#17140,.F.);
#24758=ORIENTED_EDGE('',*,*,#17141,.F.);
#24759=ORIENTED_EDGE('',*,*,#17142,.F.);
#24760=ORIENTED_EDGE('',*,*,#17137,.T.);
#24761=ORIENTED_EDGE('',*,*,#17143,.F.);
#24762=ORIENTED_EDGE('',*,*,#17144,.F.);
#24763=ORIENTED_EDGE('',*,*,#17145,.F.);
#24764=ORIENTED_EDGE('',*,*,#17146,.F.);
#24765=ORIENTED_EDGE('',*,*,#17147,.F.);
#24766=ORIENTED_EDGE('',*,*,#17140,.T.);
#24767=ORIENTED_EDGE('',*,*,#17148,.F.);
#24768=ORIENTED_EDGE('',*,*,#17149,.F.);
#24769=ORIENTED_EDGE('',*,*,#17150,.F.);
#24770=ORIENTED_EDGE('',*,*,#17151,.F.);
#24771=ORIENTED_EDGE('',*,*,#17145,.T.);
#24772=ORIENTED_EDGE('',*,*,#17152,.F.);
#24773=ORIENTED_EDGE('',*,*,#17153,.F.);
#24774=ORIENTED_EDGE('',*,*,#17154,.F.);
#24775=ORIENTED_EDGE('',*,*,#17155,.F.);
#24776=ORIENTED_EDGE('',*,*,#17149,.T.);
#24777=ORIENTED_EDGE('',*,*,#17156,.F.);
#24778=ORIENTED_EDGE('',*,*,#17157,.F.);
#24779=ORIENTED_EDGE('',*,*,#17158,.F.);
#24780=ORIENTED_EDGE('',*,*,#17159,.F.);
#24781=ORIENTED_EDGE('',*,*,#17160,.F.);
#24782=ORIENTED_EDGE('',*,*,#17154,.T.);
#24783=ORIENTED_EDGE('',*,*,#17161,.F.);
#24784=ORIENTED_EDGE('',*,*,#17162,.F.);
#24785=ORIENTED_EDGE('',*,*,#17163,.F.);
#24786=ORIENTED_EDGE('',*,*,#17164,.F.);
#24787=ORIENTED_EDGE('',*,*,#17158,.T.);
#24788=ORIENTED_EDGE('',*,*,#17165,.F.);
#24789=ORIENTED_EDGE('',*,*,#17166,.F.);
#24790=ORIENTED_EDGE('',*,*,#17167,.F.);
#24791=ORIENTED_EDGE('',*,*,#17168,.F.);
#24792=ORIENTED_EDGE('',*,*,#17163,.T.);
#24793=ORIENTED_EDGE('',*,*,#17169,.F.);
#24794=ORIENTED_EDGE('',*,*,#17170,.F.);
#24795=ORIENTED_EDGE('',*,*,#17171,.F.);
#24796=ORIENTED_EDGE('',*,*,#17172,.F.);
#24797=ORIENTED_EDGE('',*,*,#17173,.F.);
#24798=ORIENTED_EDGE('',*,*,#17166,.T.);
#24799=ORIENTED_EDGE('',*,*,#17174,.F.);
#24800=ORIENTED_EDGE('',*,*,#17175,.F.);
#24801=ORIENTED_EDGE('',*,*,#17176,.F.);
#24802=ORIENTED_EDGE('',*,*,#17177,.F.);
#24803=ORIENTED_EDGE('',*,*,#17171,.T.);
#24804=ORIENTED_EDGE('',*,*,#17178,.F.);
#24805=ORIENTED_EDGE('',*,*,#17179,.F.);
#24806=ORIENTED_EDGE('',*,*,#17180,.F.);
#24807=ORIENTED_EDGE('',*,*,#17181,.F.);
#24808=ORIENTED_EDGE('',*,*,#17175,.T.);
#24809=ORIENTED_EDGE('',*,*,#17182,.F.);
#24810=ORIENTED_EDGE('',*,*,#17183,.F.);
#24811=ORIENTED_EDGE('',*,*,#17184,.F.);
#24812=ORIENTED_EDGE('',*,*,#17185,.F.);
#24813=ORIENTED_EDGE('',*,*,#17180,.T.);
#24814=ORIENTED_EDGE('',*,*,#17186,.F.);
#24815=ORIENTED_EDGE('',*,*,#17187,.F.);
#24816=ORIENTED_EDGE('',*,*,#17188,.F.);
#24817=ORIENTED_EDGE('',*,*,#17189,.F.);
#24818=ORIENTED_EDGE('',*,*,#17183,.T.);
#24819=ORIENTED_EDGE('',*,*,#17190,.F.);
#24820=ORIENTED_EDGE('',*,*,#17191,.F.);
#24821=ORIENTED_EDGE('',*,*,#17192,.F.);
#24822=ORIENTED_EDGE('',*,*,#17193,.F.);
#24823=ORIENTED_EDGE('',*,*,#17188,.T.);
#24824=ORIENTED_EDGE('',*,*,#17194,.F.);
#24825=ORIENTED_EDGE('',*,*,#17195,.F.);
#24826=ORIENTED_EDGE('',*,*,#17196,.F.);
#24827=ORIENTED_EDGE('',*,*,#17197,.F.);
#24828=ORIENTED_EDGE('',*,*,#17198,.F.);
#24829=ORIENTED_EDGE('',*,*,#17191,.T.);
#24830=ORIENTED_EDGE('',*,*,#17199,.F.);
#24831=ORIENTED_EDGE('',*,*,#17200,.F.);
#24832=ORIENTED_EDGE('',*,*,#17201,.F.);
#24833=ORIENTED_EDGE('',*,*,#17196,.T.);
#24834=ORIENTED_EDGE('',*,*,#17202,.F.);
#24835=ORIENTED_EDGE('',*,*,#17203,.F.);
#24836=ORIENTED_EDGE('',*,*,#17204,.F.);
#24837=ORIENTED_EDGE('',*,*,#17205,.F.);
#24838=ORIENTED_EDGE('',*,*,#17206,.F.);
#24839=ORIENTED_EDGE('',*,*,#17200,.T.);
#24840=ORIENTED_EDGE('',*,*,#17207,.F.);
#24841=ORIENTED_EDGE('',*,*,#17208,.F.);
#24842=ORIENTED_EDGE('',*,*,#17204,.T.);
#24843=ORIENTED_EDGE('',*,*,#17209,.F.);
#24844=ORIENTED_EDGE('',*,*,#17210,.T.);
#24845=ORIENTED_EDGE('',*,*,#17211,.F.);
#24846=ORIENTED_EDGE('',*,*,#17088,.T.);
#24847=ORIENTED_EDGE('',*,*,#17212,.F.);
#24848=ORIENTED_EDGE('',*,*,#17213,.T.);
#24849=ORIENTED_EDGE('',*,*,#17214,.F.);
#24850=ORIENTED_EDGE('',*,*,#16972,.T.);
#24851=ORIENTED_EDGE('',*,*,#17215,.F.);
#24852=ORIENTED_EDGE('',*,*,#17216,.T.);
#24853=ORIENTED_EDGE('',*,*,#17217,.F.);
#24854=ORIENTED_EDGE('',*,*,#16856,.T.);
#24855=ORIENTED_EDGE('',*,*,#17218,.F.);
#24856=ORIENTED_EDGE('',*,*,#17219,.T.);
#24857=ORIENTED_EDGE('',*,*,#17220,.F.);
#24858=ORIENTED_EDGE('',*,*,#16741,.T.);
#24859=ORIENTED_EDGE('',*,*,#17221,.F.);
#24860=ORIENTED_EDGE('',*,*,#17222,.F.);
#24861=ORIENTED_EDGE('',*,*,#16728,.T.);
#24862=ORIENTED_EDGE('',*,*,#17223,.F.);
#24863=ORIENTED_EDGE('',*,*,#17224,.F.);
#24864=ORIENTED_EDGE('',*,*,#17225,.F.);
#24865=ORIENTED_EDGE('',*,*,#16713,.T.);
#24866=ORIENTED_EDGE('',*,*,#17226,.T.);
#24867=ORIENTED_EDGE('',*,*,#17227,.T.);
#24868=ORIENTED_EDGE('',*,*,#17228,.T.);
#24869=ORIENTED_EDGE('',*,*,#17229,.F.);
#24870=ORIENTED_EDGE('',*,*,#17230,.F.);
#24871=ORIENTED_EDGE('',*,*,#16577,.T.);
#24872=ORIENTED_EDGE('',*,*,#17231,.T.);
#24873=ORIENTED_EDGE('',*,*,#17232,.T.);
#24874=ORIENTED_EDGE('',*,*,#17233,.T.);
#24875=ORIENTED_EDGE('',*,*,#17234,.F.);
#24876=ORIENTED_EDGE('',*,*,#17235,.F.);
#24877=ORIENTED_EDGE('',*,*,#16441,.T.);
#24878=ORIENTED_EDGE('',*,*,#17236,.T.);
#24879=ORIENTED_EDGE('',*,*,#17237,.T.);
#24880=ORIENTED_EDGE('',*,*,#17238,.T.);
#24881=ORIENTED_EDGE('',*,*,#17239,.F.);
#24882=ORIENTED_EDGE('',*,*,#17240,.F.);
#24883=ORIENTED_EDGE('',*,*,#16305,.T.);
#24884=ORIENTED_EDGE('',*,*,#17241,.T.);
#24885=ORIENTED_EDGE('',*,*,#17242,.T.);
#24886=ORIENTED_EDGE('',*,*,#17243,.T.);
#24887=ORIENTED_EDGE('',*,*,#17244,.F.);
#24888=ORIENTED_EDGE('',*,*,#17245,.F.);
#24889=ORIENTED_EDGE('',*,*,#16169,.T.);
#24890=ORIENTED_EDGE('',*,*,#17246,.T.);
#24891=ORIENTED_EDGE('',*,*,#17247,.T.);
#24892=ORIENTED_EDGE('',*,*,#17248,.T.);
#24893=ORIENTED_EDGE('',*,*,#17249,.F.);
#24894=ORIENTED_EDGE('',*,*,#17250,.F.);
#24895=ORIENTED_EDGE('',*,*,#16150,.T.);
#24896=ORIENTED_EDGE('',*,*,#17251,.T.);
#24897=ORIENTED_EDGE('',*,*,#17252,.T.);
#24898=ORIENTED_EDGE('',*,*,#17253,.T.);
#24899=ORIENTED_EDGE('',*,*,#17254,.F.);
#24900=ORIENTED_EDGE('',*,*,#17255,.F.);
#24901=ORIENTED_EDGE('',*,*,#17256,.F.);
#24902=ORIENTED_EDGE('',*,*,#17257,.T.);
#24903=ORIENTED_EDGE('',*,*,#17258,.T.);
#24904=ORIENTED_EDGE('',*,*,#17257,.F.);
#24905=ORIENTED_EDGE('',*,*,#17256,.T.);
#24906=ORIENTED_EDGE('',*,*,#17259,.T.);
#24907=ORIENTED_EDGE('',*,*,#17260,.T.);
#24908=ORIENTED_EDGE('',*,*,#17261,.F.);
#24909=ORIENTED_EDGE('',*,*,#17262,.T.);
#24910=ORIENTED_EDGE('',*,*,#17263,.T.);
#24911=ORIENTED_EDGE('',*,*,#17264,.T.);
#24912=ORIENTED_EDGE('',*,*,#17265,.T.);
#24913=ORIENTED_EDGE('',*,*,#17266,.T.);
#24914=ORIENTED_EDGE('',*,*,#17261,.T.);
#24915=ORIENTED_EDGE('',*,*,#17267,.F.);
#24916=ORIENTED_EDGE('',*,*,#17268,.T.);
#24917=ORIENTED_EDGE('',*,*,#17269,.T.);
#24918=ORIENTED_EDGE('',*,*,#17268,.F.);
#24919=ORIENTED_EDGE('',*,*,#17267,.T.);
#24920=ORIENTED_EDGE('',*,*,#17270,.T.);
#24921=ORIENTED_EDGE('',*,*,#17271,.T.);
#24922=ORIENTED_EDGE('',*,*,#17272,.F.);
#24923=ORIENTED_EDGE('',*,*,#17273,.T.);
#24924=ORIENTED_EDGE('',*,*,#17274,.T.);
#24925=ORIENTED_EDGE('',*,*,#17275,.T.);
#24926=ORIENTED_EDGE('',*,*,#17276,.T.);
#24927=ORIENTED_EDGE('',*,*,#17272,.T.);
#24928=ORIENTED_EDGE('',*,*,#17277,.T.);
#24929=ORIENTED_EDGE('',*,*,#17278,.F.);
#24930=ORIENTED_EDGE('',*,*,#17279,.T.);
#24931=ORIENTED_EDGE('',*,*,#17280,.T.);
#24932=ORIENTED_EDGE('',*,*,#17279,.F.);
#24933=ORIENTED_EDGE('',*,*,#17278,.T.);
#24934=ORIENTED_EDGE('',*,*,#17265,.F.);
#24935=ORIENTED_EDGE('',*,*,#17281,.F.);
#24936=ORIENTED_EDGE('',*,*,#17282,.F.);
#24937=ORIENTED_EDGE('',*,*,#17283,.T.);
#24938=ORIENTED_EDGE('',*,*,#17276,.F.);
#24939=ORIENTED_EDGE('',*,*,#17284,.F.);
#24940=ORIENTED_EDGE('',*,*,#17285,.T.);
#24941=ORIENTED_EDGE('',*,*,#17286,.T.);
#24942=ORIENTED_EDGE('',*,*,#17287,.T.);
#24943=ORIENTED_EDGE('',*,*,#17273,.F.);
#24944=ORIENTED_EDGE('',*,*,#17266,.F.);
#24945=ORIENTED_EDGE('',*,*,#17283,.F.);
#24946=ORIENTED_EDGE('',*,*,#17288,.T.);
#24947=ORIENTED_EDGE('',*,*,#17289,.T.);
#24948=ORIENTED_EDGE('',*,*,#17277,.F.);
#24949=ORIENTED_EDGE('',*,*,#17271,.F.);
#24950=ORIENTED_EDGE('',*,*,#17290,.T.);
#24951=ORIENTED_EDGE('',*,*,#17262,.F.);
#24952=ORIENTED_EDGE('',*,*,#17259,.F.);
#24953=ORIENTED_EDGE('',*,*,#17290,.F.);
#24954=ORIENTED_EDGE('',*,*,#17270,.F.);
#24955=ORIENTED_EDGE('',*,*,#17287,.F.);
#24956=ORIENTED_EDGE('',*,*,#17291,.F.);
#24957=ORIENTED_EDGE('',*,*,#17292,.F.);
#24958=ORIENTED_EDGE('',*,*,#17293,.F.);
#24959=ORIENTED_EDGE('',*,*,#17294,.F.);
#24960=ORIENTED_EDGE('',*,*,#17295,.F.);
#24961=ORIENTED_EDGE('',*,*,#17296,.F.);
#24962=ORIENTED_EDGE('',*,*,#17297,.F.);
#24963=ORIENTED_EDGE('',*,*,#17298,.F.);
#24964=ORIENTED_EDGE('',*,*,#17299,.F.);
#24965=ORIENTED_EDGE('',*,*,#17300,.F.);
#24966=ORIENTED_EDGE('',*,*,#17301,.F.);
#24967=ORIENTED_EDGE('',*,*,#17302,.F.);
#24968=ORIENTED_EDGE('',*,*,#17303,.F.);
#24969=ORIENTED_EDGE('',*,*,#17304,.F.);
#24970=ORIENTED_EDGE('',*,*,#17305,.F.);
#24971=ORIENTED_EDGE('',*,*,#17306,.F.);
#24972=ORIENTED_EDGE('',*,*,#17307,.F.);
#24973=ORIENTED_EDGE('',*,*,#17308,.F.);
#24974=ORIENTED_EDGE('',*,*,#17309,.F.);
#24975=ORIENTED_EDGE('',*,*,#17310,.F.);
#24976=ORIENTED_EDGE('',*,*,#17311,.F.);
#24977=ORIENTED_EDGE('',*,*,#17312,.F.);
#24978=ORIENTED_EDGE('',*,*,#17313,.F.);
#24979=ORIENTED_EDGE('',*,*,#17314,.F.);
#24980=ORIENTED_EDGE('',*,*,#17315,.F.);
#24981=ORIENTED_EDGE('',*,*,#17316,.F.);
#24982=ORIENTED_EDGE('',*,*,#17317,.F.);
#24983=ORIENTED_EDGE('',*,*,#17318,.F.);
#24984=ORIENTED_EDGE('',*,*,#17319,.F.);
#24985=ORIENTED_EDGE('',*,*,#17320,.F.);
#24986=ORIENTED_EDGE('',*,*,#17321,.F.);
#24987=ORIENTED_EDGE('',*,*,#17210,.F.);
#24988=ORIENTED_EDGE('',*,*,#17322,.F.);
#24989=ORIENTED_EDGE('',*,*,#17243,.F.);
#24990=ORIENTED_EDGE('',*,*,#17323,.F.);
#24991=ORIENTED_EDGE('',*,*,#17213,.F.);
#24992=ORIENTED_EDGE('',*,*,#17324,.F.);
#24993=ORIENTED_EDGE('',*,*,#17238,.F.);
#24994=ORIENTED_EDGE('',*,*,#17325,.F.);
#24995=ORIENTED_EDGE('',*,*,#17216,.F.);
#24996=ORIENTED_EDGE('',*,*,#17326,.F.);
#24997=ORIENTED_EDGE('',*,*,#17233,.F.);
#24998=ORIENTED_EDGE('',*,*,#17327,.F.);
#24999=ORIENTED_EDGE('',*,*,#17219,.F.);
#25000=ORIENTED_EDGE('',*,*,#17328,.F.);
#25001=ORIENTED_EDGE('',*,*,#17228,.F.);
#25002=ORIENTED_EDGE('',*,*,#17280,.F.);
#25003=ORIENTED_EDGE('',*,*,#17269,.F.);
#25004=ORIENTED_EDGE('',*,*,#17258,.F.);
#25005=ORIENTED_EDGE('',*,*,#17329,.T.);
#25006=ORIENTED_EDGE('',*,*,#17221,.T.);
#25007=ORIENTED_EDGE('',*,*,#16744,.T.);
#25008=ORIENTED_EDGE('',*,*,#16740,.T.);
#25009=ORIENTED_EDGE('',*,*,#16737,.T.);
#25010=ORIENTED_EDGE('',*,*,#16734,.T.);
#25011=ORIENTED_EDGE('',*,*,#17330,.T.);
#25012=ORIENTED_EDGE('',*,*,#16137,.T.);
#25013=ORIENTED_EDGE('',*,*,#16142,.T.);
#25014=ORIENTED_EDGE('',*,*,#16141,.T.);
#25015=ORIENTED_EDGE('',*,*,#16147,.T.);
#25016=ORIENTED_EDGE('',*,*,#16146,.T.);
#25017=ORIENTED_EDGE('',*,*,#16152,.T.);
#25018=ORIENTED_EDGE('',*,*,#16151,.T.);
#25019=ORIENTED_EDGE('',*,*,#17255,.T.);
#25020=ORIENTED_EDGE('',*,*,#17254,.T.);
#25021=ORIENTED_EDGE('',*,*,#17331,.T.);
#25022=ORIENTED_EDGE('',*,*,#17252,.F.);
#25023=ORIENTED_EDGE('',*,*,#17251,.F.);
#25024=ORIENTED_EDGE('',*,*,#16154,.F.);
#25025=ORIENTED_EDGE('',*,*,#16153,.F.);
#25026=ORIENTED_EDGE('',*,*,#16149,.F.);
#25027=ORIENTED_EDGE('',*,*,#16148,.F.);
#25028=ORIENTED_EDGE('',*,*,#16144,.F.);
#25029=ORIENTED_EDGE('',*,*,#16143,.F.);
#25030=ORIENTED_EDGE('',*,*,#16139,.F.);
#25031=ORIENTED_EDGE('',*,*,#17332,.T.);
#25032=ORIENTED_EDGE('',*,*,#16732,.T.);
#25033=ORIENTED_EDGE('',*,*,#16736,.T.);
#25034=ORIENTED_EDGE('',*,*,#16739,.T.);
#25035=ORIENTED_EDGE('',*,*,#16743,.T.);
#25036=ORIENTED_EDGE('',*,*,#17333,.T.);
#25037=ORIENTED_EDGE('',*,*,#16719,.T.);
#25038=ORIENTED_EDGE('',*,*,#16722,.T.);
#25039=ORIENTED_EDGE('',*,*,#16726,.T.);
#25040=ORIENTED_EDGE('',*,*,#16729,.T.);
#25041=ORIENTED_EDGE('',*,*,#17225,.T.);
#25042=ORIENTED_EDGE('',*,*,#17334,.T.);
#25043=ORIENTED_EDGE('',*,*,#16156,.T.);
#25044=ORIENTED_EDGE('',*,*,#16161,.T.);
#25045=ORIENTED_EDGE('',*,*,#16160,.T.);
#25046=ORIENTED_EDGE('',*,*,#16166,.T.);
#25047=ORIENTED_EDGE('',*,*,#16165,.T.);
#25048=ORIENTED_EDGE('',*,*,#16171,.T.);
#25049=ORIENTED_EDGE('',*,*,#16170,.T.);
#25050=ORIENTED_EDGE('',*,*,#17250,.T.);
#25051=ORIENTED_EDGE('',*,*,#17249,.T.);
#25052=ORIENTED_EDGE('',*,*,#17335,.T.);
#25053=ORIENTED_EDGE('',*,*,#17247,.F.);
#25054=ORIENTED_EDGE('',*,*,#17246,.F.);
#25055=ORIENTED_EDGE('',*,*,#16173,.F.);
#25056=ORIENTED_EDGE('',*,*,#16172,.F.);
#25057=ORIENTED_EDGE('',*,*,#16168,.F.);
#25058=ORIENTED_EDGE('',*,*,#16167,.F.);
#25059=ORIENTED_EDGE('',*,*,#16163,.F.);
#25060=ORIENTED_EDGE('',*,*,#16162,.F.);
#25061=ORIENTED_EDGE('',*,*,#16158,.F.);
#25062=ORIENTED_EDGE('',*,*,#17336,.T.);
#25063=ORIENTED_EDGE('',*,*,#17223,.T.);
#25064=ORIENTED_EDGE('',*,*,#16730,.T.);
#25065=ORIENTED_EDGE('',*,*,#16727,.T.);
#25066=ORIENTED_EDGE('',*,*,#16724,.T.);
#25067=ORIENTED_EDGE('',*,*,#17322,.T.);
#25068=ORIENTED_EDGE('',*,*,#17209,.T.);
#25069=ORIENTED_EDGE('',*,*,#17208,.T.);
#25070=ORIENTED_EDGE('',*,*,#17207,.T.);
#25071=ORIENTED_EDGE('',*,*,#17203,.T.);
#25072=ORIENTED_EDGE('',*,*,#17202,.T.);
#25073=ORIENTED_EDGE('',*,*,#17199,.T.);
#25074=ORIENTED_EDGE('',*,*,#17195,.T.);
#25075=ORIENTED_EDGE('',*,*,#17194,.T.);
#25076=ORIENTED_EDGE('',*,*,#17190,.T.);
#25077=ORIENTED_EDGE('',*,*,#17187,.T.);
#25078=ORIENTED_EDGE('',*,*,#17186,.T.);
#25079=ORIENTED_EDGE('',*,*,#17182,.T.);
#25080=ORIENTED_EDGE('',*,*,#17179,.T.);
#25081=ORIENTED_EDGE('',*,*,#17178,.T.);
#25082=ORIENTED_EDGE('',*,*,#17174,.T.);
#25083=ORIENTED_EDGE('',*,*,#17170,.T.);
#25084=ORIENTED_EDGE('',*,*,#17169,.T.);
#25085=ORIENTED_EDGE('',*,*,#17165,.T.);
#25086=ORIENTED_EDGE('',*,*,#17162,.T.);
#25087=ORIENTED_EDGE('',*,*,#17161,.T.);
#25088=ORIENTED_EDGE('',*,*,#17157,.T.);
#25089=ORIENTED_EDGE('',*,*,#17156,.T.);
#25090=ORIENTED_EDGE('',*,*,#17153,.T.);
#25091=ORIENTED_EDGE('',*,*,#17152,.T.);
#25092=ORIENTED_EDGE('',*,*,#17148,.T.);
#25093=ORIENTED_EDGE('',*,*,#17144,.T.);
#25094=ORIENTED_EDGE('',*,*,#17143,.T.);
#25095=ORIENTED_EDGE('',*,*,#17139,.T.);
#25096=ORIENTED_EDGE('',*,*,#17136,.T.);
#25097=ORIENTED_EDGE('',*,*,#17135,.T.);
#25098=ORIENTED_EDGE('',*,*,#17131,.T.);
#25099=ORIENTED_EDGE('',*,*,#17130,.T.);
#25100=ORIENTED_EDGE('',*,*,#17127,.T.);
#25101=ORIENTED_EDGE('',*,*,#17126,.T.);
#25102=ORIENTED_EDGE('',*,*,#17122,.T.);
#25103=ORIENTED_EDGE('',*,*,#17119,.T.);
#25104=ORIENTED_EDGE('',*,*,#17118,.T.);
#25105=ORIENTED_EDGE('',*,*,#17114,.T.);
#25106=ORIENTED_EDGE('',*,*,#17111,.T.);
#25107=ORIENTED_EDGE('',*,*,#17110,.T.);
#25108=ORIENTED_EDGE('',*,*,#17106,.T.);
#25109=ORIENTED_EDGE('',*,*,#17105,.T.);
#25110=ORIENTED_EDGE('',*,*,#17102,.T.);
#25111=ORIENTED_EDGE('',*,*,#17098,.T.);
#25112=ORIENTED_EDGE('',*,*,#17097,.T.);
#25113=ORIENTED_EDGE('',*,*,#17337,.T.);
#25114=ORIENTED_EDGE('',*,*,#16176,.T.);
#25115=ORIENTED_EDGE('',*,*,#16175,.T.);
#25116=ORIENTED_EDGE('',*,*,#16182,.T.);
#25117=ORIENTED_EDGE('',*,*,#16181,.T.);
#25118=ORIENTED_EDGE('',*,*,#16187,.T.);
#25119=ORIENTED_EDGE('',*,*,#16186,.T.);
#25120=ORIENTED_EDGE('',*,*,#16192,.T.);
#25121=ORIENTED_EDGE('',*,*,#16191,.T.);
#25122=ORIENTED_EDGE('',*,*,#16197,.T.);
#25123=ORIENTED_EDGE('',*,*,#16196,.T.);
#25124=ORIENTED_EDGE('',*,*,#16202,.T.);
#25125=ORIENTED_EDGE('',*,*,#16201,.T.);
#25126=ORIENTED_EDGE('',*,*,#16207,.T.);
#25127=ORIENTED_EDGE('',*,*,#16206,.T.);
#25128=ORIENTED_EDGE('',*,*,#16212,.T.);
#25129=ORIENTED_EDGE('',*,*,#16211,.T.);
#25130=ORIENTED_EDGE('',*,*,#16217,.T.);
#25131=ORIENTED_EDGE('',*,*,#16216,.T.);
#25132=ORIENTED_EDGE('',*,*,#16222,.T.);
#25133=ORIENTED_EDGE('',*,*,#16221,.T.);
#25134=ORIENTED_EDGE('',*,*,#16227,.T.);
#25135=ORIENTED_EDGE('',*,*,#16226,.T.);
#25136=ORIENTED_EDGE('',*,*,#16232,.T.);
#25137=ORIENTED_EDGE('',*,*,#16231,.T.);
#25138=ORIENTED_EDGE('',*,*,#16237,.T.);
#25139=ORIENTED_EDGE('',*,*,#16236,.T.);
#25140=ORIENTED_EDGE('',*,*,#16242,.T.);
#25141=ORIENTED_EDGE('',*,*,#16241,.T.);
#25142=ORIENTED_EDGE('',*,*,#16247,.T.);
#25143=ORIENTED_EDGE('',*,*,#16246,.T.);
#25144=ORIENTED_EDGE('',*,*,#16252,.T.);
#25145=ORIENTED_EDGE('',*,*,#16251,.T.);
#25146=ORIENTED_EDGE('',*,*,#16257,.T.);
#25147=ORIENTED_EDGE('',*,*,#16256,.T.);
#25148=ORIENTED_EDGE('',*,*,#16262,.T.);
#25149=ORIENTED_EDGE('',*,*,#16261,.T.);
#25150=ORIENTED_EDGE('',*,*,#16267,.T.);
#25151=ORIENTED_EDGE('',*,*,#16266,.T.);
#25152=ORIENTED_EDGE('',*,*,#16272,.T.);
#25153=ORIENTED_EDGE('',*,*,#16271,.T.);
#25154=ORIENTED_EDGE('',*,*,#16277,.T.);
#25155=ORIENTED_EDGE('',*,*,#16276,.T.);
#25156=ORIENTED_EDGE('',*,*,#16282,.T.);
#25157=ORIENTED_EDGE('',*,*,#16281,.T.);
#25158=ORIENTED_EDGE('',*,*,#16287,.T.);
#25159=ORIENTED_EDGE('',*,*,#16286,.T.);
#25160=ORIENTED_EDGE('',*,*,#16292,.T.);
#25161=ORIENTED_EDGE('',*,*,#16291,.T.);
#25162=ORIENTED_EDGE('',*,*,#16297,.T.);
#25163=ORIENTED_EDGE('',*,*,#16296,.T.);
#25164=ORIENTED_EDGE('',*,*,#16302,.T.);
#25165=ORIENTED_EDGE('',*,*,#16301,.T.);
#25166=ORIENTED_EDGE('',*,*,#16307,.T.);
#25167=ORIENTED_EDGE('',*,*,#16306,.T.);
#25168=ORIENTED_EDGE('',*,*,#17245,.T.);
#25169=ORIENTED_EDGE('',*,*,#17244,.T.);
#25170=ORIENTED_EDGE('',*,*,#17321,.T.);
#25171=ORIENTED_EDGE('',*,*,#17242,.F.);
#25172=ORIENTED_EDGE('',*,*,#17241,.F.);
#25173=ORIENTED_EDGE('',*,*,#16309,.F.);
#25174=ORIENTED_EDGE('',*,*,#16308,.F.);
#25175=ORIENTED_EDGE('',*,*,#16304,.F.);
#25176=ORIENTED_EDGE('',*,*,#16303,.F.);
#25177=ORIENTED_EDGE('',*,*,#16299,.F.);
#25178=ORIENTED_EDGE('',*,*,#16298,.F.);
#25179=ORIENTED_EDGE('',*,*,#16294,.F.);
#25180=ORIENTED_EDGE('',*,*,#16293,.F.);
#25181=ORIENTED_EDGE('',*,*,#16289,.F.);
#25182=ORIENTED_EDGE('',*,*,#16288,.F.);
#25183=ORIENTED_EDGE('',*,*,#16284,.F.);
#25184=ORIENTED_EDGE('',*,*,#16283,.F.);
#25185=ORIENTED_EDGE('',*,*,#16279,.F.);
#25186=ORIENTED_EDGE('',*,*,#16278,.F.);
#25187=ORIENTED_EDGE('',*,*,#16274,.F.);
#25188=ORIENTED_EDGE('',*,*,#16273,.F.);
#25189=ORIENTED_EDGE('',*,*,#16269,.F.);
#25190=ORIENTED_EDGE('',*,*,#16268,.F.);
#25191=ORIENTED_EDGE('',*,*,#16264,.F.);
#25192=ORIENTED_EDGE('',*,*,#16263,.F.);
#25193=ORIENTED_EDGE('',*,*,#16259,.F.);
#25194=ORIENTED_EDGE('',*,*,#16258,.F.);
#25195=ORIENTED_EDGE('',*,*,#16254,.F.);
#25196=ORIENTED_EDGE('',*,*,#16253,.F.);
#25197=ORIENTED_EDGE('',*,*,#16249,.F.);
#25198=ORIENTED_EDGE('',*,*,#16248,.F.);
#25199=ORIENTED_EDGE('',*,*,#16244,.F.);
#25200=ORIENTED_EDGE('',*,*,#16243,.F.);
#25201=ORIENTED_EDGE('',*,*,#16239,.F.);
#25202=ORIENTED_EDGE('',*,*,#16238,.F.);
#25203=ORIENTED_EDGE('',*,*,#16234,.F.);
#25204=ORIENTED_EDGE('',*,*,#16233,.F.);
#25205=ORIENTED_EDGE('',*,*,#16229,.F.);
#25206=ORIENTED_EDGE('',*,*,#16228,.F.);
#25207=ORIENTED_EDGE('',*,*,#16224,.F.);
#25208=ORIENTED_EDGE('',*,*,#16223,.F.);
#25209=ORIENTED_EDGE('',*,*,#16219,.F.);
#25210=ORIENTED_EDGE('',*,*,#16218,.F.);
#25211=ORIENTED_EDGE('',*,*,#16214,.F.);
#25212=ORIENTED_EDGE('',*,*,#16213,.F.);
#25213=ORIENTED_EDGE('',*,*,#16209,.F.);
#25214=ORIENTED_EDGE('',*,*,#16208,.F.);
#25215=ORIENTED_EDGE('',*,*,#16204,.F.);
#25216=ORIENTED_EDGE('',*,*,#16203,.F.);
#25217=ORIENTED_EDGE('',*,*,#16199,.F.);
#25218=ORIENTED_EDGE('',*,*,#16198,.F.);
#25219=ORIENTED_EDGE('',*,*,#16194,.F.);
#25220=ORIENTED_EDGE('',*,*,#16193,.F.);
#25221=ORIENTED_EDGE('',*,*,#16189,.F.);
#25222=ORIENTED_EDGE('',*,*,#16188,.F.);
#25223=ORIENTED_EDGE('',*,*,#16184,.F.);
#25224=ORIENTED_EDGE('',*,*,#16183,.F.);
#25225=ORIENTED_EDGE('',*,*,#16179,.F.);
#25226=ORIENTED_EDGE('',*,*,#16178,.F.);
#25227=ORIENTED_EDGE('',*,*,#17338,.T.);
#25228=ORIENTED_EDGE('',*,*,#17095,.T.);
#25229=ORIENTED_EDGE('',*,*,#17094,.T.);
#25230=ORIENTED_EDGE('',*,*,#17101,.T.);
#25231=ORIENTED_EDGE('',*,*,#17100,.T.);
#25232=ORIENTED_EDGE('',*,*,#17104,.T.);
#25233=ORIENTED_EDGE('',*,*,#17109,.T.);
#25234=ORIENTED_EDGE('',*,*,#17108,.T.);
#25235=ORIENTED_EDGE('',*,*,#17113,.T.);
#25236=ORIENTED_EDGE('',*,*,#17117,.T.);
#25237=ORIENTED_EDGE('',*,*,#17116,.T.);
#25238=ORIENTED_EDGE('',*,*,#17121,.T.);
#25239=ORIENTED_EDGE('',*,*,#17125,.T.);
#25240=ORIENTED_EDGE('',*,*,#17124,.T.);
#25241=ORIENTED_EDGE('',*,*,#17129,.T.);
#25242=ORIENTED_EDGE('',*,*,#17134,.T.);
#25243=ORIENTED_EDGE('',*,*,#17133,.T.);
#25244=ORIENTED_EDGE('',*,*,#17138,.T.);
#25245=ORIENTED_EDGE('',*,*,#17142,.T.);
#25246=ORIENTED_EDGE('',*,*,#17141,.T.);
#25247=ORIENTED_EDGE('',*,*,#17147,.T.);
#25248=ORIENTED_EDGE('',*,*,#17146,.T.);
#25249=ORIENTED_EDGE('',*,*,#17151,.T.);
#25250=ORIENTED_EDGE('',*,*,#17150,.T.);
#25251=ORIENTED_EDGE('',*,*,#17155,.T.);
#25252=ORIENTED_EDGE('',*,*,#17160,.T.);
#25253=ORIENTED_EDGE('',*,*,#17159,.T.);
#25254=ORIENTED_EDGE('',*,*,#17164,.T.);
#25255=ORIENTED_EDGE('',*,*,#17168,.T.);
#25256=ORIENTED_EDGE('',*,*,#17167,.T.);
#25257=ORIENTED_EDGE('',*,*,#17173,.T.);
#25258=ORIENTED_EDGE('',*,*,#17172,.T.);
#25259=ORIENTED_EDGE('',*,*,#17177,.T.);
#25260=ORIENTED_EDGE('',*,*,#17176,.T.);
#25261=ORIENTED_EDGE('',*,*,#17181,.T.);
#25262=ORIENTED_EDGE('',*,*,#17185,.T.);
#25263=ORIENTED_EDGE('',*,*,#17184,.T.);
#25264=ORIENTED_EDGE('',*,*,#17189,.T.);
#25265=ORIENTED_EDGE('',*,*,#17193,.T.);
#25266=ORIENTED_EDGE('',*,*,#17192,.T.);
#25267=ORIENTED_EDGE('',*,*,#17198,.T.);
#25268=ORIENTED_EDGE('',*,*,#17197,.T.);
#25269=ORIENTED_EDGE('',*,*,#17201,.T.);
#25270=ORIENTED_EDGE('',*,*,#17206,.T.);
#25271=ORIENTED_EDGE('',*,*,#17205,.T.);
#25272=ORIENTED_EDGE('',*,*,#17211,.T.);
#25273=ORIENTED_EDGE('',*,*,#17324,.T.);
#25274=ORIENTED_EDGE('',*,*,#17212,.T.);
#25275=ORIENTED_EDGE('',*,*,#17092,.T.);
#25276=ORIENTED_EDGE('',*,*,#17091,.T.);
#25277=ORIENTED_EDGE('',*,*,#17087,.T.);
#25278=ORIENTED_EDGE('',*,*,#17086,.T.);
#25279=ORIENTED_EDGE('',*,*,#17083,.T.);
#25280=ORIENTED_EDGE('',*,*,#17079,.T.);
#25281=ORIENTED_EDGE('',*,*,#17078,.T.);
#25282=ORIENTED_EDGE('',*,*,#17074,.T.);
#25283=ORIENTED_EDGE('',*,*,#17071,.T.);
#25284=ORIENTED_EDGE('',*,*,#17070,.T.);
#25285=ORIENTED_EDGE('',*,*,#17066,.T.);
#25286=ORIENTED_EDGE('',*,*,#17063,.T.);
#25287=ORIENTED_EDGE('',*,*,#17062,.T.);
#25288=ORIENTED_EDGE('',*,*,#17058,.T.);
#25289=ORIENTED_EDGE('',*,*,#17054,.T.);
#25290=ORIENTED_EDGE('',*,*,#17053,.T.);
#25291=ORIENTED_EDGE('',*,*,#17049,.T.);
#25292=ORIENTED_EDGE('',*,*,#17046,.T.);
#25293=ORIENTED_EDGE('',*,*,#17045,.T.);
#25294=ORIENTED_EDGE('',*,*,#17041,.T.);
#25295=ORIENTED_EDGE('',*,*,#17040,.T.);
#25296=ORIENTED_EDGE('',*,*,#17037,.T.);
#25297=ORIENTED_EDGE('',*,*,#17036,.T.);
#25298=ORIENTED_EDGE('',*,*,#17032,.T.);
#25299=ORIENTED_EDGE('',*,*,#17028,.T.);
#25300=ORIENTED_EDGE('',*,*,#17027,.T.);
#25301=ORIENTED_EDGE('',*,*,#17023,.T.);
#25302=ORIENTED_EDGE('',*,*,#17020,.T.);
#25303=ORIENTED_EDGE('',*,*,#17019,.T.);
#25304=ORIENTED_EDGE('',*,*,#17015,.T.);
#25305=ORIENTED_EDGE('',*,*,#17014,.T.);
#25306=ORIENTED_EDGE('',*,*,#17011,.T.);
#25307=ORIENTED_EDGE('',*,*,#17010,.T.);
#25308=ORIENTED_EDGE('',*,*,#17006,.T.);
#25309=ORIENTED_EDGE('',*,*,#17003,.T.);
#25310=ORIENTED_EDGE('',*,*,#17002,.T.);
#25311=ORIENTED_EDGE('',*,*,#16998,.T.);
#25312=ORIENTED_EDGE('',*,*,#16995,.T.);
#25313=ORIENTED_EDGE('',*,*,#16994,.T.);
#25314=ORIENTED_EDGE('',*,*,#16990,.T.);
#25315=ORIENTED_EDGE('',*,*,#16989,.T.);
#25316=ORIENTED_EDGE('',*,*,#16986,.T.);
#25317=ORIENTED_EDGE('',*,*,#16982,.T.);
#25318=ORIENTED_EDGE('',*,*,#16981,.T.);
#25319=ORIENTED_EDGE('',*,*,#17339,.T.);
#25320=ORIENTED_EDGE('',*,*,#16312,.T.);
#25321=ORIENTED_EDGE('',*,*,#16311,.T.);
#25322=ORIENTED_EDGE('',*,*,#16318,.T.);
#25323=ORIENTED_EDGE('',*,*,#16317,.T.);
#25324=ORIENTED_EDGE('',*,*,#16323,.T.);
#25325=ORIENTED_EDGE('',*,*,#16322,.T.);
#25326=ORIENTED_EDGE('',*,*,#16328,.T.);
#25327=ORIENTED_EDGE('',*,*,#16327,.T.);
#25328=ORIENTED_EDGE('',*,*,#16333,.T.);
#25329=ORIENTED_EDGE('',*,*,#16332,.T.);
#25330=ORIENTED_EDGE('',*,*,#16338,.T.);
#25331=ORIENTED_EDGE('',*,*,#16337,.T.);
#25332=ORIENTED_EDGE('',*,*,#16343,.T.);
#25333=ORIENTED_EDGE('',*,*,#16342,.T.);
#25334=ORIENTED_EDGE('',*,*,#16348,.T.);
#25335=ORIENTED_EDGE('',*,*,#16347,.T.);
#25336=ORIENTED_EDGE('',*,*,#16353,.T.);
#25337=ORIENTED_EDGE('',*,*,#16352,.T.);
#25338=ORIENTED_EDGE('',*,*,#16358,.T.);
#25339=ORIENTED_EDGE('',*,*,#16357,.T.);
#25340=ORIENTED_EDGE('',*,*,#16363,.T.);
#25341=ORIENTED_EDGE('',*,*,#16362,.T.);
#25342=ORIENTED_EDGE('',*,*,#16368,.T.);
#25343=ORIENTED_EDGE('',*,*,#16367,.T.);
#25344=ORIENTED_EDGE('',*,*,#16373,.T.);
#25345=ORIENTED_EDGE('',*,*,#16372,.T.);
#25346=ORIENTED_EDGE('',*,*,#16378,.T.);
#25347=ORIENTED_EDGE('',*,*,#16377,.T.);
#25348=ORIENTED_EDGE('',*,*,#16383,.T.);
#25349=ORIENTED_EDGE('',*,*,#16382,.T.);
#25350=ORIENTED_EDGE('',*,*,#16388,.T.);
#25351=ORIENTED_EDGE('',*,*,#16387,.T.);
#25352=ORIENTED_EDGE('',*,*,#16393,.T.);
#25353=ORIENTED_EDGE('',*,*,#16392,.T.);
#25354=ORIENTED_EDGE('',*,*,#16398,.T.);
#25355=ORIENTED_EDGE('',*,*,#16397,.T.);
#25356=ORIENTED_EDGE('',*,*,#16403,.T.);
#25357=ORIENTED_EDGE('',*,*,#16402,.T.);
#25358=ORIENTED_EDGE('',*,*,#16408,.T.);
#25359=ORIENTED_EDGE('',*,*,#16407,.T.);
#25360=ORIENTED_EDGE('',*,*,#16413,.T.);
#25361=ORIENTED_EDGE('',*,*,#16412,.T.);
#25362=ORIENTED_EDGE('',*,*,#16418,.T.);
#25363=ORIENTED_EDGE('',*,*,#16417,.T.);
#25364=ORIENTED_EDGE('',*,*,#16423,.T.);
#25365=ORIENTED_EDGE('',*,*,#16422,.T.);
#25366=ORIENTED_EDGE('',*,*,#16428,.T.);
#25367=ORIENTED_EDGE('',*,*,#16427,.T.);
#25368=ORIENTED_EDGE('',*,*,#16433,.T.);
#25369=ORIENTED_EDGE('',*,*,#16432,.T.);
#25370=ORIENTED_EDGE('',*,*,#16438,.T.);
#25371=ORIENTED_EDGE('',*,*,#16437,.T.);
#25372=ORIENTED_EDGE('',*,*,#16443,.T.);
#25373=ORIENTED_EDGE('',*,*,#16442,.T.);
#25374=ORIENTED_EDGE('',*,*,#17240,.T.);
#25375=ORIENTED_EDGE('',*,*,#17239,.T.);
#25376=ORIENTED_EDGE('',*,*,#17323,.T.);
#25377=ORIENTED_EDGE('',*,*,#17237,.F.);
#25378=ORIENTED_EDGE('',*,*,#17236,.F.);
#25379=ORIENTED_EDGE('',*,*,#16445,.F.);
#25380=ORIENTED_EDGE('',*,*,#16444,.F.);
#25381=ORIENTED_EDGE('',*,*,#16440,.F.);
#25382=ORIENTED_EDGE('',*,*,#16439,.F.);
#25383=ORIENTED_EDGE('',*,*,#16435,.F.);
#25384=ORIENTED_EDGE('',*,*,#16434,.F.);
#25385=ORIENTED_EDGE('',*,*,#16430,.F.);
#25386=ORIENTED_EDGE('',*,*,#16429,.F.);
#25387=ORIENTED_EDGE('',*,*,#16425,.F.);
#25388=ORIENTED_EDGE('',*,*,#16424,.F.);
#25389=ORIENTED_EDGE('',*,*,#16420,.F.);
#25390=ORIENTED_EDGE('',*,*,#16419,.F.);
#25391=ORIENTED_EDGE('',*,*,#16415,.F.);
#25392=ORIENTED_EDGE('',*,*,#16414,.F.);
#25393=ORIENTED_EDGE('',*,*,#16410,.F.);
#25394=ORIENTED_EDGE('',*,*,#16409,.F.);
#25395=ORIENTED_EDGE('',*,*,#16405,.F.);
#25396=ORIENTED_EDGE('',*,*,#16404,.F.);
#25397=ORIENTED_EDGE('',*,*,#16400,.F.);
#25398=ORIENTED_EDGE('',*,*,#16399,.F.);
#25399=ORIENTED_EDGE('',*,*,#16395,.F.);
#25400=ORIENTED_EDGE('',*,*,#16394,.F.);
#25401=ORIENTED_EDGE('',*,*,#16390,.F.);
#25402=ORIENTED_EDGE('',*,*,#16389,.F.);
#25403=ORIENTED_EDGE('',*,*,#16385,.F.);
#25404=ORIENTED_EDGE('',*,*,#16384,.F.);
#25405=ORIENTED_EDGE('',*,*,#16380,.F.);
#25406=ORIENTED_EDGE('',*,*,#16379,.F.);
#25407=ORIENTED_EDGE('',*,*,#16375,.F.);
#25408=ORIENTED_EDGE('',*,*,#16374,.F.);
#25409=ORIENTED_EDGE('',*,*,#16370,.F.);
#25410=ORIENTED_EDGE('',*,*,#16369,.F.);
#25411=ORIENTED_EDGE('',*,*,#16365,.F.);
#25412=ORIENTED_EDGE('',*,*,#16364,.F.);
#25413=ORIENTED_EDGE('',*,*,#16360,.F.);
#25414=ORIENTED_EDGE('',*,*,#16359,.F.);
#25415=ORIENTED_EDGE('',*,*,#16355,.F.);
#25416=ORIENTED_EDGE('',*,*,#16354,.F.);
#25417=ORIENTED_EDGE('',*,*,#16350,.F.);
#25418=ORIENTED_EDGE('',*,*,#16349,.F.);
#25419=ORIENTED_EDGE('',*,*,#16345,.F.);
#25420=ORIENTED_EDGE('',*,*,#16344,.F.);
#25421=ORIENTED_EDGE('',*,*,#16340,.F.);
#25422=ORIENTED_EDGE('',*,*,#16339,.F.);
#25423=ORIENTED_EDGE('',*,*,#16335,.F.);
#25424=ORIENTED_EDGE('',*,*,#16334,.F.);
#25425=ORIENTED_EDGE('',*,*,#16330,.F.);
#25426=ORIENTED_EDGE('',*,*,#16329,.F.);
#25427=ORIENTED_EDGE('',*,*,#16325,.F.);
#25428=ORIENTED_EDGE('',*,*,#16324,.F.);
#25429=ORIENTED_EDGE('',*,*,#16320,.F.);
#25430=ORIENTED_EDGE('',*,*,#16319,.F.);
#25431=ORIENTED_EDGE('',*,*,#16315,.F.);
#25432=ORIENTED_EDGE('',*,*,#16314,.F.);
#25433=ORIENTED_EDGE('',*,*,#17340,.T.);
#25434=ORIENTED_EDGE('',*,*,#16979,.T.);
#25435=ORIENTED_EDGE('',*,*,#16978,.T.);
#25436=ORIENTED_EDGE('',*,*,#16985,.T.);
#25437=ORIENTED_EDGE('',*,*,#16984,.T.);
#25438=ORIENTED_EDGE('',*,*,#16988,.T.);
#25439=ORIENTED_EDGE('',*,*,#16993,.T.);
#25440=ORIENTED_EDGE('',*,*,#16992,.T.);
#25441=ORIENTED_EDGE('',*,*,#16997,.T.);
#25442=ORIENTED_EDGE('',*,*,#17001,.T.);
#25443=ORIENTED_EDGE('',*,*,#17000,.T.);
#25444=ORIENTED_EDGE('',*,*,#17005,.T.);
#25445=ORIENTED_EDGE('',*,*,#17009,.T.);
#25446=ORIENTED_EDGE('',*,*,#17008,.T.);
#25447=ORIENTED_EDGE('',*,*,#17013,.T.);
#25448=ORIENTED_EDGE('',*,*,#17018,.T.);
#25449=ORIENTED_EDGE('',*,*,#17017,.T.);
#25450=ORIENTED_EDGE('',*,*,#17022,.T.);
#25451=ORIENTED_EDGE('',*,*,#17026,.T.);
#25452=ORIENTED_EDGE('',*,*,#17025,.T.);
#25453=ORIENTED_EDGE('',*,*,#17031,.T.);
#25454=ORIENTED_EDGE('',*,*,#17030,.T.);
#25455=ORIENTED_EDGE('',*,*,#17035,.T.);
#25456=ORIENTED_EDGE('',*,*,#17034,.T.);
#25457=ORIENTED_EDGE('',*,*,#17039,.T.);
#25458=ORIENTED_EDGE('',*,*,#17044,.T.);
#25459=ORIENTED_EDGE('',*,*,#17043,.T.);
#25460=ORIENTED_EDGE('',*,*,#17048,.T.);
#25461=ORIENTED_EDGE('',*,*,#17052,.T.);
#25462=ORIENTED_EDGE('',*,*,#17051,.T.);
#25463=ORIENTED_EDGE('',*,*,#17057,.T.);
#25464=ORIENTED_EDGE('',*,*,#17056,.T.);
#25465=ORIENTED_EDGE('',*,*,#17061,.T.);
#25466=ORIENTED_EDGE('',*,*,#17060,.T.);
#25467=ORIENTED_EDGE('',*,*,#17065,.T.);
#25468=ORIENTED_EDGE('',*,*,#17069,.T.);
#25469=ORIENTED_EDGE('',*,*,#17068,.T.);
#25470=ORIENTED_EDGE('',*,*,#17073,.T.);
#25471=ORIENTED_EDGE('',*,*,#17077,.T.);
#25472=ORIENTED_EDGE('',*,*,#17076,.T.);
#25473=ORIENTED_EDGE('',*,*,#17082,.T.);
#25474=ORIENTED_EDGE('',*,*,#17081,.T.);
#25475=ORIENTED_EDGE('',*,*,#17085,.T.);
#25476=ORIENTED_EDGE('',*,*,#17090,.T.);
#25477=ORIENTED_EDGE('',*,*,#17089,.T.);
#25478=ORIENTED_EDGE('',*,*,#17214,.T.);
#25479=ORIENTED_EDGE('',*,*,#17326,.T.);
#25480=ORIENTED_EDGE('',*,*,#17215,.T.);
#25481=ORIENTED_EDGE('',*,*,#16976,.T.);
#25482=ORIENTED_EDGE('',*,*,#16975,.T.);
#25483=ORIENTED_EDGE('',*,*,#16971,.T.);
#25484=ORIENTED_EDGE('',*,*,#16970,.T.);
#25485=ORIENTED_EDGE('',*,*,#16967,.T.);
#25486=ORIENTED_EDGE('',*,*,#16963,.T.);
#25487=ORIENTED_EDGE('',*,*,#16962,.T.);
#25488=ORIENTED_EDGE('',*,*,#16958,.T.);
#25489=ORIENTED_EDGE('',*,*,#16955,.T.);
#25490=ORIENTED_EDGE('',*,*,#16954,.T.);
#25491=ORIENTED_EDGE('',*,*,#16950,.T.);
#25492=ORIENTED_EDGE('',*,*,#16947,.T.);
#25493=ORIENTED_EDGE('',*,*,#16946,.T.);
#25494=ORIENTED_EDGE('',*,*,#16942,.T.);
#25495=ORIENTED_EDGE('',*,*,#16938,.T.);
#25496=ORIENTED_EDGE('',*,*,#16937,.T.);
#25497=ORIENTED_EDGE('',*,*,#16933,.T.);
#25498=ORIENTED_EDGE('',*,*,#16930,.T.);
#25499=ORIENTED_EDGE('',*,*,#16929,.T.);
#25500=ORIENTED_EDGE('',*,*,#16925,.T.);
#25501=ORIENTED_EDGE('',*,*,#16924,.T.);
#25502=ORIENTED_EDGE('',*,*,#16921,.T.);
#25503=ORIENTED_EDGE('',*,*,#16920,.T.);
#25504=ORIENTED_EDGE('',*,*,#16916,.T.);
#25505=ORIENTED_EDGE('',*,*,#16912,.T.);
#25506=ORIENTED_EDGE('',*,*,#16911,.T.);
#25507=ORIENTED_EDGE('',*,*,#16907,.T.);
#25508=ORIENTED_EDGE('',*,*,#16904,.T.);
#25509=ORIENTED_EDGE('',*,*,#16903,.T.);
#25510=ORIENTED_EDGE('',*,*,#16899,.T.);
#25511=ORIENTED_EDGE('',*,*,#16898,.T.);
#25512=ORIENTED_EDGE('',*,*,#16895,.T.);
#25513=ORIENTED_EDGE('',*,*,#16894,.T.);
#25514=ORIENTED_EDGE('',*,*,#16890,.T.);
#25515=ORIENTED_EDGE('',*,*,#16887,.T.);
#25516=ORIENTED_EDGE('',*,*,#16886,.T.);
#25517=ORIENTED_EDGE('',*,*,#16882,.T.);
#25518=ORIENTED_EDGE('',*,*,#16879,.T.);
#25519=ORIENTED_EDGE('',*,*,#16878,.T.);
#25520=ORIENTED_EDGE('',*,*,#16874,.T.);
#25521=ORIENTED_EDGE('',*,*,#16873,.T.);
#25522=ORIENTED_EDGE('',*,*,#16870,.T.);
#25523=ORIENTED_EDGE('',*,*,#16866,.T.);
#25524=ORIENTED_EDGE('',*,*,#16865,.T.);
#25525=ORIENTED_EDGE('',*,*,#17341,.T.);
#25526=ORIENTED_EDGE('',*,*,#16448,.T.);
#25527=ORIENTED_EDGE('',*,*,#16447,.T.);
#25528=ORIENTED_EDGE('',*,*,#16454,.T.);
#25529=ORIENTED_EDGE('',*,*,#16453,.T.);
#25530=ORIENTED_EDGE('',*,*,#16459,.T.);
#25531=ORIENTED_EDGE('',*,*,#16458,.T.);
#25532=ORIENTED_EDGE('',*,*,#16464,.T.);
#25533=ORIENTED_EDGE('',*,*,#16463,.T.);
#25534=ORIENTED_EDGE('',*,*,#16469,.T.);
#25535=ORIENTED_EDGE('',*,*,#16468,.T.);
#25536=ORIENTED_EDGE('',*,*,#16474,.T.);
#25537=ORIENTED_EDGE('',*,*,#16473,.T.);
#25538=ORIENTED_EDGE('',*,*,#16479,.T.);
#25539=ORIENTED_EDGE('',*,*,#16478,.T.);
#25540=ORIENTED_EDGE('',*,*,#16484,.T.);
#25541=ORIENTED_EDGE('',*,*,#16483,.T.);
#25542=ORIENTED_EDGE('',*,*,#16489,.T.);
#25543=ORIENTED_EDGE('',*,*,#16488,.T.);
#25544=ORIENTED_EDGE('',*,*,#16494,.T.);
#25545=ORIENTED_EDGE('',*,*,#16493,.T.);
#25546=ORIENTED_EDGE('',*,*,#16499,.T.);
#25547=ORIENTED_EDGE('',*,*,#16498,.T.);
#25548=ORIENTED_EDGE('',*,*,#16504,.T.);
#25549=ORIENTED_EDGE('',*,*,#16503,.T.);
#25550=ORIENTED_EDGE('',*,*,#16509,.T.);
#25551=ORIENTED_EDGE('',*,*,#16508,.T.);
#25552=ORIENTED_EDGE('',*,*,#16514,.T.);
#25553=ORIENTED_EDGE('',*,*,#16513,.T.);
#25554=ORIENTED_EDGE('',*,*,#16519,.T.);
#25555=ORIENTED_EDGE('',*,*,#16518,.T.);
#25556=ORIENTED_EDGE('',*,*,#16524,.T.);
#25557=ORIENTED_EDGE('',*,*,#16523,.T.);
#25558=ORIENTED_EDGE('',*,*,#16529,.T.);
#25559=ORIENTED_EDGE('',*,*,#16528,.T.);
#25560=ORIENTED_EDGE('',*,*,#16534,.T.);
#25561=ORIENTED_EDGE('',*,*,#16533,.T.);
#25562=ORIENTED_EDGE('',*,*,#16539,.T.);
#25563=ORIENTED_EDGE('',*,*,#16538,.T.);
#25564=ORIENTED_EDGE('',*,*,#16544,.T.);
#25565=ORIENTED_EDGE('',*,*,#16543,.T.);
#25566=ORIENTED_EDGE('',*,*,#16549,.T.);
#25567=ORIENTED_EDGE('',*,*,#16548,.T.);
#25568=ORIENTED_EDGE('',*,*,#16554,.T.);
#25569=ORIENTED_EDGE('',*,*,#16553,.T.);
#25570=ORIENTED_EDGE('',*,*,#16559,.T.);
#25571=ORIENTED_EDGE('',*,*,#16558,.T.);
#25572=ORIENTED_EDGE('',*,*,#16564,.T.);
#25573=ORIENTED_EDGE('',*,*,#16563,.T.);
#25574=ORIENTED_EDGE('',*,*,#16569,.T.);
#25575=ORIENTED_EDGE('',*,*,#16568,.T.);
#25576=ORIENTED_EDGE('',*,*,#16574,.T.);
#25577=ORIENTED_EDGE('',*,*,#16573,.T.);
#25578=ORIENTED_EDGE('',*,*,#16579,.T.);
#25579=ORIENTED_EDGE('',*,*,#16578,.T.);
#25580=ORIENTED_EDGE('',*,*,#17235,.T.);
#25581=ORIENTED_EDGE('',*,*,#17234,.T.);
#25582=ORIENTED_EDGE('',*,*,#17325,.T.);
#25583=ORIENTED_EDGE('',*,*,#17232,.F.);
#25584=ORIENTED_EDGE('',*,*,#17231,.F.);
#25585=ORIENTED_EDGE('',*,*,#16581,.F.);
#25586=ORIENTED_EDGE('',*,*,#16580,.F.);
#25587=ORIENTED_EDGE('',*,*,#16576,.F.);
#25588=ORIENTED_EDGE('',*,*,#16575,.F.);
#25589=ORIENTED_EDGE('',*,*,#16571,.F.);
#25590=ORIENTED_EDGE('',*,*,#16570,.F.);
#25591=ORIENTED_EDGE('',*,*,#16566,.F.);
#25592=ORIENTED_EDGE('',*,*,#16565,.F.);
#25593=ORIENTED_EDGE('',*,*,#16561,.F.);
#25594=ORIENTED_EDGE('',*,*,#16560,.F.);
#25595=ORIENTED_EDGE('',*,*,#16556,.F.);
#25596=ORIENTED_EDGE('',*,*,#16555,.F.);
#25597=ORIENTED_EDGE('',*,*,#16551,.F.);
#25598=ORIENTED_EDGE('',*,*,#16550,.F.);
#25599=ORIENTED_EDGE('',*,*,#16546,.F.);
#25600=ORIENTED_EDGE('',*,*,#16545,.F.);
#25601=ORIENTED_EDGE('',*,*,#16541,.F.);
#25602=ORIENTED_EDGE('',*,*,#16540,.F.);
#25603=ORIENTED_EDGE('',*,*,#16536,.F.);
#25604=ORIENTED_EDGE('',*,*,#16535,.F.);
#25605=ORIENTED_EDGE('',*,*,#16531,.F.);
#25606=ORIENTED_EDGE('',*,*,#16530,.F.);
#25607=ORIENTED_EDGE('',*,*,#16526,.F.);
#25608=ORIENTED_EDGE('',*,*,#16525,.F.);
#25609=ORIENTED_EDGE('',*,*,#16521,.F.);
#25610=ORIENTED_EDGE('',*,*,#16520,.F.);
#25611=ORIENTED_EDGE('',*,*,#16516,.F.);
#25612=ORIENTED_EDGE('',*,*,#16515,.F.);
#25613=ORIENTED_EDGE('',*,*,#16511,.F.);
#25614=ORIENTED_EDGE('',*,*,#16510,.F.);
#25615=ORIENTED_EDGE('',*,*,#16506,.F.);
#25616=ORIENTED_EDGE('',*,*,#16505,.F.);
#25617=ORIENTED_EDGE('',*,*,#16501,.F.);
#25618=ORIENTED_EDGE('',*,*,#16500,.F.);
#25619=ORIENTED_EDGE('',*,*,#16496,.F.);
#25620=ORIENTED_EDGE('',*,*,#16495,.F.);
#25621=ORIENTED_EDGE('',*,*,#16491,.F.);
#25622=ORIENTED_EDGE('',*,*,#16490,.F.);
#25623=ORIENTED_EDGE('',*,*,#16486,.F.);
#25624=ORIENTED_EDGE('',*,*,#16485,.F.);
#25625=ORIENTED_EDGE('',*,*,#16481,.F.);
#25626=ORIENTED_EDGE('',*,*,#16480,.F.);
#25627=ORIENTED_EDGE('',*,*,#16476,.F.);
#25628=ORIENTED_EDGE('',*,*,#16475,.F.);
#25629=ORIENTED_EDGE('',*,*,#16471,.F.);
#25630=ORIENTED_EDGE('',*,*,#16470,.F.);
#25631=ORIENTED_EDGE('',*,*,#16466,.F.);
#25632=ORIENTED_EDGE('',*,*,#16465,.F.);
#25633=ORIENTED_EDGE('',*,*,#16461,.F.);
#25634=ORIENTED_EDGE('',*,*,#16460,.F.);
#25635=ORIENTED_EDGE('',*,*,#16456,.F.);
#25636=ORIENTED_EDGE('',*,*,#16455,.F.);
#25637=ORIENTED_EDGE('',*,*,#16451,.F.);
#25638=ORIENTED_EDGE('',*,*,#16450,.F.);
#25639=ORIENTED_EDGE('',*,*,#17342,.T.);
#25640=ORIENTED_EDGE('',*,*,#16863,.T.);
#25641=ORIENTED_EDGE('',*,*,#16862,.T.);
#25642=ORIENTED_EDGE('',*,*,#16869,.T.);
#25643=ORIENTED_EDGE('',*,*,#16868,.T.);
#25644=ORIENTED_EDGE('',*,*,#16872,.T.);
#25645=ORIENTED_EDGE('',*,*,#16877,.T.);
#25646=ORIENTED_EDGE('',*,*,#16876,.T.);
#25647=ORIENTED_EDGE('',*,*,#16881,.T.);
#25648=ORIENTED_EDGE('',*,*,#16885,.T.);
#25649=ORIENTED_EDGE('',*,*,#16884,.T.);
#25650=ORIENTED_EDGE('',*,*,#16889,.T.);
#25651=ORIENTED_EDGE('',*,*,#16893,.T.);
#25652=ORIENTED_EDGE('',*,*,#16892,.T.);
#25653=ORIENTED_EDGE('',*,*,#16897,.T.);
#25654=ORIENTED_EDGE('',*,*,#16902,.T.);
#25655=ORIENTED_EDGE('',*,*,#16901,.T.);
#25656=ORIENTED_EDGE('',*,*,#16906,.T.);
#25657=ORIENTED_EDGE('',*,*,#16910,.T.);
#25658=ORIENTED_EDGE('',*,*,#16909,.T.);
#25659=ORIENTED_EDGE('',*,*,#16915,.T.);
#25660=ORIENTED_EDGE('',*,*,#16914,.T.);
#25661=ORIENTED_EDGE('',*,*,#16919,.T.);
#25662=ORIENTED_EDGE('',*,*,#16918,.T.);
#25663=ORIENTED_EDGE('',*,*,#16923,.T.);
#25664=ORIENTED_EDGE('',*,*,#16928,.T.);
#25665=ORIENTED_EDGE('',*,*,#16927,.T.);
#25666=ORIENTED_EDGE('',*,*,#16932,.T.);
#25667=ORIENTED_EDGE('',*,*,#16936,.T.);
#25668=ORIENTED_EDGE('',*,*,#16935,.T.);
#25669=ORIENTED_EDGE('',*,*,#16941,.T.);
#25670=ORIENTED_EDGE('',*,*,#16940,.T.);
#25671=ORIENTED_EDGE('',*,*,#16945,.T.);
#25672=ORIENTED_EDGE('',*,*,#16944,.T.);
#25673=ORIENTED_EDGE('',*,*,#16949,.T.);
#25674=ORIENTED_EDGE('',*,*,#16953,.T.);
#25675=ORIENTED_EDGE('',*,*,#16952,.T.);
#25676=ORIENTED_EDGE('',*,*,#16957,.T.);
#25677=ORIENTED_EDGE('',*,*,#16961,.T.);
#25678=ORIENTED_EDGE('',*,*,#16960,.T.);
#25679=ORIENTED_EDGE('',*,*,#16966,.T.);
#25680=ORIENTED_EDGE('',*,*,#16965,.T.);
#25681=ORIENTED_EDGE('',*,*,#16969,.T.);
#25682=ORIENTED_EDGE('',*,*,#16974,.T.);
#25683=ORIENTED_EDGE('',*,*,#16973,.T.);
#25684=ORIENTED_EDGE('',*,*,#17217,.T.);
#25685=ORIENTED_EDGE('',*,*,#17328,.T.);
#25686=ORIENTED_EDGE('',*,*,#17218,.T.);
#25687=ORIENTED_EDGE('',*,*,#16860,.T.);
#25688=ORIENTED_EDGE('',*,*,#16859,.T.);
#25689=ORIENTED_EDGE('',*,*,#16855,.T.);
#25690=ORIENTED_EDGE('',*,*,#16854,.T.);
#25691=ORIENTED_EDGE('',*,*,#16851,.T.);
#25692=ORIENTED_EDGE('',*,*,#16847,.T.);
#25693=ORIENTED_EDGE('',*,*,#16846,.T.);
#25694=ORIENTED_EDGE('',*,*,#16842,.T.);
#25695=ORIENTED_EDGE('',*,*,#16839,.T.);
#25696=ORIENTED_EDGE('',*,*,#16838,.T.);
#25697=ORIENTED_EDGE('',*,*,#16834,.T.);
#25698=ORIENTED_EDGE('',*,*,#16831,.T.);
#25699=ORIENTED_EDGE('',*,*,#16830,.T.);
#25700=ORIENTED_EDGE('',*,*,#16826,.T.);
#25701=ORIENTED_EDGE('',*,*,#16822,.T.);
#25702=ORIENTED_EDGE('',*,*,#16821,.T.);
#25703=ORIENTED_EDGE('',*,*,#16817,.T.);
#25704=ORIENTED_EDGE('',*,*,#16814,.T.);
#25705=ORIENTED_EDGE('',*,*,#16813,.T.);
#25706=ORIENTED_EDGE('',*,*,#16809,.T.);
#25707=ORIENTED_EDGE('',*,*,#16808,.T.);
#25708=ORIENTED_EDGE('',*,*,#16805,.T.);
#25709=ORIENTED_EDGE('',*,*,#16804,.T.);
#25710=ORIENTED_EDGE('',*,*,#16800,.T.);
#25711=ORIENTED_EDGE('',*,*,#16796,.T.);
#25712=ORIENTED_EDGE('',*,*,#16795,.T.);
#25713=ORIENTED_EDGE('',*,*,#16791,.T.);
#25714=ORIENTED_EDGE('',*,*,#16788,.T.);
#25715=ORIENTED_EDGE('',*,*,#16787,.T.);
#25716=ORIENTED_EDGE('',*,*,#16783,.T.);
#25717=ORIENTED_EDGE('',*,*,#16782,.T.);
#25718=ORIENTED_EDGE('',*,*,#16779,.T.);
#25719=ORIENTED_EDGE('',*,*,#16778,.T.);
#25720=ORIENTED_EDGE('',*,*,#16774,.T.);
#25721=ORIENTED_EDGE('',*,*,#16771,.T.);
#25722=ORIENTED_EDGE('',*,*,#16770,.T.);
#25723=ORIENTED_EDGE('',*,*,#16766,.T.);
#25724=ORIENTED_EDGE('',*,*,#16763,.T.);
#25725=ORIENTED_EDGE('',*,*,#16762,.T.);
#25726=ORIENTED_EDGE('',*,*,#16758,.T.);
#25727=ORIENTED_EDGE('',*,*,#16757,.T.);
#25728=ORIENTED_EDGE('',*,*,#16754,.T.);
#25729=ORIENTED_EDGE('',*,*,#16750,.T.);
#25730=ORIENTED_EDGE('',*,*,#16749,.T.);
#25731=ORIENTED_EDGE('',*,*,#17343,.T.);
#25732=ORIENTED_EDGE('',*,*,#16584,.T.);
#25733=ORIENTED_EDGE('',*,*,#16583,.T.);
#25734=ORIENTED_EDGE('',*,*,#16590,.T.);
#25735=ORIENTED_EDGE('',*,*,#16589,.T.);
#25736=ORIENTED_EDGE('',*,*,#16595,.T.);
#25737=ORIENTED_EDGE('',*,*,#16594,.T.);
#25738=ORIENTED_EDGE('',*,*,#16600,.T.);
#25739=ORIENTED_EDGE('',*,*,#16599,.T.);
#25740=ORIENTED_EDGE('',*,*,#16605,.T.);
#25741=ORIENTED_EDGE('',*,*,#16604,.T.);
#25742=ORIENTED_EDGE('',*,*,#16610,.T.);
#25743=ORIENTED_EDGE('',*,*,#16609,.T.);
#25744=ORIENTED_EDGE('',*,*,#16615,.T.);
#25745=ORIENTED_EDGE('',*,*,#16614,.T.);
#25746=ORIENTED_EDGE('',*,*,#16620,.T.);
#25747=ORIENTED_EDGE('',*,*,#16619,.T.);
#25748=ORIENTED_EDGE('',*,*,#16625,.T.);
#25749=ORIENTED_EDGE('',*,*,#16624,.T.);
#25750=ORIENTED_EDGE('',*,*,#16630,.T.);
#25751=ORIENTED_EDGE('',*,*,#16629,.T.);
#25752=ORIENTED_EDGE('',*,*,#16635,.T.);
#25753=ORIENTED_EDGE('',*,*,#16634,.T.);
#25754=ORIENTED_EDGE('',*,*,#16640,.T.);
#25755=ORIENTED_EDGE('',*,*,#16639,.T.);
#25756=ORIENTED_EDGE('',*,*,#16645,.T.);
#25757=ORIENTED_EDGE('',*,*,#16644,.T.);
#25758=ORIENTED_EDGE('',*,*,#16650,.T.);
#25759=ORIENTED_EDGE('',*,*,#16649,.T.);
#25760=ORIENTED_EDGE('',*,*,#16655,.T.);
#25761=ORIENTED_EDGE('',*,*,#16654,.T.);
#25762=ORIENTED_EDGE('',*,*,#16660,.T.);
#25763=ORIENTED_EDGE('',*,*,#16659,.T.);
#25764=ORIENTED_EDGE('',*,*,#16665,.T.);
#25765=ORIENTED_EDGE('',*,*,#16664,.T.);
#25766=ORIENTED_EDGE('',*,*,#16670,.T.);
#25767=ORIENTED_EDGE('',*,*,#16669,.T.);
#25768=ORIENTED_EDGE('',*,*,#16675,.T.);
#25769=ORIENTED_EDGE('',*,*,#16674,.T.);
#25770=ORIENTED_EDGE('',*,*,#16680,.T.);
#25771=ORIENTED_EDGE('',*,*,#16679,.T.);
#25772=ORIENTED_EDGE('',*,*,#16685,.T.);
#25773=ORIENTED_EDGE('',*,*,#16684,.T.);
#25774=ORIENTED_EDGE('',*,*,#16690,.T.);
#25775=ORIENTED_EDGE('',*,*,#16689,.T.);
#25776=ORIENTED_EDGE('',*,*,#16695,.T.);
#25777=ORIENTED_EDGE('',*,*,#16694,.T.);
#25778=ORIENTED_EDGE('',*,*,#16700,.T.);
#25779=ORIENTED_EDGE('',*,*,#16699,.T.);
#25780=ORIENTED_EDGE('',*,*,#16705,.T.);
#25781=ORIENTED_EDGE('',*,*,#16704,.T.);
#25782=ORIENTED_EDGE('',*,*,#16710,.T.);
#25783=ORIENTED_EDGE('',*,*,#16709,.T.);
#25784=ORIENTED_EDGE('',*,*,#16715,.T.);
#25785=ORIENTED_EDGE('',*,*,#16714,.T.);
#25786=ORIENTED_EDGE('',*,*,#17230,.T.);
#25787=ORIENTED_EDGE('',*,*,#17229,.T.);
#25788=ORIENTED_EDGE('',*,*,#17327,.T.);
#25789=ORIENTED_EDGE('',*,*,#17227,.F.);
#25790=ORIENTED_EDGE('',*,*,#17226,.F.);
#25791=ORIENTED_EDGE('',*,*,#16717,.F.);
#25792=ORIENTED_EDGE('',*,*,#16716,.F.);
#25793=ORIENTED_EDGE('',*,*,#16712,.F.);
#25794=ORIENTED_EDGE('',*,*,#16711,.F.);
#25795=ORIENTED_EDGE('',*,*,#16707,.F.);
#25796=ORIENTED_EDGE('',*,*,#16706,.F.);
#25797=ORIENTED_EDGE('',*,*,#16702,.F.);
#25798=ORIENTED_EDGE('',*,*,#16701,.F.);
#25799=ORIENTED_EDGE('',*,*,#16697,.F.);
#25800=ORIENTED_EDGE('',*,*,#16696,.F.);
#25801=ORIENTED_EDGE('',*,*,#16692,.F.);
#25802=ORIENTED_EDGE('',*,*,#16691,.F.);
#25803=ORIENTED_EDGE('',*,*,#16687,.F.);
#25804=ORIENTED_EDGE('',*,*,#16686,.F.);
#25805=ORIENTED_EDGE('',*,*,#16682,.F.);
#25806=ORIENTED_EDGE('',*,*,#16681,.F.);
#25807=ORIENTED_EDGE('',*,*,#16677,.F.);
#25808=ORIENTED_EDGE('',*,*,#16676,.F.);
#25809=ORIENTED_EDGE('',*,*,#16672,.F.);
#25810=ORIENTED_EDGE('',*,*,#16671,.F.);
#25811=ORIENTED_EDGE('',*,*,#16667,.F.);
#25812=ORIENTED_EDGE('',*,*,#16666,.F.);
#25813=ORIENTED_EDGE('',*,*,#16662,.F.);
#25814=ORIENTED_EDGE('',*,*,#16661,.F.);
#25815=ORIENTED_EDGE('',*,*,#16657,.F.);
#25816=ORIENTED_EDGE('',*,*,#16656,.F.);
#25817=ORIENTED_EDGE('',*,*,#16652,.F.);
#25818=ORIENTED_EDGE('',*,*,#16651,.F.);
#25819=ORIENTED_EDGE('',*,*,#16647,.F.);
#25820=ORIENTED_EDGE('',*,*,#16646,.F.);
#25821=ORIENTED_EDGE('',*,*,#16642,.F.);
#25822=ORIENTED_EDGE('',*,*,#16641,.F.);
#25823=ORIENTED_EDGE('',*,*,#16637,.F.);
#25824=ORIENTED_EDGE('',*,*,#16636,.F.);
#25825=ORIENTED_EDGE('',*,*,#16632,.F.);
#25826=ORIENTED_EDGE('',*,*,#16631,.F.);
#25827=ORIENTED_EDGE('',*,*,#16627,.F.);
#25828=ORIENTED_EDGE('',*,*,#16626,.F.);
#25829=ORIENTED_EDGE('',*,*,#16622,.F.);
#25830=ORIENTED_EDGE('',*,*,#16621,.F.);
#25831=ORIENTED_EDGE('',*,*,#16617,.F.);
#25832=ORIENTED_EDGE('',*,*,#16616,.F.);
#25833=ORIENTED_EDGE('',*,*,#16612,.F.);
#25834=ORIENTED_EDGE('',*,*,#16611,.F.);
#25835=ORIENTED_EDGE('',*,*,#16607,.F.);
#25836=ORIENTED_EDGE('',*,*,#16606,.F.);
#25837=ORIENTED_EDGE('',*,*,#16602,.F.);
#25838=ORIENTED_EDGE('',*,*,#16601,.F.);
#25839=ORIENTED_EDGE('',*,*,#16597,.F.);
#25840=ORIENTED_EDGE('',*,*,#16596,.F.);
#25841=ORIENTED_EDGE('',*,*,#16592,.F.);
#25842=ORIENTED_EDGE('',*,*,#16591,.F.);
#25843=ORIENTED_EDGE('',*,*,#16587,.F.);
#25844=ORIENTED_EDGE('',*,*,#16586,.F.);
#25845=ORIENTED_EDGE('',*,*,#17344,.T.);
#25846=ORIENTED_EDGE('',*,*,#16747,.T.);
#25847=ORIENTED_EDGE('',*,*,#16746,.T.);
#25848=ORIENTED_EDGE('',*,*,#16753,.T.);
#25849=ORIENTED_EDGE('',*,*,#16752,.T.);
#25850=ORIENTED_EDGE('',*,*,#16756,.T.);
#25851=ORIENTED_EDGE('',*,*,#16761,.T.);
#25852=ORIENTED_EDGE('',*,*,#16760,.T.);
#25853=ORIENTED_EDGE('',*,*,#16765,.T.);
#25854=ORIENTED_EDGE('',*,*,#16769,.T.);
#25855=ORIENTED_EDGE('',*,*,#16768,.T.);
#25856=ORIENTED_EDGE('',*,*,#16773,.T.);
#25857=ORIENTED_EDGE('',*,*,#16777,.T.);
#25858=ORIENTED_EDGE('',*,*,#16776,.T.);
#25859=ORIENTED_EDGE('',*,*,#16781,.T.);
#25860=ORIENTED_EDGE('',*,*,#16786,.T.);
#25861=ORIENTED_EDGE('',*,*,#16785,.T.);
#25862=ORIENTED_EDGE('',*,*,#16790,.T.);
#25863=ORIENTED_EDGE('',*,*,#16794,.T.);
#25864=ORIENTED_EDGE('',*,*,#16793,.T.);
#25865=ORIENTED_EDGE('',*,*,#16799,.T.);
#25866=ORIENTED_EDGE('',*,*,#16798,.T.);
#25867=ORIENTED_EDGE('',*,*,#16803,.T.);
#25868=ORIENTED_EDGE('',*,*,#16802,.T.);
#25869=ORIENTED_EDGE('',*,*,#16807,.T.);
#25870=ORIENTED_EDGE('',*,*,#16812,.T.);
#25871=ORIENTED_EDGE('',*,*,#16811,.T.);
#25872=ORIENTED_EDGE('',*,*,#16816,.T.);
#25873=ORIENTED_EDGE('',*,*,#16820,.T.);
#25874=ORIENTED_EDGE('',*,*,#16819,.T.);
#25875=ORIENTED_EDGE('',*,*,#16825,.T.);
#25876=ORIENTED_EDGE('',*,*,#16824,.T.);
#25877=ORIENTED_EDGE('',*,*,#16829,.T.);
#25878=ORIENTED_EDGE('',*,*,#16828,.T.);
#25879=ORIENTED_EDGE('',*,*,#16833,.T.);
#25880=ORIENTED_EDGE('',*,*,#16837,.T.);
#25881=ORIENTED_EDGE('',*,*,#16836,.T.);
#25882=ORIENTED_EDGE('',*,*,#16841,.T.);
#25883=ORIENTED_EDGE('',*,*,#16845,.T.);
#25884=ORIENTED_EDGE('',*,*,#16844,.T.);
#25885=ORIENTED_EDGE('',*,*,#16850,.T.);
#25886=ORIENTED_EDGE('',*,*,#16849,.T.);
#25887=ORIENTED_EDGE('',*,*,#16853,.T.);
#25888=ORIENTED_EDGE('',*,*,#16858,.T.);
#25889=ORIENTED_EDGE('',*,*,#16857,.T.);
#25890=ORIENTED_EDGE('',*,*,#17220,.T.);
#25891=ORIENTED_EDGE('',*,*,#17345,.T.);
#25892=ORIENTED_EDGE('',*,*,#17346,.T.);
#25893=ORIENTED_EDGE('',*,*,#17347,.T.);
#25894=ORIENTED_EDGE('',*,*,#17348,.F.);
#25895=ORIENTED_EDGE('',*,*,#17349,.T.);
#25896=ORIENTED_EDGE('',*,*,#17350,.T.);
#25897=ORIENTED_EDGE('',*,*,#17351,.T.);
#25898=ORIENTED_EDGE('',*,*,#17346,.F.);
#25899=ORIENTED_EDGE('',*,*,#17352,.T.);
#25900=ORIENTED_EDGE('',*,*,#17353,.T.);
#25901=ORIENTED_EDGE('',*,*,#17354,.T.);
#25902=ORIENTED_EDGE('',*,*,#17350,.F.);
#25903=ORIENTED_EDGE('',*,*,#17355,.T.);
#25904=ORIENTED_EDGE('',*,*,#17356,.T.);
#25905=ORIENTED_EDGE('',*,*,#17357,.T.);
#25906=ORIENTED_EDGE('',*,*,#17353,.F.);
#25907=ORIENTED_EDGE('',*,*,#17358,.T.);
#25908=ORIENTED_EDGE('',*,*,#17359,.T.);
#25909=ORIENTED_EDGE('',*,*,#17360,.T.);
#25910=ORIENTED_EDGE('',*,*,#17356,.F.);
#25911=ORIENTED_EDGE('',*,*,#17361,.T.);
#25912=ORIENTED_EDGE('',*,*,#17362,.T.);
#25913=ORIENTED_EDGE('',*,*,#17363,.T.);
#25914=ORIENTED_EDGE('',*,*,#17359,.F.);
#25915=ORIENTED_EDGE('',*,*,#17364,.T.);
#25916=ORIENTED_EDGE('',*,*,#17348,.T.);
#25917=ORIENTED_EDGE('',*,*,#17365,.T.);
#25918=ORIENTED_EDGE('',*,*,#17362,.F.);
#25919=ORIENTED_EDGE('',*,*,#17366,.T.);
#25920=ORIENTED_EDGE('',*,*,#17367,.T.);
#25921=ORIENTED_EDGE('',*,*,#17368,.T.);
#25922=ORIENTED_EDGE('',*,*,#17367,.F.);
#25923=ORIENTED_EDGE('',*,*,#17368,.F.);
#25924=ORIENTED_EDGE('',*,*,#17365,.F.);
#25925=ORIENTED_EDGE('',*,*,#17347,.F.);
#25926=ORIENTED_EDGE('',*,*,#17351,.F.);
#25927=ORIENTED_EDGE('',*,*,#17354,.F.);
#25928=ORIENTED_EDGE('',*,*,#17357,.F.);
#25929=ORIENTED_EDGE('',*,*,#17360,.F.);
#25930=ORIENTED_EDGE('',*,*,#17363,.F.);
#25931=ORIENTED_EDGE('',*,*,#17369,.T.);
#25932=ORIENTED_EDGE('',*,*,#17370,.T.);
#25933=ORIENTED_EDGE('',*,*,#17371,.T.);
#25934=ORIENTED_EDGE('',*,*,#17372,.F.);
#25935=ORIENTED_EDGE('',*,*,#17373,.T.);
#25936=ORIENTED_EDGE('',*,*,#17374,.T.);
#25937=ORIENTED_EDGE('',*,*,#17375,.T.);
#25938=ORIENTED_EDGE('',*,*,#17370,.F.);
#25939=ORIENTED_EDGE('',*,*,#17376,.T.);
#25940=ORIENTED_EDGE('',*,*,#17377,.T.);
#25941=ORIENTED_EDGE('',*,*,#17378,.T.);
#25942=ORIENTED_EDGE('',*,*,#17374,.F.);
#25943=ORIENTED_EDGE('',*,*,#17379,.T.);
#25944=ORIENTED_EDGE('',*,*,#17309,.T.);
#25945=ORIENTED_EDGE('',*,*,#17380,.T.);
#25946=ORIENTED_EDGE('',*,*,#17377,.F.);
#25947=ORIENTED_EDGE('',*,*,#17381,.T.);
#25948=ORIENTED_EDGE('',*,*,#17372,.T.);
#25949=ORIENTED_EDGE('',*,*,#17382,.T.);
#25950=ORIENTED_EDGE('',*,*,#17307,.T.);
#25951=ORIENTED_EDGE('',*,*,#17382,.F.);
#25952=ORIENTED_EDGE('',*,*,#17371,.F.);
#25953=ORIENTED_EDGE('',*,*,#17375,.F.);
#25954=ORIENTED_EDGE('',*,*,#17378,.F.);
#25955=ORIENTED_EDGE('',*,*,#17380,.F.);
#25956=ORIENTED_EDGE('',*,*,#17308,.T.);
#25957=ORIENTED_EDGE('',*,*,#17336,.F.);
#25958=ORIENTED_EDGE('',*,*,#16157,.F.);
#25959=ORIENTED_EDGE('',*,*,#17334,.F.);
#25960=ORIENTED_EDGE('',*,*,#17224,.T.);
#25961=ORIENTED_EDGE('',*,*,#17383,.T.);
#25962=ORIENTED_EDGE('',*,*,#17384,.T.);
#25963=ORIENTED_EDGE('',*,*,#17385,.T.);
#25964=ORIENTED_EDGE('',*,*,#17386,.T.);
#25965=ORIENTED_EDGE('',*,*,#17387,.T.);
#25966=ORIENTED_EDGE('',*,*,#17388,.F.);
#25967=ORIENTED_EDGE('',*,*,#17389,.T.);
#25968=ORIENTED_EDGE('',*,*,#17390,.T.);
#25969=ORIENTED_EDGE('',*,*,#17391,.T.);
#25970=ORIENTED_EDGE('',*,*,#17386,.F.);
#25971=ORIENTED_EDGE('',*,*,#17392,.T.);
#25972=ORIENTED_EDGE('',*,*,#17393,.T.);
#25973=ORIENTED_EDGE('',*,*,#17394,.T.);
#25974=ORIENTED_EDGE('',*,*,#17390,.F.);
#25975=ORIENTED_EDGE('',*,*,#17395,.T.);
#25976=ORIENTED_EDGE('',*,*,#17396,.T.);
#25977=ORIENTED_EDGE('',*,*,#17397,.T.);
#25978=ORIENTED_EDGE('',*,*,#17393,.F.);
#25979=ORIENTED_EDGE('',*,*,#17398,.T.);
#25980=ORIENTED_EDGE('',*,*,#17399,.T.);
#25981=ORIENTED_EDGE('',*,*,#17400,.T.);
#25982=ORIENTED_EDGE('',*,*,#17396,.F.);
#25983=ORIENTED_EDGE('',*,*,#17401,.T.);
#25984=ORIENTED_EDGE('',*,*,#17402,.T.);
#25985=ORIENTED_EDGE('',*,*,#17403,.T.);
#25986=ORIENTED_EDGE('',*,*,#17399,.F.);
#25987=ORIENTED_EDGE('',*,*,#17404,.T.);
#25988=ORIENTED_EDGE('',*,*,#17388,.T.);
#25989=ORIENTED_EDGE('',*,*,#17405,.T.);
#25990=ORIENTED_EDGE('',*,*,#17402,.F.);
#25991=ORIENTED_EDGE('',*,*,#17406,.T.);
#25992=ORIENTED_EDGE('',*,*,#17407,.T.);
#25993=ORIENTED_EDGE('',*,*,#17408,.T.);
#25994=ORIENTED_EDGE('',*,*,#17407,.F.);
#25995=ORIENTED_EDGE('',*,*,#17408,.F.);
#25996=ORIENTED_EDGE('',*,*,#17405,.F.);
#25997=ORIENTED_EDGE('',*,*,#17387,.F.);
#25998=ORIENTED_EDGE('',*,*,#17391,.F.);
#25999=ORIENTED_EDGE('',*,*,#17394,.F.);
#26000=ORIENTED_EDGE('',*,*,#17397,.F.);
#26001=ORIENTED_EDGE('',*,*,#17400,.F.);
#26002=ORIENTED_EDGE('',*,*,#17403,.F.);
#26003=ORIENTED_EDGE('',*,*,#17385,.F.);
#26004=ORIENTED_EDGE('',*,*,#17404,.F.);
#26005=ORIENTED_EDGE('',*,*,#17401,.F.);
#26006=ORIENTED_EDGE('',*,*,#17398,.F.);
#26007=ORIENTED_EDGE('',*,*,#17395,.F.);
#26008=ORIENTED_EDGE('',*,*,#17392,.F.);
#26009=ORIENTED_EDGE('',*,*,#17389,.F.);
#26010=ORIENTED_EDGE('',*,*,#17345,.F.);
#26011=ORIENTED_EDGE('',*,*,#17364,.F.);
#26012=ORIENTED_EDGE('',*,*,#17361,.F.);
#26013=ORIENTED_EDGE('',*,*,#17358,.F.);
#26014=ORIENTED_EDGE('',*,*,#17355,.F.);
#26015=ORIENTED_EDGE('',*,*,#17352,.F.);
#26016=ORIENTED_EDGE('',*,*,#17349,.F.);
#26017=ORIENTED_EDGE('',*,*,#17383,.F.);
#26018=ORIENTED_EDGE('',*,*,#17409,.T.);
#26019=ORIENTED_EDGE('',*,*,#17410,.T.);
#26020=ORIENTED_EDGE('',*,*,#17409,.F.);
#26021=ORIENTED_EDGE('',*,*,#17410,.F.);
#26022=ORIENTED_EDGE('',*,*,#16720,.F.);
#26023=ORIENTED_EDGE('',*,*,#17333,.F.);
#26024=ORIENTED_EDGE('',*,*,#17248,.F.);
#26025=ORIENTED_EDGE('',*,*,#17335,.F.);
#26026=ORIENTED_EDGE('',*,*,#16723,.F.);
#26027=ORIENTED_EDGE('',*,*,#17384,.F.);
#26028=ORIENTED_EDGE('',*,*,#17411,.T.);
#26029=ORIENTED_EDGE('',*,*,#17412,.T.);
#26030=ORIENTED_EDGE('',*,*,#17411,.F.);
#26031=ORIENTED_EDGE('',*,*,#17412,.F.);
#26032=ORIENTED_EDGE('',*,*,#17413,.T.);
#26033=ORIENTED_EDGE('',*,*,#17414,.T.);
#26034=ORIENTED_EDGE('',*,*,#17415,.F.);
#26035=ORIENTED_EDGE('',*,*,#17416,.F.);
#26036=ORIENTED_EDGE('',*,*,#17417,.T.);
#26037=ORIENTED_EDGE('',*,*,#17416,.T.);
#26038=ORIENTED_EDGE('',*,*,#17418,.F.);
#26039=ORIENTED_EDGE('',*,*,#17419,.F.);
#26040=ORIENTED_EDGE('',*,*,#17420,.T.);
#26041=ORIENTED_EDGE('',*,*,#17419,.T.);
#26042=ORIENTED_EDGE('',*,*,#17421,.F.);
#26043=ORIENTED_EDGE('',*,*,#17422,.F.);
#26044=ORIENTED_EDGE('',*,*,#17423,.T.);
#26045=ORIENTED_EDGE('',*,*,#17422,.T.);
#26046=ORIENTED_EDGE('',*,*,#17424,.F.);
#26047=ORIENTED_EDGE('',*,*,#17299,.T.);
#26048=ORIENTED_EDGE('',*,*,#17425,.T.);
#26049=ORIENTED_EDGE('',*,*,#17301,.T.);
#26050=ORIENTED_EDGE('',*,*,#17426,.F.);
#26051=ORIENTED_EDGE('',*,*,#17414,.F.);
#26052=ORIENTED_EDGE('',*,*,#17426,.T.);
#26053=ORIENTED_EDGE('',*,*,#17300,.T.);
#26054=ORIENTED_EDGE('',*,*,#17424,.T.);
#26055=ORIENTED_EDGE('',*,*,#17421,.T.);
#26056=ORIENTED_EDGE('',*,*,#17418,.T.);
#26057=ORIENTED_EDGE('',*,*,#17415,.T.);
#26058=ORIENTED_EDGE('',*,*,#17332,.F.);
#26059=ORIENTED_EDGE('',*,*,#16138,.F.);
#26060=ORIENTED_EDGE('',*,*,#17330,.F.);
#26061=ORIENTED_EDGE('',*,*,#16733,.T.);
#26062=ORIENTED_EDGE('',*,*,#17427,.T.);
#26063=ORIENTED_EDGE('',*,*,#17428,.T.);
#26064=ORIENTED_EDGE('',*,*,#17429,.T.);
#26065=ORIENTED_EDGE('',*,*,#17430,.T.);
#26066=ORIENTED_EDGE('',*,*,#17431,.F.);
#26067=ORIENTED_EDGE('',*,*,#17432,.F.);
#26068=ORIENTED_EDGE('',*,*,#17433,.T.);
#26069=ORIENTED_EDGE('',*,*,#17432,.T.);
#26070=ORIENTED_EDGE('',*,*,#17434,.F.);
#26071=ORIENTED_EDGE('',*,*,#17435,.F.);
#26072=ORIENTED_EDGE('',*,*,#17436,.T.);
#26073=ORIENTED_EDGE('',*,*,#17435,.T.);
#26074=ORIENTED_EDGE('',*,*,#17437,.F.);
#26075=ORIENTED_EDGE('',*,*,#17438,.F.);
#26076=ORIENTED_EDGE('',*,*,#17439,.T.);
#26077=ORIENTED_EDGE('',*,*,#17438,.T.);
#26078=ORIENTED_EDGE('',*,*,#17440,.F.);
#26079=ORIENTED_EDGE('',*,*,#17441,.F.);
#26080=ORIENTED_EDGE('',*,*,#17442,.T.);
#26081=ORIENTED_EDGE('',*,*,#17441,.T.);
#26082=ORIENTED_EDGE('',*,*,#17443,.F.);
#26083=ORIENTED_EDGE('',*,*,#17444,.F.);
#26084=ORIENTED_EDGE('',*,*,#17445,.T.);
#26085=ORIENTED_EDGE('',*,*,#17444,.T.);
#26086=ORIENTED_EDGE('',*,*,#17446,.F.);
#26087=ORIENTED_EDGE('',*,*,#17447,.F.);
#26088=ORIENTED_EDGE('',*,*,#17448,.T.);
#26089=ORIENTED_EDGE('',*,*,#17447,.T.);
#26090=ORIENTED_EDGE('',*,*,#17449,.F.);
#26091=ORIENTED_EDGE('',*,*,#17430,.F.);
#26092=ORIENTED_EDGE('',*,*,#17450,.F.);
#26093=ORIENTED_EDGE('',*,*,#17451,.T.);
#26094=ORIENTED_EDGE('',*,*,#17452,.T.);
#26095=ORIENTED_EDGE('',*,*,#17451,.F.);
#26096=ORIENTED_EDGE('',*,*,#17450,.T.);
#26097=ORIENTED_EDGE('',*,*,#17449,.T.);
#26098=ORIENTED_EDGE('',*,*,#17446,.T.);
#26099=ORIENTED_EDGE('',*,*,#17443,.T.);
#26100=ORIENTED_EDGE('',*,*,#17440,.T.);
#26101=ORIENTED_EDGE('',*,*,#17437,.T.);
#26102=ORIENTED_EDGE('',*,*,#17434,.T.);
#26103=ORIENTED_EDGE('',*,*,#17431,.T.);
#26104=ORIENTED_EDGE('',*,*,#17453,.T.);
#26105=ORIENTED_EDGE('',*,*,#17454,.T.);
#26106=ORIENTED_EDGE('',*,*,#17455,.F.);
#26107=ORIENTED_EDGE('',*,*,#17456,.F.);
#26108=ORIENTED_EDGE('',*,*,#17457,.T.);
#26109=ORIENTED_EDGE('',*,*,#17456,.T.);
#26110=ORIENTED_EDGE('',*,*,#17458,.F.);
#26111=ORIENTED_EDGE('',*,*,#17459,.F.);
#26112=ORIENTED_EDGE('',*,*,#17460,.T.);
#26113=ORIENTED_EDGE('',*,*,#17459,.T.);
#26114=ORIENTED_EDGE('',*,*,#17461,.F.);
#26115=ORIENTED_EDGE('',*,*,#17462,.F.);
#26116=ORIENTED_EDGE('',*,*,#17463,.T.);
#26117=ORIENTED_EDGE('',*,*,#17462,.T.);
#26118=ORIENTED_EDGE('',*,*,#17464,.F.);
#26119=ORIENTED_EDGE('',*,*,#17465,.F.);
#26120=ORIENTED_EDGE('',*,*,#17466,.T.);
#26121=ORIENTED_EDGE('',*,*,#17465,.T.);
#26122=ORIENTED_EDGE('',*,*,#17467,.F.);
#26123=ORIENTED_EDGE('',*,*,#17468,.F.);
#26124=ORIENTED_EDGE('',*,*,#17469,.T.);
#26125=ORIENTED_EDGE('',*,*,#17468,.T.);
#26126=ORIENTED_EDGE('',*,*,#17470,.F.);
#26127=ORIENTED_EDGE('',*,*,#17471,.F.);
#26128=ORIENTED_EDGE('',*,*,#17472,.T.);
#26129=ORIENTED_EDGE('',*,*,#17471,.T.);
#26130=ORIENTED_EDGE('',*,*,#17473,.F.);
#26131=ORIENTED_EDGE('',*,*,#17454,.F.);
#26132=ORIENTED_EDGE('',*,*,#17474,.F.);
#26133=ORIENTED_EDGE('',*,*,#17475,.T.);
#26134=ORIENTED_EDGE('',*,*,#17476,.T.);
#26135=ORIENTED_EDGE('',*,*,#17475,.F.);
#26136=ORIENTED_EDGE('',*,*,#17474,.T.);
#26137=ORIENTED_EDGE('',*,*,#17473,.T.);
#26138=ORIENTED_EDGE('',*,*,#17470,.T.);
#26139=ORIENTED_EDGE('',*,*,#17467,.T.);
#26140=ORIENTED_EDGE('',*,*,#17464,.T.);
#26141=ORIENTED_EDGE('',*,*,#17461,.T.);
#26142=ORIENTED_EDGE('',*,*,#17458,.T.);
#26143=ORIENTED_EDGE('',*,*,#17455,.T.);
#26144=ORIENTED_EDGE('',*,*,#17453,.F.);
#26145=ORIENTED_EDGE('',*,*,#17457,.F.);
#26146=ORIENTED_EDGE('',*,*,#17460,.F.);
#26147=ORIENTED_EDGE('',*,*,#17463,.F.);
#26148=ORIENTED_EDGE('',*,*,#17466,.F.);
#26149=ORIENTED_EDGE('',*,*,#17469,.F.);
#26150=ORIENTED_EDGE('',*,*,#17472,.F.);
#26151=ORIENTED_EDGE('',*,*,#17429,.F.);
#26152=ORIENTED_EDGE('',*,*,#17433,.F.);
#26153=ORIENTED_EDGE('',*,*,#17436,.F.);
#26154=ORIENTED_EDGE('',*,*,#17439,.F.);
#26155=ORIENTED_EDGE('',*,*,#17442,.F.);
#26156=ORIENTED_EDGE('',*,*,#17445,.F.);
#26157=ORIENTED_EDGE('',*,*,#17448,.F.);
#26158=ORIENTED_EDGE('',*,*,#17423,.F.);
#26159=ORIENTED_EDGE('',*,*,#17298,.T.);
#26160=ORIENTED_EDGE('',*,*,#17477,.F.);
#26161=ORIENTED_EDGE('',*,*,#17478,.T.);
#26162=ORIENTED_EDGE('',*,*,#17479,.T.);
#26163=ORIENTED_EDGE('',*,*,#17302,.T.);
#26164=ORIENTED_EDGE('',*,*,#17425,.F.);
#26165=ORIENTED_EDGE('',*,*,#17413,.F.);
#26166=ORIENTED_EDGE('',*,*,#17417,.F.);
#26167=ORIENTED_EDGE('',*,*,#17420,.F.);
#26168=ORIENTED_EDGE('',*,*,#17476,.F.);
#26169=ORIENTED_EDGE('',*,*,#17452,.F.);
#26170=ORIENTED_EDGE('',*,*,#16742,.T.);
#26171=ORIENTED_EDGE('',*,*,#17222,.T.);
#26172=ORIENTED_EDGE('',*,*,#17329,.F.);
#26173=ORIENTED_EDGE('',*,*,#17253,.F.);
#26174=ORIENTED_EDGE('',*,*,#17331,.F.);
#26175=ORIENTED_EDGE('',*,*,#17480,.F.);
#26176=ORIENTED_EDGE('',*,*,#17481,.T.);
#26177=ORIENTED_EDGE('',*,*,#17428,.F.);
#26178=ORIENTED_EDGE('',*,*,#17481,.F.);
#26179=ORIENTED_EDGE('',*,*,#17480,.T.);
#26180=ORIENTED_EDGE('',*,*,#17482,.F.);
#26181=ORIENTED_EDGE('',*,*,#17483,.T.);
#26182=ORIENTED_EDGE('',*,*,#17427,.F.);
#26183=ORIENTED_EDGE('',*,*,#17483,.F.);
#26184=ORIENTED_EDGE('',*,*,#17482,.T.);
#26185=ORIENTED_EDGE('',*,*,#17484,.F.);
#26186=ORIENTED_EDGE('',*,*,#17485,.T.);
#26187=ORIENTED_EDGE('',*,*,#17319,.T.);
#26188=ORIENTED_EDGE('',*,*,#17485,.F.);
#26189=ORIENTED_EDGE('',*,*,#17484,.T.);
#26190=ORIENTED_EDGE('',*,*,#17486,.F.);
#26191=ORIENTED_EDGE('',*,*,#17487,.T.);
#26192=ORIENTED_EDGE('',*,*,#17320,.T.);
#26193=ORIENTED_EDGE('',*,*,#17487,.F.);
#26194=ORIENTED_EDGE('',*,*,#17486,.T.);
#26195=ORIENTED_EDGE('',*,*,#17274,.F.);
#26196=ORIENTED_EDGE('',*,*,#17289,.F.);
#26197=ORIENTED_EDGE('',*,*,#17488,.T.);
#26198=ORIENTED_EDGE('',*,*,#17489,.T.);
#26199=ORIENTED_EDGE('',*,*,#17275,.F.);
#26200=ORIENTED_EDGE('',*,*,#17489,.F.);
#26201=ORIENTED_EDGE('',*,*,#17490,.T.);
#26202=ORIENTED_EDGE('',*,*,#17284,.T.);
#26203=ORIENTED_EDGE('',*,*,#17491,.F.);
#26204=ORIENTED_EDGE('',*,*,#17492,.T.);
#26205=ORIENTED_EDGE('',*,*,#17291,.T.);
#26206=ORIENTED_EDGE('',*,*,#17286,.F.);
#26207=ORIENTED_EDGE('',*,*,#17493,.T.);
#26208=ORIENTED_EDGE('',*,*,#17494,.T.);
#26209=ORIENTED_EDGE('',*,*,#17292,.T.);
#26210=ORIENTED_EDGE('',*,*,#17492,.F.);
#26211=ORIENTED_EDGE('',*,*,#17495,.T.);
#26212=ORIENTED_EDGE('',*,*,#17496,.T.);
#26213=ORIENTED_EDGE('',*,*,#17293,.T.);
#26214=ORIENTED_EDGE('',*,*,#17494,.F.);
#26215=ORIENTED_EDGE('',*,*,#17497,.T.);
#26216=ORIENTED_EDGE('',*,*,#17498,.T.);
#26217=ORIENTED_EDGE('',*,*,#17294,.T.);
#26218=ORIENTED_EDGE('',*,*,#17496,.F.);
#26219=ORIENTED_EDGE('',*,*,#17499,.T.);
#26220=ORIENTED_EDGE('',*,*,#17500,.T.);
#26221=ORIENTED_EDGE('',*,*,#17295,.T.);
#26222=ORIENTED_EDGE('',*,*,#17498,.F.);
#26223=ORIENTED_EDGE('',*,*,#17501,.T.);
#26224=ORIENTED_EDGE('',*,*,#17502,.T.);
#26225=ORIENTED_EDGE('',*,*,#17296,.T.);
#26226=ORIENTED_EDGE('',*,*,#17500,.F.);
#26227=ORIENTED_EDGE('',*,*,#17503,.T.);
#26228=ORIENTED_EDGE('',*,*,#17477,.T.);
#26229=ORIENTED_EDGE('',*,*,#17297,.T.);
#26230=ORIENTED_EDGE('',*,*,#17502,.F.);
#26231=ORIENTED_EDGE('',*,*,#17504,.T.);
#26232=ORIENTED_EDGE('',*,*,#17505,.T.);
#26233=ORIENTED_EDGE('',*,*,#17303,.T.);
#26234=ORIENTED_EDGE('',*,*,#17479,.F.);
#26235=ORIENTED_EDGE('',*,*,#17506,.T.);
#26236=ORIENTED_EDGE('',*,*,#17507,.T.);
#26237=ORIENTED_EDGE('',*,*,#17304,.T.);
#26238=ORIENTED_EDGE('',*,*,#17505,.F.);
#26239=ORIENTED_EDGE('',*,*,#17508,.T.);
#26240=ORIENTED_EDGE('',*,*,#17509,.T.);
#26241=ORIENTED_EDGE('',*,*,#17305,.T.);
#26242=ORIENTED_EDGE('',*,*,#17507,.F.);
#26243=ORIENTED_EDGE('',*,*,#17379,.F.);
#26244=ORIENTED_EDGE('',*,*,#17376,.F.);
#26245=ORIENTED_EDGE('',*,*,#17373,.F.);
#26246=ORIENTED_EDGE('',*,*,#17369,.F.);
#26247=ORIENTED_EDGE('',*,*,#17381,.F.);
#26248=ORIENTED_EDGE('',*,*,#17306,.T.);
#26249=ORIENTED_EDGE('',*,*,#17509,.F.);
#26250=ORIENTED_EDGE('',*,*,#17510,.F.);
#26251=ORIENTED_EDGE('',*,*,#17511,.T.);
#26252=ORIENTED_EDGE('',*,*,#17310,.T.);
#26253=ORIENTED_EDGE('',*,*,#17406,.F.);
#26254=ORIENTED_EDGE('',*,*,#17366,.F.);
#26255=ORIENTED_EDGE('',*,*,#17512,.T.);
#26256=ORIENTED_EDGE('',*,*,#17513,.T.);
#26257=ORIENTED_EDGE('',*,*,#17311,.T.);
#26258=ORIENTED_EDGE('',*,*,#17511,.F.);
#26259=ORIENTED_EDGE('',*,*,#17514,.F.);
#26260=ORIENTED_EDGE('',*,*,#17515,.T.);
#26261=ORIENTED_EDGE('',*,*,#17312,.T.);
#26262=ORIENTED_EDGE('',*,*,#17513,.F.);
#26263=ORIENTED_EDGE('',*,*,#17516,.T.);
#26264=ORIENTED_EDGE('',*,*,#17517,.T.);
#26265=ORIENTED_EDGE('',*,*,#17313,.T.);
#26266=ORIENTED_EDGE('',*,*,#17515,.F.);
#26267=ORIENTED_EDGE('',*,*,#17518,.F.);
#26268=ORIENTED_EDGE('',*,*,#17519,.T.);
#26269=ORIENTED_EDGE('',*,*,#17314,.T.);
#26270=ORIENTED_EDGE('',*,*,#17517,.F.);
#26271=ORIENTED_EDGE('',*,*,#17520,.T.);
#26272=ORIENTED_EDGE('',*,*,#17521,.T.);
#26273=ORIENTED_EDGE('',*,*,#17315,.T.);
#26274=ORIENTED_EDGE('',*,*,#17519,.F.);
#26275=ORIENTED_EDGE('',*,*,#17522,.F.);
#26276=ORIENTED_EDGE('',*,*,#17523,.T.);
#26277=ORIENTED_EDGE('',*,*,#17316,.T.);
#26278=ORIENTED_EDGE('',*,*,#17521,.F.);
#26279=ORIENTED_EDGE('',*,*,#17524,.F.);
#26280=ORIENTED_EDGE('',*,*,#17525,.T.);
#26281=ORIENTED_EDGE('',*,*,#17317,.T.);
#26282=ORIENTED_EDGE('',*,*,#17523,.F.);
#26283=ORIENTED_EDGE('',*,*,#17263,.F.);
#26284=ORIENTED_EDGE('',*,*,#17260,.F.);
#26285=ORIENTED_EDGE('',*,*,#17318,.T.);
#26286=ORIENTED_EDGE('',*,*,#17525,.F.);
#26287=ORIENTED_EDGE('',*,*,#17526,.F.);
#26288=ORIENTED_EDGE('',*,*,#17527,.T.);
#26289=ORIENTED_EDGE('',*,*,#17264,.F.);
#26290=ORIENTED_EDGE('',*,*,#17527,.F.);
#26291=ORIENTED_EDGE('',*,*,#17528,.T.);
#26292=ORIENTED_EDGE('',*,*,#17281,.T.);
#26293=ORIENTED_EDGE('',*,*,#17528,.F.);
#26294=ORIENTED_EDGE('',*,*,#17526,.T.);
#26295=ORIENTED_EDGE('',*,*,#17524,.T.);
#26296=ORIENTED_EDGE('',*,*,#17522,.T.);
#26297=ORIENTED_EDGE('',*,*,#17520,.F.);
#26298=ORIENTED_EDGE('',*,*,#17518,.T.);
#26299=ORIENTED_EDGE('',*,*,#17516,.F.);
#26300=ORIENTED_EDGE('',*,*,#17514,.T.);
#26301=ORIENTED_EDGE('',*,*,#17512,.F.);
#26302=ORIENTED_EDGE('',*,*,#17510,.T.);
#26303=ORIENTED_EDGE('',*,*,#17508,.F.);
#26304=ORIENTED_EDGE('',*,*,#17506,.F.);
#26305=ORIENTED_EDGE('',*,*,#17504,.F.);
#26306=ORIENTED_EDGE('',*,*,#17478,.F.);
#26307=ORIENTED_EDGE('',*,*,#17503,.F.);
#26308=ORIENTED_EDGE('',*,*,#17501,.F.);
#26309=ORIENTED_EDGE('',*,*,#17499,.F.);
#26310=ORIENTED_EDGE('',*,*,#17497,.F.);
#26311=ORIENTED_EDGE('',*,*,#17495,.F.);
#26312=ORIENTED_EDGE('',*,*,#17493,.F.);
#26313=ORIENTED_EDGE('',*,*,#17491,.T.);
#26314=ORIENTED_EDGE('',*,*,#17285,.F.);
#26315=ORIENTED_EDGE('',*,*,#17490,.F.);
#26316=ORIENTED_EDGE('',*,*,#17488,.F.);
#26317=ORIENTED_EDGE('',*,*,#17288,.F.);
#26318=ORIENTED_EDGE('',*,*,#17282,.T.);
#26319=ORIENTED_EDGE('',*,*,#17338,.F.);
#26320=ORIENTED_EDGE('',*,*,#16177,.F.);
#26321=ORIENTED_EDGE('',*,*,#17337,.F.);
#26322=ORIENTED_EDGE('',*,*,#17096,.F.);
#26323=ORIENTED_EDGE('',*,*,#17340,.F.);
#26324=ORIENTED_EDGE('',*,*,#16313,.F.);
#26325=ORIENTED_EDGE('',*,*,#17339,.F.);
#26326=ORIENTED_EDGE('',*,*,#16980,.F.);
#26327=ORIENTED_EDGE('',*,*,#17342,.F.);
#26328=ORIENTED_EDGE('',*,*,#16449,.F.);
#26329=ORIENTED_EDGE('',*,*,#17341,.F.);
#26330=ORIENTED_EDGE('',*,*,#16864,.F.);
#26331=ORIENTED_EDGE('',*,*,#17344,.F.);
#26332=ORIENTED_EDGE('',*,*,#16585,.F.);
#26333=ORIENTED_EDGE('',*,*,#17343,.F.);
#26334=ORIENTED_EDGE('',*,*,#16748,.F.);
#26335=PLANE('',#28180);
#26336=PLANE('',#28191);
#26337=PLANE('',#28192);
#26338=PLANE('',#28195);
#26339=PLANE('',#28198);
#26340=PLANE('',#28201);
#26341=PLANE('',#28204);
#26342=PLANE('',#28207);
#26343=PLANE('',#28208);
#26344=PLANE('',#28211);
#26345=PLANE('',#28214);
#26346=PLANE('',#28217);
#26347=PLANE('',#28220);
#26348=PLANE('',#28223);
#26349=PLANE('',#28224);
#26350=PLANE('',#28225);
#26351=PLANE('',#28226);
#26352=PLANE('',#28228);
#26353=PLANE('',#28239);
#26354=PLANE('',#28242);
#26355=PLANE('',#28245);
#26356=PLANE('',#28246);
#26357=PLANE('',#28247);
#26358=PLANE('',#28248);
#26359=PLANE('',#28249);
#26360=PLANE('',#28250);
#26361=PLANE('',#28253);
#26362=PLANE('',#28256);
#26363=PLANE('',#28259);
#26364=PLANE('',#28262);
#26365=PLANE('',#28263);
#26366=PLANE('',#28264);
#26367=PLANE('',#28265);
#26368=PLANE('',#28266);
#26369=PLANE('',#28267);
#26370=PLANE('',#28270);
#26371=PLANE('',#28271);
#26372=PLANE('',#28546);
#26373=PLANE('',#28550);
#26374=PLANE('',#28555);
#26375=PLANE('',#28559);
#26376=PLANE('',#28564);
#26377=PLANE('',#28565);
#26378=PLANE('',#28566);
#26379=PLANE('',#28567);
#26380=PLANE('',#28568);
#26381=PLANE('',#28581);
#26382=PLANE('',#28582);
#26383=PLANE('',#28583);
#26384=PLANE('',#28584);
#26385=PLANE('',#28585);
#26386=PLANE('',#28586);
#26387=PLANE('',#28587);
#26388=PLANE('',#28591);
#26389=PLANE('',#28595);
#26390=PLANE('',#28599);
#26391=PLANE('',#28600);
#26392=PLANE('',#28601);
#26393=PLANE('',#28604);
#26394=PLANE('',#28605);
#26395=PLANE('',#28606);
#26396=PLANE('',#28607);
#26397=PLANE('',#28608);
#26398=PLANE('',#28609);
#26399=PLANE('',#28610);
#26400=PLANE('',#28614);
#26401=PLANE('',#28615);
#26402=PLANE('',#28616);
#26403=PLANE('',#28619);
#26404=PLANE('',#28620);
#26405=PLANE('',#28623);
#26406=PLANE('',#28627);
#26407=PLANE('',#28631);
#26408=PLANE('',#28632);
#26409=PLANE('',#28633);
#26410=PLANE('',#28636);
#26411=PLANE('',#28637);
#26412=PLANE('',#28638);
#26413=PLANE('',#28639);
#26414=PLANE('',#28640);
#26415=PLANE('',#28641);
#26416=PLANE('',#28642);
#26417=PLANE('',#28646);
#26418=PLANE('',#28647);
#26419=PLANE('',#28648);
#26420=PLANE('',#28649);
#26421=PLANE('',#28650);
#26422=PLANE('',#28651);
#26423=PLANE('',#28652);
#26424=PLANE('',#28653);
#26425=PLANE('',#28657);
#26426=PLANE('',#28658);
#26427=PLANE('',#28659);
#26428=PLANE('',#28660);
#26429=PLANE('',#28661);
#26430=PLANE('',#28664);
#26431=PLANE('',#28667);
#26432=PLANE('',#28670);
#26433=PLANE('',#28673);
#26434=PLANE('',#28674);
#26435=PLANE('',#28679);
#26436=PLANE('',#28682);
#26437=PLANE('',#28685);
#26438=PLANE('',#28690);
#26439=PLANE('',#28693);
#26440=PLANE('',#28696);
#26441=PLANE('',#28699);
#26442=PLANE('',#28702);
#26443=PLANE('',#28705);
#26444=PLANE('',#28708);
#26445=PLANE('',#28714);
#26446=PLANE('',#28718);
#26447=PLANE('',#28807);
#26448=PLANE('',#28810);
#26449=PLANE('',#28811);
#26450=PLANE('',#28812);
#26451=PLANE('',#28815);
#26452=PLANE('',#28818);
#26453=PLANE('',#28822);
#26454=PLANE('',#28825);
#26455=PLANE('',#28828);
#26456=PLANE('',#28829);
#26457=PLANE('',#28830);
#26458=PLANE('',#28831);
#26459=PLANE('',#28855);
#26460=PLANE('',#28906);
#26461=PLANE('',#28907);
#26462=PLANE('',#28908);
#26463=PLANE('',#28909);
#26464=PLANE('',#28911);
#26465=PLANE('',#28912);
#26466=PLANE('',#28913);
#26467=PLANE('',#28915);
#26468=PLANE('',#28917);
#26469=PLANE('',#28924);
#26470=PLANE('',#28925);
#26471=PLANE('',#28927);
#26472=PLANE('',#28929);
#26473=PLANE('',#28935);
#26474=PLANE('',#28939);
#26475=PLANE('',#29028);
#26476=PLANE('',#29031);
#26477=PLANE('',#29032);
#26478=PLANE('',#29033);
#26479=PLANE('',#29036);
#26480=PLANE('',#29039);
#26481=PLANE('',#29043);
#26482=PLANE('',#29046);
#26483=PLANE('',#29049);
#26484=PLANE('',#29050);
#26485=PLANE('',#29051);
#26486=PLANE('',#29052);
#26487=PLANE('',#29076);
#26488=PLANE('',#29127);
#26489=PLANE('',#29128);
#26490=PLANE('',#29129);
#26491=PLANE('',#29130);
#26492=PLANE('',#29132);
#26493=PLANE('',#29133);
#26494=PLANE('',#29134);
#26495=PLANE('',#29136);
#26496=PLANE('',#29138);
#26497=PLANE('',#29145);
#26498=PLANE('',#29146);
#26499=PLANE('',#29148);
#26500=PLANE('',#29150);
#26501=PLANE('',#29156);
#26502=PLANE('',#29161);
#26503=PLANE('',#29162);
#26504=PLANE('',#29163);
#26505=PLANE('',#29183);
#26506=PLANE('',#29203);
#26507=PLANE('',#29226);
#26508=PLANE('',#29227);
#26509=PLANE('',#29228);
#26510=PLANE('',#29234);
#26511=PLANE('',#29235);
#26512=PLANE('',#29236);
#26513=PLANE('',#29242);
#26514=PLANE('',#29243);
#26515=PLANE('',#29244);
#26516=PLANE('',#29250);
#26517=PLANE('',#29251);
#26518=PLANE('',#29252);
#26519=PLANE('',#29258);
#26520=PLANE('',#29259);
#26521=PLANE('',#29260);
#26522=PLANE('',#29266);
#26523=PLANE('',#29267);
#26524=PLANE('',#29268);
#26525=PLANE('',#29272);
#26526=PLANE('',#29273);
#26527=PLANE('',#29274);
#26528=PLANE('',#29279);
#26529=PLANE('',#29280);
#26530=PLANE('',#29281);
#26531=PLANE('',#29286);
#26532=PLANE('',#29287);
#26533=PLANE('',#29288);
#26534=PLANE('',#29293);
#26535=PLANE('',#29294);
#26536=PLANE('',#29295);
#26537=PLANE('',#29300);
#26538=PLANE('',#29301);
#26539=PLANE('',#29302);
#26540=PLANE('',#29307);
#26541=PLANE('',#29308);
#26542=PLANE('',#29309);
#26543=PLANE('',#29319);
#26544=PLANE('',#29320);
#26545=PLANE('',#29324);
#26546=PLANE('',#29328);
#26547=PLANE('',#29330);
#26548=PLANE('',#29332);
#26549=PLANE('',#29334);
#26550=PLANE('',#29336);
#26551=PLANE('',#29338);
#26552=PLANE('',#29339);
#26553=PLANE('',#29343);
#26554=PLANE('',#29347);
#26555=PLANE('',#29351);
#26556=PLANE('',#29355);
#26557=PLANE('',#29359);
#26558=PLANE('',#29363);
#26559=PLANE('',#29364);
#26560=PLANE('',#29365);
#26561=PLANE('',#29369);
#26562=PLANE('',#29370);
#26563=PLANE('',#29371);
#26564=PLANE('',#29372);
#26565=PLANE('',#29376);
#26566=PLANE('',#29380);
#26567=PLANE('',#29383);
#26568=PLANE('',#29386);
#26569=PLANE('',#29389);
#26570=PLANE('',#29392);
#26571=PLANE('',#29395);
#26572=PLANE('',#29396);
#26573=PLANE('',#29400);
#26574=PLANE('',#29404);
#26575=PLANE('',#29408);
#26576=PLANE('',#29412);
#26577=PLANE('',#29416);
#26578=PLANE('',#29420);
#26579=PLANE('',#29421);
#26580=PLANE('',#29422);
#26581=PLANE('',#29426);
#26582=PLANE('',#29427);
#26583=PLANE('',#29428);
#26584=PLANE('',#29429);
#26585=PLANE('',#29430);
#26586=PLANE('',#29434);
#26587=PLANE('',#29436);
#26588=PLANE('',#29438);
#26589=PLANE('',#29440);
#26590=PLANE('',#29441);
#26591=PLANE('',#29450);
#26592=PLANE('',#29451);
#26593=PLANE('',#29462);
#26594=PLANE('',#29463);
#26595=PLANE('',#29464);
#26596=PLANE('',#29465);
#26597=PLANE('',#29466);
#26598=PLANE('',#29469);
#26599=PLANE('',#29470);
#26600=PLANE('',#29471);
#26601=PLANE('',#29472);
#26602=PLANE('',#29473);
#26603=PLANE('',#29474);
#26604=PLANE('',#29477);
#26605=PLANE('',#29481);
#26606=PLANE('',#29486);
#26607=PLANE('',#29488);
#26608=PLANE('',#29490);
#26609=PLANE('',#29492);
#26610=PLANE('',#29494);
#26611=PLANE('',#29495);
#26612=PLANE('',#29496);
#26613=PLANE('',#29503);
#26614=PLANE('',#29506);
#26615=PLANE('',#29507);
#26616=PLANE('',#29517);
#26617=PLANE('',#29519);
#26618=PLANE('',#29520);
#26619=PLANE('',#29521);
#26620=PLANE('',#29522);
#26621=PLANE('',#29523);
#26622=PLANE('',#29526);
#26623=PLANE('',#29527);
#26624=PLANE('',#29528);
#26625=PLANE('',#29529);
#26626=PLANE('',#29530);
#26627=PLANE('',#29531);
#26628=PLANE('',#29532);
#26629=PLANE('',#29533);
#26630=PLANE('',#29534);
#26631=PLANE('',#29537);
#26632=PLANE('',#29540);
#26633=PLANE('',#29541);
#26634=PLANE('',#29543);
#26635=PLANE('',#29548);
#26636=PLANE('',#29557);
#26637=PLANE('',#29558);
#26638=PLANE('',#29559);
#26639=PLANE('',#29560);
#26640=PLANE('',#29561);
#26641=PLANE('',#29565);
#26642=PLANE('',#29566);
#26643=PLANE('',#29576);
#26644=PLANE('',#29577);
#26645=PLANE('',#29578);
#26646=PLANE('',#29582);
#26647=PLANE('',#29586);
#26648=PLANE('',#29590);
#26649=PLANE('',#29591);
#26650=PLANE('',#29592);
#26651=PLANE('',#29596);
#26652=PLANE('',#29600);
#26653=PLANE('',#29604);
#26654=PLANE('',#29608);
#26655=PLANE('',#29609);
#26656=PLANE('',#29610);
#26657=PLANE('',#29614);
#26658=PLANE('',#29618);
#26659=PLANE('',#29622);
#26660=PLANE('',#29623);
#26661=PLANE('',#29624);
#26662=PLANE('',#29634);
#26663=PLANE('',#29635);
#26664=PLANE('',#29639);
#26665=PLANE('',#29640);
#26666=PLANE('',#29641);
#26667=PLANE('',#29642);
#26668=PLANE('',#29643);
#26669=PLANE('',#29647);
#26670=PLANE('',#29648);
#26671=PLANE('',#29658);
#26672=PLANE('',#29659);
#26673=PLANE('',#29660);
#26674=PLANE('',#29664);
#26675=PLANE('',#29668);
#26676=PLANE('',#29672);
#26677=PLANE('',#29673);
#26678=PLANE('',#29674);
#26679=PLANE('',#29678);
#26680=PLANE('',#29682);
#26681=PLANE('',#29686);
#26682=PLANE('',#29690);
#26683=PLANE('',#29691);
#26684=PLANE('',#29692);
#26685=PLANE('',#29696);
#26686=PLANE('',#29700);
#26687=PLANE('',#29704);
#26688=PLANE('',#29705);
#26689=PLANE('',#29706);
#26690=PLANE('',#29716);
#26691=PLANE('',#29717);
#26692=PLANE('',#29718);
#26693=PLANE('',#29719);
#26694=PLANE('',#29994);
#26695=PLANE('',#29998);
#26696=PLANE('',#30003);
#26697=PLANE('',#30007);
#26698=PLANE('',#30012);
#26699=PLANE('',#30013);
#26700=PLANE('',#30014);
#26701=PLANE('',#30015);
#26702=PLANE('',#30016);
#26703=PLANE('',#30029);
#26704=PLANE('',#30030);
#26705=PLANE('',#30031);
#26706=PLANE('',#30032);
#26707=PLANE('',#30033);
#26708=PLANE('',#30034);
#26709=PLANE('',#30035);
#26710=PLANE('',#30039);
#26711=PLANE('',#30043);
#26712=PLANE('',#30047);
#26713=PLANE('',#30048);
#26714=PLANE('',#30049);
#26715=PLANE('',#30052);
#26716=PLANE('',#30053);
#26717=PLANE('',#30054);
#26718=PLANE('',#30055);
#26719=PLANE('',#30056);
#26720=PLANE('',#30057);
#26721=PLANE('',#30058);
#26722=PLANE('',#30062);
#26723=PLANE('',#30063);
#26724=PLANE('',#30064);
#26725=PLANE('',#30067);
#26726=PLANE('',#30068);
#26727=PLANE('',#30071);
#26728=PLANE('',#30075);
#26729=PLANE('',#30079);
#26730=PLANE('',#30080);
#26731=PLANE('',#30081);
#26732=PLANE('',#30084);
#26733=PLANE('',#30085);
#26734=PLANE('',#30086);
#26735=PLANE('',#30087);
#26736=PLANE('',#30088);
#26737=PLANE('',#30089);
#26738=PLANE('',#30090);
#26739=PLANE('',#30094);
#26740=PLANE('',#30095);
#26741=PLANE('',#30096);
#26742=PLANE('',#30097);
#26743=PLANE('',#30098);
#26744=PLANE('',#30099);
#26745=PLANE('',#30100);
#26746=PLANE('',#30101);
#26747=PLANE('',#30105);
#26748=PLANE('',#30106);
#26749=PLANE('',#30107);
#26750=PLANE('',#30108);
#26751=PLANE('',#30109);
#26752=PLANE('',#30112);
#26753=PLANE('',#30115);
#26754=PLANE('',#30118);
#26755=PLANE('',#30121);
#26756=PLANE('',#30122);
#26757=PLANE('',#30127);
#26758=PLANE('',#30130);
#26759=PLANE('',#30133);
#26760=PLANE('',#30138);
#26761=PLANE('',#30141);
#26762=PLANE('',#30144);
#26763=PLANE('',#30147);
#26764=PLANE('',#30150);
#26765=PLANE('',#30153);
#26766=PLANE('',#30156);
#26767=ADVANCED_FACE('',(#2964),#26335,.F.);
#26768=ADVANCED_FACE('',(#2965),#26336,.T.);
#26769=ADVANCED_FACE('',(#2966),#26337,.T.);
#26770=ADVANCED_FACE('',(#2967),#2155,.F.);
#26771=ADVANCED_FACE('',(#2968),#26338,.T.);
#26772=ADVANCED_FACE('',(#2969),#2156,.T.);
#26773=ADVANCED_FACE('',(#2970),#26339,.T.);
#26774=ADVANCED_FACE('',(#2971),#2157,.T.);
#26775=ADVANCED_FACE('',(#2972),#26340,.T.);
#26776=ADVANCED_FACE('',(#2973),#2158,.F.);
#26777=ADVANCED_FACE('',(#2974),#26341,.T.);
#26778=ADVANCED_FACE('',(#2975),#2159,.T.);
#26779=ADVANCED_FACE('',(#2976),#26342,.T.);
#26780=ADVANCED_FACE('',(#2977),#26343,.T.);
#26781=ADVANCED_FACE('',(#2978),#2160,.T.);
#26782=ADVANCED_FACE('',(#2979),#26344,.T.);
#26783=ADVANCED_FACE('',(#2980),#2161,.F.);
#26784=ADVANCED_FACE('',(#2981),#26345,.T.);
#26785=ADVANCED_FACE('',(#2982),#2162,.T.);
#26786=ADVANCED_FACE('',(#2983),#26346,.T.);
#26787=ADVANCED_FACE('',(#2984),#2163,.T.);
#26788=ADVANCED_FACE('',(#2985),#26347,.T.);
#26789=ADVANCED_FACE('',(#2986),#2164,.F.);
#26790=ADVANCED_FACE('',(#2987),#26348,.T.);
#26791=ADVANCED_FACE('',(#2988),#26349,.T.);
#26792=ADVANCED_FACE('',(#2989),#26350,.T.);
#26793=ADVANCED_FACE('',(#2990),#26351,.T.);
#26794=ADVANCED_FACE('',(#2991),#26352,.F.);
#26795=ADVANCED_FACE('',(#2992),#2165,.F.);
#26796=ADVANCED_FACE('',(#2993),#26353,.T.);
#26797=ADVANCED_FACE('',(#2994),#2166,.F.);
#26798=ADVANCED_FACE('',(#2995),#26354,.T.);
#26799=ADVANCED_FACE('',(#2996),#2167,.T.);
#26800=ADVANCED_FACE('',(#2997),#26355,.T.);
#26801=ADVANCED_FACE('',(#2998),#26356,.T.);
#26802=ADVANCED_FACE('',(#2999),#26357,.T.);
#26803=ADVANCED_FACE('',(#3000),#26358,.T.);
#26804=ADVANCED_FACE('',(#3001),#26359,.T.);
#26805=ADVANCED_FACE('',(#3002),#26360,.T.);
#26806=ADVANCED_FACE('',(#3003),#2168,.T.);
#26807=ADVANCED_FACE('',(#3004),#26361,.T.);
#26808=ADVANCED_FACE('',(#3005),#2169,.T.);
#26809=ADVANCED_FACE('',(#3006),#26362,.T.);
#26810=ADVANCED_FACE('',(#3007),#2170,.T.);
#26811=ADVANCED_FACE('',(#3008),#26363,.T.);
#26812=ADVANCED_FACE('',(#3009),#2171,.T.);
#26813=ADVANCED_FACE('',(#3010),#26364,.T.);
#26814=ADVANCED_FACE('',(#3011),#26365,.T.);
#26815=ADVANCED_FACE('',(#3012),#26366,.T.);
#26816=ADVANCED_FACE('',(#3013),#26367,.T.);
#26817=ADVANCED_FACE('',(#3014),#26368,.T.);
#26818=ADVANCED_FACE('',(#3015),#26369,.T.);
#26819=ADVANCED_FACE('',(#3016),#2172,.T.);
#26820=ADVANCED_FACE('',(#3017),#26370,.T.);
#26821=ADVANCED_FACE('',(#3018),#26371,.T.);
#26822=ADVANCED_FACE('',(#3019),#2173,.F.);
#26823=ADVANCED_FACE('',(#3020),#2174,.F.);
#26824=ADVANCED_FACE('',(#3021),#2175,.F.);
#26825=ADVANCED_FACE('',(#3022),#2176,.F.);
#26826=ADVANCED_FACE('',(#3023),#2177,.F.);
#26827=ADVANCED_FACE('',(#3024),#2178,.F.);
#26828=ADVANCED_FACE('',(#3025),#2179,.F.);
#26829=ADVANCED_FACE('',(#3026),#2180,.F.);
#26830=ADVANCED_FACE('',(#3027),#2181,.F.);
#26831=ADVANCED_FACE('',(#3028),#2182,.F.);
#26832=ADVANCED_FACE('',(#3029),#2183,.F.);
#26833=ADVANCED_FACE('',(#3030),#2184,.F.);
#26834=ADVANCED_FACE('',(#3031),#2185,.F.);
#26835=ADVANCED_FACE('',(#3032),#2186,.F.);
#26836=ADVANCED_FACE('',(#3033),#2187,.F.);
#26837=ADVANCED_FACE('',(#3034),#2188,.F.);
#26838=ADVANCED_FACE('',(#3035),#2189,.F.);
#26839=ADVANCED_FACE('',(#3036),#2190,.F.);
#26840=ADVANCED_FACE('',(#3037),#2191,.F.);
#26841=ADVANCED_FACE('',(#3038),#2192,.F.);
#26842=ADVANCED_FACE('',(#3039),#2193,.F.);
#26843=ADVANCED_FACE('',(#3040),#2194,.F.);
#26844=ADVANCED_FACE('',(#3041),#2195,.F.);
#26845=ADVANCED_FACE('',(#3042),#2196,.F.);
#26846=ADVANCED_FACE('',(#3043),#2197,.F.);
#26847=ADVANCED_FACE('',(#3044),#2198,.F.);
#26848=ADVANCED_FACE('',(#3045),#2199,.F.);
#26849=ADVANCED_FACE('',(#3046),#2200,.F.);
#26850=ADVANCED_FACE('',(#3047),#2201,.F.);
#26851=ADVANCED_FACE('',(#3048),#2202,.F.);
#26852=ADVANCED_FACE('',(#3049),#2203,.F.);
#26853=ADVANCED_FACE('',(#3050),#2204,.F.);
#26854=ADVANCED_FACE('',(#3051),#2205,.F.);
#26855=ADVANCED_FACE('',(#3052),#2206,.F.);
#26856=ADVANCED_FACE('',(#3053),#2207,.F.);
#26857=ADVANCED_FACE('',(#3054),#2208,.F.);
#26858=ADVANCED_FACE('',(#3055),#2209,.F.);
#26859=ADVANCED_FACE('',(#3056),#2210,.F.);
#26860=ADVANCED_FACE('',(#3057),#2211,.F.);
#26861=ADVANCED_FACE('',(#3058),#2212,.F.);
#26862=ADVANCED_FACE('',(#3059),#2213,.F.);
#26863=ADVANCED_FACE('',(#3060),#2214,.F.);
#26864=ADVANCED_FACE('',(#3061),#2215,.F.);
#26865=ADVANCED_FACE('',(#3062),#2216,.F.);
#26866=ADVANCED_FACE('',(#3063),#2217,.F.);
#26867=ADVANCED_FACE('',(#3064),#2218,.F.);
#26868=ADVANCED_FACE('',(#3065),#2219,.F.);
#26869=ADVANCED_FACE('',(#3066),#2220,.F.);
#26870=ADVANCED_FACE('',(#3067),#2221,.F.);
#26871=ADVANCED_FACE('',(#3068),#2222,.F.);
#26872=ADVANCED_FACE('',(#3069),#2223,.F.);
#26873=ADVANCED_FACE('',(#3070),#2224,.F.);
#26874=ADVANCED_FACE('',(#3071),#2225,.F.);
#26875=ADVANCED_FACE('',(#3072),#2226,.F.);
#26876=ADVANCED_FACE('',(#3073),#2227,.F.);
#26877=ADVANCED_FACE('',(#3074),#2228,.F.);
#26878=ADVANCED_FACE('',(#3075),#2229,.F.);
#26879=ADVANCED_FACE('',(#3076),#2230,.F.);
#26880=ADVANCED_FACE('',(#3077),#2231,.F.);
#26881=ADVANCED_FACE('',(#3078),#2232,.F.);
#26882=ADVANCED_FACE('',(#3079),#2233,.F.);
#26883=ADVANCED_FACE('',(#3080),#2234,.F.);
#26884=ADVANCED_FACE('',(#3081),#2235,.F.);
#26885=ADVANCED_FACE('',(#3082),#2236,.F.);
#26886=ADVANCED_FACE('',(#3083),#2237,.F.);
#26887=ADVANCED_FACE('',(#3084),#2238,.F.);
#26888=ADVANCED_FACE('',(#3085),#2239,.F.);
#26889=ADVANCED_FACE('',(#3086),#2240,.F.);
#26890=ADVANCED_FACE('',(#3087),#2241,.F.);
#26891=ADVANCED_FACE('',(#3088),#2242,.F.);
#26892=ADVANCED_FACE('',(#3089),#2243,.F.);
#26893=ADVANCED_FACE('',(#3090),#2244,.F.);
#26894=ADVANCED_FACE('',(#3091),#2245,.F.);
#26895=ADVANCED_FACE('',(#3092),#2246,.F.);
#26896=ADVANCED_FACE('',(#3093),#2247,.F.);
#26897=ADVANCED_FACE('',(#3094),#2248,.F.);
#26898=ADVANCED_FACE('',(#3095),#2249,.F.);
#26899=ADVANCED_FACE('',(#3096),#2250,.F.);
#26900=ADVANCED_FACE('',(#3097),#2251,.F.);
#26901=ADVANCED_FACE('',(#3098),#2252,.F.);
#26902=ADVANCED_FACE('',(#3099),#2253,.F.);
#26903=ADVANCED_FACE('',(#3100),#2254,.F.);
#26904=ADVANCED_FACE('',(#3101),#2255,.F.);
#26905=ADVANCED_FACE('',(#3102),#2256,.F.);
#26906=ADVANCED_FACE('',(#3103),#2257,.F.);
#26907=ADVANCED_FACE('',(#3104),#2258,.F.);
#26908=ADVANCED_FACE('',(#3105),#2259,.F.);
#26909=ADVANCED_FACE('',(#3106),#2260,.F.);
#26910=ADVANCED_FACE('',(#3107),#2261,.F.);
#26911=ADVANCED_FACE('',(#3108),#2262,.F.);
#26912=ADVANCED_FACE('',(#3109),#2263,.F.);
#26913=ADVANCED_FACE('',(#3110),#2264,.F.);
#26914=ADVANCED_FACE('',(#3111),#2265,.F.);
#26915=ADVANCED_FACE('',(#3112),#2266,.F.);
#26916=ADVANCED_FACE('',(#3113),#2267,.F.);
#26917=ADVANCED_FACE('',(#3114),#2268,.F.);
#26918=ADVANCED_FACE('',(#3115),#2269,.F.);
#26919=ADVANCED_FACE('',(#3116),#2270,.F.);
#26920=ADVANCED_FACE('',(#3117),#2271,.F.);
#26921=ADVANCED_FACE('',(#3118),#2272,.F.);
#26922=ADVANCED_FACE('',(#3119),#2273,.F.);
#26923=ADVANCED_FACE('',(#3120),#2274,.F.);
#26924=ADVANCED_FACE('',(#3121),#2275,.F.);
#26925=ADVANCED_FACE('',(#3122),#2276,.F.);
#26926=ADVANCED_FACE('',(#3123),#2277,.F.);
#26927=ADVANCED_FACE('',(#3124),#2278,.F.);
#26928=ADVANCED_FACE('',(#3125),#2279,.F.);
#26929=ADVANCED_FACE('',(#3126),#2280,.F.);
#26930=ADVANCED_FACE('',(#3127),#2281,.F.);
#26931=ADVANCED_FACE('',(#3128),#2282,.F.);
#26932=ADVANCED_FACE('',(#3129),#2283,.F.);
#26933=ADVANCED_FACE('',(#3130),#2284,.F.);
#26934=ADVANCED_FACE('',(#3131),#2285,.F.);
#26935=ADVANCED_FACE('',(#3132),#2286,.F.);
#26936=ADVANCED_FACE('',(#3133),#2287,.F.);
#26937=ADVANCED_FACE('',(#3134),#2288,.F.);
#26938=ADVANCED_FACE('',(#3135),#2289,.F.);
#26939=ADVANCED_FACE('',(#3136),#2290,.F.);
#26940=ADVANCED_FACE('',(#3137),#2291,.F.);
#26941=ADVANCED_FACE('',(#3138),#2292,.F.);
#26942=ADVANCED_FACE('',(#3139),#2293,.F.);
#26943=ADVANCED_FACE('',(#3140),#2294,.F.);
#26944=ADVANCED_FACE('',(#3141),#2295,.F.);
#26945=ADVANCED_FACE('',(#3142),#2296,.F.);
#26946=ADVANCED_FACE('',(#3143),#2297,.F.);
#26947=ADVANCED_FACE('',(#3144),#2298,.F.);
#26948=ADVANCED_FACE('',(#3145),#2299,.F.);
#26949=ADVANCED_FACE('',(#3146),#2300,.F.);
#26950=ADVANCED_FACE('',(#3147),#2301,.F.);
#26951=ADVANCED_FACE('',(#3148),#2302,.F.);
#26952=ADVANCED_FACE('',(#3149),#2303,.F.);
#26953=ADVANCED_FACE('',(#3150),#2304,.F.);
#26954=ADVANCED_FACE('',(#3151),#2305,.F.);
#26955=ADVANCED_FACE('',(#3152),#2306,.F.);
#26956=ADVANCED_FACE('',(#3153),#2307,.F.);
#26957=ADVANCED_FACE('',(#3154),#2308,.F.);
#26958=ADVANCED_FACE('',(#3155),#2309,.F.);
#26959=ADVANCED_FACE('',(#3156),#2310,.F.);
#26960=ADVANCED_FACE('',(#3157),#2311,.F.);
#26961=ADVANCED_FACE('',(#3158),#2312,.F.);
#26962=ADVANCED_FACE('',(#3159),#2313,.F.);
#26963=ADVANCED_FACE('',(#3160),#2314,.F.);
#26964=ADVANCED_FACE('',(#3161),#2315,.F.);
#26965=ADVANCED_FACE('',(#3162),#2316,.F.);
#26966=ADVANCED_FACE('',(#3163),#2317,.F.);
#26967=ADVANCED_FACE('',(#3164),#2318,.F.);
#26968=ADVANCED_FACE('',(#3165),#2319,.F.);
#26969=ADVANCED_FACE('',(#3166),#2320,.F.);
#26970=ADVANCED_FACE('',(#3167),#2321,.F.);
#26971=ADVANCED_FACE('',(#3168),#2322,.F.);
#26972=ADVANCED_FACE('',(#3169),#2323,.F.);
#26973=ADVANCED_FACE('',(#3170),#2324,.F.);
#26974=ADVANCED_FACE('',(#3171),#2325,.F.);
#26975=ADVANCED_FACE('',(#3172),#2326,.F.);
#26976=ADVANCED_FACE('',(#3173),#2327,.F.);
#26977=ADVANCED_FACE('',(#3174),#2328,.F.);
#26978=ADVANCED_FACE('',(#3175),#2329,.F.);
#26979=ADVANCED_FACE('',(#3176),#2330,.F.);
#26980=ADVANCED_FACE('',(#3177),#2331,.F.);
#26981=ADVANCED_FACE('',(#3178),#2332,.F.);
#26982=ADVANCED_FACE('',(#3179),#2333,.F.);
#26983=ADVANCED_FACE('',(#3180),#2334,.F.);
#26984=ADVANCED_FACE('',(#3181),#2335,.F.);
#26985=ADVANCED_FACE('',(#3182),#2336,.F.);
#26986=ADVANCED_FACE('',(#3183),#2337,.F.);
#26987=ADVANCED_FACE('',(#3184),#2338,.F.);
#26988=ADVANCED_FACE('',(#3185),#2339,.F.);
#26989=ADVANCED_FACE('',(#3186),#2340,.F.);
#26990=ADVANCED_FACE('',(#3187),#2341,.F.);
#26991=ADVANCED_FACE('',(#3188),#2342,.F.);
#26992=ADVANCED_FACE('',(#3189),#2343,.F.);
#26993=ADVANCED_FACE('',(#3190),#2344,.F.);
#26994=ADVANCED_FACE('',(#3191),#2345,.F.);
#26995=ADVANCED_FACE('',(#3192),#2346,.F.);
#26996=ADVANCED_FACE('',(#3193),#2347,.F.);
#26997=ADVANCED_FACE('',(#3194),#2348,.F.);
#26998=ADVANCED_FACE('',(#3195),#2349,.F.);
#26999=ADVANCED_FACE('',(#3196),#2350,.F.);
#27000=ADVANCED_FACE('',(#3197),#2351,.F.);
#27001=ADVANCED_FACE('',(#3198),#2352,.F.);
#27002=ADVANCED_FACE('',(#3199),#2353,.F.);
#27003=ADVANCED_FACE('',(#3200),#2354,.F.);
#27004=ADVANCED_FACE('',(#3201),#2355,.F.);
#27005=ADVANCED_FACE('',(#3202),#2356,.F.);
#27006=ADVANCED_FACE('',(#3203),#2357,.F.);
#27007=ADVANCED_FACE('',(#3204),#2358,.F.);
#27008=ADVANCED_FACE('',(#3205),#2359,.F.);
#27009=ADVANCED_FACE('',(#3206),#2360,.F.);
#27010=ADVANCED_FACE('',(#3207),#2361,.F.);
#27011=ADVANCED_FACE('',(#3208),#2362,.F.);
#27012=ADVANCED_FACE('',(#3209),#2363,.F.);
#27013=ADVANCED_FACE('',(#3210),#2364,.F.);
#27014=ADVANCED_FACE('',(#3211),#2365,.F.);
#27015=ADVANCED_FACE('',(#3212),#2366,.F.);
#27016=ADVANCED_FACE('',(#3213),#2367,.F.);
#27017=ADVANCED_FACE('',(#3214),#2368,.F.);
#27018=ADVANCED_FACE('',(#3215),#2369,.F.);
#27019=ADVANCED_FACE('',(#3216),#2370,.F.);
#27020=ADVANCED_FACE('',(#3217),#2371,.F.);
#27021=ADVANCED_FACE('',(#3218),#2372,.F.);
#27022=ADVANCED_FACE('',(#3219),#2373,.F.);
#27023=ADVANCED_FACE('',(#3220),#2374,.F.);
#27024=ADVANCED_FACE('',(#3221),#2375,.F.);
#27025=ADVANCED_FACE('',(#3222),#2376,.F.);
#27026=ADVANCED_FACE('',(#3223),#2377,.F.);
#27027=ADVANCED_FACE('',(#3224),#2378,.F.);
#27028=ADVANCED_FACE('',(#3225),#2379,.F.);
#27029=ADVANCED_FACE('',(#3226),#2380,.F.);
#27030=ADVANCED_FACE('',(#3227),#2381,.F.);
#27031=ADVANCED_FACE('',(#3228),#2382,.F.);
#27032=ADVANCED_FACE('',(#3229),#2383,.F.);
#27033=ADVANCED_FACE('',(#3230),#2384,.F.);
#27034=ADVANCED_FACE('',(#3231),#2385,.F.);
#27035=ADVANCED_FACE('',(#3232),#2386,.F.);
#27036=ADVANCED_FACE('',(#3233),#2387,.F.);
#27037=ADVANCED_FACE('',(#3234),#2388,.F.);
#27038=ADVANCED_FACE('',(#3235),#2389,.F.);
#27039=ADVANCED_FACE('',(#3236),#2390,.F.);
#27040=ADVANCED_FACE('',(#3237),#2391,.F.);
#27041=ADVANCED_FACE('',(#3238),#2392,.F.);
#27042=ADVANCED_FACE('',(#3239),#2393,.F.);
#27043=ADVANCED_FACE('',(#3240),#2394,.F.);
#27044=ADVANCED_FACE('',(#3241),#2395,.F.);
#27045=ADVANCED_FACE('',(#3242),#2396,.F.);
#27046=ADVANCED_FACE('',(#3243),#2397,.F.);
#27047=ADVANCED_FACE('',(#3244),#2398,.F.);
#27048=ADVANCED_FACE('',(#3245),#2399,.F.);
#27049=ADVANCED_FACE('',(#3246),#2400,.F.);
#27050=ADVANCED_FACE('',(#3247),#2401,.F.);
#27051=ADVANCED_FACE('',(#3248),#2402,.F.);
#27052=ADVANCED_FACE('',(#3249),#2403,.F.);
#27053=ADVANCED_FACE('',(#3250),#2404,.F.);
#27054=ADVANCED_FACE('',(#3251),#2405,.F.);
#27055=ADVANCED_FACE('',(#3252),#2406,.F.);
#27056=ADVANCED_FACE('',(#3253),#2407,.F.);
#27057=ADVANCED_FACE('',(#3254),#2408,.F.);
#27058=ADVANCED_FACE('',(#3255),#2409,.F.);
#27059=ADVANCED_FACE('',(#3256),#2410,.F.);
#27060=ADVANCED_FACE('',(#3257),#2411,.F.);
#27061=ADVANCED_FACE('',(#3258),#2412,.F.);
#27062=ADVANCED_FACE('',(#3259),#2413,.F.);
#27063=ADVANCED_FACE('',(#3260),#2414,.F.);
#27064=ADVANCED_FACE('',(#3261),#2415,.F.);
#27065=ADVANCED_FACE('',(#3262),#2416,.F.);
#27066=ADVANCED_FACE('',(#3263),#2417,.F.);
#27067=ADVANCED_FACE('',(#3264),#26372,.T.);
#27068=ADVANCED_FACE('',(#3265),#2418,.F.);
#27069=ADVANCED_FACE('',(#3266),#26373,.T.);
#27070=ADVANCED_FACE('',(#3267),#2419,.F.);
#27071=ADVANCED_FACE('',(#3268),#26374,.T.);
#27072=ADVANCED_FACE('',(#3269),#2420,.F.);
#27073=ADVANCED_FACE('',(#3270),#26375,.T.);
#27074=ADVANCED_FACE('',(#3271),#2421,.F.);
#27075=ADVANCED_FACE('',(#3272),#26376,.T.);
#27076=ADVANCED_FACE('',(#3273),#26377,.T.);
#27077=ADVANCED_FACE('',(#3274),#26378,.T.);
#27078=ADVANCED_FACE('',(#3275),#26379,.T.);
#27079=ADVANCED_FACE('',(#3276,#173,#174,#175,#176,#177,#178,#179,#180,
#181),#26380,.F.);
#27080=ADVANCED_FACE('',(#3277),#149,.F.);
#27081=ADVANCED_FACE('',(#3278),#150,.F.);
#27082=ADVANCED_FACE('',(#3279),#151,.F.);
#27083=ADVANCED_FACE('',(#3280),#152,.F.);
#27084=ADVANCED_FACE('',(#3281),#153,.F.);
#27085=ADVANCED_FACE('',(#3282),#154,.F.);
#27086=ADVANCED_FACE('',(#3283),#155,.F.);
#27087=ADVANCED_FACE('',(#3284),#156,.F.);
#27088=ADVANCED_FACE('',(#3285),#157,.F.);
#27089=ADVANCED_FACE('',(#3286),#158,.F.);
#27090=ADVANCED_FACE('',(#3287),#159,.F.);
#27091=ADVANCED_FACE('',(#3288),#160,.F.);
#27092=ADVANCED_FACE('',(#3289),#26381,.T.);
#27093=ADVANCED_FACE('',(#3290),#26382,.T.);
#27094=ADVANCED_FACE('',(#3291),#26383,.T.);
#27095=ADVANCED_FACE('',(#3292),#26384,.T.);
#27096=ADVANCED_FACE('',(#3293),#26385,.T.);
#27097=ADVANCED_FACE('',(#3294),#26386,.T.);
#27098=ADVANCED_FACE('',(#3295),#26387,.T.);
#27099=ADVANCED_FACE('',(#3296),#2422,.F.);
#27100=ADVANCED_FACE('',(#3297,#182),#26388,.F.);
#27101=ADVANCED_FACE('',(#3298),#2423,.F.);
#27102=ADVANCED_FACE('',(#3299),#26389,.T.);
#27103=ADVANCED_FACE('',(#3300),#2424,.F.);
#27104=ADVANCED_FACE('',(#3301),#26390,.T.);
#27105=ADVANCED_FACE('',(#3302),#26391,.T.);
#27106=ADVANCED_FACE('',(#3303,#183,#184,#185),#26392,.F.);
#27107=ADVANCED_FACE('',(#3304),#26393,.T.);
#27108=ADVANCED_FACE('',(#3305),#26394,.T.);
#27109=ADVANCED_FACE('',(#3306),#26395,.T.);
#27110=ADVANCED_FACE('',(#3307),#26396,.T.);
#27111=ADVANCED_FACE('',(#3308),#26397,.T.);
#27112=ADVANCED_FACE('',(#3309),#26398,.T.);
#27113=ADVANCED_FACE('',(#3310),#26399,.T.);
#27114=ADVANCED_FACE('',(#3311),#2425,.F.);
#27115=ADVANCED_FACE('',(#3312,#186),#26400,.F.);
#27116=ADVANCED_FACE('',(#3313),#26401,.T.);
#27117=ADVANCED_FACE('',(#3314),#26402,.T.);
#27118=ADVANCED_FACE('',(#3315),#2426,.F.);
#27119=ADVANCED_FACE('',(#3316),#26403,.F.);
#27120=ADVANCED_FACE('',(#3317),#26404,.F.);
#27121=ADVANCED_FACE('',(#3318),#2427,.F.);
#27122=ADVANCED_FACE('',(#3319),#26405,.F.);
#27123=ADVANCED_FACE('',(#3320),#2428,.F.);
#27124=ADVANCED_FACE('',(#3321),#26406,.F.);
#27125=ADVANCED_FACE('',(#3322),#2429,.F.);
#27126=ADVANCED_FACE('',(#3323),#26407,.F.);
#27127=ADVANCED_FACE('',(#3324),#26408,.F.);
#27128=ADVANCED_FACE('',(#3325,#187,#188,#189),#26409,.T.);
#27129=ADVANCED_FACE('',(#3326),#26410,.F.);
#27130=ADVANCED_FACE('',(#3327),#26411,.F.);
#27131=ADVANCED_FACE('',(#3328),#26412,.F.);
#27132=ADVANCED_FACE('',(#3329),#26413,.F.);
#27133=ADVANCED_FACE('',(#3330),#26414,.F.);
#27134=ADVANCED_FACE('',(#3331),#26415,.F.);
#27135=ADVANCED_FACE('',(#3332),#26416,.F.);
#27136=ADVANCED_FACE('',(#3333),#2430,.F.);
#27137=ADVANCED_FACE('',(#3334,#190),#26417,.T.);
#27138=ADVANCED_FACE('',(#3335),#26418,.F.);
#27139=ADVANCED_FACE('',(#3336),#26419,.F.);
#27140=ADVANCED_FACE('',(#3337),#26420,.F.);
#27141=ADVANCED_FACE('',(#3338),#26421,.F.);
#27142=ADVANCED_FACE('',(#3339),#26422,.F.);
#27143=ADVANCED_FACE('',(#3340),#26423,.F.);
#27144=ADVANCED_FACE('',(#3341),#26424,.F.);
#27145=ADVANCED_FACE('',(#3342),#2431,.F.);
#27146=ADVANCED_FACE('',(#3343,#191),#26425,.T.);
#27147=ADVANCED_FACE('',(#3344),#26426,.T.);
#27148=ADVANCED_FACE('',(#3345),#26427,.T.);
#27149=ADVANCED_FACE('',(#3346,#192,#193),#26428,.T.);
#27150=ADVANCED_FACE('',(#3347),#26429,.T.);
#27151=ADVANCED_FACE('',(#3348),#2432,.F.);
#27152=ADVANCED_FACE('',(#3349),#26430,.T.);
#27153=ADVANCED_FACE('',(#3350),#2433,.F.);
#27154=ADVANCED_FACE('',(#3351),#26431,.T.);
#27155=ADVANCED_FACE('',(#3352),#2434,.F.);
#27156=ADVANCED_FACE('',(#3353),#26432,.T.);
#27157=ADVANCED_FACE('',(#3354),#2435,.F.);
#27158=ADVANCED_FACE('',(#3355),#26433,.T.);
#27159=ADVANCED_FACE('',(#3356),#26434,.T.);
#27160=ADVANCED_FACE('',(#3357),#2436,.T.);
#27161=ADVANCED_FACE('',(#3358),#2437,.F.);
#27162=ADVANCED_FACE('',(#3359),#26435,.T.);
#27163=ADVANCED_FACE('',(#3360),#2438,.T.);
#27164=ADVANCED_FACE('',(#3361),#26436,.T.);
#27165=ADVANCED_FACE('',(#3362),#2439,.T.);
#27166=ADVANCED_FACE('',(#3363),#26437,.T.);
#27167=ADVANCED_FACE('',(#3364),#2440,.T.);
#27168=ADVANCED_FACE('',(#3365),#2441,.T.);
#27169=ADVANCED_FACE('',(#3366),#26438,.T.);
#27170=ADVANCED_FACE('',(#3367),#2442,.T.);
#27171=ADVANCED_FACE('',(#3368,#194,#195),#26439,.T.);
#27172=ADVANCED_FACE('',(#3369),#2443,.T.);
#27173=ADVANCED_FACE('',(#3370),#26440,.T.);
#27174=ADVANCED_FACE('',(#3371),#2444,.T.);
#27175=ADVANCED_FACE('',(#3372),#26441,.T.);
#27176=ADVANCED_FACE('',(#3373),#2445,.T.);
#27177=ADVANCED_FACE('',(#3374),#26442,.T.);
#27178=ADVANCED_FACE('',(#3375),#2446,.F.);
#27179=ADVANCED_FACE('',(#3376),#26443,.T.);
#27180=ADVANCED_FACE('',(#3377),#2447,.T.);
#27181=ADVANCED_FACE('',(#3378,#196,#197,#198,#199),#26444,.T.);
#27182=ADVANCED_FACE('',(#3379),#2448,.F.);
#27183=ADVANCED_FACE('',(#3380),#26445,.F.);
#27184=ADVANCED_FACE('',(#3381),#2449,.F.);
#27185=ADVANCED_FACE('',(#3382),#26446,.T.);
#27186=ADVANCED_FACE('',(#3383),#2450,.T.);
#27187=ADVANCED_FACE('',(#3384),#2451,.T.);
#27188=ADVANCED_FACE('',(#3385),#2452,.T.);
#27189=ADVANCED_FACE('',(#3386),#63,.T.);
#27190=ADVANCED_FACE('',(#3387),#2453,.T.);
#27191=ADVANCED_FACE('',(#3388),#64,.T.);
#27192=ADVANCED_FACE('',(#3389),#2454,.T.);
#27193=ADVANCED_FACE('',(#3390),#65,.T.);
#27194=ADVANCED_FACE('',(#3391),#2455,.T.);
#27195=ADVANCED_FACE('',(#3392),#55,.F.);
#27196=ADVANCED_FACE('',(#3393),#2456,.T.);
#27197=ADVANCED_FACE('',(#3394),#2457,.T.);
#27198=ADVANCED_FACE('',(#3395),#2458,.T.);
#27199=ADVANCED_FACE('',(#3396),#66,.T.);
#27200=ADVANCED_FACE('',(#3397),#2459,.T.);
#27201=ADVANCED_FACE('',(#3398),#2460,.T.);
#27202=ADVANCED_FACE('',(#3399),#2461,.T.);
#27203=ADVANCED_FACE('',(#3400),#67,.T.);
#27204=ADVANCED_FACE('',(#3401),#2462,.T.);
#27205=ADVANCED_FACE('',(#3402),#2463,.T.);
#27206=ADVANCED_FACE('',(#3403),#2464,.T.);
#27207=ADVANCED_FACE('',(#3404),#56,.F.);
#27208=ADVANCED_FACE('',(#3405),#2465,.T.);
#27209=ADVANCED_FACE('',(#3406),#68,.T.);
#27210=ADVANCED_FACE('',(#3407),#2466,.T.);
#27211=ADVANCED_FACE('',(#3408),#69,.T.);
#27212=ADVANCED_FACE('',(#3409),#2467,.T.);
#27213=ADVANCED_FACE('',(#3410),#70,.T.);
#27214=ADVANCED_FACE('',(#3411),#2468,.T.);
#27215=ADVANCED_FACE('',(#3412),#2469,.T.);
#27216=ADVANCED_FACE('',(#3413),#2470,.T.);
#27217=ADVANCED_FACE('',(#3414),#2471,.T.);
#27218=ADVANCED_FACE('',(#3415),#47,.T.);
#27219=ADVANCED_FACE('',(#3416),#48,.T.);
#27220=ADVANCED_FACE('',(#3417),#26447,.T.);
#27221=ADVANCED_FACE('',(#3418),#2472,.F.);
#27222=ADVANCED_FACE('',(#3419),#26448,.T.);
#27223=ADVANCED_FACE('',(#3420),#26449,.T.);
#27224=ADVANCED_FACE('',(#3421),#26450,.T.);
#27225=ADVANCED_FACE('',(#3422),#2473,.T.);
#27226=ADVANCED_FACE('',(#3423,#200),#26451,.T.);
#27227=ADVANCED_FACE('',(#3424),#2474,.T.);
#27228=ADVANCED_FACE('',(#3425),#26452,.T.);
#27229=ADVANCED_FACE('',(#3426),#2475,.T.);
#27230=ADVANCED_FACE('',(#3427),#26453,.T.);
#27231=ADVANCED_FACE('',(#3428),#2476,.F.);
#27232=ADVANCED_FACE('',(#3429),#26454,.T.);
#27233=ADVANCED_FACE('',(#3430),#2477,.T.);
#27234=ADVANCED_FACE('',(#3431),#26455,.T.);
#27235=ADVANCED_FACE('',(#3432),#26456,.T.);
#27236=ADVANCED_FACE('',(#3433),#26457,.T.);
#27237=ADVANCED_FACE('',(#3434),#26458,.F.);
#27238=ADVANCED_FACE('',(#3435),#2478,.T.);
#27239=ADVANCED_FACE('',(#3436),#71,.T.);
#27240=ADVANCED_FACE('',(#3437),#2479,.T.);
#27241=ADVANCED_FACE('',(#3438),#2480,.T.);
#27242=ADVANCED_FACE('',(#3439),#2481,.T.);
#27243=ADVANCED_FACE('',(#3440),#49,.T.);
#27244=ADVANCED_FACE('',(#3441),#72,.T.);
#27245=ADVANCED_FACE('',(#3442),#2482,.T.);
#27246=ADVANCED_FACE('',(#3443),#50,.T.);
#27247=ADVANCED_FACE('',(#3444),#2483,.T.);
#27248=ADVANCED_FACE('',(#3445),#26459,.T.);
#27249=ADVANCED_FACE('',(#3446),#2484,.T.);
#27250=ADVANCED_FACE('',(#3447),#73,.T.);
#27251=ADVANCED_FACE('',(#3448),#2485,.T.);
#27252=ADVANCED_FACE('',(#3449),#57,.F.);
#27253=ADVANCED_FACE('',(#3450),#2486,.T.);
#27254=ADVANCED_FACE('',(#3451),#74,.T.);
#27255=ADVANCED_FACE('',(#3452),#75,.T.);
#27256=ADVANCED_FACE('',(#3453),#2487,.T.);
#27257=ADVANCED_FACE('',(#3454),#2488,.T.);
#27258=ADVANCED_FACE('',(#3455),#76,.T.);
#27259=ADVANCED_FACE('',(#3456),#2489,.T.);
#27260=ADVANCED_FACE('',(#3457),#2490,.T.);
#27261=ADVANCED_FACE('',(#3458),#2491,.T.);
#27262=ADVANCED_FACE('',(#3459),#2492,.T.);
#27263=ADVANCED_FACE('',(#3460),#2493,.T.);
#27264=ADVANCED_FACE('',(#3461),#77,.T.);
#27265=ADVANCED_FACE('',(#3462),#2494,.T.);
#27266=ADVANCED_FACE('',(#3463),#2495,.T.);
#27267=ADVANCED_FACE('',(#3464),#78,.T.);
#27268=ADVANCED_FACE('',(#3465),#2496,.T.);
#27269=ADVANCED_FACE('',(#3466),#58,.F.);
#27270=ADVANCED_FACE('',(#3467),#2497,.T.);
#27271=ADVANCED_FACE('',(#3468),#26460,.T.);
#27272=ADVANCED_FACE('',(#3469),#26461,.T.);
#27273=ADVANCED_FACE('',(#3470),#26462,.T.);
#27274=ADVANCED_FACE('',(#3471),#26463,.T.);
#27275=ADVANCED_FACE('',(#3472),#2498,.F.);
#27276=ADVANCED_FACE('',(#3473),#26464,.T.);
#27277=ADVANCED_FACE('',(#3474),#26465,.T.);
#27278=ADVANCED_FACE('',(#3475),#26466,.T.);
#27279=ADVANCED_FACE('',(#3476),#2499,.T.);
#27280=ADVANCED_FACE('',(#3477,#201),#26467,.T.);
#27281=ADVANCED_FACE('',(#3478),#2500,.T.);
#27282=ADVANCED_FACE('',(#3479),#26468,.T.);
#27283=ADVANCED_FACE('',(#3480),#2501,.T.);
#27284=ADVANCED_FACE('',(#3481),#2502,.F.);
#27285=ADVANCED_FACE('',(#3482),#2503,.F.);
#27286=ADVANCED_FACE('',(#3483),#26469,.T.);
#27287=ADVANCED_FACE('',(#3484),#26470,.T.);
#27288=ADVANCED_FACE('',(#3485),#26471,.T.);
#27289=ADVANCED_FACE('',(#3486),#2504,.F.);
#27290=ADVANCED_FACE('',(#3487),#26472,.T.);
#27291=ADVANCED_FACE('',(#3488),#2505,.T.);
#27292=ADVANCED_FACE('',(#3489),#2506,.F.);
#27293=ADVANCED_FACE('',(#3490),#26473,.T.);
#27294=ADVANCED_FACE('',(#3491),#2507,.F.);
#27295=ADVANCED_FACE('',(#3492),#26474,.F.);
#27296=ADVANCED_FACE('',(#3493),#2508,.T.);
#27297=ADVANCED_FACE('',(#3494),#2509,.T.);
#27298=ADVANCED_FACE('',(#3495),#2510,.T.);
#27299=ADVANCED_FACE('',(#3496),#79,.T.);
#27300=ADVANCED_FACE('',(#3497),#2511,.T.);
#27301=ADVANCED_FACE('',(#3498),#80,.T.);
#27302=ADVANCED_FACE('',(#3499),#2512,.T.);
#27303=ADVANCED_FACE('',(#3500),#81,.T.);
#27304=ADVANCED_FACE('',(#3501),#2513,.T.);
#27305=ADVANCED_FACE('',(#3502),#59,.F.);
#27306=ADVANCED_FACE('',(#3503),#2514,.T.);
#27307=ADVANCED_FACE('',(#3504),#2515,.T.);
#27308=ADVANCED_FACE('',(#3505),#2516,.T.);
#27309=ADVANCED_FACE('',(#3506),#82,.T.);
#27310=ADVANCED_FACE('',(#3507),#2517,.T.);
#27311=ADVANCED_FACE('',(#3508),#2518,.T.);
#27312=ADVANCED_FACE('',(#3509),#2519,.T.);
#27313=ADVANCED_FACE('',(#3510),#83,.T.);
#27314=ADVANCED_FACE('',(#3511),#2520,.T.);
#27315=ADVANCED_FACE('',(#3512),#2521,.T.);
#27316=ADVANCED_FACE('',(#3513),#2522,.T.);
#27317=ADVANCED_FACE('',(#3514),#60,.F.);
#27318=ADVANCED_FACE('',(#3515),#2523,.T.);
#27319=ADVANCED_FACE('',(#3516),#84,.T.);
#27320=ADVANCED_FACE('',(#3517),#2524,.T.);
#27321=ADVANCED_FACE('',(#3518),#85,.T.);
#27322=ADVANCED_FACE('',(#3519),#2525,.T.);
#27323=ADVANCED_FACE('',(#3520),#86,.T.);
#27324=ADVANCED_FACE('',(#3521),#2526,.T.);
#27325=ADVANCED_FACE('',(#3522),#2527,.T.);
#27326=ADVANCED_FACE('',(#3523),#2528,.T.);
#27327=ADVANCED_FACE('',(#3524),#2529,.T.);
#27328=ADVANCED_FACE('',(#3525),#51,.T.);
#27329=ADVANCED_FACE('',(#3526),#52,.T.);
#27330=ADVANCED_FACE('',(#3527),#26475,.F.);
#27331=ADVANCED_FACE('',(#3528),#2530,.F.);
#27332=ADVANCED_FACE('',(#3529),#26476,.F.);
#27333=ADVANCED_FACE('',(#3530),#26477,.F.);
#27334=ADVANCED_FACE('',(#3531),#26478,.F.);
#27335=ADVANCED_FACE('',(#3532),#2531,.T.);
#27336=ADVANCED_FACE('',(#3533,#202),#26479,.F.);
#27337=ADVANCED_FACE('',(#3534),#2532,.T.);
#27338=ADVANCED_FACE('',(#3535),#26480,.F.);
#27339=ADVANCED_FACE('',(#3536),#2533,.T.);
#27340=ADVANCED_FACE('',(#3537),#26481,.F.);
#27341=ADVANCED_FACE('',(#3538),#2534,.F.);
#27342=ADVANCED_FACE('',(#3539),#26482,.F.);
#27343=ADVANCED_FACE('',(#3540),#2535,.T.);
#27344=ADVANCED_FACE('',(#3541),#26483,.F.);
#27345=ADVANCED_FACE('',(#3542),#26484,.F.);
#27346=ADVANCED_FACE('',(#3543),#26485,.F.);
#27347=ADVANCED_FACE('',(#3544),#26486,.T.);
#27348=ADVANCED_FACE('',(#3545),#2536,.T.);
#27349=ADVANCED_FACE('',(#3546),#87,.T.);
#27350=ADVANCED_FACE('',(#3547),#2537,.T.);
#27351=ADVANCED_FACE('',(#3548),#2538,.T.);
#27352=ADVANCED_FACE('',(#3549),#2539,.T.);
#27353=ADVANCED_FACE('',(#3550),#53,.T.);
#27354=ADVANCED_FACE('',(#3551),#88,.T.);
#27355=ADVANCED_FACE('',(#3552),#2540,.T.);
#27356=ADVANCED_FACE('',(#3553),#54,.T.);
#27357=ADVANCED_FACE('',(#3554),#2541,.T.);
#27358=ADVANCED_FACE('',(#3555),#26487,.F.);
#27359=ADVANCED_FACE('',(#3556),#2542,.T.);
#27360=ADVANCED_FACE('',(#3557),#89,.T.);
#27361=ADVANCED_FACE('',(#3558),#2543,.T.);
#27362=ADVANCED_FACE('',(#3559),#61,.F.);
#27363=ADVANCED_FACE('',(#3560),#2544,.T.);
#27364=ADVANCED_FACE('',(#3561),#90,.T.);
#27365=ADVANCED_FACE('',(#3562),#91,.T.);
#27366=ADVANCED_FACE('',(#3563),#2545,.T.);
#27367=ADVANCED_FACE('',(#3564),#2546,.T.);
#27368=ADVANCED_FACE('',(#3565),#92,.T.);
#27369=ADVANCED_FACE('',(#3566),#2547,.T.);
#27370=ADVANCED_FACE('',(#3567),#2548,.T.);
#27371=ADVANCED_FACE('',(#3568),#2549,.T.);
#27372=ADVANCED_FACE('',(#3569),#2550,.T.);
#27373=ADVANCED_FACE('',(#3570),#2551,.T.);
#27374=ADVANCED_FACE('',(#3571),#93,.T.);
#27375=ADVANCED_FACE('',(#3572),#2552,.T.);
#27376=ADVANCED_FACE('',(#3573),#2553,.T.);
#27377=ADVANCED_FACE('',(#3574),#94,.T.);
#27378=ADVANCED_FACE('',(#3575),#2554,.T.);
#27379=ADVANCED_FACE('',(#3576),#62,.F.);
#27380=ADVANCED_FACE('',(#3577),#2555,.T.);
#27381=ADVANCED_FACE('',(#3578),#26488,.F.);
#27382=ADVANCED_FACE('',(#3579),#26489,.F.);
#27383=ADVANCED_FACE('',(#3580),#26490,.F.);
#27384=ADVANCED_FACE('',(#3581),#26491,.F.);
#27385=ADVANCED_FACE('',(#3582),#2556,.F.);
#27386=ADVANCED_FACE('',(#3583),#26492,.F.);
#27387=ADVANCED_FACE('',(#3584),#26493,.F.);
#27388=ADVANCED_FACE('',(#3585),#26494,.F.);
#27389=ADVANCED_FACE('',(#3586),#2557,.T.);
#27390=ADVANCED_FACE('',(#3587,#203),#26495,.F.);
#27391=ADVANCED_FACE('',(#3588),#2558,.T.);
#27392=ADVANCED_FACE('',(#3589),#26496,.F.);
#27393=ADVANCED_FACE('',(#3590),#2559,.T.);
#27394=ADVANCED_FACE('',(#3591),#2560,.F.);
#27395=ADVANCED_FACE('',(#3592),#2561,.F.);
#27396=ADVANCED_FACE('',(#3593),#26497,.F.);
#27397=ADVANCED_FACE('',(#3594),#26498,.F.);
#27398=ADVANCED_FACE('',(#3595),#26499,.F.);
#27399=ADVANCED_FACE('',(#3596),#2562,.F.);
#27400=ADVANCED_FACE('',(#3597),#26500,.F.);
#27401=ADVANCED_FACE('',(#3598),#2563,.T.);
#27402=ADVANCED_FACE('',(#3599),#2564,.F.);
#27403=ADVANCED_FACE('',(#3600),#26501,.T.);
#27404=ADVANCED_FACE('',(#3601),#2565,.F.);
#27405=ADVANCED_FACE('',(#3602),#26502,.T.);
#27406=ADVANCED_FACE('',(#3603),#26503,.T.);
#27407=ADVANCED_FACE('',(#3604),#26504,.T.);
#27408=ADVANCED_FACE('',(#3605),#2566,.F.);
#27409=ADVANCED_FACE('',(#3606),#26505,.T.);
#27410=ADVANCED_FACE('',(#3607),#2567,.F.);
#27411=ADVANCED_FACE('',(#3608),#26506,.T.);
#27412=ADVANCED_FACE('',(#3609),#2568,.F.);
#27413=ADVANCED_FACE('',(#3610),#2569,.T.);
#27414=ADVANCED_FACE('',(#3611),#26507,.F.);
#27415=ADVANCED_FACE('',(#3612),#26508,.F.);
#27416=ADVANCED_FACE('',(#3613),#26509,.F.);
#27417=ADVANCED_FACE('',(#3614),#2570,.F.);
#27418=ADVANCED_FACE('',(#3615),#2571,.F.);
#27419=ADVANCED_FACE('',(#3616),#2572,.F.);
#27420=ADVANCED_FACE('',(#3617),#26510,.F.);
#27421=ADVANCED_FACE('',(#3618),#26511,.F.);
#27422=ADVANCED_FACE('',(#3619),#26512,.F.);
#27423=ADVANCED_FACE('',(#3620),#2573,.F.);
#27424=ADVANCED_FACE('',(#3621),#2574,.F.);
#27425=ADVANCED_FACE('',(#3622),#2575,.F.);
#27426=ADVANCED_FACE('',(#3623),#26513,.F.);
#27427=ADVANCED_FACE('',(#3624),#26514,.F.);
#27428=ADVANCED_FACE('',(#3625),#26515,.F.);
#27429=ADVANCED_FACE('',(#3626),#2576,.F.);
#27430=ADVANCED_FACE('',(#3627),#2577,.F.);
#27431=ADVANCED_FACE('',(#3628),#2578,.F.);
#27432=ADVANCED_FACE('',(#3629),#26516,.F.);
#27433=ADVANCED_FACE('',(#3630),#26517,.F.);
#27434=ADVANCED_FACE('',(#3631),#26518,.F.);
#27435=ADVANCED_FACE('',(#3632),#2579,.F.);
#27436=ADVANCED_FACE('',(#3633),#2580,.F.);
#27437=ADVANCED_FACE('',(#3634),#2581,.F.);
#27438=ADVANCED_FACE('',(#3635),#26519,.F.);
#27439=ADVANCED_FACE('',(#3636),#26520,.F.);
#27440=ADVANCED_FACE('',(#3637),#26521,.F.);
#27441=ADVANCED_FACE('',(#3638),#2582,.F.);
#27442=ADVANCED_FACE('',(#3639),#2583,.F.);
#27443=ADVANCED_FACE('',(#3640),#2584,.F.);
#27444=ADVANCED_FACE('',(#3641),#26522,.F.);
#27445=ADVANCED_FACE('',(#3642),#26523,.F.);
#27446=ADVANCED_FACE('',(#3643),#26524,.F.);
#27447=ADVANCED_FACE('',(#3644),#2585,.T.);
#27448=ADVANCED_FACE('',(#3645),#26525,.T.);
#27449=ADVANCED_FACE('',(#3646),#26526,.T.);
#27450=ADVANCED_FACE('',(#3647),#26527,.T.);
#27451=ADVANCED_FACE('',(#3648),#2586,.F.);
#27452=ADVANCED_FACE('',(#3649),#2587,.F.);
#27453=ADVANCED_FACE('',(#3650),#2588,.F.);
#27454=ADVANCED_FACE('',(#3651),#26528,.T.);
#27455=ADVANCED_FACE('',(#3652),#26529,.T.);
#27456=ADVANCED_FACE('',(#3653),#26530,.T.);
#27457=ADVANCED_FACE('',(#3654),#2589,.F.);
#27458=ADVANCED_FACE('',(#3655),#2590,.F.);
#27459=ADVANCED_FACE('',(#3656),#2591,.F.);
#27460=ADVANCED_FACE('',(#3657),#26531,.T.);
#27461=ADVANCED_FACE('',(#3658),#26532,.T.);
#27462=ADVANCED_FACE('',(#3659),#26533,.T.);
#27463=ADVANCED_FACE('',(#3660),#2592,.F.);
#27464=ADVANCED_FACE('',(#3661),#2593,.F.);
#27465=ADVANCED_FACE('',(#3662),#2594,.F.);
#27466=ADVANCED_FACE('',(#3663),#26534,.T.);
#27467=ADVANCED_FACE('',(#3664),#26535,.T.);
#27468=ADVANCED_FACE('',(#3665),#26536,.T.);
#27469=ADVANCED_FACE('',(#3666),#2595,.F.);
#27470=ADVANCED_FACE('',(#3667),#2596,.F.);
#27471=ADVANCED_FACE('',(#3668),#2597,.F.);
#27472=ADVANCED_FACE('',(#3669),#26537,.T.);
#27473=ADVANCED_FACE('',(#3670),#26538,.T.);
#27474=ADVANCED_FACE('',(#3671),#26539,.T.);
#27475=ADVANCED_FACE('',(#3672),#2598,.F.);
#27476=ADVANCED_FACE('',(#3673),#2599,.F.);
#27477=ADVANCED_FACE('',(#3674),#2600,.F.);
#27478=ADVANCED_FACE('',(#3675),#26540,.T.);
#27479=ADVANCED_FACE('',(#3676),#26541,.T.);
#27480=ADVANCED_FACE('',(#3677),#26542,.T.);
#27481=ADVANCED_FACE('',(#3678),#2601,.F.);
#27482=ADVANCED_FACE('',(#3679),#2602,.F.);
#27483=ADVANCED_FACE('',(#3680),#2603,.F.);
#27484=ADVANCED_FACE('',(#3681),#26543,.F.);
#27485=ADVANCED_FACE('',(#3682),#26544,.F.);
#27486=ADVANCED_FACE('',(#3683),#2604,.T.);
#27487=ADVANCED_FACE('',(#3684),#26545,.F.);
#27488=ADVANCED_FACE('',(#3685),#2605,.T.);
#27489=ADVANCED_FACE('',(#3686),#26546,.F.);
#27490=ADVANCED_FACE('',(#3687),#2606,.F.);
#27491=ADVANCED_FACE('',(#3688),#26547,.F.);
#27492=ADVANCED_FACE('',(#3689),#2607,.F.);
#27493=ADVANCED_FACE('',(#3690),#26548,.F.);
#27494=ADVANCED_FACE('',(#3691),#2608,.F.);
#27495=ADVANCED_FACE('',(#3692),#26549,.F.);
#27496=ADVANCED_FACE('',(#3693),#2609,.F.);
#27497=ADVANCED_FACE('',(#3694),#26550,.F.);
#27498=ADVANCED_FACE('',(#3695),#2610,.F.);
#27499=ADVANCED_FACE('',(#3696),#26551,.F.);
#27500=ADVANCED_FACE('',(#3697),#26552,.F.);
#27501=ADVANCED_FACE('',(#3698),#2611,.T.);
#27502=ADVANCED_FACE('',(#3699),#26553,.F.);
#27503=ADVANCED_FACE('',(#3700),#2612,.T.);
#27504=ADVANCED_FACE('',(#3701,#204,#205,#206),#26554,.F.);
#27505=ADVANCED_FACE('',(#3702),#2613,.F.);
#27506=ADVANCED_FACE('',(#3703),#26555,.F.);
#27507=ADVANCED_FACE('',(#3704),#2614,.T.);
#27508=ADVANCED_FACE('',(#3705),#26556,.F.);
#27509=ADVANCED_FACE('',(#3706),#2615,.T.);
#27510=ADVANCED_FACE('',(#3707,#207,#208,#209),#26557,.F.);
#27511=ADVANCED_FACE('',(#3708),#2616,.T.);
#27512=ADVANCED_FACE('',(#3709),#26558,.F.);
#27513=ADVANCED_FACE('',(#3710),#26559,.F.);
#27514=ADVANCED_FACE('',(#3711,#210,#211,#212),#26560,.F.);
#27515=ADVANCED_FACE('',(#3712),#2617,.F.);
#27516=ADVANCED_FACE('',(#3713),#26561,.F.);
#27517=ADVANCED_FACE('',(#3714),#26562,.F.);
#27518=ADVANCED_FACE('',(#3715),#26563,.F.);
#27519=ADVANCED_FACE('',(#3716),#26564,.T.);
#27520=ADVANCED_FACE('',(#3717),#2618,.T.);
#27521=ADVANCED_FACE('',(#3718),#26565,.T.);
#27522=ADVANCED_FACE('',(#3719),#2619,.T.);
#27523=ADVANCED_FACE('',(#3720),#26566,.T.);
#27524=ADVANCED_FACE('',(#3721),#2620,.F.);
#27525=ADVANCED_FACE('',(#3722),#26567,.T.);
#27526=ADVANCED_FACE('',(#3723),#2621,.F.);
#27527=ADVANCED_FACE('',(#3724),#26568,.T.);
#27528=ADVANCED_FACE('',(#3725),#2622,.F.);
#27529=ADVANCED_FACE('',(#3726),#26569,.T.);
#27530=ADVANCED_FACE('',(#3727),#2623,.F.);
#27531=ADVANCED_FACE('',(#3728),#26570,.T.);
#27532=ADVANCED_FACE('',(#3729),#2624,.F.);
#27533=ADVANCED_FACE('',(#3730),#26571,.T.);
#27534=ADVANCED_FACE('',(#3731),#26572,.T.);
#27535=ADVANCED_FACE('',(#3732),#2625,.T.);
#27536=ADVANCED_FACE('',(#3733),#26573,.T.);
#27537=ADVANCED_FACE('',(#3734),#2626,.T.);
#27538=ADVANCED_FACE('',(#3735,#213,#214,#215),#26574,.T.);
#27539=ADVANCED_FACE('',(#3736),#2627,.F.);
#27540=ADVANCED_FACE('',(#3737),#26575,.T.);
#27541=ADVANCED_FACE('',(#3738),#2628,.T.);
#27542=ADVANCED_FACE('',(#3739),#26576,.T.);
#27543=ADVANCED_FACE('',(#3740),#2629,.T.);
#27544=ADVANCED_FACE('',(#3741),#26577,.T.);
#27545=ADVANCED_FACE('',(#3742),#2630,.T.);
#27546=ADVANCED_FACE('',(#3743),#26578,.T.);
#27547=ADVANCED_FACE('',(#3744),#26579,.T.);
#27548=ADVANCED_FACE('',(#3745),#26580,.T.);
#27549=ADVANCED_FACE('',(#3746),#2631,.F.);
#27550=ADVANCED_FACE('',(#3747),#26581,.T.);
#27551=ADVANCED_FACE('',(#3748),#26582,.T.);
#27552=ADVANCED_FACE('',(#3749),#26583,.T.);
#27553=ADVANCED_FACE('',(#3750),#26584,.T.);
#27554=ADVANCED_FACE('',(#3751),#26585,.F.);
#27555=ADVANCED_FACE('',(#3752),#26586,.T.);
#27556=ADVANCED_FACE('',(#3753),#26587,.F.);
#27557=ADVANCED_FACE('',(#3754),#26588,.F.);
#27558=ADVANCED_FACE('',(#3755),#26589,.F.);
#27559=ADVANCED_FACE('',(#3756),#26590,.F.);
#27560=ADVANCED_FACE('',(#3757),#2632,.T.);
#27561=ADVANCED_FACE('',(#3758),#26591,.F.);
#27562=ADVANCED_FACE('',(#3759),#26592,.T.);
#27563=ADVANCED_FACE('',(#3760),#2633,.T.);
#27564=ADVANCED_FACE('',(#3761),#26593,.F.);
#27565=ADVANCED_FACE('',(#3762,#216),#26594,.F.);
#27566=ADVANCED_FACE('',(#3763),#26595,.F.);
#27567=ADVANCED_FACE('',(#3764),#26596,.F.);
#27568=ADVANCED_FACE('',(#3765),#26597,.F.);
#27569=ADVANCED_FACE('',(#3766),#2634,.F.);
#27570=ADVANCED_FACE('',(#3767),#2635,.F.);
#27571=ADVANCED_FACE('',(#3768),#26598,.F.);
#27572=ADVANCED_FACE('',(#3769),#26599,.F.);
#27573=ADVANCED_FACE('',(#3770),#26600,.F.);
#27574=ADVANCED_FACE('',(#3771),#26601,.F.);
#27575=ADVANCED_FACE('',(#3772),#26602,.T.);
#27576=ADVANCED_FACE('',(#3773),#26603,.F.);
#27577=ADVANCED_FACE('',(#3774),#26604,.F.);
#27578=ADVANCED_FACE('',(#3775),#2636,.F.);
#27579=ADVANCED_FACE('',(#3776),#26605,.F.);
#27580=ADVANCED_FACE('',(#3777),#2637,.T.);
#27581=ADVANCED_FACE('',(#3778),#2638,.F.);
#27582=ADVANCED_FACE('',(#3779),#2639,.F.);
#27583=ADVANCED_FACE('',(#3780),#2640,.T.);
#27584=ADVANCED_FACE('',(#3781),#26606,.F.);
#27585=ADVANCED_FACE('',(#3782),#2641,.F.);
#27586=ADVANCED_FACE('',(#3783),#26607,.F.);
#27587=ADVANCED_FACE('',(#3784),#26608,.T.);
#27588=ADVANCED_FACE('',(#3785),#26609,.T.);
#27589=ADVANCED_FACE('',(#3786),#26610,.T.);
#27590=ADVANCED_FACE('',(#3787),#26611,.T.);
#27591=ADVANCED_FACE('',(#3788),#26612,.T.);
#27592=ADVANCED_FACE('',(#3789),#26613,.T.);
#27593=ADVANCED_FACE('',(#3790),#2642,.T.);
#27594=ADVANCED_FACE('',(#3791),#26614,.T.);
#27595=ADVANCED_FACE('',(#3792),#26615,.F.);
#27596=ADVANCED_FACE('',(#3793),#26616,.T.);
#27597=ADVANCED_FACE('',(#3794),#2643,.T.);
#27598=ADVANCED_FACE('',(#3795),#26617,.T.);
#27599=ADVANCED_FACE('',(#3796,#217),#26618,.T.);
#27600=ADVANCED_FACE('',(#3797),#26619,.T.);
#27601=ADVANCED_FACE('',(#3798),#26620,.T.);
#27602=ADVANCED_FACE('',(#3799),#26621,.T.);
#27603=ADVANCED_FACE('',(#3800),#2644,.F.);
#27604=ADVANCED_FACE('',(#3801),#2645,.F.);
#27605=ADVANCED_FACE('',(#3802),#26622,.T.);
#27606=ADVANCED_FACE('',(#3803),#26623,.T.);
#27607=ADVANCED_FACE('',(#3804),#26624,.T.);
#27608=ADVANCED_FACE('',(#3805),#26625,.T.);
#27609=ADVANCED_FACE('',(#3806),#26626,.F.);
#27610=ADVANCED_FACE('',(#3807),#26627,.T.);
#27611=ADVANCED_FACE('',(#3808),#26628,.T.);
#27612=ADVANCED_FACE('',(#3809),#26629,.T.);
#27613=ADVANCED_FACE('',(#3810),#26630,.T.);
#27614=ADVANCED_FACE('',(#3811),#26631,.T.);
#27615=ADVANCED_FACE('',(#3812),#26632,.T.);
#27616=ADVANCED_FACE('',(#3813),#26633,.T.);
#27617=ADVANCED_FACE('',(#3814),#2646,.F.);
#27618=ADVANCED_FACE('',(#3815),#26634,.T.);
#27619=ADVANCED_FACE('',(#3816),#2647,.T.);
#27620=ADVANCED_FACE('',(#3817),#2648,.F.);
#27621=ADVANCED_FACE('',(#3818),#2649,.F.);
#27622=ADVANCED_FACE('',(#3819),#2650,.T.);
#27623=ADVANCED_FACE('',(#3820),#26635,.T.);
#27624=ADVANCED_FACE('',(#3821),#2651,.F.);
#27625=ADVANCED_FACE('',(#3822),#2652,.F.);
#27626=ADVANCED_FACE('',(#3823),#2653,.T.);
#27627=ADVANCED_FACE('',(#3824),#26636,.T.);
#27628=ADVANCED_FACE('',(#3825),#26637,.T.);
#27629=ADVANCED_FACE('',(#3826),#26638,.T.);
#27630=ADVANCED_FACE('',(#3827),#26639,.T.);
#27631=ADVANCED_FACE('',(#3828),#26640,.T.);
#27632=ADVANCED_FACE('',(#3829),#2654,.T.);
#27633=ADVANCED_FACE('',(#3830),#26641,.T.);
#27634=ADVANCED_FACE('',(#3831),#26642,.T.);
#27635=ADVANCED_FACE('',(#3832),#2655,.T.);
#27636=ADVANCED_FACE('',(#3833),#2656,.F.);
#27637=ADVANCED_FACE('',(#3834),#2657,.T.);
#27638=ADVANCED_FACE('',(#3835),#26643,.T.);
#27639=ADVANCED_FACE('',(#3836),#26644,.T.);
#27640=ADVANCED_FACE('',(#3837),#26645,.T.);
#27641=ADVANCED_FACE('',(#3838),#2658,.F.);
#27642=ADVANCED_FACE('',(#3839),#26646,.T.);
#27643=ADVANCED_FACE('',(#3840),#2659,.T.);
#27644=ADVANCED_FACE('',(#3841),#26647,.T.);
#27645=ADVANCED_FACE('',(#3842),#2660,.T.);
#27646=ADVANCED_FACE('',(#3843),#26648,.T.);
#27647=ADVANCED_FACE('',(#3844),#26649,.T.);
#27648=ADVANCED_FACE('',(#3845),#26650,.T.);
#27649=ADVANCED_FACE('',(#3846),#2661,.F.);
#27650=ADVANCED_FACE('',(#3847),#26651,.T.);
#27651=ADVANCED_FACE('',(#3848),#2662,.F.);
#27652=ADVANCED_FACE('',(#3849),#26652,.T.);
#27653=ADVANCED_FACE('',(#3850),#2663,.F.);
#27654=ADVANCED_FACE('',(#3851),#26653,.T.);
#27655=ADVANCED_FACE('',(#3852),#2664,.F.);
#27656=ADVANCED_FACE('',(#3853),#26654,.T.);
#27657=ADVANCED_FACE('',(#3854),#26655,.T.);
#27658=ADVANCED_FACE('',(#3855),#26656,.T.);
#27659=ADVANCED_FACE('',(#3856),#2665,.T.);
#27660=ADVANCED_FACE('',(#3857),#26657,.T.);
#27661=ADVANCED_FACE('',(#3858),#2666,.T.);
#27662=ADVANCED_FACE('',(#3859),#26658,.T.);
#27663=ADVANCED_FACE('',(#3860),#2667,.F.);
#27664=ADVANCED_FACE('',(#3861),#26659,.T.);
#27665=ADVANCED_FACE('',(#3862),#26660,.T.);
#27666=ADVANCED_FACE('',(#3863),#26661,.T.);
#27667=ADVANCED_FACE('',(#3864),#2668,.T.);
#27668=ADVANCED_FACE('',(#3865),#2669,.F.);
#27669=ADVANCED_FACE('',(#3866),#2670,.T.);
#27670=ADVANCED_FACE('',(#3867),#26662,.T.);
#27671=ADVANCED_FACE('',(#3868),#26663,.T.);
#27672=ADVANCED_FACE('',(#3869),#2671,.T.);
#27673=ADVANCED_FACE('',(#3870),#26664,.T.);
#27674=ADVANCED_FACE('',(#3871),#26665,.T.);
#27675=ADVANCED_FACE('',(#3872),#26666,.T.);
#27676=ADVANCED_FACE('',(#3873),#26667,.T.);
#27677=ADVANCED_FACE('',(#3874),#26668,.T.);
#27678=ADVANCED_FACE('',(#3875),#2672,.T.);
#27679=ADVANCED_FACE('',(#3876),#26669,.T.);
#27680=ADVANCED_FACE('',(#3877),#26670,.T.);
#27681=ADVANCED_FACE('',(#3878),#2673,.T.);
#27682=ADVANCED_FACE('',(#3879),#2674,.F.);
#27683=ADVANCED_FACE('',(#3880),#2675,.T.);
#27684=ADVANCED_FACE('',(#3881),#26671,.T.);
#27685=ADVANCED_FACE('',(#3882),#26672,.T.);
#27686=ADVANCED_FACE('',(#3883),#26673,.T.);
#27687=ADVANCED_FACE('',(#3884),#2676,.F.);
#27688=ADVANCED_FACE('',(#3885),#26674,.T.);
#27689=ADVANCED_FACE('',(#3886),#2677,.T.);
#27690=ADVANCED_FACE('',(#3887),#26675,.T.);
#27691=ADVANCED_FACE('',(#3888),#2678,.T.);
#27692=ADVANCED_FACE('',(#3889),#26676,.T.);
#27693=ADVANCED_FACE('',(#3890),#26677,.T.);
#27694=ADVANCED_FACE('',(#3891),#26678,.T.);
#27695=ADVANCED_FACE('',(#3892),#2679,.F.);
#27696=ADVANCED_FACE('',(#3893),#26679,.T.);
#27697=ADVANCED_FACE('',(#3894),#2680,.F.);
#27698=ADVANCED_FACE('',(#3895),#26680,.T.);
#27699=ADVANCED_FACE('',(#3896),#2681,.F.);
#27700=ADVANCED_FACE('',(#3897),#26681,.T.);
#27701=ADVANCED_FACE('',(#3898),#2682,.F.);
#27702=ADVANCED_FACE('',(#3899),#26682,.T.);
#27703=ADVANCED_FACE('',(#3900),#26683,.T.);
#27704=ADVANCED_FACE('',(#3901),#26684,.T.);
#27705=ADVANCED_FACE('',(#3902),#2683,.T.);
#27706=ADVANCED_FACE('',(#3903),#26685,.T.);
#27707=ADVANCED_FACE('',(#3904),#2684,.T.);
#27708=ADVANCED_FACE('',(#3905),#26686,.T.);
#27709=ADVANCED_FACE('',(#3906),#2685,.F.);
#27710=ADVANCED_FACE('',(#3907),#26687,.T.);
#27711=ADVANCED_FACE('',(#3908),#26688,.T.);
#27712=ADVANCED_FACE('',(#3909),#26689,.T.);
#27713=ADVANCED_FACE('',(#3910),#2686,.T.);
#27714=ADVANCED_FACE('',(#3911),#2687,.F.);
#27715=ADVANCED_FACE('',(#3912),#2688,.T.);
#27716=ADVANCED_FACE('',(#3913),#26690,.T.);
#27717=ADVANCED_FACE('',(#3914),#26691,.T.);
#27718=ADVANCED_FACE('',(#3915,#218),#26692,.T.);
#27719=ADVANCED_FACE('',(#3916,#219),#26693,.F.);
#27720=ADVANCED_FACE('',(#3917),#2689,.F.);
#27721=ADVANCED_FACE('',(#3918),#2690,.F.);
#27722=ADVANCED_FACE('',(#3919),#2691,.F.);
#27723=ADVANCED_FACE('',(#3920),#2692,.F.);
#27724=ADVANCED_FACE('',(#3921),#2693,.F.);
#27725=ADVANCED_FACE('',(#3922),#2694,.F.);
#27726=ADVANCED_FACE('',(#3923),#2695,.F.);
#27727=ADVANCED_FACE('',(#3924),#2696,.F.);
#27728=ADVANCED_FACE('',(#3925),#2697,.F.);
#27729=ADVANCED_FACE('',(#3926),#2698,.F.);
#27730=ADVANCED_FACE('',(#3927),#2699,.F.);
#27731=ADVANCED_FACE('',(#3928),#2700,.F.);
#27732=ADVANCED_FACE('',(#3929),#2701,.F.);
#27733=ADVANCED_FACE('',(#3930),#2702,.F.);
#27734=ADVANCED_FACE('',(#3931),#2703,.F.);
#27735=ADVANCED_FACE('',(#3932),#2704,.F.);
#27736=ADVANCED_FACE('',(#3933),#2705,.F.);
#27737=ADVANCED_FACE('',(#3934),#2706,.F.);
#27738=ADVANCED_FACE('',(#3935),#2707,.F.);
#27739=ADVANCED_FACE('',(#3936),#2708,.F.);
#27740=ADVANCED_FACE('',(#3937),#2709,.F.);
#27741=ADVANCED_FACE('',(#3938),#2710,.F.);
#27742=ADVANCED_FACE('',(#3939),#2711,.F.);
#27743=ADVANCED_FACE('',(#3940),#2712,.F.);
#27744=ADVANCED_FACE('',(#3941),#2713,.F.);
#27745=ADVANCED_FACE('',(#3942),#2714,.F.);
#27746=ADVANCED_FACE('',(#3943),#2715,.F.);
#27747=ADVANCED_FACE('',(#3944),#2716,.F.);
#27748=ADVANCED_FACE('',(#3945),#2717,.F.);
#27749=ADVANCED_FACE('',(#3946),#2718,.F.);
#27750=ADVANCED_FACE('',(#3947),#2719,.F.);
#27751=ADVANCED_FACE('',(#3948),#2720,.F.);
#27752=ADVANCED_FACE('',(#3949),#2721,.F.);
#27753=ADVANCED_FACE('',(#3950),#2722,.F.);
#27754=ADVANCED_FACE('',(#3951),#2723,.F.);
#27755=ADVANCED_FACE('',(#3952),#2724,.F.);
#27756=ADVANCED_FACE('',(#3953),#2725,.F.);
#27757=ADVANCED_FACE('',(#3954),#2726,.F.);
#27758=ADVANCED_FACE('',(#3955),#2727,.F.);
#27759=ADVANCED_FACE('',(#3956),#2728,.F.);
#27760=ADVANCED_FACE('',(#3957),#2729,.F.);
#27761=ADVANCED_FACE('',(#3958),#2730,.F.);
#27762=ADVANCED_FACE('',(#3959),#2731,.F.);
#27763=ADVANCED_FACE('',(#3960),#2732,.F.);
#27764=ADVANCED_FACE('',(#3961),#2733,.F.);
#27765=ADVANCED_FACE('',(#3962),#2734,.F.);
#27766=ADVANCED_FACE('',(#3963),#2735,.F.);
#27767=ADVANCED_FACE('',(#3964),#2736,.F.);
#27768=ADVANCED_FACE('',(#3965),#2737,.F.);
#27769=ADVANCED_FACE('',(#3966),#2738,.F.);
#27770=ADVANCED_FACE('',(#3967),#2739,.F.);
#27771=ADVANCED_FACE('',(#3968),#2740,.F.);
#27772=ADVANCED_FACE('',(#3969),#2741,.F.);
#27773=ADVANCED_FACE('',(#3970),#2742,.F.);
#27774=ADVANCED_FACE('',(#3971),#2743,.F.);
#27775=ADVANCED_FACE('',(#3972),#2744,.F.);
#27776=ADVANCED_FACE('',(#3973),#2745,.F.);
#27777=ADVANCED_FACE('',(#3974),#2746,.F.);
#27778=ADVANCED_FACE('',(#3975),#2747,.F.);
#27779=ADVANCED_FACE('',(#3976),#2748,.F.);
#27780=ADVANCED_FACE('',(#3977),#2749,.F.);
#27781=ADVANCED_FACE('',(#3978),#2750,.F.);
#27782=ADVANCED_FACE('',(#3979),#2751,.F.);
#27783=ADVANCED_FACE('',(#3980),#2752,.F.);
#27784=ADVANCED_FACE('',(#3981),#2753,.F.);
#27785=ADVANCED_FACE('',(#3982),#2754,.F.);
#27786=ADVANCED_FACE('',(#3983),#2755,.F.);
#27787=ADVANCED_FACE('',(#3984),#2756,.F.);
#27788=ADVANCED_FACE('',(#3985),#2757,.F.);
#27789=ADVANCED_FACE('',(#3986),#2758,.F.);
#27790=ADVANCED_FACE('',(#3987),#2759,.F.);
#27791=ADVANCED_FACE('',(#3988),#2760,.F.);
#27792=ADVANCED_FACE('',(#3989),#2761,.F.);
#27793=ADVANCED_FACE('',(#3990),#2762,.F.);
#27794=ADVANCED_FACE('',(#3991),#2763,.F.);
#27795=ADVANCED_FACE('',(#3992),#2764,.F.);
#27796=ADVANCED_FACE('',(#3993),#2765,.F.);
#27797=ADVANCED_FACE('',(#3994),#2766,.F.);
#27798=ADVANCED_FACE('',(#3995),#2767,.F.);
#27799=ADVANCED_FACE('',(#3996),#2768,.F.);
#27800=ADVANCED_FACE('',(#3997),#2769,.F.);
#27801=ADVANCED_FACE('',(#3998),#2770,.F.);
#27802=ADVANCED_FACE('',(#3999),#2771,.F.);
#27803=ADVANCED_FACE('',(#4000),#2772,.F.);
#27804=ADVANCED_FACE('',(#4001),#2773,.F.);
#27805=ADVANCED_FACE('',(#4002),#2774,.F.);
#27806=ADVANCED_FACE('',(#4003),#2775,.F.);
#27807=ADVANCED_FACE('',(#4004),#2776,.F.);
#27808=ADVANCED_FACE('',(#4005),#2777,.F.);
#27809=ADVANCED_FACE('',(#4006),#2778,.F.);
#27810=ADVANCED_FACE('',(#4007),#2779,.F.);
#27811=ADVANCED_FACE('',(#4008),#2780,.F.);
#27812=ADVANCED_FACE('',(#4009),#2781,.F.);
#27813=ADVANCED_FACE('',(#4010),#2782,.F.);
#27814=ADVANCED_FACE('',(#4011),#2783,.F.);
#27815=ADVANCED_FACE('',(#4012),#2784,.F.);
#27816=ADVANCED_FACE('',(#4013),#2785,.F.);
#27817=ADVANCED_FACE('',(#4014),#2786,.F.);
#27818=ADVANCED_FACE('',(#4015),#2787,.F.);
#27819=ADVANCED_FACE('',(#4016),#2788,.F.);
#27820=ADVANCED_FACE('',(#4017),#2789,.F.);
#27821=ADVANCED_FACE('',(#4018),#2790,.F.);
#27822=ADVANCED_FACE('',(#4019),#2791,.F.);
#27823=ADVANCED_FACE('',(#4020),#2792,.F.);
#27824=ADVANCED_FACE('',(#4021),#2793,.F.);
#27825=ADVANCED_FACE('',(#4022),#2794,.F.);
#27826=ADVANCED_FACE('',(#4023),#2795,.F.);
#27827=ADVANCED_FACE('',(#4024),#2796,.F.);
#27828=ADVANCED_FACE('',(#4025),#2797,.F.);
#27829=ADVANCED_FACE('',(#4026),#2798,.F.);
#27830=ADVANCED_FACE('',(#4027),#2799,.F.);
#27831=ADVANCED_FACE('',(#4028),#2800,.F.);
#27832=ADVANCED_FACE('',(#4029),#2801,.F.);
#27833=ADVANCED_FACE('',(#4030),#2802,.F.);
#27834=ADVANCED_FACE('',(#4031),#2803,.F.);
#27835=ADVANCED_FACE('',(#4032),#2804,.F.);
#27836=ADVANCED_FACE('',(#4033),#2805,.F.);
#27837=ADVANCED_FACE('',(#4034),#2806,.F.);
#27838=ADVANCED_FACE('',(#4035),#2807,.F.);
#27839=ADVANCED_FACE('',(#4036),#2808,.F.);
#27840=ADVANCED_FACE('',(#4037),#2809,.F.);
#27841=ADVANCED_FACE('',(#4038),#2810,.F.);
#27842=ADVANCED_FACE('',(#4039),#2811,.F.);
#27843=ADVANCED_FACE('',(#4040),#2812,.F.);
#27844=ADVANCED_FACE('',(#4041),#2813,.F.);
#27845=ADVANCED_FACE('',(#4042),#2814,.F.);
#27846=ADVANCED_FACE('',(#4043),#2815,.F.);
#27847=ADVANCED_FACE('',(#4044),#2816,.F.);
#27848=ADVANCED_FACE('',(#4045),#2817,.F.);
#27849=ADVANCED_FACE('',(#4046),#2818,.F.);
#27850=ADVANCED_FACE('',(#4047),#2819,.F.);
#27851=ADVANCED_FACE('',(#4048),#2820,.F.);
#27852=ADVANCED_FACE('',(#4049),#2821,.F.);
#27853=ADVANCED_FACE('',(#4050),#2822,.F.);
#27854=ADVANCED_FACE('',(#4051),#2823,.F.);
#27855=ADVANCED_FACE('',(#4052),#2824,.F.);
#27856=ADVANCED_FACE('',(#4053),#2825,.F.);
#27857=ADVANCED_FACE('',(#4054),#2826,.F.);
#27858=ADVANCED_FACE('',(#4055),#2827,.F.);
#27859=ADVANCED_FACE('',(#4056),#2828,.F.);
#27860=ADVANCED_FACE('',(#4057),#2829,.F.);
#27861=ADVANCED_FACE('',(#4058),#2830,.F.);
#27862=ADVANCED_FACE('',(#4059),#2831,.F.);
#27863=ADVANCED_FACE('',(#4060),#2832,.F.);
#27864=ADVANCED_FACE('',(#4061),#2833,.F.);
#27865=ADVANCED_FACE('',(#4062),#2834,.F.);
#27866=ADVANCED_FACE('',(#4063),#2835,.F.);
#27867=ADVANCED_FACE('',(#4064),#2836,.F.);
#27868=ADVANCED_FACE('',(#4065),#2837,.F.);
#27869=ADVANCED_FACE('',(#4066),#2838,.F.);
#27870=ADVANCED_FACE('',(#4067),#2839,.F.);
#27871=ADVANCED_FACE('',(#4068),#2840,.F.);
#27872=ADVANCED_FACE('',(#4069),#2841,.F.);
#27873=ADVANCED_FACE('',(#4070),#2842,.F.);
#27874=ADVANCED_FACE('',(#4071),#2843,.F.);
#27875=ADVANCED_FACE('',(#4072),#2844,.F.);
#27876=ADVANCED_FACE('',(#4073),#2845,.F.);
#27877=ADVANCED_FACE('',(#4074),#2846,.F.);
#27878=ADVANCED_FACE('',(#4075),#2847,.F.);
#27879=ADVANCED_FACE('',(#4076),#2848,.F.);
#27880=ADVANCED_FACE('',(#4077),#2849,.F.);
#27881=ADVANCED_FACE('',(#4078),#2850,.F.);
#27882=ADVANCED_FACE('',(#4079),#2851,.F.);
#27883=ADVANCED_FACE('',(#4080),#2852,.F.);
#27884=ADVANCED_FACE('',(#4081),#2853,.F.);
#27885=ADVANCED_FACE('',(#4082),#2854,.F.);
#27886=ADVANCED_FACE('',(#4083),#2855,.F.);
#27887=ADVANCED_FACE('',(#4084),#2856,.F.);
#27888=ADVANCED_FACE('',(#4085),#2857,.F.);
#27889=ADVANCED_FACE('',(#4086),#2858,.F.);
#27890=ADVANCED_FACE('',(#4087),#2859,.F.);
#27891=ADVANCED_FACE('',(#4088),#2860,.F.);
#27892=ADVANCED_FACE('',(#4089),#2861,.F.);
#27893=ADVANCED_FACE('',(#4090),#2862,.F.);
#27894=ADVANCED_FACE('',(#4091),#2863,.F.);
#27895=ADVANCED_FACE('',(#4092),#2864,.F.);
#27896=ADVANCED_FACE('',(#4093),#2865,.F.);
#27897=ADVANCED_FACE('',(#4094),#2866,.F.);
#27898=ADVANCED_FACE('',(#4095),#2867,.F.);
#27899=ADVANCED_FACE('',(#4096),#2868,.F.);
#27900=ADVANCED_FACE('',(#4097),#2869,.F.);
#27901=ADVANCED_FACE('',(#4098),#2870,.F.);
#27902=ADVANCED_FACE('',(#4099),#2871,.F.);
#27903=ADVANCED_FACE('',(#4100),#2872,.F.);
#27904=ADVANCED_FACE('',(#4101),#2873,.F.);
#27905=ADVANCED_FACE('',(#4102),#2874,.F.);
#27906=ADVANCED_FACE('',(#4103),#2875,.F.);
#27907=ADVANCED_FACE('',(#4104),#2876,.F.);
#27908=ADVANCED_FACE('',(#4105),#2877,.F.);
#27909=ADVANCED_FACE('',(#4106),#2878,.F.);
#27910=ADVANCED_FACE('',(#4107),#2879,.F.);
#27911=ADVANCED_FACE('',(#4108),#2880,.F.);
#27912=ADVANCED_FACE('',(#4109),#2881,.F.);
#27913=ADVANCED_FACE('',(#4110),#2882,.F.);
#27914=ADVANCED_FACE('',(#4111),#2883,.F.);
#27915=ADVANCED_FACE('',(#4112),#2884,.F.);
#27916=ADVANCED_FACE('',(#4113),#2885,.F.);
#27917=ADVANCED_FACE('',(#4114),#2886,.F.);
#27918=ADVANCED_FACE('',(#4115),#2887,.F.);
#27919=ADVANCED_FACE('',(#4116),#2888,.F.);
#27920=ADVANCED_FACE('',(#4117),#2889,.F.);
#27921=ADVANCED_FACE('',(#4118),#2890,.F.);
#27922=ADVANCED_FACE('',(#4119),#2891,.F.);
#27923=ADVANCED_FACE('',(#4120),#2892,.F.);
#27924=ADVANCED_FACE('',(#4121),#2893,.F.);
#27925=ADVANCED_FACE('',(#4122),#2894,.F.);
#27926=ADVANCED_FACE('',(#4123),#2895,.F.);
#27927=ADVANCED_FACE('',(#4124),#2896,.F.);
#27928=ADVANCED_FACE('',(#4125),#2897,.F.);
#27929=ADVANCED_FACE('',(#4126),#2898,.F.);
#27930=ADVANCED_FACE('',(#4127),#2899,.F.);
#27931=ADVANCED_FACE('',(#4128),#2900,.F.);
#27932=ADVANCED_FACE('',(#4129),#2901,.F.);
#27933=ADVANCED_FACE('',(#4130),#2902,.F.);
#27934=ADVANCED_FACE('',(#4131),#2903,.F.);
#27935=ADVANCED_FACE('',(#4132),#2904,.F.);
#27936=ADVANCED_FACE('',(#4133),#2905,.F.);
#27937=ADVANCED_FACE('',(#4134),#2906,.F.);
#27938=ADVANCED_FACE('',(#4135),#2907,.F.);
#27939=ADVANCED_FACE('',(#4136),#2908,.F.);
#27940=ADVANCED_FACE('',(#4137),#2909,.F.);
#27941=ADVANCED_FACE('',(#4138),#2910,.F.);
#27942=ADVANCED_FACE('',(#4139),#2911,.F.);
#27943=ADVANCED_FACE('',(#4140),#2912,.F.);
#27944=ADVANCED_FACE('',(#4141),#2913,.F.);
#27945=ADVANCED_FACE('',(#4142),#2914,.F.);
#27946=ADVANCED_FACE('',(#4143),#2915,.F.);
#27947=ADVANCED_FACE('',(#4144),#2916,.F.);
#27948=ADVANCED_FACE('',(#4145),#2917,.F.);
#27949=ADVANCED_FACE('',(#4146),#2918,.F.);
#27950=ADVANCED_FACE('',(#4147),#2919,.F.);
#27951=ADVANCED_FACE('',(#4148),#2920,.F.);
#27952=ADVANCED_FACE('',(#4149),#2921,.F.);
#27953=ADVANCED_FACE('',(#4150),#2922,.F.);
#27954=ADVANCED_FACE('',(#4151),#2923,.F.);
#27955=ADVANCED_FACE('',(#4152),#2924,.F.);
#27956=ADVANCED_FACE('',(#4153),#2925,.F.);
#27957=ADVANCED_FACE('',(#4154),#2926,.F.);
#27958=ADVANCED_FACE('',(#4155),#2927,.F.);
#27959=ADVANCED_FACE('',(#4156),#2928,.F.);
#27960=ADVANCED_FACE('',(#4157),#2929,.F.);
#27961=ADVANCED_FACE('',(#4158),#2930,.F.);
#27962=ADVANCED_FACE('',(#4159),#2931,.F.);
#27963=ADVANCED_FACE('',(#4160),#2932,.F.);
#27964=ADVANCED_FACE('',(#4161),#2933,.F.);
#27965=ADVANCED_FACE('',(#4162),#26694,.F.);
#27966=ADVANCED_FACE('',(#4163),#2934,.F.);
#27967=ADVANCED_FACE('',(#4164),#26695,.F.);
#27968=ADVANCED_FACE('',(#4165),#2935,.F.);
#27969=ADVANCED_FACE('',(#4166),#26696,.F.);
#27970=ADVANCED_FACE('',(#4167),#2936,.F.);
#27971=ADVANCED_FACE('',(#4168),#26697,.F.);
#27972=ADVANCED_FACE('',(#4169),#2937,.F.);
#27973=ADVANCED_FACE('',(#4170),#26698,.F.);
#27974=ADVANCED_FACE('',(#4171),#26699,.F.);
#27975=ADVANCED_FACE('',(#4172),#26700,.F.);
#27976=ADVANCED_FACE('',(#4173),#26701,.F.);
#27977=ADVANCED_FACE('',(#4174,#220,#221,#222,#223,#224,#225,#226,#227,
#228),#26702,.T.);
#27978=ADVANCED_FACE('',(#4175),#161,.T.);
#27979=ADVANCED_FACE('',(#4176),#162,.T.);
#27980=ADVANCED_FACE('',(#4177),#163,.T.);
#27981=ADVANCED_FACE('',(#4178),#164,.T.);
#27982=ADVANCED_FACE('',(#4179),#165,.T.);
#27983=ADVANCED_FACE('',(#4180),#166,.T.);
#27984=ADVANCED_FACE('',(#4181),#167,.T.);
#27985=ADVANCED_FACE('',(#4182),#168,.T.);
#27986=ADVANCED_FACE('',(#4183),#169,.T.);
#27987=ADVANCED_FACE('',(#4184),#170,.T.);
#27988=ADVANCED_FACE('',(#4185),#171,.T.);
#27989=ADVANCED_FACE('',(#4186),#172,.T.);
#27990=ADVANCED_FACE('',(#4187),#26703,.F.);
#27991=ADVANCED_FACE('',(#4188),#26704,.F.);
#27992=ADVANCED_FACE('',(#4189),#26705,.F.);
#27993=ADVANCED_FACE('',(#4190),#26706,.F.);
#27994=ADVANCED_FACE('',(#4191),#26707,.F.);
#27995=ADVANCED_FACE('',(#4192),#26708,.F.);
#27996=ADVANCED_FACE('',(#4193),#26709,.F.);
#27997=ADVANCED_FACE('',(#4194),#2938,.F.);
#27998=ADVANCED_FACE('',(#4195,#229),#26710,.T.);
#27999=ADVANCED_FACE('',(#4196),#2939,.F.);
#28000=ADVANCED_FACE('',(#4197),#26711,.F.);
#28001=ADVANCED_FACE('',(#4198),#2940,.F.);
#28002=ADVANCED_FACE('',(#4199),#26712,.F.);
#28003=ADVANCED_FACE('',(#4200),#26713,.F.);
#28004=ADVANCED_FACE('',(#4201,#230,#231,#232),#26714,.T.);
#28005=ADVANCED_FACE('',(#4202),#26715,.F.);
#28006=ADVANCED_FACE('',(#4203),#26716,.F.);
#28007=ADVANCED_FACE('',(#4204),#26717,.F.);
#28008=ADVANCED_FACE('',(#4205),#26718,.F.);
#28009=ADVANCED_FACE('',(#4206),#26719,.F.);
#28010=ADVANCED_FACE('',(#4207),#26720,.F.);
#28011=ADVANCED_FACE('',(#4208),#26721,.F.);
#28012=ADVANCED_FACE('',(#4209),#2941,.F.);
#28013=ADVANCED_FACE('',(#4210,#233),#26722,.T.);
#28014=ADVANCED_FACE('',(#4211),#26723,.F.);
#28015=ADVANCED_FACE('',(#4212),#26724,.F.);
#28016=ADVANCED_FACE('',(#4213),#2942,.F.);
#28017=ADVANCED_FACE('',(#4214),#26725,.T.);
#28018=ADVANCED_FACE('',(#4215),#26726,.T.);
#28019=ADVANCED_FACE('',(#4216),#2943,.F.);
#28020=ADVANCED_FACE('',(#4217),#26727,.T.);
#28021=ADVANCED_FACE('',(#4218),#2944,.F.);
#28022=ADVANCED_FACE('',(#4219),#26728,.T.);
#28023=ADVANCED_FACE('',(#4220),#2945,.F.);
#28024=ADVANCED_FACE('',(#4221),#26729,.T.);
#28025=ADVANCED_FACE('',(#4222),#26730,.T.);
#28026=ADVANCED_FACE('',(#4223,#234,#235,#236),#26731,.F.);
#28027=ADVANCED_FACE('',(#4224),#26732,.T.);
#28028=ADVANCED_FACE('',(#4225),#26733,.T.);
#28029=ADVANCED_FACE('',(#4226),#26734,.T.);
#28030=ADVANCED_FACE('',(#4227),#26735,.T.);
#28031=ADVANCED_FACE('',(#4228),#26736,.T.);
#28032=ADVANCED_FACE('',(#4229),#26737,.T.);
#28033=ADVANCED_FACE('',(#4230),#26738,.T.);
#28034=ADVANCED_FACE('',(#4231),#2946,.F.);
#28035=ADVANCED_FACE('',(#4232,#237),#26739,.F.);
#28036=ADVANCED_FACE('',(#4233),#26740,.T.);
#28037=ADVANCED_FACE('',(#4234),#26741,.T.);
#28038=ADVANCED_FACE('',(#4235),#26742,.T.);
#28039=ADVANCED_FACE('',(#4236),#26743,.T.);
#28040=ADVANCED_FACE('',(#4237),#26744,.T.);
#28041=ADVANCED_FACE('',(#4238),#26745,.T.);
#28042=ADVANCED_FACE('',(#4239),#26746,.T.);
#28043=ADVANCED_FACE('',(#4240),#2947,.F.);
#28044=ADVANCED_FACE('',(#4241,#238),#26747,.F.);
#28045=ADVANCED_FACE('',(#4242),#26748,.F.);
#28046=ADVANCED_FACE('',(#4243),#26749,.F.);
#28047=ADVANCED_FACE('',(#4244,#239,#240),#26750,.F.);
#28048=ADVANCED_FACE('',(#4245),#26751,.F.);
#28049=ADVANCED_FACE('',(#4246),#2948,.F.);
#28050=ADVANCED_FACE('',(#4247),#26752,.F.);
#28051=ADVANCED_FACE('',(#4248),#2949,.F.);
#28052=ADVANCED_FACE('',(#4249),#26753,.F.);
#28053=ADVANCED_FACE('',(#4250),#2950,.F.);
#28054=ADVANCED_FACE('',(#4251),#26754,.F.);
#28055=ADVANCED_FACE('',(#4252),#2951,.F.);
#28056=ADVANCED_FACE('',(#4253),#26755,.F.);
#28057=ADVANCED_FACE('',(#4254),#26756,.F.);
#28058=ADVANCED_FACE('',(#4255),#2952,.T.);
#28059=ADVANCED_FACE('',(#4256),#2953,.F.);
#28060=ADVANCED_FACE('',(#4257),#26757,.F.);
#28061=ADVANCED_FACE('',(#4258),#2954,.T.);
#28062=ADVANCED_FACE('',(#4259),#26758,.F.);
#28063=ADVANCED_FACE('',(#4260),#2955,.T.);
#28064=ADVANCED_FACE('',(#4261),#26759,.F.);
#28065=ADVANCED_FACE('',(#4262),#2956,.T.);
#28066=ADVANCED_FACE('',(#4263),#2957,.T.);
#28067=ADVANCED_FACE('',(#4264),#26760,.F.);
#28068=ADVANCED_FACE('',(#4265),#2958,.T.);
#28069=ADVANCED_FACE('',(#4266,#241,#242),#26761,.F.);
#28070=ADVANCED_FACE('',(#4267),#2959,.T.);
#28071=ADVANCED_FACE('',(#4268),#26762,.F.);
#28072=ADVANCED_FACE('',(#4269),#2960,.T.);
#28073=ADVANCED_FACE('',(#4270),#26763,.F.);
#28074=ADVANCED_FACE('',(#4271),#2961,.T.);
#28075=ADVANCED_FACE('',(#4272),#26764,.F.);
#28076=ADVANCED_FACE('',(#4273),#2962,.F.);
#28077=ADVANCED_FACE('',(#4274),#26765,.F.);
#28078=ADVANCED_FACE('',(#4275),#2963,.T.);
#28079=ADVANCED_FACE('',(#4276,#243,#244,#245,#246),#26766,.F.);
#28080=CLOSED_SHELL('',(#26767,#26768,#26769,#26770,#26771,#26772,#26773,
#26774,#26775,#26776,#26777,#26778,#26779,#26780,#26781,#26782,#26783,#26784,
#26785,#26786,#26787,#26788,#26789,#26790,#26791,#26792,#26793));
#28081=CLOSED_SHELL('',(#26794,#26795,#26796,#26797,#26798,#26799,#26800,
#26801,#26802,#26803,#26804,#26805,#26806,#26807,#26808,#26809,#26810,#26811,
#26812,#26813,#26814,#26815,#26816,#26817,#26818,#26819,#26820,#26821));
#28082=CLOSED_SHELL('',(#26822,#26823,#26824,#26825,#26826,#26827,#26828,
#26829,#26830,#26831,#26832,#26833,#26834,#26835,#26836,#26837,#26838,#26839,
#26840,#26841,#26842,#26843,#26844,#26845,#26846,#26847,#26848,#26849,#26850,
#26851,#26852,#26853,#26854,#26855,#26856,#26857,#26858,#26859,#26860,#26861,
#26862,#26863,#26864,#26865,#26866,#26867,#26868,#26869,#26870,#26871,#26872,
#26873,#26874,#26875,#26876,#26877,#26878,#26879,#26880,#26881,#26882,#26883,
#26884,#26885,#26886,#26887,#26888,#26889,#26890,#26891,#26892,#26893,#26894,
#26895,#26896,#26897,#26898,#26899,#26900,#26901,#26902,#26903,#26904,#26905,
#26906,#26907,#26908,#26909,#26910,#26911,#26912,#26913,#26914,#26915,#26916,
#26917,#26918,#26919,#26920,#26921,#26922,#26923,#26924,#26925,#26926,#26927,
#26928,#26929,#26930,#26931,#26932,#26933,#26934,#26935,#26936,#26937,#26938,
#26939,#26940,#26941,#26942,#26943,#26944,#26945,#26946,#26947,#26948,#26949,
#26950,#26951,#26952,#26953,#26954,#26955,#26956,#26957,#26958,#26959,#26960,
#26961,#26962,#26963,#26964,#26965,#26966,#26967,#26968,#26969,#26970,#26971,
#26972,#26973,#26974,#26975,#26976,#26977,#26978,#26979,#26980,#26981,#26982,
#26983,#26984,#26985,#26986,#26987,#26988,#26989,#26990,#26991,#26992,#26993,
#26994,#26995,#26996,#26997,#26998,#26999,#27000,#27001,#27002,#27003,#27004,
#27005,#27006,#27007,#27008,#27009,#27010,#27011,#27012,#27013,#27014,#27015,
#27016,#27017,#27018,#27019,#27020,#27021,#27022,#27023,#27024,#27025,#27026,
#27027,#27028,#27029,#27030,#27031,#27032,#27033,#27034,#27035,#27036,#27037,
#27038,#27039,#27040,#27041,#27042,#27043,#27044,#27045,#27046,#27047,#27048,
#27049,#27050,#27051,#27052,#27053,#27054,#27055,#27056,#27057,#27058,#27059,
#27060,#27061,#27062,#27063,#27064,#27065,#27066,#27067,#27068,#27069,#27070,
#27071,#27072,#27073,#27074,#27075,#27076,#27077,#27078,#27079,#27080,#27081,
#27082,#27083,#27084,#27085,#27086,#27087,#27088,#27089,#27090,#27091,#27092,
#27093,#27094,#27095,#27096,#27097,#27098,#27099,#27100,#27101,#27102,#27103,
#27104,#27105,#27106,#27107,#27108,#27109,#27110,#27111,#27112,#27113,#27114,
#27115,#27116,#27117,#27118,#27119,#27120,#27121,#27122,#27123,#27124,#27125,
#27126,#27127,#27128,#27129,#27130,#27131,#27132,#27133,#27134,#27135,#27136,
#27137,#27138,#27139,#27140,#27141,#27142,#27143,#27144,#27145,#27146,#27147,
#27148,#27149,#27150,#27151,#27152,#27153,#27154,#27155,#27156,#27157,#27158,
#27159,#27160,#27161,#27162,#27163,#27164,#27165,#27166,#27167,#27168,#27169,
#27170,#27171,#27172,#27173,#27174,#27175,#27176,#27177,#27178,#27179,#27180,
#27181));
#28083=CLOSED_SHELL('',(#27182,#27183,#27184,#27185,#27186,#27187,#27188,
#27189,#27190,#27191,#27192,#27193,#27194,#27195,#27196,#27197,#27198,#27199,
#27200,#27201,#27202,#27203,#27204,#27205,#27206,#27207,#27208,#27209,#27210,
#27211,#27212,#27213,#27214,#27215,#27216,#27217,#27218,#27219,#27220,#27221,
#27222,#27223,#27224,#27225,#27226,#27227,#27228,#27229,#27230,#27231,#27232,
#27233,#27234,#27235,#27236,#27237,#27238,#27239,#27240,#27241,#27242,#27243,
#27244,#27245,#27246,#27247,#27248,#27249,#27250,#27251,#27252,#27253,#27254,
#27255,#27256,#27257,#27258,#27259,#27260,#27261,#27262,#27263,#27264,#27265,
#27266,#27267,#27268,#27269,#27270,#27271,#27272,#27273,#27274,#27275,#27276,
#27277,#27278,#27279,#27280,#27281,#27282,#27283,#27284,#27285,#27286,#27287,
#27288,#27289,#27290,#27291));
#28084=CLOSED_SHELL('',(#27292,#27293,#27294,#27295,#27296,#27297,#27298,
#27299,#27300,#27301,#27302,#27303,#27304,#27305,#27306,#27307,#27308,#27309,
#27310,#27311,#27312,#27313,#27314,#27315,#27316,#27317,#27318,#27319,#27320,
#27321,#27322,#27323,#27324,#27325,#27326,#27327,#27328,#27329,#27330,#27331,
#27332,#27333,#27334,#27335,#27336,#27337,#27338,#27339,#27340,#27341,#27342,
#27343,#27344,#27345,#27346,#27347,#27348,#27349,#27350,#27351,#27352,#27353,
#27354,#27355,#27356,#27357,#27358,#27359,#27360,#27361,#27362,#27363,#27364,
#27365,#27366,#27367,#27368,#27369,#27370,#27371,#27372,#27373,#27374,#27375,
#27376,#27377,#27378,#27379,#27380,#27381,#27382,#27383,#27384,#27385,#27386,
#27387,#27388,#27389,#27390,#27391,#27392,#27393,#27394,#27395,#27396,#27397,
#27398,#27399,#27400,#27401));
#28085=CLOSED_SHELL('',(#27402,#27403,#27404,#27405,#27406,#27407,#27408,
#27409,#27410,#27411,#27412,#27413,#27414,#27415,#27416,#27417,#27418,#27419,
#27420,#27421,#27422,#27423,#27424,#27425,#27426,#27427,#27428,#27429,#27430,
#27431,#27432,#27433,#27434,#27435,#27436,#27437,#27438,#27439,#27440,#27441,
#27442,#27443,#27444,#27445,#27446,#27447,#27448,#27449,#27450,#27451,#27452,
#27453,#27454,#27455,#27456,#27457,#27458,#27459,#27460,#27461,#27462,#27463,
#27464,#27465,#27466,#27467,#27468,#27469,#27470,#27471,#27472,#27473,#27474,
#27475,#27476,#27477,#27478,#27479,#27480,#27481,#27482,#27483,#27484,#27485,
#27486,#27487,#27488,#27489,#27490,#27491,#27492,#27493,#27494,#27495,#27496,
#27497,#27498,#27499,#27500,#27501,#27502,#27503,#27504,#27505,#27506,#27507,
#27508,#27509,#27510,#27511,#27512,#27513,#27514,#27515,#27516,#27517,#27518,
#27519,#27520,#27521,#27522,#27523,#27524,#27525,#27526,#27527,#27528,#27529,
#27530,#27531,#27532,#27533,#27534,#27535,#27536,#27537,#27538,#27539,#27540,
#27541,#27542,#27543,#27544,#27545,#27546,#27547,#27548,#27549,#27550,#27551,
#27552,#27553,#27554));
#28086=CLOSED_SHELL('',(#27555,#27556,#27557,#27558,#27559,#27560,#27561,
#27562,#27563,#27564,#27565,#27566,#27567,#27568,#27569,#27570,#27571,#27572,
#27573,#27574,#27575,#27576,#27577,#27578,#27579,#27580,#27581,#27582,#27583,
#27584,#27585,#27586,#27587,#27588,#27589,#27590,#27591,#27592,#27593,#27594,
#27595,#27596,#27597,#27598,#27599,#27600,#27601,#27602,#27603,#27604,#27605,
#27606,#27607,#27608,#27609,#27610,#27611,#27612,#27613,#27614,#27615,#27616,
#27617,#27618,#27619,#27620,#27621,#27622,#27623,#27624));
#28087=CLOSED_SHELL('',(#27625,#27626,#27627,#27628,#27629,#27630,#27631,
#27632,#27633,#27634,#27635,#27636,#27637,#27638,#27639,#27640,#27641,#27642,
#27643,#27644,#27645,#27646,#27647,#27648,#27649,#27650,#27651,#27652,#27653,
#27654,#27655,#27656,#27657,#27658,#27659,#27660,#27661,#27662,#27663,#27664,
#27665,#27666,#27667,#27668,#27669,#27670,#27671,#27672,#27673,#27674,#27675,
#27676,#27677,#27678,#27679,#27680,#27681,#27682,#27683,#27684,#27685,#27686,
#27687,#27688,#27689,#27690,#27691,#27692,#27693,#27694,#27695,#27696,#27697,
#27698,#27699,#27700,#27701,#27702,#27703,#27704,#27705,#27706,#27707,#27708,
#27709,#27710,#27711,#27712,#27713,#27714,#27715,#27716,#27717,#27718,#27719));
#28088=CLOSED_SHELL('',(#27720,#27721,#27722,#27723,#27724,#27725,#27726,
#27727,#27728,#27729,#27730,#27731,#27732,#27733,#27734,#27735,#27736,#27737,
#27738,#27739,#27740,#27741,#27742,#27743,#27744,#27745,#27746,#27747,#27748,
#27749,#27750,#27751,#27752,#27753,#27754,#27755,#27756,#27757,#27758,#27759,
#27760,#27761,#27762,#27763,#27764,#27765,#27766,#27767,#27768,#27769,#27770,
#27771,#27772,#27773,#27774,#27775,#27776,#27777,#27778,#27779,#27780,#27781,
#27782,#27783,#27784,#27785,#27786,#27787,#27788,#27789,#27790,#27791,#27792,
#27793,#27794,#27795,#27796,#27797,#27798,#27799,#27800,#27801,#27802,#27803,
#27804,#27805,#27806,#27807,#27808,#27809,#27810,#27811,#27812,#27813,#27814,
#27815,#27816,#27817,#27818,#27819,#27820,#27821,#27822,#27823,#27824,#27825,
#27826,#27827,#27828,#27829,#27830,#27831,#27832,#27833,#27834,#27835,#27836,
#27837,#27838,#27839,#27840,#27841,#27842,#27843,#27844,#27845,#27846,#27847,
#27848,#27849,#27850,#27851,#27852,#27853,#27854,#27855,#27856,#27857,#27858,
#27859,#27860,#27861,#27862,#27863,#27864,#27865,#27866,#27867,#27868,#27869,
#27870,#27871,#27872,#27873,#27874,#27875,#27876,#27877,#27878,#27879,#27880,
#27881,#27882,#27883,#27884,#27885,#27886,#27887,#27888,#27889,#27890,#27891,
#27892,#27893,#27894,#27895,#27896,#27897,#27898,#27899,#27900,#27901,#27902,
#27903,#27904,#27905,#27906,#27907,#27908,#27909,#27910,#27911,#27912,#27913,
#27914,#27915,#27916,#27917,#27918,#27919,#27920,#27921,#27922,#27923,#27924,
#27925,#27926,#27927,#27928,#27929,#27930,#27931,#27932,#27933,#27934,#27935,
#27936,#27937,#27938,#27939,#27940,#27941,#27942,#27943,#27944,#27945,#27946,
#27947,#27948,#27949,#27950,#27951,#27952,#27953,#27954,#27955,#27956,#27957,
#27958,#27959,#27960,#27961,#27962,#27963,#27964,#27965,#27966,#27967,#27968,
#27969,#27970,#27971,#27972,#27973,#27974,#27975,#27976,#27977,#27978,#27979,
#27980,#27981,#27982,#27983,#27984,#27985,#27986,#27987,#27988,#27989,#27990,
#27991,#27992,#27993,#27994,#27995,#27996,#27997,#27998,#27999,#28000,#28001,
#28002,#28003,#28004,#28005,#28006,#28007,#28008,#28009,#28010,#28011,#28012,
#28013,#28014,#28015,#28016,#28017,#28018,#28019,#28020,#28021,#28022,#28023,
#28024,#28025,#28026,#28027,#28028,#28029,#28030,#28031,#28032,#28033,#28034,
#28035,#28036,#28037,#28038,#28039,#28040,#28041,#28042,#28043,#28044,#28045,
#28046,#28047,#28048,#28049,#28050,#28051,#28052,#28053,#28054,#28055,#28056,
#28057,#28058,#28059,#28060,#28061,#28062,#28063,#28064,#28065,#28066,#28067,
#28068,#28069,#28070,#28071,#28072,#28073,#28074,#28075,#28076,#28077,#28078,
#28079));
#28089=DERIVED_UNIT_ELEMENT(#28105,1.);
#28090=DERIVED_UNIT_ELEMENT(#215611,-3.);
#28091=DERIVED_UNIT_ELEMENT(#28105,1.);
#28092=DERIVED_UNIT_ELEMENT(#215611,-3.);
#28093=DERIVED_UNIT_ELEMENT(#28105,1.);
#28094=DERIVED_UNIT_ELEMENT(#215611,-3.);
#28095=DERIVED_UNIT_ELEMENT(#28105,1.);
#28096=DERIVED_UNIT_ELEMENT(#215611,-3.);
#28097=DERIVED_UNIT_ELEMENT(#28105,1.);
#28098=DERIVED_UNIT_ELEMENT(#215611,-3.);
#28099=DERIVED_UNIT_ELEMENT(#28105,1.);
#28100=DERIVED_UNIT_ELEMENT(#215611,-3.);
#28101=DERIVED_UNIT_ELEMENT(#28105,1.);
#28102=DERIVED_UNIT_ELEMENT(#215611,-3.);
#28103=DERIVED_UNIT_ELEMENT(#28105,1.);
#28104=DERIVED_UNIT_ELEMENT(#215611,-3.);
#28105=(
MASS_UNIT()
NAMED_UNIT(*)
SI_UNIT(.KILO.,.GRAM.)
);
#28106=DERIVED_UNIT((#28089,#28090));
#28107=DERIVED_UNIT((#28091,#28092));
#28108=DERIVED_UNIT((#28093,#28094));
#28109=DERIVED_UNIT((#28095,#28096));
#28110=DERIVED_UNIT((#28097,#28098));
#28111=DERIVED_UNIT((#28099,#28100));
#28112=DERIVED_UNIT((#28101,#28102));
#28113=DERIVED_UNIT((#28103,#28104));
#28114=MEASURE_REPRESENTATION_ITEM('density measure',
POSITIVE_RATIO_MEASURE(7850.),#28106);
#28115=MEASURE_REPRESENTATION_ITEM('density measure',
POSITIVE_RATIO_MEASURE(7850.),#28107);
#28116=MEASURE_REPRESENTATION_ITEM('density measure',
POSITIVE_RATIO_MEASURE(7850.),#28108);
#28117=MEASURE_REPRESENTATION_ITEM('density measure',
POSITIVE_RATIO_MEASURE(7850.),#28109);
#28118=MEASURE_REPRESENTATION_ITEM('density measure',
POSITIVE_RATIO_MEASURE(7850.),#28110);
#28119=MEASURE_REPRESENTATION_ITEM('density measure',
POSITIVE_RATIO_MEASURE(7850.),#28111);
#28120=MEASURE_REPRESENTATION_ITEM('density measure',
POSITIVE_RATIO_MEASURE(7850.),#28112);
#28121=MEASURE_REPRESENTATION_ITEM('density measure',
POSITIVE_RATIO_MEASURE(7850.),#28113);
#28122=PROPERTY_DEFINITION_REPRESENTATION(#28162,#28138);
#28123=PROPERTY_DEFINITION_REPRESENTATION(#28163,#28139);
#28124=PROPERTY_DEFINITION_REPRESENTATION(#28164,#28140);
#28125=PROPERTY_DEFINITION_REPRESENTATION(#28165,#28141);
#28126=PROPERTY_DEFINITION_REPRESENTATION(#28166,#28142);
#28127=PROPERTY_DEFINITION_REPRESENTATION(#28167,#28143);
#28128=PROPERTY_DEFINITION_REPRESENTATION(#28168,#28144);
#28129=PROPERTY_DEFINITION_REPRESENTATION(#28169,#28145);
#28130=PROPERTY_DEFINITION_REPRESENTATION(#28170,#28146);
#28131=PROPERTY_DEFINITION_REPRESENTATION(#28171,#28147);
#28132=PROPERTY_DEFINITION_REPRESENTATION(#28172,#28148);
#28133=PROPERTY_DEFINITION_REPRESENTATION(#28173,#28149);
#28134=PROPERTY_DEFINITION_REPRESENTATION(#28174,#28150);
#28135=PROPERTY_DEFINITION_REPRESENTATION(#28175,#28151);
#28136=PROPERTY_DEFINITION_REPRESENTATION(#28176,#28152);
#28137=PROPERTY_DEFINITION_REPRESENTATION(#28177,#28153);
#28138=REPRESENTATION('material name',(#28154),#215600);
#28139=REPRESENTATION('density',(#28114),#215600);
#28140=REPRESENTATION('material name',(#28155),#215601);
#28141=REPRESENTATION('density',(#28115),#215601);
#28142=REPRESENTATION('material name',(#28156),#215602);
#28143=REPRESENTATION('density',(#28116),#215602);
#28144=REPRESENTATION('material name',(#28157),#215604);
#28145=REPRESENTATION('density',(#28117),#215604);
#28146=REPRESENTATION('material name',(#28158),#215605);
#28147=REPRESENTATION('density',(#28118),#215605);
#28148=REPRESENTATION('material name',(#28159),#215606);
#28149=REPRESENTATION('density',(#28119),#215606);
#28150=REPRESENTATION('material name',(#28160),#215607);
#28151=REPRESENTATION('density',(#28120),#215607);
#28152=REPRESENTATION('material name',(#28161),#215608);
#28153=REPRESENTATION('density',(#28121),#215608);
#28154=DESCRIPTIVE_REPRESENTATION_ITEM('Steel','Steel');
#28155=DESCRIPTIVE_REPRESENTATION_ITEM('Steel','Steel');
#28156=DESCRIPTIVE_REPRESENTATION_ITEM('Steel','Steel');
#28157=DESCRIPTIVE_REPRESENTATION_ITEM('Steel','Steel');
#28158=DESCRIPTIVE_REPRESENTATION_ITEM('Steel','Steel');
#28159=DESCRIPTIVE_REPRESENTATION_ITEM('Steel','Steel');
#28160=DESCRIPTIVE_REPRESENTATION_ITEM('Steel','Steel');
#28161=DESCRIPTIVE_REPRESENTATION_ITEM('Steel','Steel');
#28162=PROPERTY_DEFINITION('material property','material name',#215655);
#28163=PROPERTY_DEFINITION('material property','density of part',#215655);
#28164=PROPERTY_DEFINITION('material property','material name',#215656);
#28165=PROPERTY_DEFINITION('material property','density of part',#215656);
#28166=PROPERTY_DEFINITION('material property','material name',#215657);
#28167=PROPERTY_DEFINITION('material property','density of part',#215657);
#28168=PROPERTY_DEFINITION('material property','material name',#215659);
#28169=PROPERTY_DEFINITION('material property','density of part',#215659);
#28170=PROPERTY_DEFINITION('material property','material name',#215660);
#28171=PROPERTY_DEFINITION('material property','density of part',#215660);
#28172=PROPERTY_DEFINITION('material property','material name',#215661);
#28173=PROPERTY_DEFINITION('material property','density of part',#215661);
#28174=PROPERTY_DEFINITION('material property','material name',#215662);
#28175=PROPERTY_DEFINITION('material property','density of part',#215662);
#28176=PROPERTY_DEFINITION('material property','material name',#215663);
#28177=PROPERTY_DEFINITION('material property','density of part',#215663);
#28178=AXIS2_PLACEMENT_3D('',#35981,#30164,#30165);
#28179=AXIS2_PLACEMENT_3D('',#35982,#30166,#30167);
#28180=AXIS2_PLACEMENT_3D('',#35983,#30168,#30169);
#28181=AXIS2_PLACEMENT_3D('',#35992,#30173,#30174);
#28182=AXIS2_PLACEMENT_3D('',#35996,#30176,#30177);
#28183=AXIS2_PLACEMENT_3D('',#36000,#30179,#30180);
#28184=AXIS2_PLACEMENT_3D('',#36004,#30182,#30183);
#28185=AXIS2_PLACEMENT_3D('',#36008,#30185,#30186);
#28186=AXIS2_PLACEMENT_3D('',#36014,#30189,#30190);
#28187=AXIS2_PLACEMENT_3D('',#36018,#30192,#30193);
#28188=AXIS2_PLACEMENT_3D('',#36022,#30195,#30196);
#28189=AXIS2_PLACEMENT_3D('',#36026,#30198,#30199);
#28190=AXIS2_PLACEMENT_3D('',#36030,#30201,#30202);
#28191=AXIS2_PLACEMENT_3D('',#36034,#30205,#30206);
#28192=AXIS2_PLACEMENT_3D('',#36040,#30210,#30211);
#28193=AXIS2_PLACEMENT_3D('',#36044,#30214,#30215);
#28194=AXIS2_PLACEMENT_3D('',#36046,#30216,#30217);
#28195=AXIS2_PLACEMENT_3D('',#36048,#30219,#30220);
#28196=AXIS2_PLACEMENT_3D('',#36052,#30223,#30224);
#28197=AXIS2_PLACEMENT_3D('',#36054,#30225,#30226);
#28198=AXIS2_PLACEMENT_3D('',#36056,#30228,#30229);
#28199=AXIS2_PLACEMENT_3D('',#36060,#30232,#30233);
#28200=AXIS2_PLACEMENT_3D('',#36062,#30234,#30235);
#28201=AXIS2_PLACEMENT_3D('',#36064,#30237,#30238);
#28202=AXIS2_PLACEMENT_3D('',#36068,#30241,#30242);
#28203=AXIS2_PLACEMENT_3D('',#36070,#30243,#30244);
#28204=AXIS2_PLACEMENT_3D('',#36072,#30246,#30247);
#28205=AXIS2_PLACEMENT_3D('',#36076,#30250,#30251);
#28206=AXIS2_PLACEMENT_3D('',#36078,#30252,#30253);
#28207=AXIS2_PLACEMENT_3D('',#36080,#30255,#30256);
#28208=AXIS2_PLACEMENT_3D('',#36084,#30259,#30260);
#28209=AXIS2_PLACEMENT_3D('',#36088,#30263,#30264);
#28210=AXIS2_PLACEMENT_3D('',#36090,#30265,#30266);
#28211=AXIS2_PLACEMENT_3D('',#36092,#30268,#30269);
#28212=AXIS2_PLACEMENT_3D('',#36096,#30272,#30273);
#28213=AXIS2_PLACEMENT_3D('',#36098,#30274,#30275);
#28214=AXIS2_PLACEMENT_3D('',#36100,#30277,#30278);
#28215=AXIS2_PLACEMENT_3D('',#36104,#30281,#30282);
#28216=AXIS2_PLACEMENT_3D('',#36106,#30283,#30284);
#28217=AXIS2_PLACEMENT_3D('',#36108,#30286,#30287);
#28218=AXIS2_PLACEMENT_3D('',#36112,#30290,#30291);
#28219=AXIS2_PLACEMENT_3D('',#36114,#30292,#30293);
#28220=AXIS2_PLACEMENT_3D('',#36116,#30295,#30296);
#28221=AXIS2_PLACEMENT_3D('',#36120,#30299,#30300);
#28222=AXIS2_PLACEMENT_3D('',#36122,#30301,#30302);
#28223=AXIS2_PLACEMENT_3D('',#36124,#30304,#30305);
#28224=AXIS2_PLACEMENT_3D('',#36128,#30308,#30309);
#28225=AXIS2_PLACEMENT_3D('',#36132,#30312,#30313);
#28226=AXIS2_PLACEMENT_3D('',#36134,#30315,#30316);
#28227=AXIS2_PLACEMENT_3D('',#36135,#30317,#30318);
#28228=AXIS2_PLACEMENT_3D('',#36136,#30319,#30320);
#28229=AXIS2_PLACEMENT_3D('',#36141,#30322,#30323);
#28230=AXIS2_PLACEMENT_3D('',#36145,#30325,#30326);
#28231=AXIS2_PLACEMENT_3D('',#36149,#30328,#30329);
#28232=AXIS2_PLACEMENT_3D('',#36163,#30336,#30337);
#28233=AXIS2_PLACEMENT_3D('',#36167,#30339,#30340);
#28234=AXIS2_PLACEMENT_3D('',#36171,#30342,#30343);
#28235=AXIS2_PLACEMENT_3D('',#36175,#30345,#30346);
#28236=AXIS2_PLACEMENT_3D('',#36188,#30353,#30354);
#28237=AXIS2_PLACEMENT_3D('',#36189,#30355,#30356);
#28238=AXIS2_PLACEMENT_3D('',#36193,#30358,#30359);
#28239=AXIS2_PLACEMENT_3D('',#36195,#30361,#30362);
#28240=AXIS2_PLACEMENT_3D('',#36199,#30365,#30366);
#28241=AXIS2_PLACEMENT_3D('',#36201,#30367,#30368);
#28242=AXIS2_PLACEMENT_3D('',#36203,#30370,#30371);
#28243=AXIS2_PLACEMENT_3D('',#36207,#30374,#30375);
#28244=AXIS2_PLACEMENT_3D('',#36209,#30376,#30377);
#28245=AXIS2_PLACEMENT_3D('',#36211,#30379,#30380);
#28246=AXIS2_PLACEMENT_3D('',#36215,#30383,#30384);
#28247=AXIS2_PLACEMENT_3D('',#36219,#30387,#30388);
#28248=AXIS2_PLACEMENT_3D('',#36223,#30391,#30392);
#28249=AXIS2_PLACEMENT_3D('',#36227,#30395,#30396);
#28250=AXIS2_PLACEMENT_3D('',#36231,#30399,#30400);
#28251=AXIS2_PLACEMENT_3D('',#36235,#30403,#30404);
#28252=AXIS2_PLACEMENT_3D('',#36237,#30405,#30406);
#28253=AXIS2_PLACEMENT_3D('',#36239,#30408,#30409);
#28254=AXIS2_PLACEMENT_3D('',#36243,#30412,#30413);
#28255=AXIS2_PLACEMENT_3D('',#36245,#30414,#30415);
#28256=AXIS2_PLACEMENT_3D('',#36247,#30417,#30418);
#28257=AXIS2_PLACEMENT_3D('',#36251,#30421,#30422);
#28258=AXIS2_PLACEMENT_3D('',#36253,#30423,#30424);
#28259=AXIS2_PLACEMENT_3D('',#36255,#30426,#30427);
#28260=AXIS2_PLACEMENT_3D('',#36259,#30430,#30431);
#28261=AXIS2_PLACEMENT_3D('',#36261,#30432,#30433);
#28262=AXIS2_PLACEMENT_3D('',#36263,#30435,#30436);
#28263=AXIS2_PLACEMENT_3D('',#36267,#30439,#30440);
#28264=AXIS2_PLACEMENT_3D('',#36271,#30443,#30444);
#28265=AXIS2_PLACEMENT_3D('',#36275,#30447,#30448);
#28266=AXIS2_PLACEMENT_3D('',#36279,#30451,#30452);
#28267=AXIS2_PLACEMENT_3D('',#36283,#30455,#30456);
#28268=AXIS2_PLACEMENT_3D('',#36287,#30459,#30460);
#28269=AXIS2_PLACEMENT_3D('',#36289,#30461,#30462);
#28270=AXIS2_PLACEMENT_3D('',#36291,#30464,#30465);
#28271=AXIS2_PLACEMENT_3D('',#36293,#30467,#30468);
#28272=AXIS2_PLACEMENT_3D('',#36294,#30469,#30470);
#28273=AXIS2_PLACEMENT_3D('',#36295,#30471,#30472);
#28274=AXIS2_PLACEMENT_3D('',#36307,#30474,#30475);
#28275=AXIS2_PLACEMENT_3D('',#36381,#30476,#30477);
#28276=AXIS2_PLACEMENT_3D('',#36644,#30479,#30480);
#28277=AXIS2_PLACEMENT_3D('',#37042,#30482,#30483);
#28278=AXIS2_PLACEMENT_3D('',#37140,#30485,#30486);
#28279=AXIS2_PLACEMENT_3D('',#37218,#30487,#30488);
#28280=AXIS2_PLACEMENT_3D('',#37230,#30490,#30491);
#28281=AXIS2_PLACEMENT_3D('',#37304,#30492,#30493);
#28282=AXIS2_PLACEMENT_3D('',#37567,#30495,#30496);
#28283=AXIS2_PLACEMENT_3D('',#37965,#30498,#30499);
#28284=AXIS2_PLACEMENT_3D('',#38063,#30501,#30502);
#28285=AXIS2_PLACEMENT_3D('',#38141,#30503,#30504);
#28286=AXIS2_PLACEMENT_3D('',#38161,#30506,#30507);
#28287=AXIS2_PLACEMENT_3D('',#38229,#30508,#30509);
#28288=AXIS2_PLACEMENT_3D('',#38380,#30511,#30512);
#28289=AXIS2_PLACEMENT_3D('',#38713,#30514,#30515);
#28290=AXIS2_PLACEMENT_3D('',#38994,#30517,#30518);
#28291=AXIS2_PLACEMENT_3D('',#39330,#30520,#30521);
#28292=AXIS2_PLACEMENT_3D('',#39492,#30523,#30524);
#28293=AXIS2_PLACEMENT_3D('',#39762,#30526,#30527);
#28294=AXIS2_PLACEMENT_3D('',#40037,#30529,#30530);
#28295=AXIS2_PLACEMENT_3D('',#40371,#30532,#30533);
#28296=AXIS2_PLACEMENT_3D('',#40533,#30535,#30536);
#28297=AXIS2_PLACEMENT_3D('',#40800,#30538,#30539);
#28298=AXIS2_PLACEMENT_3D('',#41078,#30541,#30542);
#28299=AXIS2_PLACEMENT_3D('',#41411,#30544,#30545);
#28300=AXIS2_PLACEMENT_3D('',#41576,#30547,#30548);
#28301=AXIS2_PLACEMENT_3D('',#41845,#30550,#30551);
#28302=AXIS2_PLACEMENT_3D('',#42126,#30553,#30554);
#28303=AXIS2_PLACEMENT_3D('',#42459,#30556,#30557);
#28304=AXIS2_PLACEMENT_3D('',#42618,#30559,#30560);
#28305=AXIS2_PLACEMENT_3D('',#42888,#30562,#30563);
#28306=AXIS2_PLACEMENT_3D('',#43169,#30565,#30566);
#28307=AXIS2_PLACEMENT_3D('',#43500,#30568,#30569);
#28308=AXIS2_PLACEMENT_3D('',#43663,#30571,#30572);
#28309=AXIS2_PLACEMENT_3D('',#43929,#30574,#30575);
#28310=AXIS2_PLACEMENT_3D('',#44210,#30577,#30578);
#28311=AXIS2_PLACEMENT_3D('',#44543,#30580,#30581);
#28312=AXIS2_PLACEMENT_3D('',#44824,#30583,#30584);
#28313=AXIS2_PLACEMENT_3D('',#44842,#30586,#30587);
#28314=AXIS2_PLACEMENT_3D('',#44909,#30588,#30589);
#28315=AXIS2_PLACEMENT_3D('',#44929,#30591,#30592);
#28316=AXIS2_PLACEMENT_3D('',#44997,#30593,#30594);
#28317=AXIS2_PLACEMENT_3D('',#45148,#30596,#30597);
#28318=AXIS2_PLACEMENT_3D('',#45481,#30599,#30600);
#28319=AXIS2_PLACEMENT_3D('',#45762,#30602,#30603);
#28320=AXIS2_PLACEMENT_3D('',#46098,#30605,#30606);
#28321=AXIS2_PLACEMENT_3D('',#46260,#30608,#30609);
#28322=AXIS2_PLACEMENT_3D('',#46530,#30611,#30612);
#28323=AXIS2_PLACEMENT_3D('',#46805,#30614,#30615);
#28324=AXIS2_PLACEMENT_3D('',#47139,#30617,#30618);
#28325=AXIS2_PLACEMENT_3D('',#47301,#30620,#30621);
#28326=AXIS2_PLACEMENT_3D('',#47568,#30623,#30624);
#28327=AXIS2_PLACEMENT_3D('',#47846,#30626,#30627);
#28328=AXIS2_PLACEMENT_3D('',#48179,#30629,#30630);
#28329=AXIS2_PLACEMENT_3D('',#48344,#30632,#30633);
#28330=AXIS2_PLACEMENT_3D('',#48613,#30635,#30636);
#28331=AXIS2_PLACEMENT_3D('',#48894,#30638,#30639);
#28332=AXIS2_PLACEMENT_3D('',#49227,#30641,#30642);
#28333=AXIS2_PLACEMENT_3D('',#49386,#30644,#30645);
#28334=AXIS2_PLACEMENT_3D('',#49656,#30647,#30648);
#28335=AXIS2_PLACEMENT_3D('',#49937,#30650,#30651);
#28336=AXIS2_PLACEMENT_3D('',#50268,#30653,#30654);
#28337=AXIS2_PLACEMENT_3D('',#50431,#30656,#30657);
#28338=AXIS2_PLACEMENT_3D('',#50697,#30659,#30660);
#28339=AXIS2_PLACEMENT_3D('',#50978,#30662,#30663);
#28340=AXIS2_PLACEMENT_3D('',#51311,#30665,#30666);
#28341=AXIS2_PLACEMENT_3D('',#51592,#30668,#30669);
#28342=AXIS2_PLACEMENT_3D('',#51610,#30671,#30672);
#28343=AXIS2_PLACEMENT_3D('',#51677,#30673,#30674);
#28344=AXIS2_PLACEMENT_3D('',#51697,#30676,#30677);
#28345=AXIS2_PLACEMENT_3D('',#51765,#30678,#30679);
#28346=AXIS2_PLACEMENT_3D('',#51916,#30681,#30682);
#28347=AXIS2_PLACEMENT_3D('',#52249,#30684,#30685);
#28348=AXIS2_PLACEMENT_3D('',#52530,#30687,#30688);
#28349=AXIS2_PLACEMENT_3D('',#52866,#30690,#30691);
#28350=AXIS2_PLACEMENT_3D('',#53028,#30693,#30694);
#28351=AXIS2_PLACEMENT_3D('',#53298,#30696,#30697);
#28352=AXIS2_PLACEMENT_3D('',#53573,#30699,#30700);
#28353=AXIS2_PLACEMENT_3D('',#53907,#30702,#30703);
#28354=AXIS2_PLACEMENT_3D('',#54069,#30705,#30706);
#28355=AXIS2_PLACEMENT_3D('',#54336,#30708,#30709);
#28356=AXIS2_PLACEMENT_3D('',#54614,#30711,#30712);
#28357=AXIS2_PLACEMENT_3D('',#54947,#30714,#30715);
#28358=AXIS2_PLACEMENT_3D('',#55112,#30717,#30718);
#28359=AXIS2_PLACEMENT_3D('',#55381,#30720,#30721);
#28360=AXIS2_PLACEMENT_3D('',#55662,#30723,#30724);
#28361=AXIS2_PLACEMENT_3D('',#55995,#30726,#30727);
#28362=AXIS2_PLACEMENT_3D('',#56154,#30729,#30730);
#28363=AXIS2_PLACEMENT_3D('',#56424,#30732,#30733);
#28364=AXIS2_PLACEMENT_3D('',#56705,#30735,#30736);
#28365=AXIS2_PLACEMENT_3D('',#57036,#30738,#30739);
#28366=AXIS2_PLACEMENT_3D('',#57199,#30741,#30742);
#28367=AXIS2_PLACEMENT_3D('',#57465,#30744,#30745);
#28368=AXIS2_PLACEMENT_3D('',#57746,#30747,#30748);
#28369=AXIS2_PLACEMENT_3D('',#58079,#30750,#30751);
#28370=AXIS2_PLACEMENT_3D('',#58360,#30753,#30754);
#28371=AXIS2_PLACEMENT_3D('',#58378,#30756,#30757);
#28372=AXIS2_PLACEMENT_3D('',#58445,#30758,#30759);
#28373=AXIS2_PLACEMENT_3D('',#58465,#30761,#30762);
#28374=AXIS2_PLACEMENT_3D('',#58533,#30763,#30764);
#28375=AXIS2_PLACEMENT_3D('',#58684,#30766,#30767);
#28376=AXIS2_PLACEMENT_3D('',#59017,#30769,#30770);
#28377=AXIS2_PLACEMENT_3D('',#59298,#30772,#30773);
#28378=AXIS2_PLACEMENT_3D('',#59634,#30775,#30776);
#28379=AXIS2_PLACEMENT_3D('',#59796,#30778,#30779);
#28380=AXIS2_PLACEMENT_3D('',#60066,#30781,#30782);
#28381=AXIS2_PLACEMENT_3D('',#60341,#30784,#30785);
#28382=AXIS2_PLACEMENT_3D('',#60675,#30787,#30788);
#28383=AXIS2_PLACEMENT_3D('',#60837,#30790,#30791);
#28384=AXIS2_PLACEMENT_3D('',#61104,#30793,#30794);
#28385=AXIS2_PLACEMENT_3D('',#61382,#30796,#30797);
#28386=AXIS2_PLACEMENT_3D('',#61715,#30799,#30800);
#28387=AXIS2_PLACEMENT_3D('',#61880,#30802,#30803);
#28388=AXIS2_PLACEMENT_3D('',#62149,#30805,#30806);
#28389=AXIS2_PLACEMENT_3D('',#62430,#30808,#30809);
#28390=AXIS2_PLACEMENT_3D('',#62763,#30811,#30812);
#28391=AXIS2_PLACEMENT_3D('',#62922,#30814,#30815);
#28392=AXIS2_PLACEMENT_3D('',#63192,#30817,#30818);
#28393=AXIS2_PLACEMENT_3D('',#63473,#30820,#30821);
#28394=AXIS2_PLACEMENT_3D('',#63804,#30823,#30824);
#28395=AXIS2_PLACEMENT_3D('',#63967,#30826,#30827);
#28396=AXIS2_PLACEMENT_3D('',#64233,#30829,#30830);
#28397=AXIS2_PLACEMENT_3D('',#64514,#30832,#30833);
#28398=AXIS2_PLACEMENT_3D('',#64847,#30835,#30836);
#28399=AXIS2_PLACEMENT_3D('',#65128,#30838,#30839);
#28400=AXIS2_PLACEMENT_3D('',#65146,#30841,#30842);
#28401=AXIS2_PLACEMENT_3D('',#65213,#30843,#30844);
#28402=AXIS2_PLACEMENT_3D('',#65257,#30846,#30847);
#28403=AXIS2_PLACEMENT_3D('',#65290,#30848,#30849);
#28404=AXIS2_PLACEMENT_3D('',#65590,#30851,#30852);
#28405=AXIS2_PLACEMENT_3D('',#66043,#30854,#30855);
#28406=AXIS2_PLACEMENT_3D('',#66048,#30857,#30858);
#28407=AXIS2_PLACEMENT_3D('',#66063,#30859,#30860);
#28408=AXIS2_PLACEMENT_3D('',#66068,#30862,#30863);
#28409=AXIS2_PLACEMENT_3D('',#66083,#30864,#30865);
#28410=AXIS2_PLACEMENT_3D('',#66302,#30867,#30868);
#28411=AXIS2_PLACEMENT_3D('',#66357,#30869,#30870);
#28412=AXIS2_PLACEMENT_3D('',#66810,#30872,#30873);
#28413=AXIS2_PLACEMENT_3D('',#66854,#30875,#30876);
#28414=AXIS2_PLACEMENT_3D('',#66887,#30877,#30878);
#28415=AXIS2_PLACEMENT_3D('',#67038,#30880,#30881);
#28416=AXIS2_PLACEMENT_3D('',#67217,#30882,#30883);
#28417=AXIS2_PLACEMENT_3D('',#67687,#30885,#30886);
#28418=AXIS2_PLACEMENT_3D('',#68143,#30888,#30889);
#28419=AXIS2_PLACEMENT_3D('',#68401,#30891,#30892);
#28420=AXIS2_PLACEMENT_3D('',#68848,#30894,#30895);
#28421=AXIS2_PLACEMENT_3D('',#69358,#30897,#30898);
#28422=AXIS2_PLACEMENT_3D('',#69864,#30900,#30901);
#28423=AXIS2_PLACEMENT_3D('',#70340,#30903,#30904);
#28424=AXIS2_PLACEMENT_3D('',#70824,#30906,#30907);
#28425=AXIS2_PLACEMENT_3D('',#71116,#30909,#30910);
#28426=AXIS2_PLACEMENT_3D('',#71552,#30912,#30913);
#28427=AXIS2_PLACEMENT_3D('',#71963,#30915,#30916);
#28428=AXIS2_PLACEMENT_3D('',#72233,#30918,#30919);
#28429=AXIS2_PLACEMENT_3D('',#72743,#30921,#30922);
#28430=AXIS2_PLACEMENT_3D('',#73246,#30924,#30925);
#28431=AXIS2_PLACEMENT_3D('',#73510,#30927,#30928);
#28432=AXIS2_PLACEMENT_3D('',#73944,#30930,#30931);
#28433=AXIS2_PLACEMENT_3D('',#74367,#30933,#30934);
#28434=AXIS2_PLACEMENT_3D('',#74661,#30936,#30937);
#28435=AXIS2_PLACEMENT_3D('',#75135,#30939,#30940);
#28436=AXIS2_PLACEMENT_3D('',#75621,#30942,#30943);
#28437=AXIS2_PLACEMENT_3D('',#76121,#30945,#30946);
#28438=AXIS2_PLACEMENT_3D('',#76635,#30948,#30949);
#28439=AXIS2_PLACEMENT_3D('',#77055,#30951,#30952);
#28440=AXIS2_PLACEMENT_3D('',#77313,#30954,#30955);
#28441=AXIS2_PLACEMENT_3D('',#77775,#30957,#30958);
#28442=AXIS2_PLACEMENT_3D('',#77887,#30960,#30961);
#28443=AXIS2_PLACEMENT_3D('',#78048,#30962,#30963);
#28444=AXIS2_PLACEMENT_3D('',#78199,#30965,#30966);
#28445=AXIS2_PLACEMENT_3D('',#78378,#30967,#30968);
#28446=AXIS2_PLACEMENT_3D('',#78842,#30970,#30971);
#28447=AXIS2_PLACEMENT_3D('',#79300,#30973,#30974);
#28448=AXIS2_PLACEMENT_3D('',#79556,#30976,#30977);
#28449=AXIS2_PLACEMENT_3D('',#80001,#30979,#30980);
#28450=AXIS2_PLACEMENT_3D('',#80511,#30982,#30983);
#28451=AXIS2_PLACEMENT_3D('',#81015,#30985,#30986);
#28452=AXIS2_PLACEMENT_3D('',#81525,#30988,#30989);
#28453=AXIS2_PLACEMENT_3D('',#81999,#30991,#30992);
#28454=AXIS2_PLACEMENT_3D('',#82291,#30994,#30995);
#28455=AXIS2_PLACEMENT_3D('',#82723,#30997,#30998);
#28456=AXIS2_PLACEMENT_3D('',#83134,#31000,#31001);
#28457=AXIS2_PLACEMENT_3D('',#83408,#31003,#31004);
#28458=AXIS2_PLACEMENT_3D('',#83900,#31006,#31007);
#28459=AXIS2_PLACEMENT_3D('',#84401,#31009,#31010);
#28460=AXIS2_PLACEMENT_3D('',#84657,#31012,#31013);
#28461=AXIS2_PLACEMENT_3D('',#85089,#31015,#31016);
#28462=AXIS2_PLACEMENT_3D('',#85512,#31018,#31019);
#28463=AXIS2_PLACEMENT_3D('',#85808,#31021,#31022);
#28464=AXIS2_PLACEMENT_3D('',#86286,#31024,#31025);
#28465=AXIS2_PLACEMENT_3D('',#86816,#31027,#31028);
#28466=AXIS2_PLACEMENT_3D('',#87312,#31030,#31031);
#28467=AXIS2_PLACEMENT_3D('',#87846,#31033,#31034);
#28468=AXIS2_PLACEMENT_3D('',#88266,#31036,#31037);
#28469=AXIS2_PLACEMENT_3D('',#88526,#31039,#31040);
#28470=AXIS2_PLACEMENT_3D('',#88992,#31042,#31043);
#28471=AXIS2_PLACEMENT_3D('',#89104,#31045,#31046);
#28472=AXIS2_PLACEMENT_3D('',#89265,#31047,#31048);
#28473=AXIS2_PLACEMENT_3D('',#89416,#31050,#31051);
#28474=AXIS2_PLACEMENT_3D('',#89595,#31052,#31053);
#28475=AXIS2_PLACEMENT_3D('',#90057,#31055,#31056);
#28476=AXIS2_PLACEMENT_3D('',#90513,#31058,#31059);
#28477=AXIS2_PLACEMENT_3D('',#90763,#31061,#31062);
#28478=AXIS2_PLACEMENT_3D('',#91208,#31064,#31065);
#28479=AXIS2_PLACEMENT_3D('',#91730,#31067,#31068);
#28480=AXIS2_PLACEMENT_3D('',#92234,#31070,#31071);
#28481=AXIS2_PLACEMENT_3D('',#92700,#31073,#31074);
#28482=AXIS2_PLACEMENT_3D('',#93174,#31076,#31077);
#28483=AXIS2_PLACEMENT_3D('',#93466,#31079,#31080);
#28484=AXIS2_PLACEMENT_3D('',#93898,#31082,#31083);
#28485=AXIS2_PLACEMENT_3D('',#94309,#31085,#31086);
#28486=AXIS2_PLACEMENT_3D('',#94577,#31088,#31089);
#28487=AXIS2_PLACEMENT_3D('',#95071,#31091,#31092);
#28488=AXIS2_PLACEMENT_3D('',#95572,#31094,#31095);
#28489=AXIS2_PLACEMENT_3D('',#95836,#31097,#31098);
#28490=AXIS2_PLACEMENT_3D('',#96270,#31100,#31101);
#28491=AXIS2_PLACEMENT_3D('',#96691,#31103,#31104);
#28492=AXIS2_PLACEMENT_3D('',#96985,#31106,#31107);
#28493=AXIS2_PLACEMENT_3D('',#97463,#31109,#31110);
#28494=AXIS2_PLACEMENT_3D('',#97949,#31112,#31113);
#28495=AXIS2_PLACEMENT_3D('',#98445,#31115,#31116);
#28496=AXIS2_PLACEMENT_3D('',#98959,#31118,#31119);
#28497=AXIS2_PLACEMENT_3D('',#99379,#31121,#31122);
#28498=AXIS2_PLACEMENT_3D('',#99641,#31124,#31125);
#28499=AXIS2_PLACEMENT_3D('',#100103,#31127,#31128);
#28500=AXIS2_PLACEMENT_3D('',#100215,#31130,#31131);
#28501=AXIS2_PLACEMENT_3D('',#100376,#31132,#31133);
#28502=AXIS2_PLACEMENT_3D('',#100527,#31135,#31136);
#28503=AXIS2_PLACEMENT_3D('',#100706,#31137,#31138);
#28504=AXIS2_PLACEMENT_3D('',#101176,#31140,#31141);
#28505=AXIS2_PLACEMENT_3D('',#101634,#31143,#31144);
#28506=AXIS2_PLACEMENT_3D('',#101888,#31146,#31147);
#28507=AXIS2_PLACEMENT_3D('',#102333,#31149,#31150);
#28508=AXIS2_PLACEMENT_3D('',#102841,#31152,#31153);
#28509=AXIS2_PLACEMENT_3D('',#103345,#31155,#31156);
#28510=AXIS2_PLACEMENT_3D('',#103867,#31158,#31159);
#28511=AXIS2_PLACEMENT_3D('',#104351,#31161,#31162);
#28512=AXIS2_PLACEMENT_3D('',#104645,#31164,#31165);
#28513=AXIS2_PLACEMENT_3D('',#105081,#31167,#31168);
#28514=AXIS2_PLACEMENT_3D('',#105492,#31170,#31171);
#28515=AXIS2_PLACEMENT_3D('',#105756,#31173,#31174);
#28516=AXIS2_PLACEMENT_3D('',#106248,#31176,#31177);
#28517=AXIS2_PLACEMENT_3D('',#106801,#31179,#31180);
#28518=AXIS2_PLACEMENT_3D('',#107061,#31182,#31183);
#28519=AXIS2_PLACEMENT_3D('',#107493,#31185,#31186);
#28520=AXIS2_PLACEMENT_3D('',#107916,#31188,#31189);
#28521=AXIS2_PLACEMENT_3D('',#108212,#31191,#31192);
#28522=AXIS2_PLACEMENT_3D('',#108686,#31194,#31195);
#28523=AXIS2_PLACEMENT_3D('',#109164,#31197,#31198);
#28524=AXIS2_PLACEMENT_3D('',#109660,#31200,#31201);
#28525=AXIS2_PLACEMENT_3D('',#110184,#31203,#31204);
#28526=AXIS2_PLACEMENT_3D('',#110604,#31206,#31207);
#28527=AXIS2_PLACEMENT_3D('',#110864,#31209,#31210);
#28528=AXIS2_PLACEMENT_3D('',#111326,#31212,#31213);
#28529=AXIS2_PLACEMENT_3D('',#111438,#31215,#31216);
#28530=AXIS2_PLACEMENT_3D('',#111599,#31217,#31218);
#28531=AXIS2_PLACEMENT_3D('',#112074,#31219,#31220);
#28532=AXIS2_PLACEMENT_3D('',#112551,#31221,#31222);
#28533=AXIS2_PLACEMENT_3D('',#113028,#31223,#31224);
#28534=AXIS2_PLACEMENT_3D('',#113495,#31225,#31226);
#28535=AXIS2_PLACEMENT_3D('',#113790,#31227,#31228);
#28536=AXIS2_PLACEMENT_3D('',#114060,#31229,#31230);
#28537=AXIS2_PLACEMENT_3D('',#114061,#31231,#31232);
#28538=AXIS2_PLACEMENT_3D('',#114156,#31233,#31234);
#28539=AXIS2_PLACEMENT_3D('',#114251,#31235,#31236);
#28540=AXIS2_PLACEMENT_3D('',#114346,#31237,#31238);
#28541=AXIS2_PLACEMENT_3D('',#114441,#31239,#31240);
#28542=AXIS2_PLACEMENT_3D('',#114777,#31241,#31242);
#28543=AXIS2_PLACEMENT_3D('',#115113,#31243,#31244);
#28544=AXIS2_PLACEMENT_3D('',#115115,#31245,#31246);
#28545=AXIS2_PLACEMENT_3D('',#115118,#31248,#31249);
#28546=AXIS2_PLACEMENT_3D('',#115119,#31250,#31251);
#28547=AXIS2_PLACEMENT_3D('',#115120,#31252,#31253);
#28548=AXIS2_PLACEMENT_3D('',#115123,#31254,#31255);
#28549=AXIS2_PLACEMENT_3D('',#115127,#31257,#31258);
#28550=AXIS2_PLACEMENT_3D('',#115129,#31260,#31261);
#28551=AXIS2_PLACEMENT_3D('',#115136,#31265,#31266);
#28552=AXIS2_PLACEMENT_3D('',#115137,#31267,#31268);
#28553=AXIS2_PLACEMENT_3D('',#115139,#31269,#31270);
#28554=AXIS2_PLACEMENT_3D('',#115142,#31272,#31273);
#28555=AXIS2_PLACEMENT_3D('',#115143,#31274,#31275);
#28556=AXIS2_PLACEMENT_3D('',#115144,#31276,#31277);
#28557=AXIS2_PLACEMENT_3D('',#115147,#31278,#31279);
#28558=AXIS2_PLACEMENT_3D('',#115151,#31281,#31282);
#28559=AXIS2_PLACEMENT_3D('',#115153,#31284,#31285);
#28560=AXIS2_PLACEMENT_3D('',#115160,#31289,#31290);
#28561=AXIS2_PLACEMENT_3D('',#115161,#31291,#31292);
#28562=AXIS2_PLACEMENT_3D('',#115163,#31293,#31294);
#28563=AXIS2_PLACEMENT_3D('',#115166,#31296,#31297);
#28564=AXIS2_PLACEMENT_3D('',#115167,#31298,#31299);
#28565=AXIS2_PLACEMENT_3D('',#115168,#31300,#31301);
#28566=AXIS2_PLACEMENT_3D('',#115174,#31305,#31306);
#28567=AXIS2_PLACEMENT_3D('',#115182,#31311,#31312);
#28568=AXIS2_PLACEMENT_3D('',#115187,#31316,#31317);
#28569=AXIS2_PLACEMENT_3D('',#115191,#31319,#31320);
#28570=AXIS2_PLACEMENT_3D('',#115195,#31322,#31323);
#28571=AXIS2_PLACEMENT_3D('',#115199,#31325,#31326);
#28572=AXIS2_PLACEMENT_3D('',#115203,#31328,#31329);
#28573=AXIS2_PLACEMENT_3D('',#115215,#31335,#31336);
#28574=AXIS2_PLACEMENT_3D('',#115219,#31338,#31339);
#28575=AXIS2_PLACEMENT_3D('',#115231,#31345,#31346);
#28576=AXIS2_PLACEMENT_3D('',#115235,#31348,#31349);
#28577=AXIS2_PLACEMENT_3D('',#115239,#31351,#31352);
#28578=AXIS2_PLACEMENT_3D('',#115242,#31354,#31355);
#28579=AXIS2_PLACEMENT_3D('',#115244,#31356,#31357);
#28580=AXIS2_PLACEMENT_3D('',#115246,#31358,#31359);
#28581=AXIS2_PLACEMENT_3D('',#124042,#31360,#31361);
#28582=AXIS2_PLACEMENT_3D('',#124051,#31366,#31367);
#28583=AXIS2_PLACEMENT_3D('',#124057,#31371,#31372);
#28584=AXIS2_PLACEMENT_3D('',#124063,#31376,#31377);
#28585=AXIS2_PLACEMENT_3D('',#124069,#31381,#31382);
#28586=AXIS2_PLACEMENT_3D('',#124075,#31386,#31387);
#28587=AXIS2_PLACEMENT_3D('',#124081,#31391,#31392);
#28588=AXIS2_PLACEMENT_3D('',#124084,#31395,#31396);
#28589=AXIS2_PLACEMENT_3D('',#124086,#31397,#31398);
#28590=AXIS2_PLACEMENT_3D('',#124089,#31400,#31401);
#28591=AXIS2_PLACEMENT_3D('',#124090,#31402,#31403);
#28592=AXIS2_PLACEMENT_3D('',#124091,#31404,#31405);
#28593=AXIS2_PLACEMENT_3D('',#124094,#31406,#31407);
#28594=AXIS2_PLACEMENT_3D('',#124098,#31409,#31410);
#28595=AXIS2_PLACEMENT_3D('',#124100,#31412,#31413);
#28596=AXIS2_PLACEMENT_3D('',#124106,#31417,#31418);
#28597=AXIS2_PLACEMENT_3D('',#124108,#31419,#31420);
#28598=AXIS2_PLACEMENT_3D('',#124110,#31421,#31422);
#28599=AXIS2_PLACEMENT_3D('',#124112,#31424,#31425);
#28600=AXIS2_PLACEMENT_3D('',#124115,#31428,#31429);
#28601=AXIS2_PLACEMENT_3D('',#124118,#31432,#31433);
#28602=AXIS2_PLACEMENT_3D('',#124120,#31434,#31435);
#28603=AXIS2_PLACEMENT_3D('',#124122,#31436,#31437);
#28604=AXIS2_PLACEMENT_3D('',#124123,#31438,#31439);
#28605=AXIS2_PLACEMENT_3D('',#124132,#31444,#31445);
#28606=AXIS2_PLACEMENT_3D('',#124138,#31449,#31450);
#28607=AXIS2_PLACEMENT_3D('',#124144,#31454,#31455);
#28608=AXIS2_PLACEMENT_3D('',#124150,#31459,#31460);
#28609=AXIS2_PLACEMENT_3D('',#124156,#31464,#31465);
#28610=AXIS2_PLACEMENT_3D('',#124162,#31469,#31470);
#28611=AXIS2_PLACEMENT_3D('',#124165,#31473,#31474);
#28612=AXIS2_PLACEMENT_3D('',#124167,#31475,#31476);
#28613=AXIS2_PLACEMENT_3D('',#124170,#31478,#31479);
#28614=AXIS2_PLACEMENT_3D('',#124171,#31480,#31481);
#28615=AXIS2_PLACEMENT_3D('',#124172,#31482,#31483);
#28616=AXIS2_PLACEMENT_3D('',#124173,#31484,#31485);
#28617=AXIS2_PLACEMENT_3D('',#124174,#31486,#31487);
#28618=AXIS2_PLACEMENT_3D('',#124176,#31488,#31489);
#28619=AXIS2_PLACEMENT_3D('',#124178,#31491,#31492);
#28620=AXIS2_PLACEMENT_3D('',#124179,#31493,#31494);
#28621=AXIS2_PLACEMENT_3D('',#124180,#31495,#31496);
#28622=AXIS2_PLACEMENT_3D('',#124182,#31497,#31498);
#28623=AXIS2_PLACEMENT_3D('',#124184,#31500,#31501);
#28624=AXIS2_PLACEMENT_3D('',#124185,#31502,#31503);
#28625=AXIS2_PLACEMENT_3D('',#124188,#31504,#31505);
#28626=AXIS2_PLACEMENT_3D('',#124192,#31507,#31508);
#28627=AXIS2_PLACEMENT_3D('',#124194,#31510,#31511);
#28628=AXIS2_PLACEMENT_3D('',#124200,#31515,#31516);
#28629=AXIS2_PLACEMENT_3D('',#124202,#31517,#31518);
#28630=AXIS2_PLACEMENT_3D('',#124205,#31520,#31521);
#28631=AXIS2_PLACEMENT_3D('',#124206,#31522,#31523);
#28632=AXIS2_PLACEMENT_3D('',#124209,#31526,#31527);
#28633=AXIS2_PLACEMENT_3D('',#124212,#31530,#31531);
#28634=AXIS2_PLACEMENT_3D('',#124214,#31532,#31533);
#28635=AXIS2_PLACEMENT_3D('',#124216,#31534,#31535);
#28636=AXIS2_PLACEMENT_3D('',#124217,#31536,#31537);
#28637=AXIS2_PLACEMENT_3D('',#124226,#31542,#31543);
#28638=AXIS2_PLACEMENT_3D('',#124232,#31547,#31548);
#28639=AXIS2_PLACEMENT_3D('',#124238,#31552,#31553);
#28640=AXIS2_PLACEMENT_3D('',#124244,#31557,#31558);
#28641=AXIS2_PLACEMENT_3D('',#124250,#31562,#31563);
#28642=AXIS2_PLACEMENT_3D('',#124256,#31567,#31568);
#28643=AXIS2_PLACEMENT_3D('',#124259,#31571,#31572);
#28644=AXIS2_PLACEMENT_3D('',#124261,#31573,#31574);
#28645=AXIS2_PLACEMENT_3D('',#124264,#31576,#31577);
#28646=AXIS2_PLACEMENT_3D('',#124265,#31578,#31579);
#28647=AXIS2_PLACEMENT_3D('',#124266,#31580,#31581);
#28648=AXIS2_PLACEMENT_3D('',#124275,#31586,#31587);
#28649=AXIS2_PLACEMENT_3D('',#124281,#31591,#31592);
#28650=AXIS2_PLACEMENT_3D('',#124287,#31596,#31597);
#28651=AXIS2_PLACEMENT_3D('',#124293,#31601,#31602);
#28652=AXIS2_PLACEMENT_3D('',#124299,#31606,#31607);
#28653=AXIS2_PLACEMENT_3D('',#124305,#31611,#31612);
#28654=AXIS2_PLACEMENT_3D('',#124308,#31615,#31616);
#28655=AXIS2_PLACEMENT_3D('',#124310,#31617,#31618);
#28656=AXIS2_PLACEMENT_3D('',#124313,#31620,#31621);
#28657=AXIS2_PLACEMENT_3D('',#124314,#31622,#31623);
#28658=AXIS2_PLACEMENT_3D('',#124315,#31624,#31625);
#28659=AXIS2_PLACEMENT_3D('',#124316,#31626,#31627);
#28660=AXIS2_PLACEMENT_3D('',#124317,#31628,#31629);
#28661=AXIS2_PLACEMENT_3D('',#124323,#31633,#31634);
#28662=AXIS2_PLACEMENT_3D('',#124324,#31635,#31636);
#28663=AXIS2_PLACEMENT_3D('',#124327,#31638,#31639);
#28664=AXIS2_PLACEMENT_3D('',#124328,#31640,#31641);
#28665=AXIS2_PLACEMENT_3D('',#124329,#31642,#31643);
#28666=AXIS2_PLACEMENT_3D('',#124332,#31645,#31646);
#28667=AXIS2_PLACEMENT_3D('',#124333,#31647,#31648);
#28668=AXIS2_PLACEMENT_3D('',#124334,#31649,#31650);
#28669=AXIS2_PLACEMENT_3D('',#124337,#31652,#31653);
#28670=AXIS2_PLACEMENT_3D('',#124338,#31654,#31655);
#28671=AXIS2_PLACEMENT_3D('',#124339,#31656,#31657);
#28672=AXIS2_PLACEMENT_3D('',#124342,#31659,#31660);
#28673=AXIS2_PLACEMENT_3D('',#124343,#31661,#31662);
#28674=AXIS2_PLACEMENT_3D('',#124344,#31663,#31664);
#28675=AXIS2_PLACEMENT_3D('',#124348,#31667,#31668);
#28676=AXIS2_PLACEMENT_3D('',#124349,#31669,#31670);
#28677=AXIS2_PLACEMENT_3D('',#124350,#31671,#31672);
#28678=AXIS2_PLACEMENT_3D('',#124352,#31673,#31674);
#28679=AXIS2_PLACEMENT_3D('',#124354,#31676,#31677);
#28680=AXIS2_PLACEMENT_3D('',#124358,#31680,#31681);
#28681=AXIS2_PLACEMENT_3D('',#124360,#31682,#31683);
#28682=AXIS2_PLACEMENT_3D('',#124362,#31685,#31686);
#28683=AXIS2_PLACEMENT_3D('',#124366,#31689,#31690);
#28684=AXIS2_PLACEMENT_3D('',#124368,#31691,#31692);
#28685=AXIS2_PLACEMENT_3D('',#124370,#31694,#31695);
#28686=AXIS2_PLACEMENT_3D('',#124374,#31698,#31699);
#28687=AXIS2_PLACEMENT_3D('',#124375,#31700,#31701);
#28688=AXIS2_PLACEMENT_3D('',#124376,#31702,#31703);
#28689=AXIS2_PLACEMENT_3D('',#124378,#31704,#31705);
#28690=AXIS2_PLACEMENT_3D('',#124380,#31707,#31708);
#28691=AXIS2_PLACEMENT_3D('',#124384,#31711,#31712);
#28692=AXIS2_PLACEMENT_3D('',#124386,#31713,#31714);
#28693=AXIS2_PLACEMENT_3D('',#124388,#31716,#31717);
#28694=AXIS2_PLACEMENT_3D('',#124392,#31720,#31721);
#28695=AXIS2_PLACEMENT_3D('',#124394,#31722,#31723);
#28696=AXIS2_PLACEMENT_3D('',#124396,#31725,#31726);
#28697=AXIS2_PLACEMENT_3D('',#124400,#31729,#31730);
#28698=AXIS2_PLACEMENT_3D('',#124402,#31731,#31732);
#28699=AXIS2_PLACEMENT_3D('',#124404,#31734,#31735);
#28700=AXIS2_PLACEMENT_3D('',#124408,#31738,#31739);
#28701=AXIS2_PLACEMENT_3D('',#124410,#31740,#31741);
#28702=AXIS2_PLACEMENT_3D('',#124412,#31743,#31744);
#28703=AXIS2_PLACEMENT_3D('',#124416,#31747,#31748);
#28704=AXIS2_PLACEMENT_3D('',#124418,#31749,#31750);
#28705=AXIS2_PLACEMENT_3D('',#124420,#31752,#31753);
#28706=AXIS2_PLACEMENT_3D('',#124424,#31756,#31757);
#28707=AXIS2_PLACEMENT_3D('',#124425,#31758,#31759);
#28708=AXIS2_PLACEMENT_3D('',#124426,#31760,#31761);
#28709=AXIS2_PLACEMENT_3D('',#124427,#31762,#31763);
#28710=AXIS2_PLACEMENT_3D('',#124428,#31764,#31765);
#28711=AXIS2_PLACEMENT_3D('',#124429,#31766,#31767);
#28712=AXIS2_PLACEMENT_3D('',#124431,#31768,#31769);
#28713=AXIS2_PLACEMENT_3D('',#124434,#31771,#31772);
#28714=AXIS2_PLACEMENT_3D('',#124435,#31773,#31774);
#28715=AXIS2_PLACEMENT_3D('',#124436,#31775,#31776);
#28716=AXIS2_PLACEMENT_3D('',#124438,#31777,#31778);
#28717=AXIS2_PLACEMENT_3D('',#124441,#31780,#31781);
#28718=AXIS2_PLACEMENT_3D('',#124442,#31782,#31783);
#28719=AXIS2_PLACEMENT_3D('',#124443,#31784,#31785);
#28720=AXIS2_PLACEMENT_3D('',#124448,#31787,#31788);
#28721=AXIS2_PLACEMENT_3D('',#124451,#31790,#31791);
#28722=AXIS2_PLACEMENT_3D('',#124452,#31792,#31793);
#28723=AXIS2_PLACEMENT_3D('',#124456,#31795,#31796);
#28724=AXIS2_PLACEMENT_3D('',#124458,#31798,#31799);
#28725=AXIS2_PLACEMENT_3D('',#124461,#31800,#31801);
#28726=AXIS2_PLACEMENT_3D('',#124465,#31803,#31804);
#28727=AXIS2_PLACEMENT_3D('',#124467,#31806,#31807);
#28728=AXIS2_PLACEMENT_3D('',#124470,#31808,#31809);
#28729=AXIS2_PLACEMENT_3D('',#124471,#31810,#31811);
#28730=AXIS2_PLACEMENT_3D('',#124472,#31812,#31813);
#28731=AXIS2_PLACEMENT_3D('',#124473,#31814,#31815);
#28732=AXIS2_PLACEMENT_3D('',#124476,#31816,#31817);
#28733=AXIS2_PLACEMENT_3D('',#124479,#31820,#31821);
#28734=AXIS2_PLACEMENT_3D('',#124482,#31822,#31823);
#28735=AXIS2_PLACEMENT_3D('',#124483,#31824,#31825);
#28736=AXIS2_PLACEMENT_3D('',#124484,#31826,#31827);
#28737=AXIS2_PLACEMENT_3D('',#124485,#31828,#31829);
#28738=AXIS2_PLACEMENT_3D('',#124488,#31830,#31831);
#28739=AXIS2_PLACEMENT_3D('',#124491,#31834,#31835);
#28740=AXIS2_PLACEMENT_3D('',#124494,#31836,#31837);
#28741=AXIS2_PLACEMENT_3D('',#124495,#31838,#31839);
#28742=AXIS2_PLACEMENT_3D('',#124496,#31840,#31841);
#28743=AXIS2_PLACEMENT_3D('',#124497,#31842,#31843);
#28744=AXIS2_PLACEMENT_3D('',#124500,#31844,#31845);
#28745=AXIS2_PLACEMENT_3D('',#124514,#31848,#31849);
#28746=AXIS2_PLACEMENT_3D('',#124515,#31850,#31851);
#28747=AXIS2_PLACEMENT_3D('',#124516,#31852,#31853);
#28748=AXIS2_PLACEMENT_3D('',#124517,#31854,#31855);
#28749=AXIS2_PLACEMENT_3D('',#124522,#31858,#31859);
#28750=AXIS2_PLACEMENT_3D('',#124523,#31860,#31861);
#28751=AXIS2_PLACEMENT_3D('',#124528,#31864,#31865);
#28752=AXIS2_PLACEMENT_3D('',#124529,#31866,#31867);
#28753=AXIS2_PLACEMENT_3D('',#124533,#31869,#31870);
#28754=AXIS2_PLACEMENT_3D('',#124535,#31872,#31873);
#28755=AXIS2_PLACEMENT_3D('',#124538,#31874,#31875);
#28756=AXIS2_PLACEMENT_3D('',#124539,#31876,#31877);
#28757=AXIS2_PLACEMENT_3D('',#124540,#31878,#31879);
#28758=AXIS2_PLACEMENT_3D('',#124541,#31880,#31881);
#28759=AXIS2_PLACEMENT_3D('',#124546,#31884,#31885);
#28760=AXIS2_PLACEMENT_3D('',#124547,#31886,#31887);
#28761=AXIS2_PLACEMENT_3D('',#124550,#31890,#31891);
#28762=AXIS2_PLACEMENT_3D('',#124554,#31893,#31894);
#28763=AXIS2_PLACEMENT_3D('',#124556,#31896,#31897);
#28764=AXIS2_PLACEMENT_3D('',#124559,#31898,#31899);
#28765=AXIS2_PLACEMENT_3D('',#124560,#31900,#31901);
#28766=AXIS2_PLACEMENT_3D('',#124561,#31902,#31903);
#28767=AXIS2_PLACEMENT_3D('',#124562,#31904,#31905);
#28768=AXIS2_PLACEMENT_3D('',#124567,#31908,#31909);
#28769=AXIS2_PLACEMENT_3D('',#124568,#31910,#31911);
#28770=AXIS2_PLACEMENT_3D('',#124572,#31913,#31914);
#28771=AXIS2_PLACEMENT_3D('',#124574,#31916,#31917);
#28772=AXIS2_PLACEMENT_3D('',#124578,#31919,#31920);
#28773=AXIS2_PLACEMENT_3D('',#124591,#31922,#31923);
#28774=AXIS2_PLACEMENT_3D('',#124592,#31924,#31925);
#28775=AXIS2_PLACEMENT_3D('',#124593,#31926,#31927);
#28776=AXIS2_PLACEMENT_3D('',#124594,#31928,#31929);
#28777=AXIS2_PLACEMENT_3D('',#124597,#31930,#31931);
#28778=AXIS2_PLACEMENT_3D('',#124600,#31934,#31935);
#28779=AXIS2_PLACEMENT_3D('',#124603,#31936,#31937);
#28780=AXIS2_PLACEMENT_3D('',#124604,#31938,#31939);
#28781=AXIS2_PLACEMENT_3D('',#124605,#31940,#31941);
#28782=AXIS2_PLACEMENT_3D('',#124606,#31942,#31943);
#28783=AXIS2_PLACEMENT_3D('',#124609,#31944,#31945);
#28784=AXIS2_PLACEMENT_3D('',#124612,#31948,#31949);
#28785=AXIS2_PLACEMENT_3D('',#124615,#31950,#31951);
#28786=AXIS2_PLACEMENT_3D('',#124616,#31952,#31953);
#28787=AXIS2_PLACEMENT_3D('',#124617,#31954,#31955);
#28788=AXIS2_PLACEMENT_3D('',#124618,#31956,#31957);
#28789=AXIS2_PLACEMENT_3D('',#124621,#31958,#31959);
#28790=AXIS2_PLACEMENT_3D('',#124624,#31962,#31963);
#28791=AXIS2_PLACEMENT_3D('',#124627,#31964,#31965);
#28792=AXIS2_PLACEMENT_3D('',#124628,#31966,#31967);
#28793=AXIS2_PLACEMENT_3D('',#124629,#31968,#31969);
#28794=AXIS2_PLACEMENT_3D('',#124630,#31970,#31971);
#28795=AXIS2_PLACEMENT_3D('',#124633,#31972,#31973);
#28796=AXIS2_PLACEMENT_3D('',#124636,#31976,#31977);
#28797=AXIS2_PLACEMENT_3D('',#124639,#31978,#31979);
#28798=AXIS2_PLACEMENT_3D('',#124642,#31981,#31982);
#28799=AXIS2_PLACEMENT_3D('',#124644,#31984,#31985);
#28800=AXIS2_PLACEMENT_3D('',#124648,#31987,#31988);
#28801=AXIS2_PLACEMENT_3D('',#124650,#31990,#31991);
#28802=AXIS2_PLACEMENT_3D('',#124653,#31993,#31994);
#28803=AXIS2_PLACEMENT_3D('',#124655,#31996,#31997);
#28804=AXIS2_PLACEMENT_3D('',#124656,#31998,#31999);
#28805=AXIS2_PLACEMENT_3D('',#124657,#32000,#32001);
#28806=AXIS2_PLACEMENT_3D('',#124658,#32002,#32003);
#28807=AXIS2_PLACEMENT_3D('',#124659,#32004,#32005);
#28808=AXIS2_PLACEMENT_3D('',#124665,#32009,#32010);
#28809=AXIS2_PLACEMENT_3D('',#124668,#32012,#32013);
#28810=AXIS2_PLACEMENT_3D('',#124669,#32014,#32015);
#28811=AXIS2_PLACEMENT_3D('',#124673,#32018,#32019);
#28812=AXIS2_PLACEMENT_3D('',#124677,#32022,#32023);
#28813=AXIS2_PLACEMENT_3D('',#124681,#32026,#32027);
#28814=AXIS2_PLACEMENT_3D('',#124684,#32029,#32030);
#28815=AXIS2_PLACEMENT_3D('',#124685,#32031,#32032);
#28816=AXIS2_PLACEMENT_3D('',#124689,#32035,#32036);
#28817=AXIS2_PLACEMENT_3D('',#124692,#32038,#32039);
#28818=AXIS2_PLACEMENT_3D('',#124693,#32040,#32041);
#28819=AXIS2_PLACEMENT_3D('',#124697,#32044,#32045);
#28820=AXIS2_PLACEMENT_3D('',#124701,#32047,#32048);
#28821=AXIS2_PLACEMENT_3D('',#124704,#32050,#32051);
#28822=AXIS2_PLACEMENT_3D('',#124705,#32052,#32053);
#28823=AXIS2_PLACEMENT_3D('',#124709,#32056,#32057);
#28824=AXIS2_PLACEMENT_3D('',#124712,#32059,#32060);
#28825=AXIS2_PLACEMENT_3D('',#124713,#32061,#32062);
#28826=AXIS2_PLACEMENT_3D('',#124721,#32067,#32068);
#28827=AXIS2_PLACEMENT_3D('',#124724,#32070,#32071);
#28828=AXIS2_PLACEMENT_3D('',#124725,#32072,#32073);
#28829=AXIS2_PLACEMENT_3D('',#124729,#32076,#32077);
#28830=AXIS2_PLACEMENT_3D('',#124733,#32080,#32081);
#28831=AXIS2_PLACEMENT_3D('',#124737,#32084,#32085);
#28832=AXIS2_PLACEMENT_3D('',#124738,#32086,#32087);
#28833=AXIS2_PLACEMENT_3D('',#124740,#32088,#32089);
#28834=AXIS2_PLACEMENT_3D('',#124757,#32091,#32092);
#28835=AXIS2_PLACEMENT_3D('',#124759,#32093,#32094);
#28836=AXIS2_PLACEMENT_3D('',#124781,#32095,#32096);
#28837=AXIS2_PLACEMENT_3D('',#124782,#32097,#32098);
#28838=AXIS2_PLACEMENT_3D('',#124784,#32099,#32100);
#28839=AXIS2_PLACEMENT_3D('',#124786,#32102,#32103);
#28840=AXIS2_PLACEMENT_3D('',#124787,#32104,#32105);
#28841=AXIS2_PLACEMENT_3D('',#124789,#32106,#32107);
#28842=AXIS2_PLACEMENT_3D('',#124791,#32109,#32110);
#28843=AXIS2_PLACEMENT_3D('',#124793,#32111,#32112);
#28844=AXIS2_PLACEMENT_3D('',#124795,#32114,#32115);
#28845=AXIS2_PLACEMENT_3D('',#124796,#32116,#32117);
#28846=AXIS2_PLACEMENT_3D('',#124799,#32118,#32119);
#28847=AXIS2_PLACEMENT_3D('',#124823,#32120,#32121);
#28848=AXIS2_PLACEMENT_3D('',#124838,#32122,#32123);
#28849=AXIS2_PLACEMENT_3D('',#124841,#32125,#32126);
#28850=AXIS2_PLACEMENT_3D('',#124843,#32128,#32129);
#28851=AXIS2_PLACEMENT_3D('',#124844,#32130,#32131);
#28852=AXIS2_PLACEMENT_3D('',#124845,#32132,#32133);
#28853=AXIS2_PLACEMENT_3D('',#124848,#32135,#32136);
#28854=AXIS2_PLACEMENT_3D('',#124849,#32137,#32138);
#28855=AXIS2_PLACEMENT_3D('',#124850,#32139,#32140);
#28856=AXIS2_PLACEMENT_3D('',#124854,#32142,#32143);
#28857=AXIS2_PLACEMENT_3D('',#124858,#32145,#32146);
#28858=AXIS2_PLACEMENT_3D('',#124866,#32150,#32151);
#28859=AXIS2_PLACEMENT_3D('',#124878,#32157,#32158);
#28860=AXIS2_PLACEMENT_3D('',#124886,#32162,#32163);
#28861=AXIS2_PLACEMENT_3D('',#124889,#32165,#32166);
#28862=AXIS2_PLACEMENT_3D('',#124890,#32167,#32168);
#28863=AXIS2_PLACEMENT_3D('',#124892,#32169,#32170);
#28864=AXIS2_PLACEMENT_3D('',#124895,#32172,#32173);
#28865=AXIS2_PLACEMENT_3D('',#124896,#32174,#32175);
#28866=AXIS2_PLACEMENT_3D('',#124897,#32176,#32177);
#28867=AXIS2_PLACEMENT_3D('',#124898,#32178,#32179);
#28868=AXIS2_PLACEMENT_3D('',#124899,#32180,#32181);
#28869=AXIS2_PLACEMENT_3D('',#124900,#32182,#32183);
#28870=AXIS2_PLACEMENT_3D('',#124910,#32184,#32185);
#28871=AXIS2_PLACEMENT_3D('',#124911,#32186,#32187);
#28872=AXIS2_PLACEMENT_3D('',#124912,#32188,#32189);
#28873=AXIS2_PLACEMENT_3D('',#124913,#32190,#32191);
#28874=AXIS2_PLACEMENT_3D('',#124914,#32192,#32193);
#28875=AXIS2_PLACEMENT_3D('',#124915,#32194,#32195);
#28876=AXIS2_PLACEMENT_3D('',#124916,#32196,#32197);
#28877=AXIS2_PLACEMENT_3D('',#124917,#32198,#32199);
#28878=AXIS2_PLACEMENT_3D('',#124918,#32200,#32201);
#28879=AXIS2_PLACEMENT_3D('',#124919,#32202,#32203);
#28880=AXIS2_PLACEMENT_3D('',#124920,#32204,#32205);
#28881=AXIS2_PLACEMENT_3D('',#124921,#32206,#32207);
#28882=AXIS2_PLACEMENT_3D('',#124922,#32208,#32209);
#28883=AXIS2_PLACEMENT_3D('',#124923,#32210,#32211);
#28884=AXIS2_PLACEMENT_3D('',#124927,#32213,#32214);
#28885=AXIS2_PLACEMENT_3D('',#124928,#32215,#32216);
#28886=AXIS2_PLACEMENT_3D('',#124929,#32217,#32218);
#28887=AXIS2_PLACEMENT_3D('',#124931,#32219,#32220);
#28888=AXIS2_PLACEMENT_3D('',#124933,#32222,#32223);
#28889=AXIS2_PLACEMENT_3D('',#124935,#32225,#32226);
#28890=AXIS2_PLACEMENT_3D('',#124939,#32228,#32229);
#28891=AXIS2_PLACEMENT_3D('',#124940,#32230,#32231);
#28892=AXIS2_PLACEMENT_3D('',#124941,#32232,#32233);
#28893=AXIS2_PLACEMENT_3D('',#124943,#32234,#32235);
#28894=AXIS2_PLACEMENT_3D('',#124944,#32236,#32237);
#28895=AXIS2_PLACEMENT_3D('',#124945,#32238,#32239);
#28896=AXIS2_PLACEMENT_3D('',#124947,#32241,#32242);
#28897=AXIS2_PLACEMENT_3D('',#124950,#32244,#32245);
#28898=AXIS2_PLACEMENT_3D('',#124951,#32246,#32247);
#28899=AXIS2_PLACEMENT_3D('',#124953,#32248,#32249);
#28900=AXIS2_PLACEMENT_3D('',#124954,#32250,#32251);
#28901=AXIS2_PLACEMENT_3D('',#124955,#32252,#32253);
#28902=AXIS2_PLACEMENT_3D('',#124957,#32254,#32255);
#28903=AXIS2_PLACEMENT_3D('',#124969,#32257,#32258);
#28904=AXIS2_PLACEMENT_3D('',#124970,#32259,#32260);
#28905=AXIS2_PLACEMENT_3D('',#124971,#32261,#32262);
#28906=AXIS2_PLACEMENT_3D('',#124973,#32264,#32265);
#28907=AXIS2_PLACEMENT_3D('',#124975,#32267,#32268);
#28908=AXIS2_PLACEMENT_3D('',#124977,#32270,#32271);
#28909=AXIS2_PLACEMENT_3D('',#124979,#32273,#32274);
#28910=AXIS2_PLACEMENT_3D('',#124981,#32276,#32277);
#28911=AXIS2_PLACEMENT_3D('',#124983,#32279,#32280);
#28912=AXIS2_PLACEMENT_3D('',#124985,#32282,#32283);
#28913=AXIS2_PLACEMENT_3D('',#124987,#32285,#32286);
#28914=AXIS2_PLACEMENT_3D('',#124989,#32288,#32289);
#28915=AXIS2_PLACEMENT_3D('',#124991,#32291,#32292);
#28916=AXIS2_PLACEMENT_3D('',#124993,#32294,#32295);
#28917=AXIS2_PLACEMENT_3D('',#124995,#32297,#32298);
#28918=AXIS2_PLACEMENT_3D('',#124997,#32300,#32301);
#28919=AXIS2_PLACEMENT_3D('',#125001,#32303,#32304);
#28920=AXIS2_PLACEMENT_3D('',#125003,#32306,#32307);
#28921=AXIS2_PLACEMENT_3D('',#125006,#32309,#32310);
#28922=AXIS2_PLACEMENT_3D('',#125007,#32311,#32312);
#28923=AXIS2_PLACEMENT_3D('',#125008,#32313,#32314);
#28924=AXIS2_PLACEMENT_3D('',#125009,#32315,#32316);
#28925=AXIS2_PLACEMENT_3D('',#125010,#32317,#32318);
#28926=AXIS2_PLACEMENT_3D('',#125015,#32321,#32322);
#28927=AXIS2_PLACEMENT_3D('',#125016,#32323,#32324);
#28928=AXIS2_PLACEMENT_3D('',#125018,#32326,#32327);
#28929=AXIS2_PLACEMENT_3D('',#125020,#32329,#32330);
#28930=AXIS2_PLACEMENT_3D('',#125022,#32332,#32333);
#28931=AXIS2_PLACEMENT_3D('',#125023,#32334,#32335);
#28932=AXIS2_PLACEMENT_3D('',#125024,#32336,#32337);
#28933=AXIS2_PLACEMENT_3D('',#125026,#32338,#32339);
#28934=AXIS2_PLACEMENT_3D('',#125029,#32341,#32342);
#28935=AXIS2_PLACEMENT_3D('',#125030,#32343,#32344);
#28936=AXIS2_PLACEMENT_3D('',#125031,#32345,#32346);
#28937=AXIS2_PLACEMENT_3D('',#125033,#32347,#32348);
#28938=AXIS2_PLACEMENT_3D('',#125036,#32350,#32351);
#28939=AXIS2_PLACEMENT_3D('',#125037,#32352,#32353);
#28940=AXIS2_PLACEMENT_3D('',#125038,#32354,#32355);
#28941=AXIS2_PLACEMENT_3D('',#125043,#32357,#32358);
#28942=AXIS2_PLACEMENT_3D('',#125046,#32360,#32361);
#28943=AXIS2_PLACEMENT_3D('',#125047,#32362,#32363);
#28944=AXIS2_PLACEMENT_3D('',#125051,#32365,#32366);
#28945=AXIS2_PLACEMENT_3D('',#125053,#32368,#32369);
#28946=AXIS2_PLACEMENT_3D('',#125056,#32370,#32371);
#28947=AXIS2_PLACEMENT_3D('',#125060,#32373,#32374);
#28948=AXIS2_PLACEMENT_3D('',#125062,#32376,#32377);
#28949=AXIS2_PLACEMENT_3D('',#125065,#32378,#32379);
#28950=AXIS2_PLACEMENT_3D('',#125066,#32380,#32381);
#28951=AXIS2_PLACEMENT_3D('',#125067,#32382,#32383);
#28952=AXIS2_PLACEMENT_3D('',#125068,#32384,#32385);
#28953=AXIS2_PLACEMENT_3D('',#125071,#32386,#32387);
#28954=AXIS2_PLACEMENT_3D('',#125074,#32390,#32391);
#28955=AXIS2_PLACEMENT_3D('',#125077,#32392,#32393);
#28956=AXIS2_PLACEMENT_3D('',#125078,#32394,#32395);
#28957=AXIS2_PLACEMENT_3D('',#125079,#32396,#32397);
#28958=AXIS2_PLACEMENT_3D('',#125080,#32398,#32399);
#28959=AXIS2_PLACEMENT_3D('',#125083,#32400,#32401);
#28960=AXIS2_PLACEMENT_3D('',#125086,#32404,#32405);
#28961=AXIS2_PLACEMENT_3D('',#125089,#32406,#32407);
#28962=AXIS2_PLACEMENT_3D('',#125090,#32408,#32409);
#28963=AXIS2_PLACEMENT_3D('',#125091,#32410,#32411);
#28964=AXIS2_PLACEMENT_3D('',#125092,#32412,#32413);
#28965=AXIS2_PLACEMENT_3D('',#125095,#32414,#32415);
#28966=AXIS2_PLACEMENT_3D('',#125109,#32418,#32419);
#28967=AXIS2_PLACEMENT_3D('',#125110,#32420,#32421);
#28968=AXIS2_PLACEMENT_3D('',#125111,#32422,#32423);
#28969=AXIS2_PLACEMENT_3D('',#125112,#32424,#32425);
#28970=AXIS2_PLACEMENT_3D('',#125116,#32427,#32428);
#28971=AXIS2_PLACEMENT_3D('',#125118,#32430,#32431);
#28972=AXIS2_PLACEMENT_3D('',#125122,#32433,#32434);
#28973=AXIS2_PLACEMENT_3D('',#125124,#32436,#32437);
#28974=AXIS2_PLACEMENT_3D('',#125129,#32440,#32441);
#28975=AXIS2_PLACEMENT_3D('',#125130,#32442,#32443);
#28976=AXIS2_PLACEMENT_3D('',#125133,#32444,#32445);
#28977=AXIS2_PLACEMENT_3D('',#125134,#32446,#32447);
#28978=AXIS2_PLACEMENT_3D('',#125135,#32448,#32449);
#28979=AXIS2_PLACEMENT_3D('',#125136,#32450,#32451);
#28980=AXIS2_PLACEMENT_3D('',#125140,#32453,#32454);
#28981=AXIS2_PLACEMENT_3D('',#125142,#32456,#32457);
#28982=AXIS2_PLACEMENT_3D('',#125145,#32460,#32461);
#28983=AXIS2_PLACEMENT_3D('',#125150,#32464,#32465);
#28984=AXIS2_PLACEMENT_3D('',#125151,#32466,#32467);
#28985=AXIS2_PLACEMENT_3D('',#125154,#32468,#32469);
#28986=AXIS2_PLACEMENT_3D('',#125155,#32470,#32471);
#28987=AXIS2_PLACEMENT_3D('',#125156,#32472,#32473);
#28988=AXIS2_PLACEMENT_3D('',#125157,#32474,#32475);
#28989=AXIS2_PLACEMENT_3D('',#125161,#32477,#32478);
#28990=AXIS2_PLACEMENT_3D('',#125163,#32480,#32481);
#28991=AXIS2_PLACEMENT_3D('',#125168,#32484,#32485);
#28992=AXIS2_PLACEMENT_3D('',#125169,#32486,#32487);
#28993=AXIS2_PLACEMENT_3D('',#125174,#32490,#32491);
#28994=AXIS2_PLACEMENT_3D('',#125186,#32492,#32493);
#28995=AXIS2_PLACEMENT_3D('',#125187,#32494,#32495);
#28996=AXIS2_PLACEMENT_3D('',#125188,#32496,#32497);
#28997=AXIS2_PLACEMENT_3D('',#125189,#32498,#32499);
#28998=AXIS2_PLACEMENT_3D('',#125192,#32500,#32501);
#28999=AXIS2_PLACEMENT_3D('',#125195,#32504,#32505);
#29000=AXIS2_PLACEMENT_3D('',#125198,#32506,#32507);
#29001=AXIS2_PLACEMENT_3D('',#125199,#32508,#32509);
#29002=AXIS2_PLACEMENT_3D('',#125200,#32510,#32511);
#29003=AXIS2_PLACEMENT_3D('',#125201,#32512,#32513);
#29004=AXIS2_PLACEMENT_3D('',#125204,#32514,#32515);
#29005=AXIS2_PLACEMENT_3D('',#125207,#32518,#32519);
#29006=AXIS2_PLACEMENT_3D('',#125210,#32520,#32521);
#29007=AXIS2_PLACEMENT_3D('',#125211,#32522,#32523);
#29008=AXIS2_PLACEMENT_3D('',#125212,#32524,#32525);
#29009=AXIS2_PLACEMENT_3D('',#125213,#32526,#32527);
#29010=AXIS2_PLACEMENT_3D('',#125216,#32528,#32529);
#29011=AXIS2_PLACEMENT_3D('',#125219,#32532,#32533);
#29012=AXIS2_PLACEMENT_3D('',#125222,#32534,#32535);
#29013=AXIS2_PLACEMENT_3D('',#125223,#32536,#32537);
#29014=AXIS2_PLACEMENT_3D('',#125224,#32538,#32539);
#29015=AXIS2_PLACEMENT_3D('',#125225,#32540,#32541);
#29016=AXIS2_PLACEMENT_3D('',#125228,#32542,#32543);
#29017=AXIS2_PLACEMENT_3D('',#125231,#32546,#32547);
#29018=AXIS2_PLACEMENT_3D('',#125234,#32548,#32549);
#29019=AXIS2_PLACEMENT_3D('',#125237,#32551,#32552);
#29020=AXIS2_PLACEMENT_3D('',#125239,#32554,#32555);
#29021=AXIS2_PLACEMENT_3D('',#125243,#32557,#32558);
#29022=AXIS2_PLACEMENT_3D('',#125245,#32560,#32561);
#29023=AXIS2_PLACEMENT_3D('',#125248,#32563,#32564);
#29024=AXIS2_PLACEMENT_3D('',#125250,#32566,#32567);
#29025=AXIS2_PLACEMENT_3D('',#125251,#32568,#32569);
#29026=AXIS2_PLACEMENT_3D('',#125252,#32570,#32571);
#29027=AXIS2_PLACEMENT_3D('',#125253,#32572,#32573);
#29028=AXIS2_PLACEMENT_3D('',#125254,#32574,#32575);
#29029=AXIS2_PLACEMENT_3D('',#125260,#32579,#32580);
#29030=AXIS2_PLACEMENT_3D('',#125262,#32581,#32582);
#29031=AXIS2_PLACEMENT_3D('',#125264,#32584,#32585);
#29032=AXIS2_PLACEMENT_3D('',#125268,#32588,#32589);
#29033=AXIS2_PLACEMENT_3D('',#125272,#32592,#32593);
#29034=AXIS2_PLACEMENT_3D('',#125276,#32596,#32597);
#29035=AXIS2_PLACEMENT_3D('',#125278,#32598,#32599);
#29036=AXIS2_PLACEMENT_3D('',#125280,#32601,#32602);
#29037=AXIS2_PLACEMENT_3D('',#125284,#32605,#32606);
#29038=AXIS2_PLACEMENT_3D('',#125286,#32607,#32608);
#29039=AXIS2_PLACEMENT_3D('',#125288,#32610,#32611);
#29040=AXIS2_PLACEMENT_3D('',#125292,#32614,#32615);
#29041=AXIS2_PLACEMENT_3D('',#125294,#32616,#32617);
#29042=AXIS2_PLACEMENT_3D('',#125298,#32619,#32620);
#29043=AXIS2_PLACEMENT_3D('',#125300,#32622,#32623);
#29044=AXIS2_PLACEMENT_3D('',#125304,#32626,#32627);
#29045=AXIS2_PLACEMENT_3D('',#125306,#32628,#32629);
#29046=AXIS2_PLACEMENT_3D('',#125308,#32631,#32632);
#29047=AXIS2_PLACEMENT_3D('',#125316,#32637,#32638);
#29048=AXIS2_PLACEMENT_3D('',#125318,#32639,#32640);
#29049=AXIS2_PLACEMENT_3D('',#125320,#32642,#32643);
#29050=AXIS2_PLACEMENT_3D('',#125324,#32646,#32647);
#29051=AXIS2_PLACEMENT_3D('',#125328,#32650,#32651);
#29052=AXIS2_PLACEMENT_3D('',#125332,#32654,#32655);
#29053=AXIS2_PLACEMENT_3D('',#125333,#32656,#32657);
#29054=AXIS2_PLACEMENT_3D('',#125351,#32659,#32660);
#29055=AXIS2_PLACEMENT_3D('',#125352,#32661,#32662);
#29056=AXIS2_PLACEMENT_3D('',#125354,#32663,#32664);
#29057=AXIS2_PLACEMENT_3D('',#125355,#32665,#32666);
#29058=AXIS2_PLACEMENT_3D('',#125377,#32667,#32668);
#29059=AXIS2_PLACEMENT_3D('',#125379,#32669,#32670);
#29060=AXIS2_PLACEMENT_3D('',#125380,#32671,#32672);
#29061=AXIS2_PLACEMENT_3D('',#125382,#32674,#32675);
#29062=AXIS2_PLACEMENT_3D('',#125384,#32676,#32677);
#29063=AXIS2_PLACEMENT_3D('',#125386,#32679,#32680);
#29064=AXIS2_PLACEMENT_3D('',#125389,#32682,#32683);
#29065=AXIS2_PLACEMENT_3D('',#125390,#32684,#32685);
#29066=AXIS2_PLACEMENT_3D('',#125391,#32686,#32687);
#29067=AXIS2_PLACEMENT_3D('',#125394,#32688,#32689);
#29068=AXIS2_PLACEMENT_3D('',#125411,#32690,#32691);
#29069=AXIS2_PLACEMENT_3D('',#125433,#32692,#32693);
#29070=AXIS2_PLACEMENT_3D('',#125437,#32696,#32697);
#29071=AXIS2_PLACEMENT_3D('',#125438,#32698,#32699);
#29072=AXIS2_PLACEMENT_3D('',#125439,#32700,#32701);
#29073=AXIS2_PLACEMENT_3D('',#125440,#32702,#32703);
#29074=AXIS2_PLACEMENT_3D('',#125441,#32704,#32705);
#29075=AXIS2_PLACEMENT_3D('',#125443,#32706,#32707);
#29076=AXIS2_PLACEMENT_3D('',#125445,#32709,#32710);
#29077=AXIS2_PLACEMENT_3D('',#125447,#32711,#32712);
#29078=AXIS2_PLACEMENT_3D('',#125451,#32714,#32715);
#29079=AXIS2_PLACEMENT_3D('',#125459,#32719,#32720);
#29080=AXIS2_PLACEMENT_3D('',#125471,#32726,#32727);
#29081=AXIS2_PLACEMENT_3D('',#125479,#32731,#32732);
#29082=AXIS2_PLACEMENT_3D('',#125483,#32734,#32735);
#29083=AXIS2_PLACEMENT_3D('',#125485,#32737,#32738);
#29084=AXIS2_PLACEMENT_3D('',#125487,#32739,#32740);
#29085=AXIS2_PLACEMENT_3D('',#125490,#32742,#32743);
#29086=AXIS2_PLACEMENT_3D('',#125491,#32744,#32745);
#29087=AXIS2_PLACEMENT_3D('',#125492,#32746,#32747);
#29088=AXIS2_PLACEMENT_3D('',#125493,#32748,#32749);
#29089=AXIS2_PLACEMENT_3D('',#125494,#32750,#32751);
#29090=AXIS2_PLACEMENT_3D('',#125495,#32752,#32753);
#29091=AXIS2_PLACEMENT_3D('',#125505,#32754,#32755);
#29092=AXIS2_PLACEMENT_3D('',#125506,#32756,#32757);
#29093=AXIS2_PLACEMENT_3D('',#125507,#32758,#32759);
#29094=AXIS2_PLACEMENT_3D('',#125508,#32760,#32761);
#29095=AXIS2_PLACEMENT_3D('',#125509,#32762,#32763);
#29096=AXIS2_PLACEMENT_3D('',#125510,#32764,#32765);
#29097=AXIS2_PLACEMENT_3D('',#125511,#32766,#32767);
#29098=AXIS2_PLACEMENT_3D('',#125512,#32768,#32769);
#29099=AXIS2_PLACEMENT_3D('',#125513,#32770,#32771);
#29100=AXIS2_PLACEMENT_3D('',#125514,#32772,#32773);
#29101=AXIS2_PLACEMENT_3D('',#125515,#32774,#32775);
#29102=AXIS2_PLACEMENT_3D('',#125516,#32776,#32777);
#29103=AXIS2_PLACEMENT_3D('',#125517,#32778,#32779);
#29104=AXIS2_PLACEMENT_3D('',#125518,#32780,#32781);
#29105=AXIS2_PLACEMENT_3D('',#125522,#32783,#32784);
#29106=AXIS2_PLACEMENT_3D('',#125523,#32785,#32786);
#29107=AXIS2_PLACEMENT_3D('',#125524,#32787,#32788);
#29108=AXIS2_PLACEMENT_3D('',#125526,#32789,#32790);
#29109=AXIS2_PLACEMENT_3D('',#125528,#32792,#32793);
#29110=AXIS2_PLACEMENT_3D('',#125530,#32795,#32796);
#29111=AXIS2_PLACEMENT_3D('',#125534,#32798,#32799);
#29112=AXIS2_PLACEMENT_3D('',#125535,#32800,#32801);
#29113=AXIS2_PLACEMENT_3D('',#125536,#32802,#32803);
#29114=AXIS2_PLACEMENT_3D('',#125538,#32804,#32805);
#29115=AXIS2_PLACEMENT_3D('',#125539,#32806,#32807);
#29116=AXIS2_PLACEMENT_3D('',#125540,#32808,#32809);
#29117=AXIS2_PLACEMENT_3D('',#125542,#32811,#32812);
#29118=AXIS2_PLACEMENT_3D('',#125545,#32814,#32815);
#29119=AXIS2_PLACEMENT_3D('',#125546,#32816,#32817);
#29120=AXIS2_PLACEMENT_3D('',#125548,#32818,#32819);
#29121=AXIS2_PLACEMENT_3D('',#125549,#32820,#32821);
#29122=AXIS2_PLACEMENT_3D('',#125550,#32822,#32823);
#29123=AXIS2_PLACEMENT_3D('',#125552,#32824,#32825);
#29124=AXIS2_PLACEMENT_3D('',#125564,#32827,#32828);
#29125=AXIS2_PLACEMENT_3D('',#125565,#32829,#32830);
#29126=AXIS2_PLACEMENT_3D('',#125566,#32831,#32832);
#29127=AXIS2_PLACEMENT_3D('',#125568,#32834,#32835);
#29128=AXIS2_PLACEMENT_3D('',#125570,#32837,#32838);
#29129=AXIS2_PLACEMENT_3D('',#125572,#32840,#32841);
#29130=AXIS2_PLACEMENT_3D('',#125574,#32843,#32844);
#29131=AXIS2_PLACEMENT_3D('',#125576,#32846,#32847);
#29132=AXIS2_PLACEMENT_3D('',#125578,#32849,#32850);
#29133=AXIS2_PLACEMENT_3D('',#125580,#32852,#32853);
#29134=AXIS2_PLACEMENT_3D('',#125582,#32855,#32856);
#29135=AXIS2_PLACEMENT_3D('',#125584,#32858,#32859);
#29136=AXIS2_PLACEMENT_3D('',#125586,#32861,#32862);
#29137=AXIS2_PLACEMENT_3D('',#125588,#32864,#32865);
#29138=AXIS2_PLACEMENT_3D('',#125590,#32867,#32868);
#29139=AXIS2_PLACEMENT_3D('',#125592,#32870,#32871);
#29140=AXIS2_PLACEMENT_3D('',#125596,#32873,#32874);
#29141=AXIS2_PLACEMENT_3D('',#125598,#32876,#32877);
#29142=AXIS2_PLACEMENT_3D('',#125600,#32878,#32879);
#29143=AXIS2_PLACEMENT_3D('',#125602,#32881,#32882);
#29144=AXIS2_PLACEMENT_3D('',#125603,#32883,#32884);
#29145=AXIS2_PLACEMENT_3D('',#125604,#32885,#32886);
#29146=AXIS2_PLACEMENT_3D('',#125605,#32887,#32888);
#29147=AXIS2_PLACEMENT_3D('',#125609,#32890,#32891);
#29148=AXIS2_PLACEMENT_3D('',#125611,#32893,#32894);
#29149=AXIS2_PLACEMENT_3D('',#125613,#32896,#32897);
#29150=AXIS2_PLACEMENT_3D('',#125615,#32899,#32900);
#29151=AXIS2_PLACEMENT_3D('',#125617,#32902,#32903);
#29152=AXIS2_PLACEMENT_3D('',#125618,#32904,#32905);
#29153=AXIS2_PLACEMENT_3D('',#125621,#32906,#32907);
#29154=AXIS2_PLACEMENT_3D('',#125622,#32908,#32909);
#29155=AXIS2_PLACEMENT_3D('',#125625,#32911,#32912);
#29156=AXIS2_PLACEMENT_3D('',#125626,#32913,#32914);
#29157=AXIS2_PLACEMENT_3D('',#125627,#32915,#32916);
#29158=AXIS2_PLACEMENT_3D('',#125630,#32917,#32918);
#29159=AXIS2_PLACEMENT_3D('',#125631,#32919,#32920);
#29160=AXIS2_PLACEMENT_3D('',#125634,#32922,#32923);
#29161=AXIS2_PLACEMENT_3D('',#125635,#32924,#32925);
#29162=AXIS2_PLACEMENT_3D('',#125636,#32926,#32927);
#29163=AXIS2_PLACEMENT_3D('',#125647,#32934,#32935);
#29164=AXIS2_PLACEMENT_3D('',#125651,#32937,#32938);
#29165=AXIS2_PLACEMENT_3D('',#125652,#32939,#32940);
#29166=AXIS2_PLACEMENT_3D('',#125654,#32941,#32942);
#29167=AXIS2_PLACEMENT_3D('',#125663,#32944,#32945);
#29168=AXIS2_PLACEMENT_3D('',#125718,#32948,#32949);
#29169=AXIS2_PLACEMENT_3D('',#125727,#32950,#32951);
#29170=AXIS2_PLACEMENT_3D('',#125745,#32953,#32954);
#29171=AXIS2_PLACEMENT_3D('',#125812,#32957,#32958);
#29172=AXIS2_PLACEMENT_3D('',#125816,#32960,#32961);
#29173=AXIS2_PLACEMENT_3D('',#125883,#32964,#32965);
#29174=AXIS2_PLACEMENT_3D('',#125903,#32967,#32968);
#29175=AXIS2_PLACEMENT_3D('',#125916,#32969,#32970);
#29176=AXIS2_PLACEMENT_3D('',#125984,#32973,#32974);
#29177=AXIS2_PLACEMENT_3D('',#125994,#32976,#32977);
#29178=AXIS2_PLACEMENT_3D('',#125995,#32978,#32979);
#29179=AXIS2_PLACEMENT_3D('',#126006,#32980,#32981);
#29180=AXIS2_PLACEMENT_3D('',#126026,#32983,#32984);
#29181=AXIS2_PLACEMENT_3D('',#126028,#32985,#32986);
#29182=AXIS2_PLACEMENT_3D('',#126046,#32988,#32989);
#29183=AXIS2_PLACEMENT_3D('',#126053,#32990,#32991);
#29184=AXIS2_PLACEMENT_3D('',#126057,#32993,#32994);
#29185=AXIS2_PLACEMENT_3D('',#126058,#32995,#32996);
#29186=AXIS2_PLACEMENT_3D('',#126060,#32997,#32998);
#29187=AXIS2_PLACEMENT_3D('',#126069,#33000,#33001);
#29188=AXIS2_PLACEMENT_3D('',#126124,#33004,#33005);
#29189=AXIS2_PLACEMENT_3D('',#126133,#33006,#33007);
#29190=AXIS2_PLACEMENT_3D('',#126151,#33009,#33010);
#29191=AXIS2_PLACEMENT_3D('',#126218,#33013,#33014);
#29192=AXIS2_PLACEMENT_3D('',#126222,#33016,#33017);
#29193=AXIS2_PLACEMENT_3D('',#126289,#33020,#33021);
#29194=AXIS2_PLACEMENT_3D('',#126309,#33023,#33024);
#29195=AXIS2_PLACEMENT_3D('',#126322,#33025,#33026);
#29196=AXIS2_PLACEMENT_3D('',#126390,#33029,#33030);
#29197=AXIS2_PLACEMENT_3D('',#126400,#33032,#33033);
#29198=AXIS2_PLACEMENT_3D('',#126401,#33034,#33035);
#29199=AXIS2_PLACEMENT_3D('',#126412,#33036,#33037);
#29200=AXIS2_PLACEMENT_3D('',#126432,#33039,#33040);
#29201=AXIS2_PLACEMENT_3D('',#126434,#33041,#33042);
#29202=AXIS2_PLACEMENT_3D('',#126452,#33044,#33045);
#29203=AXIS2_PLACEMENT_3D('',#126459,#33046,#33047);
#29204=AXIS2_PLACEMENT_3D('',#126463,#33049,#33050);
#29205=AXIS2_PLACEMENT_3D('',#126464,#33051,#33052);
#29206=AXIS2_PLACEMENT_3D('',#126466,#33053,#33054);
#29207=AXIS2_PLACEMENT_3D('',#126475,#33056,#33057);
#29208=AXIS2_PLACEMENT_3D('',#126534,#33060,#33061);
#29209=AXIS2_PLACEMENT_3D('',#126543,#33062,#33063);
#29210=AXIS2_PLACEMENT_3D('',#126561,#33065,#33066);
#29211=AXIS2_PLACEMENT_3D('',#126628,#33069,#33070);
#29212=AXIS2_PLACEMENT_3D('',#126632,#33072,#33073);
#29213=AXIS2_PLACEMENT_3D('',#126699,#33076,#33077);
#29214=AXIS2_PLACEMENT_3D('',#126719,#33079,#33080);
#29215=AXIS2_PLACEMENT_3D('',#126732,#33081,#33082);
#29216=AXIS2_PLACEMENT_3D('',#126800,#33085,#33086);
#29217=AXIS2_PLACEMENT_3D('',#126810,#33088,#33089);
#29218=AXIS2_PLACEMENT_3D('',#126811,#33090,#33091);
#29219=AXIS2_PLACEMENT_3D('',#126822,#33092,#33093);
#29220=AXIS2_PLACEMENT_3D('',#126842,#33095,#33096);
#29221=AXIS2_PLACEMENT_3D('',#126844,#33097,#33098);
#29222=AXIS2_PLACEMENT_3D('',#126862,#33100,#33101);
#29223=AXIS2_PLACEMENT_3D('',#126869,#33102,#33103);
#29224=AXIS2_PLACEMENT_3D('',#126873,#33105,#33106);
#29225=AXIS2_PLACEMENT_3D('',#126877,#33108,#33109);
#29226=AXIS2_PLACEMENT_3D('',#126881,#33113,#33114);
#29227=AXIS2_PLACEMENT_3D('',#126885,#33117,#33118);
#29228=AXIS2_PLACEMENT_3D('',#126889,#33121,#33122);
#29229=AXIS2_PLACEMENT_3D('',#126891,#33124,#33125);
#29230=AXIS2_PLACEMENT_3D('',#126894,#33127,#33128);
#29231=AXIS2_PLACEMENT_3D('',#126895,#33129,#33130);
#29232=AXIS2_PLACEMENT_3D('',#126897,#33131,#33132);
#29233=AXIS2_PLACEMENT_3D('',#126899,#33134,#33135);
#29234=AXIS2_PLACEMENT_3D('',#126901,#33137,#33138);
#29235=AXIS2_PLACEMENT_3D('',#126905,#33141,#33142);
#29236=AXIS2_PLACEMENT_3D('',#126909,#33145,#33146);
#29237=AXIS2_PLACEMENT_3D('',#126911,#33148,#33149);
#29238=AXIS2_PLACEMENT_3D('',#126914,#33151,#33152);
#29239=AXIS2_PLACEMENT_3D('',#126915,#33153,#33154);
#29240=AXIS2_PLACEMENT_3D('',#126917,#33155,#33156);
#29241=AXIS2_PLACEMENT_3D('',#126919,#33158,#33159);
#29242=AXIS2_PLACEMENT_3D('',#126921,#33161,#33162);
#29243=AXIS2_PLACEMENT_3D('',#126925,#33165,#33166);
#29244=AXIS2_PLACEMENT_3D('',#126929,#33169,#33170);
#29245=AXIS2_PLACEMENT_3D('',#126931,#33172,#33173);
#29246=AXIS2_PLACEMENT_3D('',#126934,#33175,#33176);
#29247=AXIS2_PLACEMENT_3D('',#126935,#33177,#33178);
#29248=AXIS2_PLACEMENT_3D('',#126937,#33179,#33180);
#29249=AXIS2_PLACEMENT_3D('',#126939,#33182,#33183);
#29250=AXIS2_PLACEMENT_3D('',#126941,#33185,#33186);
#29251=AXIS2_PLACEMENT_3D('',#126945,#33189,#33190);
#29252=AXIS2_PLACEMENT_3D('',#126949,#33193,#33194);
#29253=AXIS2_PLACEMENT_3D('',#126951,#33196,#33197);
#29254=AXIS2_PLACEMENT_3D('',#126954,#33199,#33200);
#29255=AXIS2_PLACEMENT_3D('',#126955,#33201,#33202);
#29256=AXIS2_PLACEMENT_3D('',#126957,#33203,#33204);
#29257=AXIS2_PLACEMENT_3D('',#126959,#33206,#33207);
#29258=AXIS2_PLACEMENT_3D('',#126961,#33209,#33210);
#29259=AXIS2_PLACEMENT_3D('',#126965,#33213,#33214);
#29260=AXIS2_PLACEMENT_3D('',#126969,#33217,#33218);
#29261=AXIS2_PLACEMENT_3D('',#126971,#33220,#33221);
#29262=AXIS2_PLACEMENT_3D('',#126974,#33223,#33224);
#29263=AXIS2_PLACEMENT_3D('',#126975,#33225,#33226);
#29264=AXIS2_PLACEMENT_3D('',#126977,#33227,#33228);
#29265=AXIS2_PLACEMENT_3D('',#126979,#33230,#33231);
#29266=AXIS2_PLACEMENT_3D('',#126981,#33233,#33234);
#29267=AXIS2_PLACEMENT_3D('',#126985,#33237,#33238);
#29268=AXIS2_PLACEMENT_3D('',#126989,#33241,#33242);
#29269=AXIS2_PLACEMENT_3D('',#126991,#33244,#33245);
#29270=AXIS2_PLACEMENT_3D('',#126997,#33249,#33250);
#29271=AXIS2_PLACEMENT_3D('',#127001,#33252,#33253);
#29272=AXIS2_PLACEMENT_3D('',#127003,#33255,#33256);
#29273=AXIS2_PLACEMENT_3D('',#127007,#33259,#33260);
#29274=AXIS2_PLACEMENT_3D('',#127009,#33262,#33263);
#29275=AXIS2_PLACEMENT_3D('',#127011,#33265,#33266);
#29276=AXIS2_PLACEMENT_3D('',#127014,#33268,#33269);
#29277=AXIS2_PLACEMENT_3D('',#127015,#33270,#33271);
#29278=AXIS2_PLACEMENT_3D('',#127017,#33273,#33274);
#29279=AXIS2_PLACEMENT_3D('',#127019,#33276,#33277);
#29280=AXIS2_PLACEMENT_3D('',#127023,#33280,#33281);
#29281=AXIS2_PLACEMENT_3D('',#127025,#33283,#33284);
#29282=AXIS2_PLACEMENT_3D('',#127027,#33286,#33287);
#29283=AXIS2_PLACEMENT_3D('',#127030,#33289,#33290);
#29284=AXIS2_PLACEMENT_3D('',#127031,#33291,#33292);
#29285=AXIS2_PLACEMENT_3D('',#127033,#33294,#33295);
#29286=AXIS2_PLACEMENT_3D('',#127035,#33297,#33298);
#29287=AXIS2_PLACEMENT_3D('',#127039,#33301,#33302);
#29288=AXIS2_PLACEMENT_3D('',#127041,#33304,#33305);
#29289=AXIS2_PLACEMENT_3D('',#127043,#33307,#33308);
#29290=AXIS2_PLACEMENT_3D('',#127046,#33310,#33311);
#29291=AXIS2_PLACEMENT_3D('',#127047,#33312,#33313);
#29292=AXIS2_PLACEMENT_3D('',#127049,#33315,#33316);
#29293=AXIS2_PLACEMENT_3D('',#127051,#33318,#33319);
#29294=AXIS2_PLACEMENT_3D('',#127055,#33322,#33323);
#29295=AXIS2_PLACEMENT_3D('',#127057,#33325,#33326);
#29296=AXIS2_PLACEMENT_3D('',#127059,#33328,#33329);
#29297=AXIS2_PLACEMENT_3D('',#127062,#33331,#33332);
#29298=AXIS2_PLACEMENT_3D('',#127063,#33333,#33334);
#29299=AXIS2_PLACEMENT_3D('',#127065,#33336,#33337);
#29300=AXIS2_PLACEMENT_3D('',#127067,#33339,#33340);
#29301=AXIS2_PLACEMENT_3D('',#127071,#33343,#33344);
#29302=AXIS2_PLACEMENT_3D('',#127073,#33346,#33347);
#29303=AXIS2_PLACEMENT_3D('',#127075,#33349,#33350);
#29304=AXIS2_PLACEMENT_3D('',#127078,#33352,#33353);
#29305=AXIS2_PLACEMENT_3D('',#127079,#33354,#33355);
#29306=AXIS2_PLACEMENT_3D('',#127081,#33357,#33358);
#29307=AXIS2_PLACEMENT_3D('',#127083,#33360,#33361);
#29308=AXIS2_PLACEMENT_3D('',#127087,#33364,#33365);
#29309=AXIS2_PLACEMENT_3D('',#127089,#33367,#33368);
#29310=AXIS2_PLACEMENT_3D('',#127091,#33370,#33371);
#29311=AXIS2_PLACEMENT_3D('',#127093,#33372,#33373);
#29312=AXIS2_PLACEMENT_3D('',#127096,#33375,#33376);
#29313=AXIS2_PLACEMENT_3D('',#127097,#33377,#33378);
#29314=AXIS2_PLACEMENT_3D('',#127099,#33379,#33380);
#29315=AXIS2_PLACEMENT_3D('',#127102,#33382,#33383);
#29316=AXIS2_PLACEMENT_3D('',#127103,#33384,#33385);
#29317=AXIS2_PLACEMENT_3D('',#127105,#33386,#33387);
#29318=AXIS2_PLACEMENT_3D('',#127108,#33389,#33390);
#29319=AXIS2_PLACEMENT_3D('',#127109,#33391,#33392);
#29320=AXIS2_PLACEMENT_3D('',#127118,#33397,#33398);
#29321=AXIS2_PLACEMENT_3D('',#127124,#33402,#33403);
#29322=AXIS2_PLACEMENT_3D('',#127126,#33404,#33405);
#29323=AXIS2_PLACEMENT_3D('',#127129,#33407,#33408);
#29324=AXIS2_PLACEMENT_3D('',#127130,#33409,#33410);
#29325=AXIS2_PLACEMENT_3D('',#127136,#33414,#33415);
#29326=AXIS2_PLACEMENT_3D('',#127138,#33417,#33418);
#29327=AXIS2_PLACEMENT_3D('',#127139,#33419,#33420);
#29328=AXIS2_PLACEMENT_3D('',#127140,#33421,#33422);
#29329=AXIS2_PLACEMENT_3D('',#127142,#33424,#33425);
#29330=AXIS2_PLACEMENT_3D('',#127144,#33427,#33428);
#29331=AXIS2_PLACEMENT_3D('',#127146,#33430,#33431);
#29332=AXIS2_PLACEMENT_3D('',#127148,#33433,#33434);
#29333=AXIS2_PLACEMENT_3D('',#127150,#33436,#33437);
#29334=AXIS2_PLACEMENT_3D('',#127152,#33439,#33440);
#29335=AXIS2_PLACEMENT_3D('',#127154,#33442,#33443);
#29336=AXIS2_PLACEMENT_3D('',#127156,#33445,#33446);
#29337=AXIS2_PLACEMENT_3D('',#127158,#33448,#33449);
#29338=AXIS2_PLACEMENT_3D('',#127160,#33451,#33452);
#29339=AXIS2_PLACEMENT_3D('',#127161,#33453,#33454);
#29340=AXIS2_PLACEMENT_3D('',#127167,#33458,#33459);
#29341=AXIS2_PLACEMENT_3D('',#127169,#33460,#33461);
#29342=AXIS2_PLACEMENT_3D('',#127172,#33463,#33464);
#29343=AXIS2_PLACEMENT_3D('',#127173,#33465,#33466);
#29344=AXIS2_PLACEMENT_3D('',#127179,#33470,#33471);
#29345=AXIS2_PLACEMENT_3D('',#127181,#33472,#33473);
#29346=AXIS2_PLACEMENT_3D('',#127184,#33475,#33476);
#29347=AXIS2_PLACEMENT_3D('',#127185,#33477,#33478);
#29348=AXIS2_PLACEMENT_3D('',#127191,#33482,#33483);
#29349=AXIS2_PLACEMENT_3D('',#127193,#33484,#33485);
#29350=AXIS2_PLACEMENT_3D('',#127196,#33487,#33488);
#29351=AXIS2_PLACEMENT_3D('',#127197,#33489,#33490);
#29352=AXIS2_PLACEMENT_3D('',#127203,#33494,#33495);
#29353=AXIS2_PLACEMENT_3D('',#127205,#33496,#33497);
#29354=AXIS2_PLACEMENT_3D('',#127208,#33499,#33500);
#29355=AXIS2_PLACEMENT_3D('',#127209,#33501,#33502);
#29356=AXIS2_PLACEMENT_3D('',#127215,#33506,#33507);
#29357=AXIS2_PLACEMENT_3D('',#127217,#33508,#33509);
#29358=AXIS2_PLACEMENT_3D('',#127220,#33511,#33512);
#29359=AXIS2_PLACEMENT_3D('',#127221,#33513,#33514);
#29360=AXIS2_PLACEMENT_3D('',#127227,#33518,#33519);
#29361=AXIS2_PLACEMENT_3D('',#127229,#33520,#33521);
#29362=AXIS2_PLACEMENT_3D('',#127232,#33523,#33524);
#29363=AXIS2_PLACEMENT_3D('',#127233,#33525,#33526);
#29364=AXIS2_PLACEMENT_3D('',#127239,#33530,#33531);
#29365=AXIS2_PLACEMENT_3D('',#127245,#33535,#33536);
#29366=AXIS2_PLACEMENT_3D('',#127251,#33540,#33541);
#29367=AXIS2_PLACEMENT_3D('',#127253,#33542,#33543);
#29368=AXIS2_PLACEMENT_3D('',#127256,#33545,#33546);
#29369=AXIS2_PLACEMENT_3D('',#127257,#33547,#33548);
#29370=AXIS2_PLACEMENT_3D('',#127263,#33552,#33553);
#29371=AXIS2_PLACEMENT_3D('',#127269,#33557,#33558);
#29372=AXIS2_PLACEMENT_3D('',#127272,#33561,#33562);
#29373=AXIS2_PLACEMENT_3D('',#127278,#33566,#33567);
#29374=AXIS2_PLACEMENT_3D('',#127280,#33568,#33569);
#29375=AXIS2_PLACEMENT_3D('',#127282,#33570,#33571);
#29376=AXIS2_PLACEMENT_3D('',#127284,#33573,#33574);
#29377=AXIS2_PLACEMENT_3D('',#127290,#33578,#33579);
#29378=AXIS2_PLACEMENT_3D('',#127293,#33581,#33582);
#29379=AXIS2_PLACEMENT_3D('',#127294,#33583,#33584);
#29380=AXIS2_PLACEMENT_3D('',#127295,#33585,#33586);
#29381=AXIS2_PLACEMENT_3D('',#127299,#33589,#33590);
#29382=AXIS2_PLACEMENT_3D('',#127302,#33592,#33593);
#29383=AXIS2_PLACEMENT_3D('',#127303,#33594,#33595);
#29384=AXIS2_PLACEMENT_3D('',#127307,#33598,#33599);
#29385=AXIS2_PLACEMENT_3D('',#127310,#33601,#33602);
#29386=AXIS2_PLACEMENT_3D('',#127311,#33603,#33604);
#29387=AXIS2_PLACEMENT_3D('',#127315,#33607,#33608);
#29388=AXIS2_PLACEMENT_3D('',#127318,#33610,#33611);
#29389=AXIS2_PLACEMENT_3D('',#127319,#33612,#33613);
#29390=AXIS2_PLACEMENT_3D('',#127323,#33616,#33617);
#29391=AXIS2_PLACEMENT_3D('',#127326,#33619,#33620);
#29392=AXIS2_PLACEMENT_3D('',#127327,#33621,#33622);
#29393=AXIS2_PLACEMENT_3D('',#127331,#33625,#33626);
#29394=AXIS2_PLACEMENT_3D('',#127334,#33628,#33629);
#29395=AXIS2_PLACEMENT_3D('',#127335,#33630,#33631);
#29396=AXIS2_PLACEMENT_3D('',#127337,#33633,#33634);
#29397=AXIS2_PLACEMENT_3D('',#127343,#33638,#33639);
#29398=AXIS2_PLACEMENT_3D('',#127345,#33640,#33641);
#29399=AXIS2_PLACEMENT_3D('',#127347,#33642,#33643);
#29400=AXIS2_PLACEMENT_3D('',#127349,#33645,#33646);
#29401=AXIS2_PLACEMENT_3D('',#127355,#33650,#33651);
#29402=AXIS2_PLACEMENT_3D('',#127357,#33652,#33653);
#29403=AXIS2_PLACEMENT_3D('',#127359,#33654,#33655);
#29404=AXIS2_PLACEMENT_3D('',#127361,#33657,#33658);
#29405=AXIS2_PLACEMENT_3D('',#127367,#33662,#33663);
#29406=AXIS2_PLACEMENT_3D('',#127369,#33664,#33665);
#29407=AXIS2_PLACEMENT_3D('',#127371,#33666,#33667);
#29408=AXIS2_PLACEMENT_3D('',#127373,#33669,#33670);
#29409=AXIS2_PLACEMENT_3D('',#127379,#33674,#33675);
#29410=AXIS2_PLACEMENT_3D('',#127381,#33676,#33677);
#29411=AXIS2_PLACEMENT_3D('',#127383,#33678,#33679);
#29412=AXIS2_PLACEMENT_3D('',#127385,#33681,#33682);
#29413=AXIS2_PLACEMENT_3D('',#127391,#33686,#33687);
#29414=AXIS2_PLACEMENT_3D('',#127393,#33688,#33689);
#29415=AXIS2_PLACEMENT_3D('',#127395,#33690,#33691);
#29416=AXIS2_PLACEMENT_3D('',#127397,#33693,#33694);
#29417=AXIS2_PLACEMENT_3D('',#127403,#33698,#33699);
#29418=AXIS2_PLACEMENT_3D('',#127405,#33700,#33701);
#29419=AXIS2_PLACEMENT_3D('',#127407,#33702,#33703);
#29420=AXIS2_PLACEMENT_3D('',#127409,#33705,#33706);
#29421=AXIS2_PLACEMENT_3D('',#127415,#33710,#33711);
#29422=AXIS2_PLACEMENT_3D('',#127421,#33715,#33716);
#29423=AXIS2_PLACEMENT_3D('',#127427,#33720,#33721);
#29424=AXIS2_PLACEMENT_3D('',#127429,#33722,#33723);
#29425=AXIS2_PLACEMENT_3D('',#127431,#33724,#33725);
#29426=AXIS2_PLACEMENT_3D('',#127433,#33727,#33728);
#29427=AXIS2_PLACEMENT_3D('',#127439,#33732,#33733);
#29428=AXIS2_PLACEMENT_3D('',#127445,#33737,#33738);
#29429=AXIS2_PLACEMENT_3D('',#127448,#33741,#33742);
#29430=AXIS2_PLACEMENT_3D('',#127449,#33743,#33744);
#29431=AXIS2_PLACEMENT_3D('',#127450,#33745,#33746);
#29432=AXIS2_PLACEMENT_3D('',#127451,#33747,#33748);
#29433=AXIS2_PLACEMENT_3D('',#127452,#33749,#33750);
#29434=AXIS2_PLACEMENT_3D('',#127453,#33751,#33752);
#29435=AXIS2_PLACEMENT_3D('',#127459,#33755,#33756);
#29436=AXIS2_PLACEMENT_3D('',#127460,#33757,#33758);
#29437=AXIS2_PLACEMENT_3D('',#127465,#33760,#33761);
#29438=AXIS2_PLACEMENT_3D('',#127467,#33763,#33764);
#29439=AXIS2_PLACEMENT_3D('',#127469,#33765,#33766);
#29440=AXIS2_PLACEMENT_3D('',#127471,#33768,#33769);
#29441=AXIS2_PLACEMENT_3D('',#127480,#33774,#33775);
#29442=AXIS2_PLACEMENT_3D('',#127483,#33776,#33777);
#29443=AXIS2_PLACEMENT_3D('',#127491,#33781,#33782);
#29444=AXIS2_PLACEMENT_3D('',#127492,#33783,#33784);
#29445=AXIS2_PLACEMENT_3D('',#127496,#33786,#33787);
#29446=AXIS2_PLACEMENT_3D('',#127504,#33791,#33792);
#29447=AXIS2_PLACEMENT_3D('',#127509,#33795,#33796);
#29448=AXIS2_PLACEMENT_3D('',#127510,#33797,#33798);
#29449=AXIS2_PLACEMENT_3D('',#127513,#33799,#33800);
#29450=AXIS2_PLACEMENT_3D('',#127516,#33803,#33804);
#29451=AXIS2_PLACEMENT_3D('',#127520,#33807,#33808);
#29452=AXIS2_PLACEMENT_3D('',#127524,#33810,#33811);
#29453=AXIS2_PLACEMENT_3D('',#127532,#33815,#33816);
#29454=AXIS2_PLACEMENT_3D('',#127535,#33818,#33819);
#29455=AXIS2_PLACEMENT_3D('',#127537,#33820,#33821);
#29456=AXIS2_PLACEMENT_3D('',#127541,#33823,#33824);
#29457=AXIS2_PLACEMENT_3D('',#127545,#33826,#33827);
#29458=AXIS2_PLACEMENT_3D('',#127549,#33829,#33830);
#29459=AXIS2_PLACEMENT_3D('',#127553,#33832,#33833);
#29460=AXIS2_PLACEMENT_3D('',#127556,#33835,#33836);
#29461=AXIS2_PLACEMENT_3D('',#127557,#33837,#33838);
#29462=AXIS2_PLACEMENT_3D('',#127559,#33840,#33841);
#29463=AXIS2_PLACEMENT_3D('',#127561,#33843,#33844);
#29464=AXIS2_PLACEMENT_3D('',#127572,#33851,#33852);
#29465=AXIS2_PLACEMENT_3D('',#127574,#33854,#33855);
#29466=AXIS2_PLACEMENT_3D('',#127576,#33857,#33858);
#29467=AXIS2_PLACEMENT_3D('',#127578,#33860,#33861);
#29468=AXIS2_PLACEMENT_3D('',#127581,#33864,#33865);
#29469=AXIS2_PLACEMENT_3D('',#127584,#33868,#33869);
#29470=AXIS2_PLACEMENT_3D('',#127590,#33873,#33874);
#29471=AXIS2_PLACEMENT_3D('',#127594,#33877,#33878);
#29472=AXIS2_PLACEMENT_3D('',#127598,#33881,#33882);
#29473=AXIS2_PLACEMENT_3D('',#127600,#33884,#33885);
#29474=AXIS2_PLACEMENT_3D('',#127601,#33886,#33887);
#29475=AXIS2_PLACEMENT_3D('',#127606,#33889,#33890);
#29476=AXIS2_PLACEMENT_3D('',#127610,#33892,#33893);
#29477=AXIS2_PLACEMENT_3D('',#127612,#33895,#33896);
#29478=AXIS2_PLACEMENT_3D('',#127619,#33899,#33900);
#29479=AXIS2_PLACEMENT_3D('',#127622,#33902,#33903);
#29480=AXIS2_PLACEMENT_3D('',#127623,#33904,#33905);
#29481=AXIS2_PLACEMENT_3D('',#127626,#33908,#33909);
#29482=AXIS2_PLACEMENT_3D('',#127628,#33911,#33912);
#29483=AXIS2_PLACEMENT_3D('',#127630,#33914,#33915);
#29484=AXIS2_PLACEMENT_3D('',#127631,#33916,#33917);
#29485=AXIS2_PLACEMENT_3D('',#127632,#33918,#33919);
#29486=AXIS2_PLACEMENT_3D('',#127635,#33922,#33923);
#29487=AXIS2_PLACEMENT_3D('',#127637,#33925,#33926);
#29488=AXIS2_PLACEMENT_3D('',#127639,#33928,#33929);
#29489=AXIS2_PLACEMENT_3D('',#127644,#33931,#33932);
#29490=AXIS2_PLACEMENT_3D('',#127646,#33934,#33935);
#29491=AXIS2_PLACEMENT_3D('',#127652,#33938,#33939);
#29492=AXIS2_PLACEMENT_3D('',#127653,#33940,#33941);
#29493=AXIS2_PLACEMENT_3D('',#127655,#33942,#33943);
#29494=AXIS2_PLACEMENT_3D('',#127657,#33945,#33946);
#29495=AXIS2_PLACEMENT_3D('',#127664,#33951,#33952);
#29496=AXIS2_PLACEMENT_3D('',#127673,#33957,#33958);
#29497=AXIS2_PLACEMENT_3D('',#127675,#33959,#33960);
#29498=AXIS2_PLACEMENT_3D('',#127677,#33961,#33962);
#29499=AXIS2_PLACEMENT_3D('',#127683,#33965,#33966);
#29500=AXIS2_PLACEMENT_3D('',#127691,#33970,#33971);
#29501=AXIS2_PLACEMENT_3D('',#127694,#33973,#33974);
#29502=AXIS2_PLACEMENT_3D('',#127696,#33975,#33976);
#29503=AXIS2_PLACEMENT_3D('',#127700,#33979,#33980);
#29504=AXIS2_PLACEMENT_3D('',#127704,#33984,#33985);
#29505=AXIS2_PLACEMENT_3D('',#127707,#33986,#33987);
#29506=AXIS2_PLACEMENT_3D('',#127710,#33990,#33991);
#29507=AXIS2_PLACEMENT_3D('',#127714,#33994,#33995);
#29508=AXIS2_PLACEMENT_3D('',#127716,#33996,#33997);
#29509=AXIS2_PLACEMENT_3D('',#127720,#33999,#34000);
#29510=AXIS2_PLACEMENT_3D('',#127724,#34002,#34003);
#29511=AXIS2_PLACEMENT_3D('',#127728,#34005,#34006);
#29512=AXIS2_PLACEMENT_3D('',#127732,#34008,#34009);
#29513=AXIS2_PLACEMENT_3D('',#127736,#34011,#34012);
#29514=AXIS2_PLACEMENT_3D('',#127737,#34013,#34014);
#29515=AXIS2_PLACEMENT_3D('',#127741,#34016,#34017);
#29516=AXIS2_PLACEMENT_3D('',#127749,#34021,#34022);
#29517=AXIS2_PLACEMENT_3D('',#127751,#34024,#34025);
#29518=AXIS2_PLACEMENT_3D('',#127756,#34029,#34030);
#29519=AXIS2_PLACEMENT_3D('',#127758,#34032,#34033);
#29520=AXIS2_PLACEMENT_3D('',#127760,#34035,#34036);
#29521=AXIS2_PLACEMENT_3D('',#127771,#34043,#34044);
#29522=AXIS2_PLACEMENT_3D('',#127773,#34046,#34047);
#29523=AXIS2_PLACEMENT_3D('',#127775,#34049,#34050);
#29524=AXIS2_PLACEMENT_3D('',#127777,#34052,#34053);
#29525=AXIS2_PLACEMENT_3D('',#127778,#34054,#34055);
#29526=AXIS2_PLACEMENT_3D('',#127780,#34057,#34058);
#29527=AXIS2_PLACEMENT_3D('',#127786,#34062,#34063);
#29528=AXIS2_PLACEMENT_3D('',#127790,#34066,#34067);
#29529=AXIS2_PLACEMENT_3D('',#127794,#34070,#34071);
#29530=AXIS2_PLACEMENT_3D('',#127796,#34073,#34074);
#29531=AXIS2_PLACEMENT_3D('',#127797,#34075,#34076);
#29532=AXIS2_PLACEMENT_3D('',#127798,#34077,#34078);
#29533=AXIS2_PLACEMENT_3D('',#127802,#34081,#34082);
#29534=AXIS2_PLACEMENT_3D('',#127808,#34086,#34087);
#29535=AXIS2_PLACEMENT_3D('',#127812,#34089,#34090);
#29536=AXIS2_PLACEMENT_3D('',#127815,#34092,#34093);
#29537=AXIS2_PLACEMENT_3D('',#127816,#34094,#34095);
#29538=AXIS2_PLACEMENT_3D('',#127818,#34096,#34097);
#29539=AXIS2_PLACEMENT_3D('',#127822,#34099,#34100);
#29540=AXIS2_PLACEMENT_3D('',#127824,#34102,#34103);
#29541=AXIS2_PLACEMENT_3D('',#127826,#34105,#34106);
#29542=AXIS2_PLACEMENT_3D('',#127829,#34109,#34110);
#29543=AXIS2_PLACEMENT_3D('',#127831,#34112,#34113);
#29544=AXIS2_PLACEMENT_3D('',#127833,#34115,#34116);
#29545=AXIS2_PLACEMENT_3D('',#127834,#34117,#34118);
#29546=AXIS2_PLACEMENT_3D('',#127835,#34119,#34120);
#29547=AXIS2_PLACEMENT_3D('',#127836,#34121,#34122);
#29548=AXIS2_PLACEMENT_3D('',#127838,#34124,#34125);
#29549=AXIS2_PLACEMENT_3D('',#127840,#34127,#34128);
#29550=AXIS2_PLACEMENT_3D('',#127841,#34129,#34130);
#29551=AXIS2_PLACEMENT_3D('',#127842,#34131,#34132);
#29552=AXIS2_PLACEMENT_3D('',#127844,#34133,#34134);
#29553=AXIS2_PLACEMENT_3D('',#127847,#34136,#34137);
#29554=AXIS2_PLACEMENT_3D('',#127848,#34138,#34139);
#29555=AXIS2_PLACEMENT_3D('',#127851,#34140,#34141);
#29556=AXIS2_PLACEMENT_3D('',#127855,#34143,#34144);
#29557=AXIS2_PLACEMENT_3D('',#127857,#34146,#34147);
#29558=AXIS2_PLACEMENT_3D('',#127863,#34151,#34152);
#29559=AXIS2_PLACEMENT_3D('',#127869,#34156,#34157);
#29560=AXIS2_PLACEMENT_3D('',#127875,#34161,#34162);
#29561=AXIS2_PLACEMENT_3D('',#127881,#34166,#34167);
#29562=AXIS2_PLACEMENT_3D('',#127887,#34171,#34172);
#29563=AXIS2_PLACEMENT_3D('',#127889,#34173,#34174);
#29564=AXIS2_PLACEMENT_3D('',#127891,#34175,#34176);
#29565=AXIS2_PLACEMENT_3D('',#127893,#34178,#34179);
#29566=AXIS2_PLACEMENT_3D('',#127899,#34183,#34184);
#29567=AXIS2_PLACEMENT_3D('',#127905,#34188,#34189);
#29568=AXIS2_PLACEMENT_3D('',#127907,#34190,#34191);
#29569=AXIS2_PLACEMENT_3D('',#127909,#34192,#34193);
#29570=AXIS2_PLACEMENT_3D('',#127911,#34195,#34196);
#29571=AXIS2_PLACEMENT_3D('',#127913,#34197,#34198);
#29572=AXIS2_PLACEMENT_3D('',#127915,#34199,#34200);
#29573=AXIS2_PLACEMENT_3D('',#127917,#34202,#34203);
#29574=AXIS2_PLACEMENT_3D('',#127919,#34204,#34205);
#29575=AXIS2_PLACEMENT_3D('',#127921,#34206,#34207);
#29576=AXIS2_PLACEMENT_3D('',#127923,#34209,#34210);
#29577=AXIS2_PLACEMENT_3D('',#127929,#34214,#34215);
#29578=AXIS2_PLACEMENT_3D('',#127935,#34219,#34220);
#29579=AXIS2_PLACEMENT_3D('',#127941,#34224,#34225);
#29580=AXIS2_PLACEMENT_3D('',#127943,#34226,#34227);
#29581=AXIS2_PLACEMENT_3D('',#127945,#34228,#34229);
#29582=AXIS2_PLACEMENT_3D('',#127947,#34231,#34232);
#29583=AXIS2_PLACEMENT_3D('',#127953,#34236,#34237);
#29584=AXIS2_PLACEMENT_3D('',#127955,#34238,#34239);
#29585=AXIS2_PLACEMENT_3D('',#127957,#34240,#34241);
#29586=AXIS2_PLACEMENT_3D('',#127959,#34243,#34244);
#29587=AXIS2_PLACEMENT_3D('',#127965,#34248,#34249);
#29588=AXIS2_PLACEMENT_3D('',#127967,#34250,#34251);
#29589=AXIS2_PLACEMENT_3D('',#127969,#34252,#34253);
#29590=AXIS2_PLACEMENT_3D('',#127971,#34255,#34256);
#29591=AXIS2_PLACEMENT_3D('',#127977,#34260,#34261);
#29592=AXIS2_PLACEMENT_3D('',#127983,#34265,#34266);
#29593=AXIS2_PLACEMENT_3D('',#127989,#34270,#34271);
#29594=AXIS2_PLACEMENT_3D('',#127991,#34272,#34273);
#29595=AXIS2_PLACEMENT_3D('',#127993,#34274,#34275);
#29596=AXIS2_PLACEMENT_3D('',#127995,#34277,#34278);
#29597=AXIS2_PLACEMENT_3D('',#128001,#34282,#34283);
#29598=AXIS2_PLACEMENT_3D('',#128003,#34284,#34285);
#29599=AXIS2_PLACEMENT_3D('',#128005,#34286,#34287);
#29600=AXIS2_PLACEMENT_3D('',#128007,#34289,#34290);
#29601=AXIS2_PLACEMENT_3D('',#128013,#34294,#34295);
#29602=AXIS2_PLACEMENT_3D('',#128015,#34296,#34297);
#29603=AXIS2_PLACEMENT_3D('',#128017,#34298,#34299);
#29604=AXIS2_PLACEMENT_3D('',#128019,#34301,#34302);
#29605=AXIS2_PLACEMENT_3D('',#128025,#34306,#34307);
#29606=AXIS2_PLACEMENT_3D('',#128027,#34308,#34309);
#29607=AXIS2_PLACEMENT_3D('',#128029,#34310,#34311);
#29608=AXIS2_PLACEMENT_3D('',#128031,#34313,#34314);
#29609=AXIS2_PLACEMENT_3D('',#128037,#34318,#34319);
#29610=AXIS2_PLACEMENT_3D('',#128043,#34323,#34324);
#29611=AXIS2_PLACEMENT_3D('',#128049,#34328,#34329);
#29612=AXIS2_PLACEMENT_3D('',#128051,#34330,#34331);
#29613=AXIS2_PLACEMENT_3D('',#128053,#34332,#34333);
#29614=AXIS2_PLACEMENT_3D('',#128055,#34335,#34336);
#29615=AXIS2_PLACEMENT_3D('',#128061,#34340,#34341);
#29616=AXIS2_PLACEMENT_3D('',#128063,#34342,#34343);
#29617=AXIS2_PLACEMENT_3D('',#128065,#34344,#34345);
#29618=AXIS2_PLACEMENT_3D('',#128067,#34347,#34348);
#29619=AXIS2_PLACEMENT_3D('',#128073,#34352,#34353);
#29620=AXIS2_PLACEMENT_3D('',#128075,#34354,#34355);
#29621=AXIS2_PLACEMENT_3D('',#128077,#34356,#34357);
#29622=AXIS2_PLACEMENT_3D('',#128079,#34359,#34360);
#29623=AXIS2_PLACEMENT_3D('',#128085,#34364,#34365);
#29624=AXIS2_PLACEMENT_3D('',#128091,#34369,#34370);
#29625=AXIS2_PLACEMENT_3D('',#128097,#34374,#34375);
#29626=AXIS2_PLACEMENT_3D('',#128099,#34376,#34377);
#29627=AXIS2_PLACEMENT_3D('',#128101,#34378,#34379);
#29628=AXIS2_PLACEMENT_3D('',#128103,#34381,#34382);
#29629=AXIS2_PLACEMENT_3D('',#128105,#34383,#34384);
#29630=AXIS2_PLACEMENT_3D('',#128107,#34385,#34386);
#29631=AXIS2_PLACEMENT_3D('',#128109,#34388,#34389);
#29632=AXIS2_PLACEMENT_3D('',#128111,#34390,#34391);
#29633=AXIS2_PLACEMENT_3D('',#128113,#34392,#34393);
#29634=AXIS2_PLACEMENT_3D('',#128115,#34395,#34396);
#29635=AXIS2_PLACEMENT_3D('',#128121,#34400,#34401);
#29636=AXIS2_PLACEMENT_3D('',#128127,#34405,#34406);
#29637=AXIS2_PLACEMENT_3D('',#128129,#34407,#34408);
#29638=AXIS2_PLACEMENT_3D('',#128131,#34409,#34410);
#29639=AXIS2_PLACEMENT_3D('',#128133,#34412,#34413);
#29640=AXIS2_PLACEMENT_3D('',#128139,#34417,#34418);
#29641=AXIS2_PLACEMENT_3D('',#128145,#34422,#34423);
#29642=AXIS2_PLACEMENT_3D('',#128151,#34427,#34428);
#29643=AXIS2_PLACEMENT_3D('',#128157,#34432,#34433);
#29644=AXIS2_PLACEMENT_3D('',#128163,#34437,#34438);
#29645=AXIS2_PLACEMENT_3D('',#128165,#34439,#34440);
#29646=AXIS2_PLACEMENT_3D('',#128167,#34441,#34442);
#29647=AXIS2_PLACEMENT_3D('',#128169,#34444,#34445);
#29648=AXIS2_PLACEMENT_3D('',#128175,#34449,#34450);
#29649=AXIS2_PLACEMENT_3D('',#128181,#34454,#34455);
#29650=AXIS2_PLACEMENT_3D('',#128183,#34456,#34457);
#29651=AXIS2_PLACEMENT_3D('',#128185,#34458,#34459);
#29652=AXIS2_PLACEMENT_3D('',#128187,#34461,#34462);
#29653=AXIS2_PLACEMENT_3D('',#128189,#34463,#34464);
#29654=AXIS2_PLACEMENT_3D('',#128191,#34465,#34466);
#29655=AXIS2_PLACEMENT_3D('',#128193,#34468,#34469);
#29656=AXIS2_PLACEMENT_3D('',#128195,#34470,#34471);
#29657=AXIS2_PLACEMENT_3D('',#128197,#34472,#34473);
#29658=AXIS2_PLACEMENT_3D('',#128199,#34475,#34476);
#29659=AXIS2_PLACEMENT_3D('',#128205,#34480,#34481);
#29660=AXIS2_PLACEMENT_3D('',#128211,#34485,#34486);
#29661=AXIS2_PLACEMENT_3D('',#128217,#34490,#34491);
#29662=AXIS2_PLACEMENT_3D('',#128219,#34492,#34493);
#29663=AXIS2_PLACEMENT_3D('',#128221,#34494,#34495);
#29664=AXIS2_PLACEMENT_3D('',#128223,#34497,#34498);
#29665=AXIS2_PLACEMENT_3D('',#128229,#34502,#34503);
#29666=AXIS2_PLACEMENT_3D('',#128231,#34504,#34505);
#29667=AXIS2_PLACEMENT_3D('',#128233,#34506,#34507);
#29668=AXIS2_PLACEMENT_3D('',#128235,#34509,#34510);
#29669=AXIS2_PLACEMENT_3D('',#128241,#34514,#34515);
#29670=AXIS2_PLACEMENT_3D('',#128243,#34516,#34517);
#29671=AXIS2_PLACEMENT_3D('',#128245,#34518,#34519);
#29672=AXIS2_PLACEMENT_3D('',#128247,#34521,#34522);
#29673=AXIS2_PLACEMENT_3D('',#128253,#34526,#34527);
#29674=AXIS2_PLACEMENT_3D('',#128259,#34531,#34532);
#29675=AXIS2_PLACEMENT_3D('',#128265,#34536,#34537);
#29676=AXIS2_PLACEMENT_3D('',#128267,#34538,#34539);
#29677=AXIS2_PLACEMENT_3D('',#128269,#34540,#34541);
#29678=AXIS2_PLACEMENT_3D('',#128271,#34543,#34544);
#29679=AXIS2_PLACEMENT_3D('',#128277,#34548,#34549);
#29680=AXIS2_PLACEMENT_3D('',#128279,#34550,#34551);
#29681=AXIS2_PLACEMENT_3D('',#128281,#34552,#34553);
#29682=AXIS2_PLACEMENT_3D('',#128283,#34555,#34556);
#29683=AXIS2_PLACEMENT_3D('',#128289,#34560,#34561);
#29684=AXIS2_PLACEMENT_3D('',#128291,#34562,#34563);
#29685=AXIS2_PLACEMENT_3D('',#128293,#34564,#34565);
#29686=AXIS2_PLACEMENT_3D('',#128295,#34567,#34568);
#29687=AXIS2_PLACEMENT_3D('',#128301,#34572,#34573);
#29688=AXIS2_PLACEMENT_3D('',#128303,#34574,#34575);
#29689=AXIS2_PLACEMENT_3D('',#128305,#34576,#34577);
#29690=AXIS2_PLACEMENT_3D('',#128307,#34579,#34580);
#29691=AXIS2_PLACEMENT_3D('',#128313,#34584,#34585);
#29692=AXIS2_PLACEMENT_3D('',#128319,#34589,#34590);
#29693=AXIS2_PLACEMENT_3D('',#128325,#34594,#34595);
#29694=AXIS2_PLACEMENT_3D('',#128327,#34596,#34597);
#29695=AXIS2_PLACEMENT_3D('',#128329,#34598,#34599);
#29696=AXIS2_PLACEMENT_3D('',#128331,#34601,#34602);
#29697=AXIS2_PLACEMENT_3D('',#128337,#34606,#34607);
#29698=AXIS2_PLACEMENT_3D('',#128339,#34608,#34609);
#29699=AXIS2_PLACEMENT_3D('',#128341,#34610,#34611);
#29700=AXIS2_PLACEMENT_3D('',#128343,#34613,#34614);
#29701=AXIS2_PLACEMENT_3D('',#128349,#34618,#34619);
#29702=AXIS2_PLACEMENT_3D('',#128351,#34620,#34621);
#29703=AXIS2_PLACEMENT_3D('',#128353,#34622,#34623);
#29704=AXIS2_PLACEMENT_3D('',#128355,#34625,#34626);
#29705=AXIS2_PLACEMENT_3D('',#128361,#34630,#34631);
#29706=AXIS2_PLACEMENT_3D('',#128367,#34635,#34636);
#29707=AXIS2_PLACEMENT_3D('',#128373,#34640,#34641);
#29708=AXIS2_PLACEMENT_3D('',#128375,#34642,#34643);
#29709=AXIS2_PLACEMENT_3D('',#128377,#34644,#34645);
#29710=AXIS2_PLACEMENT_3D('',#128379,#34647,#34648);
#29711=AXIS2_PLACEMENT_3D('',#128381,#34649,#34650);
#29712=AXIS2_PLACEMENT_3D('',#128383,#34651,#34652);
#29713=AXIS2_PLACEMENT_3D('',#128385,#34654,#34655);
#29714=AXIS2_PLACEMENT_3D('',#128387,#34656,#34657);
#29715=AXIS2_PLACEMENT_3D('',#128389,#34658,#34659);
#29716=AXIS2_PLACEMENT_3D('',#128391,#34661,#34662);
#29717=AXIS2_PLACEMENT_3D('',#128397,#34666,#34667);
#29718=AXIS2_PLACEMENT_3D('',#128400,#34670,#34671);
#29719=AXIS2_PLACEMENT_3D('',#128401,#34672,#34673);
#29720=AXIS2_PLACEMENT_3D('',#128402,#34674,#34675);
#29721=AXIS2_PLACEMENT_3D('',#128403,#34676,#34677);
#29722=AXIS2_PLACEMENT_3D('',#128437,#34679,#34680);
#29723=AXIS2_PLACEMENT_3D('',#128442,#34681,#34682);
#29724=AXIS2_PLACEMENT_3D('',#128702,#34684,#34685);
#29725=AXIS2_PLACEMENT_3D('',#129146,#34687,#34688);
#29726=AXIS2_PLACEMENT_3D('',#129442,#34690,#34691);
#29727=AXIS2_PLACEMENT_3D('',#129476,#34693,#34694);
#29728=AXIS2_PLACEMENT_3D('',#129481,#34695,#34696);
#29729=AXIS2_PLACEMENT_3D('',#129741,#34698,#34699);
#29730=AXIS2_PLACEMENT_3D('',#130185,#34701,#34702);
#29731=AXIS2_PLACEMENT_3D('',#130481,#34704,#34705);
#29732=AXIS2_PLACEMENT_3D('',#130554,#34707,#34708);
#29733=AXIS2_PLACEMENT_3D('',#130569,#34709,#34710);
#29734=AXIS2_PLACEMENT_3D('',#130720,#34712,#34713);
#29735=AXIS2_PLACEMENT_3D('',#131053,#34715,#34716);
#29736=AXIS2_PLACEMENT_3D('',#131334,#34718,#34719);
#29737=AXIS2_PLACEMENT_3D('',#131670,#34721,#34722);
#29738=AXIS2_PLACEMENT_3D('',#131832,#34724,#34725);
#29739=AXIS2_PLACEMENT_3D('',#132102,#34727,#34728);
#29740=AXIS2_PLACEMENT_3D('',#132377,#34730,#34731);
#29741=AXIS2_PLACEMENT_3D('',#132711,#34733,#34734);
#29742=AXIS2_PLACEMENT_3D('',#132873,#34736,#34737);
#29743=AXIS2_PLACEMENT_3D('',#133140,#34739,#34740);
#29744=AXIS2_PLACEMENT_3D('',#133418,#34742,#34743);
#29745=AXIS2_PLACEMENT_3D('',#133751,#34745,#34746);
#29746=AXIS2_PLACEMENT_3D('',#133916,#34748,#34749);
#29747=AXIS2_PLACEMENT_3D('',#134185,#34751,#34752);
#29748=AXIS2_PLACEMENT_3D('',#134466,#34754,#34755);
#29749=AXIS2_PLACEMENT_3D('',#134799,#34757,#34758);
#29750=AXIS2_PLACEMENT_3D('',#134958,#34760,#34761);
#29751=AXIS2_PLACEMENT_3D('',#135228,#34763,#34764);
#29752=AXIS2_PLACEMENT_3D('',#135509,#34766,#34767);
#29753=AXIS2_PLACEMENT_3D('',#135840,#34769,#34770);
#29754=AXIS2_PLACEMENT_3D('',#136003,#34772,#34773);
#29755=AXIS2_PLACEMENT_3D('',#136269,#34775,#34776);
#29756=AXIS2_PLACEMENT_3D('',#136550,#34778,#34779);
#29757=AXIS2_PLACEMENT_3D('',#136883,#34781,#34782);
#29758=AXIS2_PLACEMENT_3D('',#137164,#34784,#34785);
#29759=AXIS2_PLACEMENT_3D('',#137262,#34787,#34788);
#29760=AXIS2_PLACEMENT_3D('',#137335,#34790,#34791);
#29761=AXIS2_PLACEMENT_3D('',#137350,#34792,#34793);
#29762=AXIS2_PLACEMENT_3D('',#137501,#34795,#34796);
#29763=AXIS2_PLACEMENT_3D('',#137834,#34798,#34799);
#29764=AXIS2_PLACEMENT_3D('',#138115,#34801,#34802);
#29765=AXIS2_PLACEMENT_3D('',#138451,#34804,#34805);
#29766=AXIS2_PLACEMENT_3D('',#138613,#34807,#34808);
#29767=AXIS2_PLACEMENT_3D('',#138883,#34810,#34811);
#29768=AXIS2_PLACEMENT_3D('',#139158,#34813,#34814);
#29769=AXIS2_PLACEMENT_3D('',#139492,#34816,#34817);
#29770=AXIS2_PLACEMENT_3D('',#139654,#34819,#34820);
#29771=AXIS2_PLACEMENT_3D('',#139921,#34822,#34823);
#29772=AXIS2_PLACEMENT_3D('',#140199,#34825,#34826);
#29773=AXIS2_PLACEMENT_3D('',#140532,#34828,#34829);
#29774=AXIS2_PLACEMENT_3D('',#140697,#34831,#34832);
#29775=AXIS2_PLACEMENT_3D('',#140966,#34834,#34835);
#29776=AXIS2_PLACEMENT_3D('',#141247,#34837,#34838);
#29777=AXIS2_PLACEMENT_3D('',#141580,#34840,#34841);
#29778=AXIS2_PLACEMENT_3D('',#141739,#34843,#34844);
#29779=AXIS2_PLACEMENT_3D('',#142009,#34846,#34847);
#29780=AXIS2_PLACEMENT_3D('',#142290,#34849,#34850);
#29781=AXIS2_PLACEMENT_3D('',#142621,#34852,#34853);
#29782=AXIS2_PLACEMENT_3D('',#142784,#34855,#34856);
#29783=AXIS2_PLACEMENT_3D('',#143050,#34858,#34859);
#29784=AXIS2_PLACEMENT_3D('',#143331,#34861,#34862);
#29785=AXIS2_PLACEMENT_3D('',#143664,#34864,#34865);
#29786=AXIS2_PLACEMENT_3D('',#143945,#34867,#34868);
#29787=AXIS2_PLACEMENT_3D('',#144043,#34870,#34871);
#29788=AXIS2_PLACEMENT_3D('',#144116,#34873,#34874);
#29789=AXIS2_PLACEMENT_3D('',#144131,#34875,#34876);
#29790=AXIS2_PLACEMENT_3D('',#144282,#34878,#34879);
#29791=AXIS2_PLACEMENT_3D('',#144615,#34881,#34882);
#29792=AXIS2_PLACEMENT_3D('',#144896,#34884,#34885);
#29793=AXIS2_PLACEMENT_3D('',#145232,#34887,#34888);
#29794=AXIS2_PLACEMENT_3D('',#145394,#34890,#34891);
#29795=AXIS2_PLACEMENT_3D('',#145664,#34893,#34894);
#29796=AXIS2_PLACEMENT_3D('',#145939,#34896,#34897);
#29797=AXIS2_PLACEMENT_3D('',#146273,#34899,#34900);
#29798=AXIS2_PLACEMENT_3D('',#146435,#34902,#34903);
#29799=AXIS2_PLACEMENT_3D('',#146702,#34905,#34906);
#29800=AXIS2_PLACEMENT_3D('',#146980,#34908,#34909);
#29801=AXIS2_PLACEMENT_3D('',#147313,#34911,#34912);
#29802=AXIS2_PLACEMENT_3D('',#147478,#34914,#34915);
#29803=AXIS2_PLACEMENT_3D('',#147747,#34917,#34918);
#29804=AXIS2_PLACEMENT_3D('',#148028,#34920,#34921);
#29805=AXIS2_PLACEMENT_3D('',#148361,#34923,#34924);
#29806=AXIS2_PLACEMENT_3D('',#148520,#34926,#34927);
#29807=AXIS2_PLACEMENT_3D('',#148790,#34929,#34930);
#29808=AXIS2_PLACEMENT_3D('',#149071,#34932,#34933);
#29809=AXIS2_PLACEMENT_3D('',#149402,#34935,#34936);
#29810=AXIS2_PLACEMENT_3D('',#149565,#34938,#34939);
#29811=AXIS2_PLACEMENT_3D('',#149831,#34941,#34942);
#29812=AXIS2_PLACEMENT_3D('',#150112,#34944,#34945);
#29813=AXIS2_PLACEMENT_3D('',#150445,#34947,#34948);
#29814=AXIS2_PLACEMENT_3D('',#150726,#34950,#34951);
#29815=AXIS2_PLACEMENT_3D('',#150824,#34953,#34954);
#29816=AXIS2_PLACEMENT_3D('',#150897,#34956,#34957);
#29817=AXIS2_PLACEMENT_3D('',#150912,#34958,#34959);
#29818=AXIS2_PLACEMENT_3D('',#151063,#34961,#34962);
#29819=AXIS2_PLACEMENT_3D('',#151396,#34964,#34965);
#29820=AXIS2_PLACEMENT_3D('',#151677,#34967,#34968);
#29821=AXIS2_PLACEMENT_3D('',#152013,#34970,#34971);
#29822=AXIS2_PLACEMENT_3D('',#152175,#34973,#34974);
#29823=AXIS2_PLACEMENT_3D('',#152445,#34976,#34977);
#29824=AXIS2_PLACEMENT_3D('',#152720,#34979,#34980);
#29825=AXIS2_PLACEMENT_3D('',#153054,#34982,#34983);
#29826=AXIS2_PLACEMENT_3D('',#153216,#34985,#34986);
#29827=AXIS2_PLACEMENT_3D('',#153483,#34988,#34989);
#29828=AXIS2_PLACEMENT_3D('',#153761,#34991,#34992);
#29829=AXIS2_PLACEMENT_3D('',#154094,#34994,#34995);
#29830=AXIS2_PLACEMENT_3D('',#154259,#34997,#34998);
#29831=AXIS2_PLACEMENT_3D('',#154528,#35000,#35001);
#29832=AXIS2_PLACEMENT_3D('',#154809,#35003,#35004);
#29833=AXIS2_PLACEMENT_3D('',#155142,#35006,#35007);
#29834=AXIS2_PLACEMENT_3D('',#155301,#35009,#35010);
#29835=AXIS2_PLACEMENT_3D('',#155571,#35012,#35013);
#29836=AXIS2_PLACEMENT_3D('',#155852,#35015,#35016);
#29837=AXIS2_PLACEMENT_3D('',#156183,#35018,#35019);
#29838=AXIS2_PLACEMENT_3D('',#156346,#35021,#35022);
#29839=AXIS2_PLACEMENT_3D('',#156612,#35024,#35025);
#29840=AXIS2_PLACEMENT_3D('',#156893,#35027,#35028);
#29841=AXIS2_PLACEMENT_3D('',#157226,#35030,#35031);
#29842=AXIS2_PLACEMENT_3D('',#157507,#35033,#35034);
#29843=AXIS2_PLACEMENT_3D('',#157605,#35036,#35037);
#29844=AXIS2_PLACEMENT_3D('',#157626,#35039,#35040);
#29845=AXIS2_PLACEMENT_3D('',#157627,#35041,#35042);
#29846=AXIS2_PLACEMENT_3D('',#157686,#35044,#35045);
#29847=AXIS2_PLACEMENT_3D('',#157739,#35046,#35047);
#29848=AXIS2_PLACEMENT_3D('',#158027,#35049,#35050);
#29849=AXIS2_PLACEMENT_3D('',#158313,#35052,#35053);
#29850=AXIS2_PLACEMENT_3D('',#158334,#35055,#35056);
#29851=AXIS2_PLACEMENT_3D('',#158369,#35057,#35058);
#29852=AXIS2_PLACEMENT_3D('',#158655,#35060,#35061);
#29853=AXIS2_PLACEMENT_3D('',#158945,#35063,#35064);
#29854=AXIS2_PLACEMENT_3D('',#158950,#35066,#35067);
#29855=AXIS2_PLACEMENT_3D('',#159057,#35068,#35069);
#29856=AXIS2_PLACEMENT_3D('',#159243,#35071,#35072);
#29857=AXIS2_PLACEMENT_3D('',#159389,#35073,#35074);
#29858=AXIS2_PLACEMENT_3D('',#159825,#35076,#35077);
#29859=AXIS2_PLACEMENT_3D('',#160284,#35079,#35080);
#29860=AXIS2_PLACEMENT_3D('',#160586,#35082,#35083);
#29861=AXIS2_PLACEMENT_3D('',#161058,#35085,#35086);
#29862=AXIS2_PLACEMENT_3D('',#161548,#35088,#35089);
#29863=AXIS2_PLACEMENT_3D('',#162066,#35091,#35092);
#29864=AXIS2_PLACEMENT_3D('',#162545,#35094,#35095);
#29865=AXIS2_PLACEMENT_3D('',#162964,#35097,#35098);
#29866=AXIS2_PLACEMENT_3D('',#163232,#35100,#35101);
#29867=AXIS2_PLACEMENT_3D('',#163690,#35103,#35104);
#29868=AXIS2_PLACEMENT_3D('',#164153,#35106,#35107);
#29869=AXIS2_PLACEMENT_3D('',#164453,#35109,#35110);
#29870=AXIS2_PLACEMENT_3D('',#164894,#35112,#35113);
#29871=AXIS2_PLACEMENT_3D('',#165317,#35115,#35116);
#29872=AXIS2_PLACEMENT_3D('',#165615,#35118,#35119);
#29873=AXIS2_PLACEMENT_3D('',#166079,#35121,#35122);
#29874=AXIS2_PLACEMENT_3D('',#166547,#35124,#35125);
#29875=AXIS2_PLACEMENT_3D('',#166790,#35127,#35128);
#29876=AXIS2_PLACEMENT_3D('',#167222,#35130,#35131);
#29877=AXIS2_PLACEMENT_3D('',#167690,#35133,#35134);
#29878=AXIS2_PLACEMENT_3D('',#168200,#35136,#35137);
#29879=AXIS2_PLACEMENT_3D('',#168670,#35139,#35140);
#29880=AXIS2_PLACEMENT_3D('',#169136,#35142,#35143);
#29881=AXIS2_PLACEMENT_3D('',#169435,#35145,#35146);
#29882=AXIS2_PLACEMENT_3D('',#169913,#35148,#35149);
#29883=AXIS2_PLACEMENT_3D('',#170348,#35151,#35152);
#29884=AXIS2_PLACEMENT_3D('',#170534,#35154,#35155);
#29885=AXIS2_PLACEMENT_3D('',#170680,#35156,#35157);
#29886=AXIS2_PLACEMENT_3D('',#171116,#35159,#35160);
#29887=AXIS2_PLACEMENT_3D('',#171571,#35162,#35163);
#29888=AXIS2_PLACEMENT_3D('',#171875,#35165,#35166);
#29889=AXIS2_PLACEMENT_3D('',#172347,#35168,#35169);
#29890=AXIS2_PLACEMENT_3D('',#172829,#35171,#35172);
#29891=AXIS2_PLACEMENT_3D('',#173335,#35174,#35175);
#29892=AXIS2_PLACEMENT_3D('',#173816,#35177,#35178);
#29893=AXIS2_PLACEMENT_3D('',#174281,#35180,#35181);
#29894=AXIS2_PLACEMENT_3D('',#174549,#35183,#35184);
#29895=AXIS2_PLACEMENT_3D('',#175007,#35186,#35187);
#29896=AXIS2_PLACEMENT_3D('',#175470,#35189,#35190);
#29897=AXIS2_PLACEMENT_3D('',#175770,#35192,#35193);
#29898=AXIS2_PLACEMENT_3D('',#176221,#35195,#35196);
#29899=AXIS2_PLACEMENT_3D('',#176646,#35198,#35199);
#29900=AXIS2_PLACEMENT_3D('',#176932,#35201,#35202);
#29901=AXIS2_PLACEMENT_3D('',#177400,#35204,#35205);
#29902=AXIS2_PLACEMENT_3D('',#177868,#35207,#35208);
#29903=AXIS2_PLACEMENT_3D('',#178111,#35210,#35211);
#29904=AXIS2_PLACEMENT_3D('',#178543,#35213,#35214);
#29905=AXIS2_PLACEMENT_3D('',#179013,#35216,#35217);
#29906=AXIS2_PLACEMENT_3D('',#179543,#35219,#35220);
#29907=AXIS2_PLACEMENT_3D('',#180013,#35222,#35223);
#29908=AXIS2_PLACEMENT_3D('',#180477,#35225,#35226);
#29909=AXIS2_PLACEMENT_3D('',#180746,#35228,#35229);
#29910=AXIS2_PLACEMENT_3D('',#181224,#35231,#35232);
#29911=AXIS2_PLACEMENT_3D('',#181659,#35234,#35235);
#29912=AXIS2_PLACEMENT_3D('',#181845,#35237,#35238);
#29913=AXIS2_PLACEMENT_3D('',#181991,#35239,#35240);
#29914=AXIS2_PLACEMENT_3D('',#182427,#35242,#35243);
#29915=AXIS2_PLACEMENT_3D('',#182886,#35245,#35246);
#29916=AXIS2_PLACEMENT_3D('',#183188,#35248,#35249);
#29917=AXIS2_PLACEMENT_3D('',#183648,#35251,#35252);
#29918=AXIS2_PLACEMENT_3D('',#184130,#35254,#35255);
#29919=AXIS2_PLACEMENT_3D('',#184640,#35257,#35258);
#29920=AXIS2_PLACEMENT_3D('',#185111,#35260,#35261);
#29921=AXIS2_PLACEMENT_3D('',#185534,#35263,#35264);
#29922=AXIS2_PLACEMENT_3D('',#185802,#35266,#35267);
#29923=AXIS2_PLACEMENT_3D('',#186262,#35269,#35270);
#29924=AXIS2_PLACEMENT_3D('',#186725,#35272,#35273);
#29925=AXIS2_PLACEMENT_3D('',#187049,#35275,#35276);
#29926=AXIS2_PLACEMENT_3D('',#187534,#35278,#35279);
#29927=AXIS2_PLACEMENT_3D('',#187995,#35281,#35282);
#29928=AXIS2_PLACEMENT_3D('',#188295,#35284,#35285);
#29929=AXIS2_PLACEMENT_3D('',#188759,#35287,#35288);
#29930=AXIS2_PLACEMENT_3D('',#189227,#35290,#35291);
#29931=AXIS2_PLACEMENT_3D('',#189470,#35293,#35294);
#29932=AXIS2_PLACEMENT_3D('',#189902,#35296,#35297);
#29933=AXIS2_PLACEMENT_3D('',#190378,#35299,#35300);
#29934=AXIS2_PLACEMENT_3D('',#190888,#35302,#35303);
#29935=AXIS2_PLACEMENT_3D('',#191362,#35305,#35306);
#29936=AXIS2_PLACEMENT_3D('',#191820,#35308,#35309);
#29937=AXIS2_PLACEMENT_3D('',#192075,#35311,#35312);
#29938=AXIS2_PLACEMENT_3D('',#192555,#35314,#35315);
#29939=AXIS2_PLACEMENT_3D('',#192990,#35317,#35318);
#29940=AXIS2_PLACEMENT_3D('',#193176,#35320,#35321);
#29941=AXIS2_PLACEMENT_3D('',#193322,#35322,#35323);
#29942=AXIS2_PLACEMENT_3D('',#193758,#35325,#35326);
#29943=AXIS2_PLACEMENT_3D('',#194215,#35328,#35329);
#29944=AXIS2_PLACEMENT_3D('',#194519,#35331,#35332);
#29945=AXIS2_PLACEMENT_3D('',#194981,#35334,#35335);
#29946=AXIS2_PLACEMENT_3D('',#195459,#35337,#35338);
#29947=AXIS2_PLACEMENT_3D('',#195951,#35340,#35341);
#29948=AXIS2_PLACEMENT_3D('',#196422,#35343,#35344);
#29949=AXIS2_PLACEMENT_3D('',#196891,#35346,#35347);
#29950=AXIS2_PLACEMENT_3D('',#197159,#35349,#35350);
#29951=AXIS2_PLACEMENT_3D('',#197625,#35352,#35353);
#29952=AXIS2_PLACEMENT_3D('',#198090,#35355,#35356);
#29953=AXIS2_PLACEMENT_3D('',#198388,#35358,#35359);
#29954=AXIS2_PLACEMENT_3D('',#198839,#35361,#35362);
#29955=AXIS2_PLACEMENT_3D('',#199264,#35364,#35365);
#29956=AXIS2_PLACEMENT_3D('',#199558,#35367,#35368);
#29957=AXIS2_PLACEMENT_3D('',#200024,#35370,#35371);
#29958=AXIS2_PLACEMENT_3D('',#200492,#35373,#35374);
#29959=AXIS2_PLACEMENT_3D('',#200735,#35376,#35377);
#29960=AXIS2_PLACEMENT_3D('',#201213,#35379,#35380);
#29961=AXIS2_PLACEMENT_3D('',#201691,#35382,#35383);
#29962=AXIS2_PLACEMENT_3D('',#202219,#35385,#35386);
#29963=AXIS2_PLACEMENT_3D('',#202693,#35388,#35389);
#29964=AXIS2_PLACEMENT_3D('',#203139,#35391,#35392);
#29965=AXIS2_PLACEMENT_3D('',#203436,#35394,#35395);
#29966=AXIS2_PLACEMENT_3D('',#203912,#35397,#35398);
#29967=AXIS2_PLACEMENT_3D('',#204347,#35400,#35401);
#29968=AXIS2_PLACEMENT_3D('',#204510,#35402,#35403);
#29969=AXIS2_PLACEMENT_3D('',#204617,#35404,#35405);
#29970=AXIS2_PLACEMENT_3D('',#204780,#35406,#35407);
#29971=AXIS2_PLACEMENT_3D('',#204887,#35408,#35409);
#29972=AXIS2_PLACEMENT_3D('',#205050,#35410,#35411);
#29973=AXIS2_PLACEMENT_3D('',#205157,#35412,#35413);
#29974=AXIS2_PLACEMENT_3D('',#205320,#35414,#35415);
#29975=AXIS2_PLACEMENT_3D('',#205427,#35416,#35417);
#29976=AXIS2_PLACEMENT_3D('',#205445,#35418,#35419);
#29977=AXIS2_PLACEMENT_3D('',#205446,#35420,#35421);
#29978=AXIS2_PLACEMENT_3D('',#205464,#35422,#35423);
#29979=AXIS2_PLACEMENT_3D('',#205499,#35424,#35425);
#29980=AXIS2_PLACEMENT_3D('',#205568,#35426,#35427);
#29981=AXIS2_PLACEMENT_3D('',#205581,#35428,#35429);
#29982=AXIS2_PLACEMENT_3D('',#205650,#35430,#35431);
#29983=AXIS2_PLACEMENT_3D('',#205663,#35432,#35433);
#29984=AXIS2_PLACEMENT_3D('',#205732,#35434,#35435);
#29985=AXIS2_PLACEMENT_3D('',#205745,#35436,#35437);
#29986=AXIS2_PLACEMENT_3D('',#205814,#35438,#35439);
#29987=AXIS2_PLACEMENT_3D('',#205827,#35440,#35441);
#29988=AXIS2_PLACEMENT_3D('',#205991,#35442,#35443);
#29989=AXIS2_PLACEMENT_3D('',#206047,#35444,#35445);
#29990=AXIS2_PLACEMENT_3D('',#206211,#35446,#35447);
#29991=AXIS2_PLACEMENT_3D('',#206267,#35448,#35449);
#29992=AXIS2_PLACEMENT_3D('',#206269,#35450,#35451);
#29993=AXIS2_PLACEMENT_3D('',#206272,#35453,#35454);
#29994=AXIS2_PLACEMENT_3D('',#206273,#35455,#35456);
#29995=AXIS2_PLACEMENT_3D('',#206274,#35457,#35458);
#29996=AXIS2_PLACEMENT_3D('',#206277,#35459,#35460);
#29997=AXIS2_PLACEMENT_3D('',#206281,#35462,#35463);
#29998=AXIS2_PLACEMENT_3D('',#206283,#35465,#35466);
#29999=AXIS2_PLACEMENT_3D('',#206287,#35468,#35469);
#30000=AXIS2_PLACEMENT_3D('',#206291,#35472,#35473);
#30001=AXIS2_PLACEMENT_3D('',#206293,#35474,#35475);
#30002=AXIS2_PLACEMENT_3D('',#206296,#35477,#35478);
#30003=AXIS2_PLACEMENT_3D('',#206297,#35479,#35480);
#30004=AXIS2_PLACEMENT_3D('',#206298,#35481,#35482);
#30005=AXIS2_PLACEMENT_3D('',#206301,#35483,#35484);
#30006=AXIS2_PLACEMENT_3D('',#206305,#35486,#35487);
#30007=AXIS2_PLACEMENT_3D('',#206307,#35489,#35490);
#30008=AXIS2_PLACEMENT_3D('',#206312,#35492,#35493);
#30009=AXIS2_PLACEMENT_3D('',#206315,#35496,#35497);
#30010=AXIS2_PLACEMENT_3D('',#206317,#35498,#35499);
#30011=AXIS2_PLACEMENT_3D('',#206320,#35501,#35502);
#30012=AXIS2_PLACEMENT_3D('',#206321,#35503,#35504);
#30013=AXIS2_PLACEMENT_3D('',#206322,#35505,#35506);
#30014=AXIS2_PLACEMENT_3D('',#206328,#35510,#35511);
#30015=AXIS2_PLACEMENT_3D('',#206336,#35516,#35517);
#30016=AXIS2_PLACEMENT_3D('',#206341,#35521,#35522);
#30017=AXIS2_PLACEMENT_3D('',#206343,#35523,#35524);
#30018=AXIS2_PLACEMENT_3D('',#206347,#35526,#35527);
#30019=AXIS2_PLACEMENT_3D('',#206351,#35529,#35530);
#30020=AXIS2_PLACEMENT_3D('',#206355,#35532,#35533);
#30021=AXIS2_PLACEMENT_3D('',#206367,#35539,#35540);
#30022=AXIS2_PLACEMENT_3D('',#206371,#35542,#35543);
#30023=AXIS2_PLACEMENT_3D('',#206383,#35549,#35550);
#30024=AXIS2_PLACEMENT_3D('',#206387,#35552,#35553);
#30025=AXIS2_PLACEMENT_3D('',#206391,#35555,#35556);
#30026=AXIS2_PLACEMENT_3D('',#206395,#35558,#35559);
#30027=AXIS2_PLACEMENT_3D('',#206398,#35561,#35562);
#30028=AXIS2_PLACEMENT_3D('',#206400,#35563,#35564);
#30029=AXIS2_PLACEMENT_3D('',#215196,#35565,#35566);
#30030=AXIS2_PLACEMENT_3D('',#215205,#35571,#35572);
#30031=AXIS2_PLACEMENT_3D('',#215211,#35576,#35577);
#30032=AXIS2_PLACEMENT_3D('',#215217,#35581,#35582);
#30033=AXIS2_PLACEMENT_3D('',#215223,#35586,#35587);
#30034=AXIS2_PLACEMENT_3D('',#215229,#35591,#35592);
#30035=AXIS2_PLACEMENT_3D('',#215235,#35596,#35597);
#30036=AXIS2_PLACEMENT_3D('',#215238,#35600,#35601);
#30037=AXIS2_PLACEMENT_3D('',#215240,#35602,#35603);
#30038=AXIS2_PLACEMENT_3D('',#215243,#35605,#35606);
#30039=AXIS2_PLACEMENT_3D('',#215244,#35607,#35608);
#30040=AXIS2_PLACEMENT_3D('',#215245,#35609,#35610);
#30041=AXIS2_PLACEMENT_3D('',#215248,#35611,#35612);
#30042=AXIS2_PLACEMENT_3D('',#215252,#35614,#35615);
#30043=AXIS2_PLACEMENT_3D('',#215254,#35617,#35618);
#30044=AXIS2_PLACEMENT_3D('',#215260,#35622,#35623);
#30045=AXIS2_PLACEMENT_3D('',#215262,#35624,#35625);
#30046=AXIS2_PLACEMENT_3D('',#215265,#35627,#35628);
#30047=AXIS2_PLACEMENT_3D('',#215266,#35629,#35630);
#30048=AXIS2_PLACEMENT_3D('',#215269,#35633,#35634);
#30049=AXIS2_PLACEMENT_3D('',#215272,#35637,#35638);
#30050=AXIS2_PLACEMENT_3D('',#215274,#35639,#35640);
#30051=AXIS2_PLACEMENT_3D('',#215276,#35641,#35642);
#30052=AXIS2_PLACEMENT_3D('',#215277,#35643,#35644);
#30053=AXIS2_PLACEMENT_3D('',#215286,#35649,#35650);
#30054=AXIS2_PLACEMENT_3D('',#215292,#35654,#35655);
#30055=AXIS2_PLACEMENT_3D('',#215298,#35659,#35660);
#30056=AXIS2_PLACEMENT_3D('',#215304,#35664,#35665);
#30057=AXIS2_PLACEMENT_3D('',#215310,#35669,#35670);
#30058=AXIS2_PLACEMENT_3D('',#215316,#35674,#35675);
#30059=AXIS2_PLACEMENT_3D('',#215319,#35678,#35679);
#30060=AXIS2_PLACEMENT_3D('',#215321,#35680,#35681);
#30061=AXIS2_PLACEMENT_3D('',#215324,#35683,#35684);
#30062=AXIS2_PLACEMENT_3D('',#215325,#35685,#35686);
#30063=AXIS2_PLACEMENT_3D('',#215326,#35687,#35688);
#30064=AXIS2_PLACEMENT_3D('',#215327,#35689,#35690);
#30065=AXIS2_PLACEMENT_3D('',#215328,#35691,#35692);
#30066=AXIS2_PLACEMENT_3D('',#215331,#35694,#35695);
#30067=AXIS2_PLACEMENT_3D('',#215332,#35696,#35697);
#30068=AXIS2_PLACEMENT_3D('',#215333,#35698,#35699);
#30069=AXIS2_PLACEMENT_3D('',#215334,#35700,#35701);
#30070=AXIS2_PLACEMENT_3D('',#215337,#35703,#35704);
#30071=AXIS2_PLACEMENT_3D('',#215338,#35705,#35706);
#30072=AXIS2_PLACEMENT_3D('',#215339,#35707,#35708);
#30073=AXIS2_PLACEMENT_3D('',#215342,#35709,#35710);
#30074=AXIS2_PLACEMENT_3D('',#215346,#35712,#35713);
#30075=AXIS2_PLACEMENT_3D('',#215348,#35715,#35716);
#30076=AXIS2_PLACEMENT_3D('',#215354,#35720,#35721);
#30077=AXIS2_PLACEMENT_3D('',#215356,#35722,#35723);
#30078=AXIS2_PLACEMENT_3D('',#215358,#35724,#35725);
#30079=AXIS2_PLACEMENT_3D('',#215360,#35727,#35728);
#30080=AXIS2_PLACEMENT_3D('',#215363,#35731,#35732);
#30081=AXIS2_PLACEMENT_3D('',#215366,#35735,#35736);
#30082=AXIS2_PLACEMENT_3D('',#215368,#35737,#35738);
#30083=AXIS2_PLACEMENT_3D('',#215370,#35739,#35740);
#30084=AXIS2_PLACEMENT_3D('',#215371,#35741,#35742);
#30085=AXIS2_PLACEMENT_3D('',#215380,#35747,#35748);
#30086=AXIS2_PLACEMENT_3D('',#215386,#35752,#35753);
#30087=AXIS2_PLACEMENT_3D('',#215392,#35757,#35758);
#30088=AXIS2_PLACEMENT_3D('',#215398,#35762,#35763);
#30089=AXIS2_PLACEMENT_3D('',#215404,#35767,#35768);
#30090=AXIS2_PLACEMENT_3D('',#215410,#35772,#35773);
#30091=AXIS2_PLACEMENT_3D('',#215413,#35776,#35777);
#30092=AXIS2_PLACEMENT_3D('',#215415,#35778,#35779);
#30093=AXIS2_PLACEMENT_3D('',#215418,#35781,#35782);
#30094=AXIS2_PLACEMENT_3D('',#215419,#35783,#35784);
#30095=AXIS2_PLACEMENT_3D('',#215420,#35785,#35786);
#30096=AXIS2_PLACEMENT_3D('',#215429,#35791,#35792);
#30097=AXIS2_PLACEMENT_3D('',#215435,#35796,#35797);
#30098=AXIS2_PLACEMENT_3D('',#215441,#35801,#35802);
#30099=AXIS2_PLACEMENT_3D('',#215447,#35806,#35807);
#30100=AXIS2_PLACEMENT_3D('',#215453,#35811,#35812);
#30101=AXIS2_PLACEMENT_3D('',#215459,#35816,#35817);
#30102=AXIS2_PLACEMENT_3D('',#215462,#35820,#35821);
#30103=AXIS2_PLACEMENT_3D('',#215464,#35822,#35823);
#30104=AXIS2_PLACEMENT_3D('',#215467,#35825,#35826);
#30105=AXIS2_PLACEMENT_3D('',#215468,#35827,#35828);
#30106=AXIS2_PLACEMENT_3D('',#215469,#35829,#35830);
#30107=AXIS2_PLACEMENT_3D('',#215470,#35831,#35832);
#30108=AXIS2_PLACEMENT_3D('',#215471,#35833,#35834);
#30109=AXIS2_PLACEMENT_3D('',#215477,#35838,#35839);
#30110=AXIS2_PLACEMENT_3D('',#215478,#35840,#35841);
#30111=AXIS2_PLACEMENT_3D('',#215480,#35842,#35843);
#30112=AXIS2_PLACEMENT_3D('',#215482,#35845,#35846);
#30113=AXIS2_PLACEMENT_3D('',#215483,#35847,#35848);
#30114=AXIS2_PLACEMENT_3D('',#215485,#35849,#35850);
#30115=AXIS2_PLACEMENT_3D('',#215487,#35852,#35853);
#30116=AXIS2_PLACEMENT_3D('',#215488,#35854,#35855);
#30117=AXIS2_PLACEMENT_3D('',#215490,#35856,#35857);
#30118=AXIS2_PLACEMENT_3D('',#215492,#35859,#35860);
#30119=AXIS2_PLACEMENT_3D('',#215493,#35861,#35862);
#30120=AXIS2_PLACEMENT_3D('',#215495,#35863,#35864);
#30121=AXIS2_PLACEMENT_3D('',#215497,#35866,#35867);
#30122=AXIS2_PLACEMENT_3D('',#215498,#35868,#35869);
#30123=AXIS2_PLACEMENT_3D('',#215502,#35872,#35873);
#30124=AXIS2_PLACEMENT_3D('',#215503,#35874,#35875);
#30125=AXIS2_PLACEMENT_3D('',#215504,#35876,#35877);
#30126=AXIS2_PLACEMENT_3D('',#215506,#35878,#35879);
#30127=AXIS2_PLACEMENT_3D('',#215508,#35881,#35882);
#30128=AXIS2_PLACEMENT_3D('',#215512,#35885,#35886);
#30129=AXIS2_PLACEMENT_3D('',#215514,#35887,#35888);
#30130=AXIS2_PLACEMENT_3D('',#215516,#35890,#35891);
#30131=AXIS2_PLACEMENT_3D('',#215520,#35894,#35895);
#30132=AXIS2_PLACEMENT_3D('',#215522,#35896,#35897);
#30133=AXIS2_PLACEMENT_3D('',#215524,#35899,#35900);
#30134=AXIS2_PLACEMENT_3D('',#215528,#35903,#35904);
#30135=AXIS2_PLACEMENT_3D('',#215529,#35905,#35906);
#30136=AXIS2_PLACEMENT_3D('',#215530,#35907,#35908);
#30137=AXIS2_PLACEMENT_3D('',#215532,#35909,#35910);
#30138=AXIS2_PLACEMENT_3D('',#215534,#35912,#35913);
#30139=AXIS2_PLACEMENT_3D('',#215538,#35916,#35917);
#30140=AXIS2_PLACEMENT_3D('',#215540,#35918,#35919);
#30141=AXIS2_PLACEMENT_3D('',#215542,#35921,#35922);
#30142=AXIS2_PLACEMENT_3D('',#215546,#35925,#35926);
#30143=AXIS2_PLACEMENT_3D('',#215548,#35927,#35928);
#30144=AXIS2_PLACEMENT_3D('',#215550,#35930,#35931);
#30145=AXIS2_PLACEMENT_3D('',#215554,#35934,#35935);
#30146=AXIS2_PLACEMENT_3D('',#215556,#35936,#35937);
#30147=AXIS2_PLACEMENT_3D('',#215558,#35939,#35940);
#30148=AXIS2_PLACEMENT_3D('',#215562,#35943,#35944);
#30149=AXIS2_PLACEMENT_3D('',#215564,#35945,#35946);
#30150=AXIS2_PLACEMENT_3D('',#215566,#35948,#35949);
#30151=AXIS2_PLACEMENT_3D('',#215570,#35952,#35953);
#30152=AXIS2_PLACEMENT_3D('',#215572,#35954,#35955);
#30153=AXIS2_PLACEMENT_3D('',#215574,#35957,#35958);
#30154=AXIS2_PLACEMENT_3D('',#215578,#35961,#35962);
#30155=AXIS2_PLACEMENT_3D('',#215579,#35963,#35964);
#30156=AXIS2_PLACEMENT_3D('',#215580,#35965,#35966);
#30157=AXIS2_PLACEMENT_3D('',#215581,#35967,#35968);
#30158=AXIS2_PLACEMENT_3D('',#215582,#35969,#35970);
#30159=AXIS2_PLACEMENT_3D('',#215583,#35971,#35972);
#30160=AXIS2_PLACEMENT_3D('',#215584,#35973,#35974);
#30161=AXIS2_PLACEMENT_3D('',#215585,#35975,#35976);
#30162=AXIS2_PLACEMENT_3D('',#215586,#35977,#35978);
#30163=AXIS2_PLACEMENT_3D('',#215587,#35979,#35980);
#30164=DIRECTION('axis',(0.,0.,1.));
#30165=DIRECTION('refdir',(1.,0.,0.));
#30166=DIRECTION('axis',(0.,0.,1.));
#30167=DIRECTION('refdir',(1.,0.,0.));
#30168=DIRECTION('center_axis',(0.,0.,1.));
#30169=DIRECTION('ref_axis',(1.,0.,0.));
#30170=DIRECTION('',(-1.,0.,0.));
#30171=DIRECTION('',(-0.992331937885489,0.123601476740492,0.));
#30172=DIRECTION('',(0.947210277746029,0.320612990585676,0.));
#30173=DIRECTION('center_axis',(0.,0.,1.));
#30174=DIRECTION('ref_axis',(0.320612990585677,-0.947210277746029,0.));
#30175=DIRECTION('',(-0.000226892800803133,0.999999974259828,0.));
#30176=DIRECTION('center_axis',(0.,0.,-1.));
#30177=DIRECTION('ref_axis',(0.341806925031389,0.939770198506308,0.));
#30178=DIRECTION('',(0.939770198506308,-0.341806925031389,0.));
#30179=DIRECTION('center_axis',(0.,0.,-1.));
#30180=DIRECTION('ref_axis',(0.721603167216852,0.692306918254186,0.));
#30181=DIRECTION('',(0.692306918254186,-0.721603167216852,0.));
#30182=DIRECTION('center_axis',(0.,0.,1.));
#30183=DIRECTION('ref_axis',(-0.721603167216849,-0.692306918254189,0.));
#30184=DIRECTION('',(-0.000226892800815894,0.999999974259828,0.));
#30185=DIRECTION('center_axis',(0.,0.,-1.));
#30186=DIRECTION('ref_axis',(-0.000226892800814663,0.999999974259828,0.));
#30187=DIRECTION('',(0.999991534671702,0.00411467920174865,0.));
#30188=DIRECTION('',(0.999991534671702,-0.00411467920174865,0.));
#30189=DIRECTION('center_axis',(0.,0.,-1.));
#30190=DIRECTION('ref_axis',(0.999999974259828,-0.000226892800814664,0.));
#30191=DIRECTION('',(-0.000226892800815894,-0.999999974259828,0.));
#30192=DIRECTION('center_axis',(0.,0.,1.));
#30193=DIRECTION('ref_axis',(-0.999999974259828,0.000226892800815902,0.));
#30194=DIRECTION('',(0.692306918254186,0.721603167216852,0.));
#30195=DIRECTION('center_axis',(0.,0.,-1.));
#30196=DIRECTION('ref_axis',(-0.341806925031389,0.939770198506308,0.));
#30197=DIRECTION('',(0.939770198506308,0.341806925031389,0.));
#30198=DIRECTION('center_axis',(0.,0.,-1.));
#30199=DIRECTION('ref_axis',(0.999999974259828,-0.000226892800803726,0.));
#30200=DIRECTION('',(-0.000226892800803133,-0.999999974259828,0.));
#30201=DIRECTION('center_axis',(0.,0.,1.));
#30202=DIRECTION('ref_axis',(-0.999999974259828,0.000226892800803038,0.));
#30203=DIRECTION('',(0.947210277746029,-0.320612990585676,0.));
#30204=DIRECTION('',(-0.992331937885489,-0.123601476740492,0.));
#30205=DIRECTION('center_axis',(-0.123601476740492,-0.992331937885489,0.));
#30206=DIRECTION('ref_axis',(0.992331937885489,-0.123601476740492,0.));
#30207=DIRECTION('',(0.,0.,-1.));
#30208=DIRECTION('',(0.992331937885489,-0.123601476740492,0.));
#30209=DIRECTION('',(0.,0.,1.));
#30210=DIRECTION('center_axis',(-0.320612990585676,0.947210277746029,0.));
#30211=DIRECTION('ref_axis',(-0.947210277746029,-0.320612990585676,0.));
#30212=DIRECTION('',(-0.947210277746029,-0.320612990585676,0.));
#30213=DIRECTION('',(0.,0.,1.));
#30214=DIRECTION('center_axis',(0.,0.,1.));
#30215=DIRECTION('ref_axis',(0.320612990585677,-0.947210277746029,0.));
#30216=DIRECTION('center_axis',(0.,0.,-1.));
#30217=DIRECTION('ref_axis',(0.320612990585677,-0.947210277746029,0.));
#30218=DIRECTION('',(0.,0.,1.));
#30219=DIRECTION('center_axis',(-0.999999974259828,-0.000226892800803133,
0.));
#30220=DIRECTION('ref_axis',(0.000226892800803133,-0.999999974259828,0.));
#30221=DIRECTION('',(0.000226892800803133,-0.999999974259828,0.));
#30222=DIRECTION('',(0.,0.,1.));
#30223=DIRECTION('center_axis',(0.,0.,1.));
#30224=DIRECTION('ref_axis',(0.341806925031389,0.939770198506308,0.));
#30225=DIRECTION('center_axis',(0.,0.,1.));
#30226=DIRECTION('ref_axis',(0.341806925031389,0.939770198506308,0.));
#30227=DIRECTION('',(0.,0.,1.));
#30228=DIRECTION('center_axis',(0.341806925031389,0.939770198506309,0.));
#30229=DIRECTION('ref_axis',(-0.939770198506308,0.341806925031389,0.));
#30230=DIRECTION('',(-0.939770198506308,0.341806925031389,0.));
#30231=DIRECTION('',(0.,0.,1.));
#30232=DIRECTION('center_axis',(0.,0.,1.));
#30233=DIRECTION('ref_axis',(0.721603167216852,0.692306918254186,0.));
#30234=DIRECTION('center_axis',(0.,0.,1.));
#30235=DIRECTION('ref_axis',(0.721603167216852,0.692306918254186,0.));
#30236=DIRECTION('',(0.,0.,1.));
#30237=DIRECTION('center_axis',(0.721603167216852,0.692306918254186,0.));
#30238=DIRECTION('ref_axis',(-0.692306918254186,0.721603167216852,0.));
#30239=DIRECTION('',(-0.692306918254186,0.721603167216852,0.));
#30240=DIRECTION('',(0.,0.,1.));
#30241=DIRECTION('center_axis',(0.,0.,1.));
#30242=DIRECTION('ref_axis',(-0.721603167216849,-0.692306918254189,0.));
#30243=DIRECTION('center_axis',(0.,0.,-1.));
#30244=DIRECTION('ref_axis',(-0.721603167216849,-0.692306918254189,0.));
#30245=DIRECTION('',(0.,0.,1.));
#30246=DIRECTION('center_axis',(-0.999999974259828,-0.000226892800815894,
0.));
#30247=DIRECTION('ref_axis',(0.000226892800815894,-0.999999974259828,0.));
#30248=DIRECTION('',(0.000226892800815894,-0.999999974259828,0.));
#30249=DIRECTION('',(0.,0.,1.));
#30250=DIRECTION('center_axis',(0.,0.,1.));
#30251=DIRECTION('ref_axis',(-0.000226892800814663,0.999999974259828,0.));
#30252=DIRECTION('center_axis',(0.,0.,1.));
#30253=DIRECTION('ref_axis',(-0.000226892800814663,0.999999974259828,0.));
#30254=DIRECTION('',(0.,0.,1.));
#30255=DIRECTION('center_axis',(-0.00411467920174865,0.999991534671702,
0.));
#30256=DIRECTION('ref_axis',(-0.999991534671703,-0.00411467920174865,0.));
#30257=DIRECTION('',(-0.999991534671702,-0.00411467920174865,0.));
#30258=DIRECTION('',(0.,0.,1.));
#30259=DIRECTION('center_axis',(0.00411467920174865,0.999991534671702,0.));
#30260=DIRECTION('ref_axis',(-0.999991534671703,0.00411467920174865,0.));
#30261=DIRECTION('',(-0.999991534671702,0.00411467920174865,0.));
#30262=DIRECTION('',(0.,0.,1.));
#30263=DIRECTION('center_axis',(0.,0.,1.));
#30264=DIRECTION('ref_axis',(0.999999974259828,-0.000226892800814664,0.));
#30265=DIRECTION('center_axis',(0.,0.,1.));
#30266=DIRECTION('ref_axis',(0.999999974259828,-0.000226892800814664,0.));
#30267=DIRECTION('',(0.,0.,1.));
#30268=DIRECTION('center_axis',(0.999999974259828,-0.000226892800815894,
0.));
#30269=DIRECTION('ref_axis',(0.000226892800815894,0.999999974259828,0.));
#30270=DIRECTION('',(0.000226892800815894,0.999999974259828,0.));
#30271=DIRECTION('',(0.,0.,1.));
#30272=DIRECTION('center_axis',(0.,0.,1.));
#30273=DIRECTION('ref_axis',(-0.999999974259828,0.000226892800815902,0.));
#30274=DIRECTION('center_axis',(0.,0.,-1.));
#30275=DIRECTION('ref_axis',(-0.999999974259828,0.000226892800815902,0.));
#30276=DIRECTION('',(0.,0.,1.));
#30277=DIRECTION('center_axis',(-0.721603167216852,0.692306918254186,0.));
#30278=DIRECTION('ref_axis',(-0.692306918254186,-0.721603167216852,0.));
#30279=DIRECTION('',(-0.692306918254186,-0.721603167216852,0.));
#30280=DIRECTION('',(0.,0.,1.));
#30281=DIRECTION('center_axis',(0.,0.,1.));
#30282=DIRECTION('ref_axis',(-0.341806925031389,0.939770198506308,0.));
#30283=DIRECTION('center_axis',(0.,0.,1.));
#30284=DIRECTION('ref_axis',(-0.341806925031389,0.939770198506308,0.));
#30285=DIRECTION('',(0.,0.,1.));
#30286=DIRECTION('center_axis',(-0.341806925031389,0.939770198506309,0.));
#30287=DIRECTION('ref_axis',(-0.939770198506308,-0.341806925031389,0.));
#30288=DIRECTION('',(-0.939770198506308,-0.341806925031389,0.));
#30289=DIRECTION('',(0.,0.,1.));
#30290=DIRECTION('center_axis',(0.,0.,1.));
#30291=DIRECTION('ref_axis',(0.999999974259828,-0.000226892800803726,0.));
#30292=DIRECTION('center_axis',(0.,0.,1.));
#30293=DIRECTION('ref_axis',(0.999999974259828,-0.000226892800803726,0.));
#30294=DIRECTION('',(0.,0.,1.));
#30295=DIRECTION('center_axis',(0.999999974259828,-0.000226892800803133,
0.));
#30296=DIRECTION('ref_axis',(0.000226892800803133,0.999999974259828,0.));
#30297=DIRECTION('',(0.000226892800803133,0.999999974259828,0.));
#30298=DIRECTION('',(0.,0.,1.));
#30299=DIRECTION('center_axis',(0.,0.,1.));
#30300=DIRECTION('ref_axis',(-0.999999974259828,0.000226892800803038,0.));
#30301=DIRECTION('center_axis',(0.,0.,-1.));
#30302=DIRECTION('ref_axis',(-0.999999974259828,0.000226892800803038,0.));
#30303=DIRECTION('',(0.,0.,1.));
#30304=DIRECTION('center_axis',(0.320612990585676,0.947210277746029,0.));
#30305=DIRECTION('ref_axis',(-0.947210277746029,0.320612990585676,0.));
#30306=DIRECTION('',(-0.947210277746029,0.320612990585676,0.));
#30307=DIRECTION('',(0.,0.,1.));
#30308=DIRECTION('center_axis',(0.123601476740492,-0.992331937885489,0.));
#30309=DIRECTION('ref_axis',(0.992331937885489,0.123601476740492,0.));
#30310=DIRECTION('',(0.992331937885489,0.123601476740492,0.));
#30311=DIRECTION('',(0.,0.,1.));
#30312=DIRECTION('center_axis',(0.,-1.,0.));
#30313=DIRECTION('ref_axis',(1.,0.,0.));
#30314=DIRECTION('',(1.,0.,0.));
#30315=DIRECTION('center_axis',(0.,0.,1.));
#30316=DIRECTION('ref_axis',(1.,0.,0.));
#30317=DIRECTION('axis',(0.,0.,1.));
#30318=DIRECTION('refdir',(1.,0.,0.));
#30319=DIRECTION('center_axis',(0.,0.,1.));
#30320=DIRECTION('ref_axis',(1.,0.,0.));
#30321=DIRECTION('',(0.,1.,0.));
#30322=DIRECTION('center_axis',(0.,0.,1.));
#30323=DIRECTION('ref_axis',(1.,0.,0.));
#30324=DIRECTION('',(-1.,0.,0.));
#30325=DIRECTION('center_axis',(0.,0.,1.));
#30326=DIRECTION('ref_axis',(-1.70908716845004E-15,1.,0.));
#30327=DIRECTION('',(1.88534624677928E-15,-1.,0.));
#30328=DIRECTION('center_axis',(0.,0.,-1.));
#30329=DIRECTION('ref_axis',(-0.721760228098359,-0.69214317387041,0.));
#30330=DIRECTION('',(-0.69214317387041,0.721760228098359,0.));
#30331=DIRECTION('',(-2.36721327212187E-15,1.,0.));
#30332=DIRECTION('',(-1.,-2.72113486427735E-15,0.));
#30333=DIRECTION('',(1.39125692308917E-15,-1.,0.));
#30334=DIRECTION('',(-1.,-1.92080108066636E-15,0.));
#30335=DIRECTION('',(-1.77825364328642E-15,1.,0.));
#30336=DIRECTION('center_axis',(0.,0.,-1.));
#30337=DIRECTION('ref_axis',(-0.268919820615266,0.963162566797658,0.));
#30338=DIRECTION('',(0.963162566797657,0.26891982061527,0.));
#30339=DIRECTION('center_axis',(0.,0.,-1.));
#30340=DIRECTION('ref_axis',(-2.02156751531155E-15,1.,0.));
#30341=DIRECTION('',(1.,0.,0.));
#30342=DIRECTION('center_axis',(0.,0.,-1.));
#30343=DIRECTION('ref_axis',(0.268930215136866,0.963159664534619,0.));
#30344=DIRECTION('',(0.963162566797658,-0.268919820615267,0.));
#30345=DIRECTION('center_axis',(0.,0.,-1.));
#30346=DIRECTION('ref_axis',(1.,0.,0.));
#30347=DIRECTION('',(0.,-1.,0.));
#30348=DIRECTION('',(-1.,0.,0.));
#30349=DIRECTION('',(0.,1.,0.));
#30350=DIRECTION('',(-1.,0.,0.));
#30351=DIRECTION('',(0.,-1.,0.));
#30352=DIRECTION('',(-0.692143173870409,-0.72176022809836,0.));
#30353=DIRECTION('center_axis',(0.,0.,-1.));
#30354=DIRECTION('ref_axis',(-1.,0.,0.));
#30355=DIRECTION('center_axis',(0.,0.,1.));
#30356=DIRECTION('ref_axis',(1.,0.,0.));
#30357=DIRECTION('',(0.,0.,-1.));
#30358=DIRECTION('center_axis',(0.,0.,-1.));
#30359=DIRECTION('ref_axis',(1.,0.,0.));
#30360=DIRECTION('',(0.,0.,1.));
#30361=DIRECTION('center_axis',(0.,-1.,0.));
#30362=DIRECTION('ref_axis',(1.,0.,0.));
#30363=DIRECTION('',(1.,0.,0.));
#30364=DIRECTION('',(0.,0.,1.));
#30365=DIRECTION('center_axis',(0.,0.,1.));
#30366=DIRECTION('ref_axis',(-1.70908716845004E-15,1.,0.));
#30367=DIRECTION('center_axis',(0.,0.,-1.));
#30368=DIRECTION('ref_axis',(-1.70908716845004E-15,1.,0.));
#30369=DIRECTION('',(0.,0.,1.));
#30370=DIRECTION('center_axis',(1.,1.88534624677928E-15,0.));
#30371=DIRECTION('ref_axis',(-1.88534624677928E-15,1.,0.));
#30372=DIRECTION('',(-1.88534624677928E-15,1.,0.));
#30373=DIRECTION('',(0.,0.,1.));
#30374=DIRECTION('center_axis',(0.,0.,1.));
#30375=DIRECTION('ref_axis',(-0.721760228098359,-0.69214317387041,0.));
#30376=DIRECTION('center_axis',(0.,0.,1.));
#30377=DIRECTION('ref_axis',(-0.721760228098359,-0.69214317387041,0.));
#30378=DIRECTION('',(0.,0.,1.));
#30379=DIRECTION('center_axis',(-0.721760228098359,-0.69214317387041,0.));
#30380=DIRECTION('ref_axis',(0.69214317387041,-0.721760228098359,0.));
#30381=DIRECTION('',(0.69214317387041,-0.721760228098359,0.));
#30382=DIRECTION('',(0.,0.,1.));
#30383=DIRECTION('center_axis',(-1.,-2.36721327212187E-15,0.));
#30384=DIRECTION('ref_axis',(2.36721327212187E-15,-1.,0.));
#30385=DIRECTION('',(2.36721327212187E-15,-1.,0.));
#30386=DIRECTION('',(0.,0.,1.));
#30387=DIRECTION('center_axis',(2.72113486427735E-15,-1.,0.));
#30388=DIRECTION('ref_axis',(1.,2.72113486427735E-15,0.));
#30389=DIRECTION('',(1.,2.72113486427735E-15,0.));
#30390=DIRECTION('',(0.,0.,1.));
#30391=DIRECTION('center_axis',(1.,1.39125692308917E-15,0.));
#30392=DIRECTION('ref_axis',(-1.39125692308917E-15,1.,0.));
#30393=DIRECTION('',(-1.39125692308917E-15,1.,0.));
#30394=DIRECTION('',(0.,0.,1.));
#30395=DIRECTION('center_axis',(1.92080108066636E-15,-1.,0.));
#30396=DIRECTION('ref_axis',(1.,1.92080108066636E-15,0.));
#30397=DIRECTION('',(1.,1.92080108066636E-15,0.));
#30398=DIRECTION('',(0.,0.,1.));
#30399=DIRECTION('center_axis',(-1.,-1.77825364328642E-15,0.));
#30400=DIRECTION('ref_axis',(1.77825364328642E-15,-1.,0.));
#30401=DIRECTION('',(1.77825364328642E-15,-1.,0.));
#30402=DIRECTION('',(0.,0.,1.));
#30403=DIRECTION('center_axis',(0.,0.,1.));
#30404=DIRECTION('ref_axis',(-0.268919820615266,0.963162566797658,0.));
#30405=DIRECTION('center_axis',(0.,0.,1.));
#30406=DIRECTION('ref_axis',(-0.268919820615266,0.963162566797658,0.));
#30407=DIRECTION('',(0.,0.,1.));
#30408=DIRECTION('center_axis',(-0.26891982061527,0.963162566797657,0.));
#30409=DIRECTION('ref_axis',(-0.963162566797657,-0.26891982061527,0.));
#30410=DIRECTION('',(-0.963162566797657,-0.26891982061527,0.));
#30411=DIRECTION('',(0.,0.,1.));
#30412=DIRECTION('center_axis',(0.,0.,1.));
#30413=DIRECTION('ref_axis',(-2.02156751531155E-15,1.,0.));
#30414=DIRECTION('center_axis',(0.,0.,1.));
#30415=DIRECTION('ref_axis',(-2.02156751531155E-15,1.,0.));
#30416=DIRECTION('',(0.,0.,1.));
#30417=DIRECTION('center_axis',(0.,1.,0.));
#30418=DIRECTION('ref_axis',(-1.,0.,0.));
#30419=DIRECTION('',(-1.,0.,0.));
#30420=DIRECTION('',(0.,0.,1.));
#30421=DIRECTION('center_axis',(0.,0.,1.));
#30422=DIRECTION('ref_axis',(0.268930215136866,0.963159664534619,0.));
#30423=DIRECTION('center_axis',(0.,0.,1.));
#30424=DIRECTION('ref_axis',(0.268930215136866,0.963159664534619,0.));
#30425=DIRECTION('',(0.,0.,1.));
#30426=DIRECTION('center_axis',(0.268919820615267,0.963162566797658,0.));
#30427=DIRECTION('ref_axis',(-0.963162566797658,0.268919820615267,0.));
#30428=DIRECTION('',(-0.963162566797658,0.268919820615267,0.));
#30429=DIRECTION('',(0.,0.,1.));
#30430=DIRECTION('center_axis',(0.,0.,1.));
#30431=DIRECTION('ref_axis',(1.,0.,0.));
#30432=DIRECTION('center_axis',(0.,0.,1.));
#30433=DIRECTION('ref_axis',(1.,0.,0.));
#30434=DIRECTION('',(0.,0.,1.));
#30435=DIRECTION('center_axis',(1.,0.,0.));
#30436=DIRECTION('ref_axis',(0.,1.,0.));
#30437=DIRECTION('',(0.,1.,0.));
#30438=DIRECTION('',(0.,0.,1.));
#30439=DIRECTION('center_axis',(0.,-1.,0.));
#30440=DIRECTION('ref_axis',(1.,0.,0.));
#30441=DIRECTION('',(1.,0.,0.));
#30442=DIRECTION('',(0.,0.,1.));
#30443=DIRECTION('center_axis',(-1.,0.,0.));
#30444=DIRECTION('ref_axis',(0.,-1.,0.));
#30445=DIRECTION('',(0.,-1.,0.));
#30446=DIRECTION('',(0.,0.,1.));
#30447=DIRECTION('center_axis',(0.,-1.,0.));
#30448=DIRECTION('ref_axis',(1.,0.,0.));
#30449=DIRECTION('',(1.,0.,0.));
#30450=DIRECTION('',(0.,0.,1.));
#30451=DIRECTION('center_axis',(1.,0.,0.));
#30452=DIRECTION('ref_axis',(0.,1.,0.));
#30453=DIRECTION('',(0.,1.,0.));
#30454=DIRECTION('',(0.,0.,1.));
#30455=DIRECTION('center_axis',(0.72176022809836,-0.692143173870409,0.));
#30456=DIRECTION('ref_axis',(0.692143173870409,0.72176022809836,0.));
#30457=DIRECTION('',(0.692143173870409,0.72176022809836,0.));
#30458=DIRECTION('',(0.,0.,1.));
#30459=DIRECTION('center_axis',(0.,0.,1.));
#30460=DIRECTION('ref_axis',(-1.,0.,0.));
#30461=DIRECTION('center_axis',(0.,0.,1.));
#30462=DIRECTION('ref_axis',(-1.,0.,0.));
#30463=DIRECTION('',(0.,0.,1.));
#30464=DIRECTION('center_axis',(-1.,0.,0.));
#30465=DIRECTION('ref_axis',(0.,-1.,0.));
#30466=DIRECTION('',(0.,-1.,0.));
#30467=DIRECTION('center_axis',(0.,0.,1.));
#30468=DIRECTION('ref_axis',(1.,0.,0.));
#30469=DIRECTION('axis',(0.,0.,1.));
#30470=DIRECTION('refdir',(1.,0.,0.));
#30471=DIRECTION('center_axis',(1.,0.,0.));
#30472=DIRECTION('ref_axis',(0.,-0.793547993282919,-0.608507668280895));
#30473=DIRECTION('',(1.,0.,0.));
#30474=DIRECTION('center_axis',(-1.,0.,0.));
#30475=DIRECTION('ref_axis',(0.,-1.74186785585433E-15,1.));
#30476=DIRECTION('center_axis',(1.,0.,0.));
#30477=DIRECTION('ref_axis',(0.,-0.793547993282919,-0.608507668280895));
#30478=DIRECTION('',(1.,0.,0.));
#30479=DIRECTION('center_axis',(1.,0.,0.));
#30480=DIRECTION('ref_axis',(0.,-0.793547993282919,-0.608507668280895));
#30481=DIRECTION('',(1.,0.,0.));
#30482=DIRECTION('center_axis',(1.,0.,0.));
#30483=DIRECTION('ref_axis',(0.,-0.793547993282919,-0.608507668280895));
#30484=DIRECTION('',(1.,0.,0.));
#30485=DIRECTION('center_axis',(1.,0.,0.));
#30486=DIRECTION('ref_axis',(0.,-1.74186785585433E-15,1.));
#30487=DIRECTION('center_axis',(-1.,0.,0.));
#30488=DIRECTION('ref_axis',(0.,0.793547993033681,-0.608507668605924));
#30489=DIRECTION('',(-1.,0.,0.));
#30490=DIRECTION('center_axis',(1.,0.,0.));
#30491=DIRECTION('ref_axis',(0.,-1.74186785585433E-15,1.));
#30492=DIRECTION('center_axis',(-1.,0.,0.));
#30493=DIRECTION('ref_axis',(0.,0.793547993033681,-0.608507668605924));
#30494=DIRECTION('',(-1.,0.,0.));
#30495=DIRECTION('center_axis',(-1.,0.,0.));
#30496=DIRECTION('ref_axis',(0.,0.793547993033681,-0.608507668605924));
#30497=DIRECTION('',(-1.,0.,0.));
#30498=DIRECTION('center_axis',(-1.,0.,0.));
#30499=DIRECTION('ref_axis',(0.,0.793547993033681,-0.608507668605924));
#30500=DIRECTION('',(-1.,0.,0.));
#30501=DIRECTION('center_axis',(-1.,0.,0.));
#30502=DIRECTION('ref_axis',(0.,-1.74186785585433E-15,1.));
#30503=DIRECTION('center_axis',(0.,0.,-1.));
#30504=DIRECTION('ref_axis',(-0.609193654691519,-0.793021494717256,0.));
#30505=DIRECTION('',(0.,0.,-1.));
#30506=DIRECTION('center_axis',(0.,0.,1.));
#30507=DIRECTION('ref_axis',(1.,8.06646416329218E-14,0.));
#30508=DIRECTION('center_axis',(0.,0.,-1.));
#30509=DIRECTION('ref_axis',(-0.609193654691519,-0.793021494717256,0.));
#30510=DIRECTION('',(0.,0.,-1.));
#30511=DIRECTION('center_axis',(0.,0.,-1.));
#30512=DIRECTION('ref_axis',(-0.609193654691519,-0.793021494717256,0.));
#30513=DIRECTION('',(0.,0.,-1.));
#30514=DIRECTION('center_axis',(0.,0.,-1.));
#30515=DIRECTION('ref_axis',(-0.609193654691519,-0.793021494717256,0.));
#30516=DIRECTION('',(0.,0.,-1.));
#30517=DIRECTION('center_axis',(0.,0.,-1.));
#30518=DIRECTION('ref_axis',(-0.609193654691519,-0.793021494717256,0.));
#30519=DIRECTION('',(0.,0.,-1.));
#30520=DIRECTION('center_axis',(0.,0.,-1.));
#30521=DIRECTION('ref_axis',(-0.609193654691519,-0.793021494717256,0.));
#30522=DIRECTION('',(0.,0.,-1.));
#30523=DIRECTION('center_axis',(0.,0.,-1.));
#30524=DIRECTION('ref_axis',(-0.609193654691519,-0.793021494717256,0.));
#30525=DIRECTION('',(0.,0.,-1.));
#30526=DIRECTION('center_axis',(0.,0.,-1.));
#30527=DIRECTION('ref_axis',(-0.609193654691519,-0.793021494717256,0.));
#30528=DIRECTION('',(0.,0.,-1.));
#30529=DIRECTION('center_axis',(0.,0.,-1.));
#30530=DIRECTION('ref_axis',(-0.609193654691519,-0.793021494717256,0.));
#30531=DIRECTION('',(0.,0.,-1.));
#30532=DIRECTION('center_axis',(0.,0.,-1.));
#30533=DIRECTION('ref_axis',(-0.609193654691519,-0.793021494717256,0.));
#30534=DIRECTION('',(0.,0.,-1.));
#30535=DIRECTION('center_axis',(0.,0.,-1.));
#30536=DIRECTION('ref_axis',(-0.609193654691519,-0.793021494717256,0.));
#30537=DIRECTION('',(0.,0.,-1.));
#30538=DIRECTION('center_axis',(0.,0.,-1.));
#30539=DIRECTION('ref_axis',(-0.609193654691519,-0.793021494717256,0.));
#30540=DIRECTION('',(0.,0.,-1.));
#30541=DIRECTION('center_axis',(0.,0.,-1.));
#30542=DIRECTION('ref_axis',(-0.609193654691519,-0.793021494717256,0.));
#30543=DIRECTION('',(0.,0.,-1.));
#30544=DIRECTION('center_axis',(0.,0.,-1.));
#30545=DIRECTION('ref_axis',(-0.609193654691519,-0.793021494717256,0.));
#30546=DIRECTION('',(0.,0.,-1.));
#30547=DIRECTION('center_axis',(0.,0.,-1.));
#30548=DIRECTION('ref_axis',(-0.609193654691519,-0.793021494717256,0.));
#30549=DIRECTION('',(0.,0.,-1.));
#30550=DIRECTION('center_axis',(0.,0.,-1.));
#30551=DIRECTION('ref_axis',(-0.609193654691519,-0.793021494717256,0.));
#30552=DIRECTION('',(0.,0.,-1.));
#30553=DIRECTION('center_axis',(0.,0.,-1.));
#30554=DIRECTION('ref_axis',(-0.609193654691519,-0.793021494717256,0.));
#30555=DIRECTION('',(0.,0.,-1.));
#30556=DIRECTION('center_axis',(0.,0.,-1.));
#30557=DIRECTION('ref_axis',(-0.609193654691519,-0.793021494717256,0.));
#30558=DIRECTION('',(0.,0.,-1.));
#30559=DIRECTION('center_axis',(0.,0.,-1.));
#30560=DIRECTION('ref_axis',(-0.609193654691519,-0.793021494717256,0.));
#30561=DIRECTION('',(0.,0.,-1.));
#30562=DIRECTION('center_axis',(0.,0.,-1.));
#30563=DIRECTION('ref_axis',(-0.609193654691519,-0.793021494717256,0.));
#30564=DIRECTION('',(0.,0.,-1.));
#30565=DIRECTION('center_axis',(0.,0.,-1.));
#30566=DIRECTION('ref_axis',(-0.609193654691519,-0.793021494717256,0.));
#30567=DIRECTION('',(0.,0.,-1.));
#30568=DIRECTION('center_axis',(0.,0.,-1.));
#30569=DIRECTION('ref_axis',(-0.609193654691519,-0.793021494717256,0.));
#30570=DIRECTION('',(0.,0.,-1.));
#30571=DIRECTION('center_axis',(0.,0.,-1.));
#30572=DIRECTION('ref_axis',(-0.609193654691519,-0.793021494717256,0.));
#30573=DIRECTION('',(0.,0.,-1.));
#30574=DIRECTION('center_axis',(0.,0.,-1.));
#30575=DIRECTION('ref_axis',(-0.609193654691519,-0.793021494717256,0.));
#30576=DIRECTION('',(0.,0.,-1.));
#30577=DIRECTION('center_axis',(0.,0.,-1.));
#30578=DIRECTION('ref_axis',(-0.609193654691519,-0.793021494717256,0.));
#30579=DIRECTION('',(0.,0.,-1.));
#30580=DIRECTION('center_axis',(0.,0.,-1.));
#30581=DIRECTION('ref_axis',(-0.609193654691519,-0.793021494717256,0.));
#30582=DIRECTION('',(0.,0.,-1.));
#30583=DIRECTION('center_axis',(0.,0.,-1.));
#30584=DIRECTION('ref_axis',(-0.609193654691519,-0.793021494717256,0.));
#30585=DIRECTION('',(0.,0.,-1.));
#30586=DIRECTION('center_axis',(0.,0.,-1.));
#30587=DIRECTION('ref_axis',(1.,8.06646416329218E-14,0.));
#30588=DIRECTION('center_axis',(0.,0.,-1.));
#30589=DIRECTION('ref_axis',(-0.609193705300279,-0.793021455839952,0.));
#30590=DIRECTION('',(0.,0.,-1.));
#30591=DIRECTION('center_axis',(0.,0.,1.));
#30592=DIRECTION('ref_axis',(1.,8.15320033709099E-14,0.));
#30593=DIRECTION('center_axis',(0.,0.,-1.));
#30594=DIRECTION('ref_axis',(-0.609193705300279,-0.793021455839952,0.));
#30595=DIRECTION('',(0.,0.,-1.));
#30596=DIRECTION('center_axis',(0.,0.,-1.));
#30597=DIRECTION('ref_axis',(-0.609193705300279,-0.793021455839952,0.));
#30598=DIRECTION('',(0.,0.,-1.));
#30599=DIRECTION('center_axis',(0.,0.,-1.));
#30600=DIRECTION('ref_axis',(-0.609193705300279,-0.793021455839952,0.));
#30601=DIRECTION('',(0.,0.,-1.));
#30602=DIRECTION('center_axis',(0.,0.,-1.));
#30603=DIRECTION('ref_axis',(-0.609193705300279,-0.793021455839952,0.));
#30604=DIRECTION('',(0.,0.,-1.));
#30605=DIRECTION('center_axis',(0.,0.,-1.));
#30606=DIRECTION('ref_axis',(-0.609193705300279,-0.793021455839952,0.));
#30607=DIRECTION('',(0.,0.,-1.));
#30608=DIRECTION('center_axis',(0.,0.,-1.));
#30609=DIRECTION('ref_axis',(-0.609193705300279,-0.793021455839952,0.));
#30610=DIRECTION('',(0.,0.,-1.));
#30611=DIRECTION('center_axis',(0.,0.,-1.));
#30612=DIRECTION('ref_axis',(-0.609193705300279,-0.793021455839952,0.));
#30613=DIRECTION('',(0.,0.,-1.));
#30614=DIRECTION('center_axis',(0.,0.,-1.));
#30615=DIRECTION('ref_axis',(-0.609193705300279,-0.793021455839952,0.));
#30616=DIRECTION('',(0.,0.,-1.));
#30617=DIRECTION('center_axis',(0.,0.,-1.));
#30618=DIRECTION('ref_axis',(-0.609193705300279,-0.793021455839952,0.));
#30619=DIRECTION('',(0.,0.,-1.));
#30620=DIRECTION('center_axis',(0.,0.,-1.));
#30621=DIRECTION('ref_axis',(-0.609193705300279,-0.793021455839952,0.));
#30622=DIRECTION('',(0.,0.,-1.));
#30623=DIRECTION('center_axis',(0.,0.,-1.));
#30624=DIRECTION('ref_axis',(-0.609193705300279,-0.793021455839952,0.));
#30625=DIRECTION('',(0.,0.,-1.));
#30626=DIRECTION('center_axis',(0.,0.,-1.));
#30627=DIRECTION('ref_axis',(-0.609193705300279,-0.793021455839952,0.));
#30628=DIRECTION('',(0.,0.,-1.));
#30629=DIRECTION('center_axis',(0.,0.,-1.));
#30630=DIRECTION('ref_axis',(-0.609193705300279,-0.793021455839952,0.));
#30631=DIRECTION('',(0.,0.,-1.));
#30632=DIRECTION('center_axis',(0.,0.,-1.));
#30633=DIRECTION('ref_axis',(-0.609193705300279,-0.793021455839952,0.));
#30634=DIRECTION('',(0.,0.,-1.));
#30635=DIRECTION('center_axis',(0.,0.,-1.));
#30636=DIRECTION('ref_axis',(-0.609193705300279,-0.793021455839952,0.));
#30637=DIRECTION('',(0.,0.,-1.));
#30638=DIRECTION('center_axis',(0.,0.,-1.));
#30639=DIRECTION('ref_axis',(-0.609193705300279,-0.793021455839952,0.));
#30640=DIRECTION('',(0.,0.,-1.));
#30641=DIRECTION('center_axis',(0.,0.,-1.));
#30642=DIRECTION('ref_axis',(-0.609193705300279,-0.793021455839952,0.));
#30643=DIRECTION('',(0.,0.,-1.));
#30644=DIRECTION('center_axis',(0.,0.,-1.));
#30645=DIRECTION('ref_axis',(-0.609193705300279,-0.793021455839952,0.));
#30646=DIRECTION('',(0.,0.,-1.));
#30647=DIRECTION('center_axis',(0.,0.,-1.));
#30648=DIRECTION('ref_axis',(-0.609193705300279,-0.793021455839952,0.));
#30649=DIRECTION('',(0.,0.,-1.));
#30650=DIRECTION('center_axis',(0.,0.,-1.));
#30651=DIRECTION('ref_axis',(-0.609193705300279,-0.793021455839952,0.));
#30652=DIRECTION('',(0.,0.,-1.));
#30653=DIRECTION('center_axis',(0.,0.,-1.));
#30654=DIRECTION('ref_axis',(-0.609193705300279,-0.793021455839952,0.));
#30655=DIRECTION('',(0.,0.,-1.));
#30656=DIRECTION('center_axis',(0.,0.,-1.));
#30657=DIRECTION('ref_axis',(-0.609193705300279,-0.793021455839952,0.));
#30658=DIRECTION('',(0.,0.,-1.));
#30659=DIRECTION('center_axis',(0.,0.,-1.));
#30660=DIRECTION('ref_axis',(-0.609193705300279,-0.793021455839952,0.));
#30661=DIRECTION('',(0.,0.,-1.));
#30662=DIRECTION('center_axis',(0.,0.,-1.));
#30663=DIRECTION('ref_axis',(-0.609193705300279,-0.793021455839952,0.));
#30664=DIRECTION('',(0.,0.,-1.));
#30665=DIRECTION('center_axis',(0.,0.,-1.));
#30666=DIRECTION('ref_axis',(-0.609193705300279,-0.793021455839952,0.));
#30667=DIRECTION('',(0.,0.,-1.));
#30668=DIRECTION('center_axis',(0.,0.,-1.));
#30669=DIRECTION('ref_axis',(-0.609193705300279,-0.793021455839952,0.));
#30670=DIRECTION('',(0.,0.,-1.));
#30671=DIRECTION('center_axis',(0.,0.,-1.));
#30672=DIRECTION('ref_axis',(1.,8.15320033709099E-14,0.));
#30673=DIRECTION('center_axis',(0.,0.,-1.));
#30674=DIRECTION('ref_axis',(-0.609193706391024,-0.793021455002049,0.));
#30675=DIRECTION('',(0.,0.,-1.));
#30676=DIRECTION('center_axis',(0.,0.,1.));
#30677=DIRECTION('ref_axis',(1.,7.80625564189562E-14,0.));
#30678=DIRECTION('center_axis',(0.,0.,-1.));
#30679=DIRECTION('ref_axis',(-0.609193706391024,-0.793021455002049,0.));
#30680=DIRECTION('',(0.,0.,-1.));
#30681=DIRECTION('center_axis',(0.,0.,-1.));
#30682=DIRECTION('ref_axis',(-0.609193706391024,-0.793021455002049,0.));
#30683=DIRECTION('',(0.,0.,-1.));
#30684=DIRECTION('center_axis',(0.,0.,-1.));
#30685=DIRECTION('ref_axis',(-0.609193706391024,-0.793021455002049,0.));
#30686=DIRECTION('',(0.,0.,-1.));
#30687=DIRECTION('center_axis',(0.,0.,-1.));
#30688=DIRECTION('ref_axis',(-0.609193706391024,-0.793021455002049,0.));
#30689=DIRECTION('',(0.,0.,-1.));
#30690=DIRECTION('center_axis',(0.,0.,-1.));
#30691=DIRECTION('ref_axis',(-0.609193706391024,-0.793021455002049,0.));
#30692=DIRECTION('',(0.,0.,-1.));
#30693=DIRECTION('center_axis',(0.,0.,-1.));
#30694=DIRECTION('ref_axis',(-0.609193706391024,-0.793021455002049,0.));
#30695=DIRECTION('',(0.,0.,-1.));
#30696=DIRECTION('center_axis',(0.,0.,-1.));
#30697=DIRECTION('ref_axis',(-0.609193706391024,-0.793021455002049,0.));
#30698=DIRECTION('',(0.,0.,-1.));
#30699=DIRECTION('center_axis',(0.,0.,-1.));
#30700=DIRECTION('ref_axis',(-0.609193706391024,-0.793021455002049,0.));
#30701=DIRECTION('',(0.,0.,-1.));
#30702=DIRECTION('center_axis',(0.,0.,-1.));
#30703=DIRECTION('ref_axis',(-0.609193706391024,-0.793021455002049,0.));
#30704=DIRECTION('',(0.,0.,-1.));
#30705=DIRECTION('center_axis',(0.,0.,-1.));
#30706=DIRECTION('ref_axis',(-0.609193706391024,-0.793021455002049,0.));
#30707=DIRECTION('',(0.,0.,-1.));
#30708=DIRECTION('center_axis',(0.,0.,-1.));
#30709=DIRECTION('ref_axis',(-0.609193706391024,-0.793021455002049,0.));
#30710=DIRECTION('',(0.,0.,-1.));
#30711=DIRECTION('center_axis',(0.,0.,-1.));
#30712=DIRECTION('ref_axis',(-0.609193706391024,-0.793021455002049,0.));
#30713=DIRECTION('',(0.,0.,-1.));
#30714=DIRECTION('center_axis',(0.,0.,-1.));
#30715=DIRECTION('ref_axis',(-0.609193706391024,-0.793021455002049,0.));
#30716=DIRECTION('',(0.,0.,-1.));
#30717=DIRECTION('center_axis',(0.,0.,-1.));
#30718=DIRECTION('ref_axis',(-0.609193706391024,-0.793021455002049,0.));
#30719=DIRECTION('',(0.,0.,-1.));
#30720=DIRECTION('center_axis',(0.,0.,-1.));
#30721=DIRECTION('ref_axis',(-0.609193706391024,-0.793021455002049,0.));
#30722=DIRECTION('',(0.,0.,-1.));
#30723=DIRECTION('center_axis',(0.,0.,-1.));
#30724=DIRECTION('ref_axis',(-0.609193706391024,-0.793021455002049,0.));
#30725=DIRECTION('',(0.,0.,-1.));
#30726=DIRECTION('center_axis',(0.,0.,-1.));
#30727=DIRECTION('ref_axis',(-0.609193706391024,-0.793021455002049,0.));
#30728=DIRECTION('',(0.,0.,-1.));
#30729=DIRECTION('center_axis',(0.,0.,-1.));
#30730=DIRECTION('ref_axis',(-0.609193706391024,-0.793021455002049,0.));
#30731=DIRECTION('',(0.,0.,-1.));
#30732=DIRECTION('center_axis',(0.,0.,-1.));
#30733=DIRECTION('ref_axis',(-0.609193706391024,-0.793021455002049,0.));
#30734=DIRECTION('',(0.,0.,-1.));
#30735=DIRECTION('center_axis',(0.,0.,-1.));
#30736=DIRECTION('ref_axis',(-0.609193706391024,-0.793021455002049,0.));
#30737=DIRECTION('',(0.,0.,-1.));
#30738=DIRECTION('center_axis',(0.,0.,-1.));
#30739=DIRECTION('ref_axis',(-0.609193706391024,-0.793021455002049,0.));
#30740=DIRECTION('',(0.,0.,-1.));
#30741=DIRECTION('center_axis',(0.,0.,-1.));
#30742=DIRECTION('ref_axis',(-0.609193706391024,-0.793021455002049,0.));
#30743=DIRECTION('',(0.,0.,-1.));
#30744=DIRECTION('center_axis',(0.,0.,-1.));
#30745=DIRECTION('ref_axis',(-0.609193706391024,-0.793021455002049,0.));
#30746=DIRECTION('',(0.,0.,-1.));
#30747=DIRECTION('center_axis',(0.,0.,-1.));
#30748=DIRECTION('ref_axis',(-0.609193706391024,-0.793021455002049,0.));
#30749=DIRECTION('',(0.,0.,-1.));
#30750=DIRECTION('center_axis',(0.,0.,-1.));
#30751=DIRECTION('ref_axis',(-0.609193706391024,-0.793021455002049,0.));
#30752=DIRECTION('',(0.,0.,-1.));
#30753=DIRECTION('center_axis',(0.,0.,-1.));
#30754=DIRECTION('ref_axis',(-0.609193706391024,-0.793021455002049,0.));
#30755=DIRECTION('',(0.,0.,-1.));
#30756=DIRECTION('center_axis',(0.,0.,-1.));
#30757=DIRECTION('ref_axis',(1.,7.80625564189563E-14,0.));
#30758=DIRECTION('center_axis',(0.,0.,-1.));
#30759=DIRECTION('ref_axis',(-0.60919368949553,-0.793021467981053,0.));
#30760=DIRECTION('',(0.,0.,-1.));
#30761=DIRECTION('center_axis',(0.,0.,1.));
#30762=DIRECTION('ref_axis',(1.,7.89299181569448E-14,0.));
#30763=DIRECTION('center_axis',(0.,0.,-1.));
#30764=DIRECTION('ref_axis',(-0.60919368949553,-0.793021467981053,0.));
#30765=DIRECTION('',(0.,0.,-1.));
#30766=DIRECTION('center_axis',(0.,0.,-1.));
#30767=DIRECTION('ref_axis',(-0.60919368949553,-0.793021467981053,0.));
#30768=DIRECTION('',(0.,0.,-1.));
#30769=DIRECTION('center_axis',(0.,0.,-1.));
#30770=DIRECTION('ref_axis',(-0.60919368949553,-0.793021467981053,0.));
#30771=DIRECTION('',(0.,0.,-1.));
#30772=DIRECTION('center_axis',(0.,0.,-1.));
#30773=DIRECTION('ref_axis',(-0.60919368949553,-0.793021467981053,0.));
#30774=DIRECTION('',(0.,0.,-1.));
#30775=DIRECTION('center_axis',(0.,0.,-1.));
#30776=DIRECTION('ref_axis',(-0.60919368949553,-0.793021467981053,0.));
#30777=DIRECTION('',(0.,0.,-1.));
#30778=DIRECTION('center_axis',(0.,0.,-1.));
#30779=DIRECTION('ref_axis',(-0.60919368949553,-0.793021467981053,0.));
#30780=DIRECTION('',(0.,0.,-1.));
#30781=DIRECTION('center_axis',(0.,0.,-1.));
#30782=DIRECTION('ref_axis',(-0.60919368949553,-0.793021467981053,0.));
#30783=DIRECTION('',(0.,0.,-1.));
#30784=DIRECTION('center_axis',(0.,0.,-1.));
#30785=DIRECTION('ref_axis',(-0.60919368949553,-0.793021467981053,0.));
#30786=DIRECTION('',(0.,0.,-1.));
#30787=DIRECTION('center_axis',(0.,0.,-1.));
#30788=DIRECTION('ref_axis',(-0.60919368949553,-0.793021467981053,0.));
#30789=DIRECTION('',(0.,0.,-1.));
#30790=DIRECTION('center_axis',(0.,0.,-1.));
#30791=DIRECTION('ref_axis',(-0.60919368949553,-0.793021467981053,0.));
#30792=DIRECTION('',(0.,0.,-1.));
#30793=DIRECTION('center_axis',(0.,0.,-1.));
#30794=DIRECTION('ref_axis',(-0.60919368949553,-0.793021467981053,0.));
#30795=DIRECTION('',(0.,0.,-1.));
#30796=DIRECTION('center_axis',(0.,0.,-1.));
#30797=DIRECTION('ref_axis',(-0.60919368949553,-0.793021467981053,0.));
#30798=DIRECTION('',(0.,0.,-1.));
#30799=DIRECTION('center_axis',(0.,0.,-1.));
#30800=DIRECTION('ref_axis',(-0.60919368949553,-0.793021467981053,0.));
#30801=DIRECTION('',(0.,0.,-1.));
#30802=DIRECTION('center_axis',(0.,0.,-1.));
#30803=DIRECTION('ref_axis',(-0.60919368949553,-0.793021467981053,0.));
#30804=DIRECTION('',(0.,0.,-1.));
#30805=DIRECTION('center_axis',(0.,0.,-1.));
#30806=DIRECTION('ref_axis',(-0.60919368949553,-0.793021467981053,0.));
#30807=DIRECTION('',(0.,0.,-1.));
#30808=DIRECTION('center_axis',(0.,0.,-1.));
#30809=DIRECTION('ref_axis',(-0.60919368949553,-0.793021467981053,0.));
#30810=DIRECTION('',(0.,0.,-1.));
#30811=DIRECTION('center_axis',(0.,0.,-1.));
#30812=DIRECTION('ref_axis',(-0.60919368949553,-0.793021467981053,0.));
#30813=DIRECTION('',(0.,0.,-1.));
#30814=DIRECTION('center_axis',(0.,0.,-1.));
#30815=DIRECTION('ref_axis',(-0.60919368949553,-0.793021467981053,0.));
#30816=DIRECTION('',(0.,0.,-1.));
#30817=DIRECTION('center_axis',(0.,0.,-1.));
#30818=DIRECTION('ref_axis',(-0.60919368949553,-0.793021467981053,0.));
#30819=DIRECTION('',(0.,0.,-1.));
#30820=DIRECTION('center_axis',(0.,0.,-1.));
#30821=DIRECTION('ref_axis',(-0.60919368949553,-0.793021467981053,0.));
#30822=DIRECTION('',(0.,0.,-1.));
#30823=DIRECTION('center_axis',(0.,0.,-1.));
#30824=DIRECTION('ref_axis',(-0.60919368949553,-0.793021467981053,0.));
#30825=DIRECTION('',(0.,0.,-1.));
#30826=DIRECTION('center_axis',(0.,0.,-1.));
#30827=DIRECTION('ref_axis',(-0.60919368949553,-0.793021467981053,0.));
#30828=DIRECTION('',(0.,0.,-1.));
#30829=DIRECTION('center_axis',(0.,0.,-1.));
#30830=DIRECTION('ref_axis',(-0.60919368949553,-0.793021467981053,0.));
#30831=DIRECTION('',(0.,0.,-1.));
#30832=DIRECTION('center_axis',(0.,0.,-1.));
#30833=DIRECTION('ref_axis',(-0.60919368949553,-0.793021467981053,0.));
#30834=DIRECTION('',(0.,0.,-1.));
#30835=DIRECTION('center_axis',(0.,0.,-1.));
#30836=DIRECTION('ref_axis',(-0.60919368949553,-0.793021467981053,0.));
#30837=DIRECTION('',(0.,0.,-1.));
#30838=DIRECTION('center_axis',(0.,0.,-1.));
#30839=DIRECTION('ref_axis',(-0.60919368949553,-0.793021467981053,0.));
#30840=DIRECTION('',(0.,0.,-1.));
#30841=DIRECTION('center_axis',(0.,0.,-1.));
#30842=DIRECTION('ref_axis',(1.,7.89299181569448E-14,0.));
#30843=DIRECTION('center_axis',(1.,0.,0.));
#30844=DIRECTION('ref_axis',(0.,0.509892606676753,0.860238065686695));
#30845=DIRECTION('',(1.,0.,0.));
#30846=DIRECTION('center_axis',(-1.,0.,0.));
#30847=DIRECTION('ref_axis',(0.,0.,1.));
#30848=DIRECTION('center_axis',(1.,0.,0.));
#30849=DIRECTION('ref_axis',(0.,0.349194145719507,0.93705039810846));
#30850=DIRECTION('',(1.,0.,0.));
#30851=DIRECTION('center_axis',(1.,0.,0.));
#30852=DIRECTION('ref_axis',(0.,0.349194145719507,0.93705039810846));
#30853=DIRECTION('',(1.,0.,0.));
#30854=DIRECTION('center_axis',(1.,0.,0.));
#30855=DIRECTION('ref_axis',(0.,0.349194145719507,0.93705039810846));
#30856=DIRECTION('',(1.,0.,0.));
#30857=DIRECTION('center_axis',(-1.,0.,0.));
#30858=DIRECTION('ref_axis',(0.,0.,1.));
#30859=DIRECTION('center_axis',(1.,0.,0.));
#30860=DIRECTION('ref_axis',(0.,-0.349194147217983,0.937050397550049));
#30861=DIRECTION('',(1.,0.,0.));
#30862=DIRECTION('center_axis',(1.,0.,0.));
#30863=DIRECTION('ref_axis',(0.,0.,1.));
#30864=DIRECTION('center_axis',(1.,0.,0.));
#30865=DIRECTION('ref_axis',(0.,-0.349194147217983,0.937050397550049));
#30866=DIRECTION('',(1.,0.,0.));
#30867=DIRECTION('center_axis',(1.,0.,0.));
#30868=DIRECTION('ref_axis',(0.,0.,1.));
#30869=DIRECTION('center_axis',(1.,0.,0.));
#30870=DIRECTION('ref_axis',(0.,-0.349194147217983,0.937050397550049));
#30871=DIRECTION('',(1.,0.,0.));
#30872=DIRECTION('center_axis',(1.,0.,0.));
#30873=DIRECTION('ref_axis',(0.,-0.509892608781802,0.86023806443896));
#30874=DIRECTION('',(1.,0.,0.));
#30875=DIRECTION('center_axis',(1.,0.,0.));
#30876=DIRECTION('ref_axis',(0.,0.,1.));
#30877=DIRECTION('center_axis',(0.,0.,-1.));
#30878=DIRECTION('ref_axis',(0.939338961794584,0.342990254751753,0.));
#30879=DIRECTION('',(0.,0.,-1.));
#30880=DIRECTION('center_axis',(0.,0.,1.));
#30881=DIRECTION('ref_axis',(1.,0.,0.));
#30882=DIRECTION('center_axis',(0.,0.,-1.));
#30883=DIRECTION('ref_axis',(0.939338961794584,0.342990254751753,0.));
#30884=DIRECTION('',(0.,0.,-1.));
#30885=DIRECTION('center_axis',(0.,0.,-1.));
#30886=DIRECTION('ref_axis',(0.939338961794584,0.342990254751753,0.));
#30887=DIRECTION('',(0.,0.,-1.));
#30888=DIRECTION('center_axis',(0.,0.,-1.));
#30889=DIRECTION('ref_axis',(0.939338961794584,0.342990254751753,0.));
#30890=DIRECTION('',(0.,0.,-1.));
#30891=DIRECTION('center_axis',(0.,0.,-1.));
#30892=DIRECTION('ref_axis',(0.939338961794584,0.342990254751753,0.));
#30893=DIRECTION('',(0.,0.,-1.));
#30894=DIRECTION('center_axis',(0.,0.,-1.));
#30895=DIRECTION('ref_axis',(0.939338961794584,0.342990254751753,0.));
#30896=DIRECTION('',(0.,0.,-1.));
#30897=DIRECTION('center_axis',(0.,0.,-1.));
#30898=DIRECTION('ref_axis',(0.939338961794584,0.342990254751753,0.));
#30899=DIRECTION('',(0.,0.,-1.));
#30900=DIRECTION('center_axis',(0.,0.,-1.));
#30901=DIRECTION('ref_axis',(0.939338961794584,0.342990254751753,0.));
#30902=DIRECTION('',(0.,0.,-1.));
#30903=DIRECTION('center_axis',(0.,0.,-1.));
#30904=DIRECTION('ref_axis',(0.939338961794584,0.342990254751753,0.));
#30905=DIRECTION('',(0.,0.,-1.));
#30906=DIRECTION('center_axis',(0.,0.,-1.));
#30907=DIRECTION('ref_axis',(0.939338961794584,0.342990254751753,0.));
#30908=DIRECTION('',(0.,0.,-1.));
#30909=DIRECTION('center_axis',(0.,0.,-1.));
#30910=DIRECTION('ref_axis',(0.939338961794584,0.342990254751753,0.));
#30911=DIRECTION('',(0.,0.,-1.));
#30912=DIRECTION('center_axis',(0.,0.,-1.));
#30913=DIRECTION('ref_axis',(0.939338961794584,0.342990254751753,0.));
#30914=DIRECTION('',(0.,0.,-1.));
#30915=DIRECTION('center_axis',(0.,0.,-1.));
#30916=DIRECTION('ref_axis',(0.939338961794584,0.342990254751753,0.));
#30917=DIRECTION('',(0.,0.,-1.));
#30918=DIRECTION('center_axis',(0.,0.,-1.));
#30919=DIRECTION('ref_axis',(0.939338961794584,0.342990254751753,0.));
#30920=DIRECTION('',(0.,0.,-1.));
#30921=DIRECTION('center_axis',(0.,0.,-1.));
#30922=DIRECTION('ref_axis',(0.939338961794584,0.342990254751753,0.));
#30923=DIRECTION('',(0.,0.,-1.));
#30924=DIRECTION('center_axis',(0.,0.,-1.));
#30925=DIRECTION('ref_axis',(0.939338961794584,0.342990254751753,0.));
#30926=DIRECTION('',(0.,0.,-1.));
#30927=DIRECTION('center_axis',(0.,0.,-1.));
#30928=DIRECTION('ref_axis',(0.939338961794584,0.342990254751753,0.));
#30929=DIRECTION('',(0.,0.,-1.));
#30930=DIRECTION('center_axis',(0.,0.,-1.));
#30931=DIRECTION('ref_axis',(0.939338961794584,0.342990254751753,0.));
#30932=DIRECTION('',(0.,0.,-1.));
#30933=DIRECTION('center_axis',(0.,0.,-1.));
#30934=DIRECTION('ref_axis',(0.939338961794584,0.342990254751753,0.));
#30935=DIRECTION('',(0.,0.,-1.));
#30936=DIRECTION('center_axis',(0.,0.,-1.));
#30937=DIRECTION('ref_axis',(0.939338961794584,0.342990254751753,0.));
#30938=DIRECTION('',(0.,0.,-1.));
#30939=DIRECTION('center_axis',(0.,0.,-1.));
#30940=DIRECTION('ref_axis',(0.939338961794584,0.342990254751753,0.));
#30941=DIRECTION('',(0.,0.,-1.));
#30942=DIRECTION('center_axis',(0.,0.,-1.));
#30943=DIRECTION('ref_axis',(0.939338961794584,0.342990254751753,0.));
#30944=DIRECTION('',(0.,0.,-1.));
#30945=DIRECTION('center_axis',(0.,0.,-1.));
#30946=DIRECTION('ref_axis',(0.939338961794584,0.342990254751753,0.));
#30947=DIRECTION('',(0.,0.,-1.));
#30948=DIRECTION('center_axis',(0.,0.,-1.));
#30949=DIRECTION('ref_axis',(0.939338961794584,0.342990254751753,0.));
#30950=DIRECTION('',(0.,0.,-1.));
#30951=DIRECTION('center_axis',(0.,0.,-1.));
#30952=DIRECTION('ref_axis',(0.939338961794584,0.342990254751753,0.));
#30953=DIRECTION('',(0.,0.,-1.));
#30954=DIRECTION('center_axis',(0.,0.,-1.));
#30955=DIRECTION('ref_axis',(0.939338961794584,0.342990254751753,0.));
#30956=DIRECTION('',(0.,0.,-1.));
#30957=DIRECTION('center_axis',(0.,0.,-1.));
#30958=DIRECTION('ref_axis',(0.939338961794584,0.342990254751753,0.));
#30959=DIRECTION('',(0.,0.,-1.));
#30960=DIRECTION('center_axis',(0.,0.,1.));
#30961=DIRECTION('ref_axis',(1.,0.,0.));
#30962=DIRECTION('center_axis',(0.,0.,-1.));
#30963=DIRECTION('ref_axis',(0.93933894663973,0.342990296255976,0.));
#30964=DIRECTION('',(0.,0.,-1.));
#30965=DIRECTION('center_axis',(0.,0.,1.));
#30966=DIRECTION('ref_axis',(1.,0.,0.));
#30967=DIRECTION('center_axis',(0.,0.,-1.));
#30968=DIRECTION('ref_axis',(0.93933894663973,0.342990296255976,0.));
#30969=DIRECTION('',(0.,0.,-1.));
#30970=DIRECTION('center_axis',(0.,0.,-1.));
#30971=DIRECTION('ref_axis',(0.93933894663973,0.342990296255976,0.));
#30972=DIRECTION('',(0.,0.,-1.));
#30973=DIRECTION('center_axis',(0.,0.,-1.));
#30974=DIRECTION('ref_axis',(0.93933894663973,0.342990296255976,0.));
#30975=DIRECTION('',(0.,0.,-1.));
#30976=DIRECTION('center_axis',(0.,0.,-1.));
#30977=DIRECTION('ref_axis',(0.93933894663973,0.342990296255976,0.));
#30978=DIRECTION('',(0.,0.,-1.));
#30979=DIRECTION('center_axis',(0.,0.,-1.));
#30980=DIRECTION('ref_axis',(0.93933894663973,0.342990296255976,0.));
#30981=DIRECTION('',(0.,0.,-1.));
#30982=DIRECTION('center_axis',(0.,0.,-1.));
#30983=DIRECTION('ref_axis',(0.93933894663973,0.342990296255976,0.));
#30984=DIRECTION('',(0.,0.,-1.));
#30985=DIRECTION('center_axis',(0.,0.,-1.));
#30986=DIRECTION('ref_axis',(0.93933894663973,0.342990296255976,0.));
#30987=DIRECTION('',(0.,0.,-1.));
#30988=DIRECTION('center_axis',(0.,0.,-1.));
#30989=DIRECTION('ref_axis',(0.93933894663973,0.342990296255976,0.));
#30990=DIRECTION('',(0.,0.,-1.));
#30991=DIRECTION('center_axis',(0.,0.,-1.));
#30992=DIRECTION('ref_axis',(0.93933894663973,0.342990296255976,0.));
#30993=DIRECTION('',(0.,0.,-1.));
#30994=DIRECTION('center_axis',(0.,0.,-1.));
#30995=DIRECTION('ref_axis',(0.93933894663973,0.342990296255976,0.));
#30996=DIRECTION('',(0.,0.,-1.));
#30997=DIRECTION('center_axis',(0.,0.,-1.));
#30998=DIRECTION('ref_axis',(0.93933894663973,0.342990296255976,0.));
#30999=DIRECTION('',(0.,0.,-1.));
#31000=DIRECTION('center_axis',(0.,0.,-1.));
#31001=DIRECTION('ref_axis',(0.93933894663973,0.342990296255976,0.));
#31002=DIRECTION('',(0.,0.,-1.));
#31003=DIRECTION('center_axis',(0.,0.,-1.));
#31004=DIRECTION('ref_axis',(0.93933894663973,0.342990296255976,0.));
#31005=DIRECTION('',(0.,0.,-1.));
#31006=DIRECTION('center_axis',(0.,0.,-1.));
#31007=DIRECTION('ref_axis',(0.93933894663973,0.342990296255976,0.));
#31008=DIRECTION('',(0.,0.,-1.));
#31009=DIRECTION('center_axis',(0.,0.,-1.));
#31010=DIRECTION('ref_axis',(0.93933894663973,0.342990296255976,0.));
#31011=DIRECTION('',(0.,0.,-1.));
#31012=DIRECTION('center_axis',(0.,0.,-1.));
#31013=DIRECTION('ref_axis',(0.93933894663973,0.342990296255976,0.));
#31014=DIRECTION('',(0.,0.,-1.));
#31015=DIRECTION('center_axis',(0.,0.,-1.));
#31016=DIRECTION('ref_axis',(0.93933894663973,0.342990296255976,0.));
#31017=DIRECTION('',(0.,0.,-1.));
#31018=DIRECTION('center_axis',(0.,0.,-1.));
#31019=DIRECTION('ref_axis',(0.93933894663973,0.342990296255976,0.));
#31020=DIRECTION('',(0.,0.,-1.));
#31021=DIRECTION('center_axis',(0.,0.,-1.));
#31022=DIRECTION('ref_axis',(0.93933894663973,0.342990296255976,0.));
#31023=DIRECTION('',(0.,0.,-1.));
#31024=DIRECTION('center_axis',(0.,0.,-1.));
#31025=DIRECTION('ref_axis',(0.93933894663973,0.342990296255976,0.));
#31026=DIRECTION('',(0.,0.,-1.));
#31027=DIRECTION('center_axis',(0.,0.,-1.));
#31028=DIRECTION('ref_axis',(0.93933894663973,0.342990296255976,0.));
#31029=DIRECTION('',(0.,0.,-1.));
#31030=DIRECTION('center_axis',(0.,0.,-1.));
#31031=DIRECTION('ref_axis',(0.93933894663973,0.342990296255976,0.));
#31032=DIRECTION('',(0.,0.,-1.));
#31033=DIRECTION('center_axis',(0.,0.,-1.));
#31034=DIRECTION('ref_axis',(0.93933894663973,0.342990296255976,0.));
#31035=DIRECTION('',(0.,0.,-1.));
#31036=DIRECTION('center_axis',(0.,0.,-1.));
#31037=DIRECTION('ref_axis',(0.93933894663973,0.342990296255976,0.));
#31038=DIRECTION('',(0.,0.,-1.));
#31039=DIRECTION('center_axis',(0.,0.,-1.));
#31040=DIRECTION('ref_axis',(0.93933894663973,0.342990296255976,0.));
#31041=DIRECTION('',(0.,0.,-1.));
#31042=DIRECTION('center_axis',(0.,0.,-1.));
#31043=DIRECTION('ref_axis',(0.93933894663973,0.342990296255976,0.));
#31044=DIRECTION('',(0.,0.,-1.));
#31045=DIRECTION('center_axis',(0.,0.,1.));
#31046=DIRECTION('ref_axis',(1.,0.,0.));
#31047=DIRECTION('center_axis',(0.,0.,-1.));
#31048=DIRECTION('ref_axis',(0.939338946471827,0.342990296715807,0.));
#31049=DIRECTION('',(0.,0.,-1.));
#31050=DIRECTION('center_axis',(0.,0.,1.));
#31051=DIRECTION('ref_axis',(1.,0.,0.));
#31052=DIRECTION('center_axis',(0.,0.,-1.));
#31053=DIRECTION('ref_axis',(0.939338946471827,0.342990296715807,0.));
#31054=DIRECTION('',(0.,0.,-1.));
#31055=DIRECTION('center_axis',(0.,0.,-1.));
#31056=DIRECTION('ref_axis',(0.939338946471827,0.342990296715807,0.));
#31057=DIRECTION('',(0.,0.,-1.));
#31058=DIRECTION('center_axis',(0.,0.,-1.));
#31059=DIRECTION('ref_axis',(0.939338946471827,0.342990296715807,0.));
#31060=DIRECTION('',(0.,0.,-1.));
#31061=DIRECTION('center_axis',(0.,0.,-1.));
#31062=DIRECTION('ref_axis',(0.939338946471827,0.342990296715807,0.));
#31063=DIRECTION('',(0.,0.,-1.));
#31064=DIRECTION('center_axis',(0.,0.,-1.));
#31065=DIRECTION('ref_axis',(0.939338946471827,0.342990296715807,0.));
#31066=DIRECTION('',(0.,0.,-1.));
#31067=DIRECTION('center_axis',(0.,0.,-1.));
#31068=DIRECTION('ref_axis',(0.939338946471827,0.342990296715807,0.));
#31069=DIRECTION('',(0.,0.,-1.));
#31070=DIRECTION('center_axis',(0.,0.,-1.));
#31071=DIRECTION('ref_axis',(0.939338946471827,0.342990296715807,0.));
#31072=DIRECTION('',(0.,0.,-1.));
#31073=DIRECTION('center_axis',(0.,0.,-1.));
#31074=DIRECTION('ref_axis',(0.939338946471827,0.342990296715807,0.));
#31075=DIRECTION('',(0.,0.,-1.));
#31076=DIRECTION('center_axis',(0.,0.,-1.));
#31077=DIRECTION('ref_axis',(0.939338946471827,0.342990296715807,0.));
#31078=DIRECTION('',(0.,0.,-1.));
#31079=DIRECTION('center_axis',(0.,0.,-1.));
#31080=DIRECTION('ref_axis',(0.939338946471827,0.342990296715807,0.));
#31081=DIRECTION('',(0.,0.,-1.));
#31082=DIRECTION('center_axis',(0.,0.,-1.));
#31083=DIRECTION('ref_axis',(0.939338946471827,0.342990296715807,0.));
#31084=DIRECTION('',(0.,0.,-1.));
#31085=DIRECTION('center_axis',(0.,0.,-1.));
#31086=DIRECTION('ref_axis',(0.939338946471827,0.342990296715807,0.));
#31087=DIRECTION('',(0.,0.,-1.));
#31088=DIRECTION('center_axis',(0.,0.,-1.));
#31089=DIRECTION('ref_axis',(0.939338946471827,0.342990296715807,0.));
#31090=DIRECTION('',(0.,0.,-1.));
#31091=DIRECTION('center_axis',(0.,0.,-1.));
#31092=DIRECTION('ref_axis',(0.939338946471827,0.342990296715807,0.));
#31093=DIRECTION('',(0.,0.,-1.));
#31094=DIRECTION('center_axis',(0.,0.,-1.));
#31095=DIRECTION('ref_axis',(0.939338946471827,0.342990296715807,0.));
#31096=DIRECTION('',(0.,0.,-1.));
#31097=DIRECTION('center_axis',(0.,0.,-1.));
#31098=DIRECTION('ref_axis',(0.939338946471827,0.342990296715807,0.));
#31099=DIRECTION('',(0.,0.,-1.));
#31100=DIRECTION('center_axis',(0.,0.,-1.));
#31101=DIRECTION('ref_axis',(0.939338946471827,0.342990296715807,0.));
#31102=DIRECTION('',(0.,0.,-1.));
#31103=DIRECTION('center_axis',(0.,0.,-1.));
#31104=DIRECTION('ref_axis',(0.939338946471827,0.342990296715807,0.));
#31105=DIRECTION('',(0.,0.,-1.));
#31106=DIRECTION('center_axis',(0.,0.,-1.));
#31107=DIRECTION('ref_axis',(0.939338946471827,0.342990296715807,0.));
#31108=DIRECTION('',(0.,0.,-1.));
#31109=DIRECTION('center_axis',(0.,0.,-1.));
#31110=DIRECTION('ref_axis',(0.939338946471827,0.342990296715807,0.));
#31111=DIRECTION('',(0.,0.,-1.));
#31112=DIRECTION('center_axis',(0.,0.,-1.));
#31113=DIRECTION('ref_axis',(0.939338946471827,0.342990296715807,0.));
#31114=DIRECTION('',(0.,0.,-1.));
#31115=DIRECTION('center_axis',(0.,0.,-1.));
#31116=DIRECTION('ref_axis',(0.939338946471827,0.342990296715807,0.));
#31117=DIRECTION('',(0.,0.,-1.));
#31118=DIRECTION('center_axis',(0.,0.,-1.));
#31119=DIRECTION('ref_axis',(0.939338946471827,0.342990296715807,0.));
#31120=DIRECTION('',(0.,0.,-1.));
#31121=DIRECTION('center_axis',(0.,0.,-1.));
#31122=DIRECTION('ref_axis',(0.939338946471827,0.342990296715807,0.));
#31123=DIRECTION('',(0.,0.,-1.));
#31124=DIRECTION('center_axis',(0.,0.,-1.));
#31125=DIRECTION('ref_axis',(0.939338946471827,0.342990296715807,0.));
#31126=DIRECTION('',(0.,0.,-1.));
#31127=DIRECTION('center_axis',(0.,0.,-1.));
#31128=DIRECTION('ref_axis',(0.939338946471827,0.342990296715807,0.));
#31129=DIRECTION('',(0.,0.,-1.));
#31130=DIRECTION('center_axis',(0.,0.,1.));
#31131=DIRECTION('ref_axis',(1.,0.,0.));
#31132=DIRECTION('center_axis',(0.,0.,-1.));
#31133=DIRECTION('ref_axis',(0.939338976758881,0.3429902137694,0.));
#31134=DIRECTION('',(0.,0.,-1.));
#31135=DIRECTION('center_axis',(0.,0.,1.));
#31136=DIRECTION('ref_axis',(1.,0.,0.));
#31137=DIRECTION('center_axis',(0.,0.,-1.));
#31138=DIRECTION('ref_axis',(0.939338976758881,0.3429902137694,0.));
#31139=DIRECTION('',(0.,0.,-1.));
#31140=DIRECTION('center_axis',(0.,0.,-1.));
#31141=DIRECTION('ref_axis',(0.939338976758881,0.3429902137694,0.));
#31142=DIRECTION('',(0.,0.,-1.));
#31143=DIRECTION('center_axis',(0.,0.,-1.));
#31144=DIRECTION('ref_axis',(0.939338976758881,0.3429902137694,0.));
#31145=DIRECTION('',(0.,0.,-1.));
#31146=DIRECTION('center_axis',(0.,0.,-1.));
#31147=DIRECTION('ref_axis',(0.939338976758881,0.3429902137694,0.));
#31148=DIRECTION('',(0.,0.,-1.));
#31149=DIRECTION('center_axis',(0.,0.,-1.));
#31150=DIRECTION('ref_axis',(0.939338976758881,0.3429902137694,0.));
#31151=DIRECTION('',(0.,0.,-1.));
#31152=DIRECTION('center_axis',(0.,0.,-1.));
#31153=DIRECTION('ref_axis',(0.939338976758881,0.3429902137694,0.));
#31154=DIRECTION('',(0.,0.,-1.));
#31155=DIRECTION('center_axis',(0.,0.,-1.));
#31156=DIRECTION('ref_axis',(0.939338976758881,0.3429902137694,0.));
#31157=DIRECTION('',(0.,0.,-1.));
#31158=DIRECTION('center_axis',(0.,0.,-1.));
#31159=DIRECTION('ref_axis',(0.939338976758881,0.3429902137694,0.));
#31160=DIRECTION('',(0.,0.,-1.));
#31161=DIRECTION('center_axis',(0.,0.,-1.));
#31162=DIRECTION('ref_axis',(0.939338976758881,0.3429902137694,0.));
#31163=DIRECTION('',(0.,0.,-1.));
#31164=DIRECTION('center_axis',(0.,0.,-1.));
#31165=DIRECTION('ref_axis',(0.939338976758881,0.3429902137694,0.));
#31166=DIRECTION('',(0.,0.,-1.));
#31167=DIRECTION('center_axis',(0.,0.,-1.));
#31168=DIRECTION('ref_axis',(0.939338976758881,0.3429902137694,0.));
#31169=DIRECTION('',(0.,0.,-1.));
#31170=DIRECTION('center_axis',(0.,0.,-1.));
#31171=DIRECTION('ref_axis',(0.939338976758881,0.3429902137694,0.));
#31172=DIRECTION('',(0.,0.,-1.));
#31173=DIRECTION('center_axis',(0.,0.,-1.));
#31174=DIRECTION('ref_axis',(0.939338976758881,0.3429902137694,0.));
#31175=DIRECTION('',(0.,0.,-1.));
#31176=DIRECTION('center_axis',(0.,0.,-1.));
#31177=DIRECTION('ref_axis',(0.939338976758881,0.3429902137694,0.));
#31178=DIRECTION('',(0.,0.,-1.));
#31179=DIRECTION('center_axis',(0.,0.,-1.));
#31180=DIRECTION('ref_axis',(0.939338976758881,0.3429902137694,0.));
#31181=DIRECTION('',(0.,0.,-1.));
#31182=DIRECTION('center_axis',(0.,0.,-1.));
#31183=DIRECTION('ref_axis',(0.939338976758881,0.3429902137694,0.));
#31184=DIRECTION('',(0.,0.,-1.));
#31185=DIRECTION('center_axis',(0.,0.,-1.));
#31186=DIRECTION('ref_axis',(0.939338976758881,0.3429902137694,0.));
#31187=DIRECTION('',(0.,0.,-1.));
#31188=DIRECTION('center_axis',(0.,0.,-1.));
#31189=DIRECTION('ref_axis',(0.939338976758881,0.3429902137694,0.));
#31190=DIRECTION('',(0.,0.,-1.));
#31191=DIRECTION('center_axis',(0.,0.,-1.));
#31192=DIRECTION('ref_axis',(0.939338976758881,0.3429902137694,0.));
#31193=DIRECTION('',(0.,0.,-1.));
#31194=DIRECTION('center_axis',(0.,0.,-1.));
#31195=DIRECTION('ref_axis',(0.939338976758881,0.3429902137694,0.));
#31196=DIRECTION('',(0.,0.,-1.));
#31197=DIRECTION('center_axis',(0.,0.,-1.));
#31198=DIRECTION('ref_axis',(0.939338976758881,0.3429902137694,0.));
#31199=DIRECTION('',(0.,0.,-1.));
#31200=DIRECTION('center_axis',(0.,0.,-1.));
#31201=DIRECTION('ref_axis',(0.939338976758881,0.3429902137694,0.));
#31202=DIRECTION('',(0.,0.,-1.));
#31203=DIRECTION('center_axis',(0.,0.,-1.));
#31204=DIRECTION('ref_axis',(0.939338976758881,0.3429902137694,0.));
#31205=DIRECTION('',(0.,0.,-1.));
#31206=DIRECTION('center_axis',(0.,0.,-1.));
#31207=DIRECTION('ref_axis',(0.939338976758881,0.3429902137694,0.));
#31208=DIRECTION('',(0.,0.,-1.));
#31209=DIRECTION('center_axis',(0.,0.,-1.));
#31210=DIRECTION('ref_axis',(0.939338976758881,0.3429902137694,0.));
#31211=DIRECTION('',(0.,0.,-1.));
#31212=DIRECTION('center_axis',(0.,0.,-1.));
#31213=DIRECTION('ref_axis',(0.939338976758881,0.3429902137694,0.));
#31214=DIRECTION('',(0.,0.,-1.));
#31215=DIRECTION('center_axis',(0.,0.,1.));
#31216=DIRECTION('ref_axis',(1.,0.,0.));
#31217=DIRECTION('center_axis',(0.,0.,-1.));
#31218=DIRECTION('ref_axis',(0.939338976758881,0.3429902137694,0.));
#31219=DIRECTION('center_axis',(0.,0.,-1.));
#31220=DIRECTION('ref_axis',(0.939338946471827,0.342990296715807,0.));
#31221=DIRECTION('center_axis',(0.,0.,-1.));
#31222=DIRECTION('ref_axis',(0.93933894663973,0.342990296255976,0.));
#31223=DIRECTION('center_axis',(0.,0.,-1.));
#31224=DIRECTION('ref_axis',(0.939338961794584,0.342990254751753,0.));
#31225=DIRECTION('center_axis',(1.,0.,0.));
#31226=DIRECTION('ref_axis',(0.,-0.349194147217983,0.937050397550049));
#31227=DIRECTION('center_axis',(1.,0.,0.));
#31228=DIRECTION('ref_axis',(0.,0.349194145719507,0.93705039810846));
#31229=DIRECTION('center_axis',(-1.,0.,0.));
#31230=DIRECTION('ref_axis',(0.,0.,1.));
#31231=DIRECTION('center_axis',(0.,0.,-1.));
#31232=DIRECTION('ref_axis',(-0.60919368949553,-0.793021467981053,0.));
#31233=DIRECTION('center_axis',(0.,0.,-1.));
#31234=DIRECTION('ref_axis',(-0.609193706391024,-0.793021455002049,0.));
#31235=DIRECTION('center_axis',(0.,0.,-1.));
#31236=DIRECTION('ref_axis',(-0.609193705300279,-0.793021455839952,0.));
#31237=DIRECTION('center_axis',(0.,0.,-1.));
#31238=DIRECTION('ref_axis',(-0.609193654691519,-0.793021494717256,0.));
#31239=DIRECTION('center_axis',(-1.,0.,0.));
#31240=DIRECTION('ref_axis',(0.,0.793547993033681,-0.608507668605924));
#31241=DIRECTION('center_axis',(1.,0.,0.));
#31242=DIRECTION('ref_axis',(0.,-0.793547993282919,-0.608507668280895));
#31243=DIRECTION('center_axis',(0.,0.,1.));
#31244=DIRECTION('ref_axis',(1.,0.,0.));
#31245=DIRECTION('center_axis',(0.,0.,1.));
#31246=DIRECTION('ref_axis',(1.,0.,0.));
#31247=DIRECTION('',(0.,0.,1.));
#31248=DIRECTION('center_axis',(0.,0.,1.));
#31249=DIRECTION('ref_axis',(1.,0.,0.));
#31250=DIRECTION('center_axis',(0.,0.,-1.));
#31251=DIRECTION('ref_axis',(-1.,0.,0.));
#31252=DIRECTION('center_axis',(0.,0.,1.));
#31253=DIRECTION('ref_axis',(1.,0.,0.));
#31254=DIRECTION('center_axis',(0.,0.,1.));
#31255=DIRECTION('ref_axis',(1.,0.,0.));
#31256=DIRECTION('',(0.,0.,-1.));
#31257=DIRECTION('center_axis',(0.,0.,1.));
#31258=DIRECTION('ref_axis',(1.,0.,0.));
#31259=DIRECTION('',(0.,0.,1.));
#31260=DIRECTION('center_axis',(0.,0.,-1.));
#31261=DIRECTION('ref_axis',(-1.,0.,0.));
#31262=DIRECTION('',(0.,-1.,0.));
#31263=DIRECTION('',(-1.,0.,0.));
#31264=DIRECTION('',(0.,-1.,0.));
#31265=DIRECTION('center_axis',(0.,0.,1.));
#31266=DIRECTION('ref_axis',(-0.374029024133323,0.927416998499529,0.));
#31267=DIRECTION('center_axis',(0.,0.,1.));
#31268=DIRECTION('ref_axis',(1.,0.,0.));
#31269=DIRECTION('center_axis',(0.,0.,1.));
#31270=DIRECTION('ref_axis',(1.,0.,0.));
#31271=DIRECTION('',(0.,0.,1.));
#31272=DIRECTION('center_axis',(0.,0.,1.));
#31273=DIRECTION('ref_axis',(1.,0.,0.));
#31274=DIRECTION('center_axis',(0.,0.,-1.));
#31275=DIRECTION('ref_axis',(-1.,0.,0.));
#31276=DIRECTION('center_axis',(0.,0.,1.));
#31277=DIRECTION('ref_axis',(-0.873226700271574,-0.487314200421882,0.));
#31278=DIRECTION('center_axis',(0.,0.,1.));
#31279=DIRECTION('ref_axis',(1.,0.,0.));
#31280=DIRECTION('',(0.,0.,-1.));
#31281=DIRECTION('center_axis',(0.,0.,1.));
#31282=DIRECTION('ref_axis',(1.,0.,0.));
#31283=DIRECTION('',(0.,0.,1.));
#31284=DIRECTION('center_axis',(0.,0.,-1.));
#31285=DIRECTION('ref_axis',(-1.,0.,0.));
#31286=DIRECTION('',(0.,1.,0.));
#31287=DIRECTION('',(-1.,0.,0.));
#31288=DIRECTION('',(0.,1.,0.));
#31289=DIRECTION('center_axis',(0.,0.,1.));
#31290=DIRECTION('ref_axis',(0.914708142118334,0.404115100859181,0.));
#31291=DIRECTION('center_axis',(0.,0.,1.));
#31292=DIRECTION('ref_axis',(1.,0.,0.));
#31293=DIRECTION('center_axis',(0.,0.,1.));
#31294=DIRECTION('ref_axis',(1.,0.,0.));
#31295=DIRECTION('',(0.,0.,1.));
#31296=DIRECTION('center_axis',(0.,0.,1.));
#31297=DIRECTION('ref_axis',(1.,0.,0.));
#31298=DIRECTION('center_axis',(0.,0.,-1.));
#31299=DIRECTION('ref_axis',(-1.,0.,0.));
#31300=DIRECTION('center_axis',(-1.,0.,0.));
#31301=DIRECTION('ref_axis',(0.,1.,0.));
#31302=DIRECTION('',(0.,0.,-1.));
#31303=DIRECTION('',(0.,1.,0.));
#31304=DIRECTION('',(0.,0.,-1.));
#31305=DIRECTION('center_axis',(1.,0.,0.));
#31306=DIRECTION('ref_axis',(0.,-1.,0.));
#31307=DIRECTION('',(0.,-1.,0.));
#31308=DIRECTION('',(0.,0.,-1.));
#31309=DIRECTION('',(0.,1.,0.));
#31310=DIRECTION('',(0.,0.,-1.));
#31311=DIRECTION('center_axis',(0.,1.,0.));
#31312=DIRECTION('ref_axis',(1.,0.,0.));
#31313=DIRECTION('',(1.,0.,0.));
#31314=DIRECTION('',(0.,0.,-1.));
#31315=DIRECTION('',(-1.,0.,0.));
#31316=DIRECTION('center_axis',(0.,0.,1.));
#31317=DIRECTION('ref_axis',(1.,0.,0.));
#31318=DIRECTION('',(0.,1.,0.));
#31319=DIRECTION('center_axis',(0.,0.,1.));
#31320=DIRECTION('ref_axis',(1.,0.,0.));
#31321=DIRECTION('',(-1.,0.,0.));
#31322=DIRECTION('center_axis',(0.,0.,-1.));
#31323=DIRECTION('ref_axis',(-1.,0.,0.));
#31324=DIRECTION('',(0.,1.,0.));
#31325=DIRECTION('center_axis',(0.,0.,-1.));
#31326=DIRECTION('ref_axis',(0.,1.,0.));
#31327=DIRECTION('',(0.987070639057186,-0.160285849379284,0.));
#31328=DIRECTION('center_axis',(0.,0.,-1.));
#31329=DIRECTION('ref_axis',(1.,4.44089209850062E-16,0.));
#31330=DIRECTION('',(0.,-1.,0.));
#31331=DIRECTION('',(-1.,0.,0.));
#31332=DIRECTION('',(0.,-1.,0.));
#31333=DIRECTION('',(1.,0.,0.));
#31334=DIRECTION('',(0.,-1.,0.));
#31335=DIRECTION('center_axis',(0.,0.,-1.));
#31336=DIRECTION('ref_axis',(0.,-1.,0.));
#31337=DIRECTION('',(-1.,3.69197497485193E-16,0.));
#31338=DIRECTION('center_axis',(0.,0.,-1.));
#31339=DIRECTION('ref_axis',(-1.,0.,0.));
#31340=DIRECTION('',(0.,1.,0.));
#31341=DIRECTION('',(1.,0.,0.));
#31342=DIRECTION('',(0.,1.,0.));
#31343=DIRECTION('',(-1.,0.,0.));
#31344=DIRECTION('',(0.,1.,0.));
#31345=DIRECTION('center_axis',(0.,0.,-1.));
#31346=DIRECTION('ref_axis',(0.,1.,0.));
#31347=DIRECTION('',(0.987070639057186,0.160285849379284,0.));
#31348=DIRECTION('center_axis',(0.,0.,-1.));
#31349=DIRECTION('ref_axis',(1.,0.,0.));
#31350=DIRECTION('',(0.,-1.,0.));
#31351=DIRECTION('center_axis',(0.,0.,-1.));
#31352=DIRECTION('ref_axis',(0.,-1.,0.));
#31353=DIRECTION('',(-1.,0.,0.));
#31354=DIRECTION('center_axis',(0.,0.,1.));
#31355=DIRECTION('ref_axis',(0.,1.,0.));
#31356=DIRECTION('center_axis',(0.,0.,1.));
#31357=DIRECTION('ref_axis',(1.,0.,0.));
#31358=DIRECTION('center_axis',(0.,0.,1.));
#31359=DIRECTION('ref_axis',(1.,0.,0.));
#31360=DIRECTION('center_axis',(0.,0.,1.));
#31361=DIRECTION('ref_axis',(0.,1.,0.));
#31362=DIRECTION('',(0.,-1.,0.));
#31363=DIRECTION('',(-1.,0.,0.));
#31364=DIRECTION('',(0.,1.,0.));
#31365=DIRECTION('',(-1.,0.,0.));
#31366=DIRECTION('center_axis',(0.,-1.,0.));
#31367=DIRECTION('ref_axis',(0.,0.,1.));
#31368=DIRECTION('',(0.,0.,-1.));
#31369=DIRECTION('',(0.,0.,1.));
#31370=DIRECTION('',(-1.,0.,0.));
#31371=DIRECTION('center_axis',(0.,0.,1.));
#31372=DIRECTION('ref_axis',(0.,1.,0.));
#31373=DIRECTION('',(0.,-1.,0.));
#31374=DIRECTION('',(0.,1.,0.));
#31375=DIRECTION('',(-1.,0.,0.));
#31376=DIRECTION('center_axis',(0.,-0.894427190999916,-0.447213595499957));
#31377=DIRECTION('ref_axis',(0.,-0.447213595499957,0.894427190999916));
#31378=DIRECTION('',(0.,0.447213595499957,-0.894427190999916));
#31379=DIRECTION('',(0.,-0.447213595499957,0.894427190999916));
#31380=DIRECTION('',(-1.,0.,0.));
#31381=DIRECTION('center_axis',(0.,0.894427190999916,-0.447213595499957));
#31382=DIRECTION('ref_axis',(0.,-0.447213595499957,-0.894427190999916));
#31383=DIRECTION('',(0.,0.447213595499957,0.894427190999916));
#31384=DIRECTION('',(0.,-0.447213595499957,-0.894427190999916));
#31385=DIRECTION('',(-1.,0.,0.));
#31386=DIRECTION('center_axis',(0.,0.,1.));
#31387=DIRECTION('ref_axis',(0.,1.,0.));
#31388=DIRECTION('',(0.,-1.,0.));
#31389=DIRECTION('',(0.,1.,0.));
#31390=DIRECTION('',(-1.,0.,0.));
#31391=DIRECTION('center_axis',(0.,1.,0.));
#31392=DIRECTION('ref_axis',(0.,0.,-1.));
#31393=DIRECTION('',(0.,0.,1.));
#31394=DIRECTION('',(0.,0.,-1.));
#31395=DIRECTION('center_axis',(1.,0.,0.));
#31396=DIRECTION('ref_axis',(0.,0.,1.));
#31397=DIRECTION('center_axis',(1.,0.,0.));
#31398=DIRECTION('ref_axis',(0.,0.,1.));
#31399=DIRECTION('',(1.,0.,0.));
#31400=DIRECTION('center_axis',(-1.,0.,0.));
#31401=DIRECTION('ref_axis',(0.,0.,1.));
#31402=DIRECTION('center_axis',(-1.,0.,0.));
#31403=DIRECTION('ref_axis',(0.,0.,1.));
#31404=DIRECTION('center_axis',(1.,0.,0.));
#31405=DIRECTION('ref_axis',(0.,-0.912870929175277,0.408248290463863));
#31406=DIRECTION('center_axis',(-1.,0.,0.));
#31407=DIRECTION('ref_axis',(0.,0.,1.));
#31408=DIRECTION('',(-1.,0.,0.));
#31409=DIRECTION('center_axis',(1.,0.,0.));
#31410=DIRECTION('ref_axis',(0.,0.,1.));
#31411=DIRECTION('',(-1.,0.,0.));
#31412=DIRECTION('center_axis',(0.,0.,-1.));
#31413=DIRECTION('ref_axis',(0.,-1.,0.));
#31414=DIRECTION('',(0.,1.,0.));
#31415=DIRECTION('',(0.,-1.,0.));
#31416=DIRECTION('',(-1.,0.,0.));
#31417=DIRECTION('center_axis',(1.,0.,0.));
#31418=DIRECTION('ref_axis',(0.,0.912870929175277,0.408248290463863));
#31419=DIRECTION('center_axis',(-1.,0.,0.));
#31420=DIRECTION('ref_axis',(0.,0.,1.));
#31421=DIRECTION('center_axis',(1.,0.,0.));
#31422=DIRECTION('ref_axis',(0.,0.,1.));
#31423=DIRECTION('',(-1.,0.,0.));
#31424=DIRECTION('center_axis',(0.,-1.,0.));
#31425=DIRECTION('ref_axis',(0.,0.,1.));
#31426=DIRECTION('',(0.,0.,-1.));
#31427=DIRECTION('',(0.,0.,1.));
#31428=DIRECTION('center_axis',(0.,1.,0.));
#31429=DIRECTION('ref_axis',(0.,0.,-1.));
#31430=DIRECTION('',(0.,0.,1.));
#31431=DIRECTION('',(0.,0.,-1.));
#31432=DIRECTION('center_axis',(-1.,0.,0.));
#31433=DIRECTION('ref_axis',(0.,0.,1.));
#31434=DIRECTION('center_axis',(1.,0.,0.));
#31435=DIRECTION('ref_axis',(0.,0.,1.));
#31436=DIRECTION('center_axis',(1.,0.,0.));
#31437=DIRECTION('ref_axis',(0.,0.,1.));
#31438=DIRECTION('center_axis',(0.,1.,0.));
#31439=DIRECTION('ref_axis',(0.,0.,-1.));
#31440=DIRECTION('',(0.,0.,1.));
#31441=DIRECTION('',(-1.,0.,0.));
#31442=DIRECTION('',(0.,0.,-1.));
#31443=DIRECTION('',(-1.,0.,0.));
#31444=DIRECTION('center_axis',(0.,0.,-1.));
#31445=DIRECTION('ref_axis',(0.,-1.,0.));
#31446=DIRECTION('',(0.,1.,0.));
#31447=DIRECTION('',(0.,-1.,0.));
#31448=DIRECTION('',(-1.,0.,0.));
#31449=DIRECTION('center_axis',(0.,0.894427190999916,0.447213595499958));
#31450=DIRECTION('ref_axis',(0.,0.447213595499958,-0.894427190999916));
#31451=DIRECTION('',(0.,-0.447213595499958,0.894427190999916));
#31452=DIRECTION('',(0.,0.447213595499958,-0.894427190999916));
#31453=DIRECTION('',(-1.,0.,0.));
#31454=DIRECTION('center_axis',(0.,-0.894427190999916,0.447213595499958));
#31455=DIRECTION('ref_axis',(0.,0.447213595499958,0.894427190999916));
#31456=DIRECTION('',(0.,-0.447213595499958,-0.894427190999916));
#31457=DIRECTION('',(0.,0.447213595499958,0.894427190999916));
#31458=DIRECTION('',(-1.,0.,0.));
#31459=DIRECTION('center_axis',(0.,0.,-1.));
#31460=DIRECTION('ref_axis',(0.,-1.,0.));
#31461=DIRECTION('',(0.,1.,0.));
#31462=DIRECTION('',(0.,-1.,0.));
#31463=DIRECTION('',(-1.,0.,0.));
#31464=DIRECTION('center_axis',(0.,-1.,0.));
#31465=DIRECTION('ref_axis',(0.,0.,1.));
#31466=DIRECTION('',(0.,0.,-1.));
#31467=DIRECTION('',(0.,0.,1.));
#31468=DIRECTION('',(-1.,0.,0.));
#31469=DIRECTION('center_axis',(0.,0.,-1.));
#31470=DIRECTION('ref_axis',(0.,-1.,0.));
#31471=DIRECTION('',(0.,1.,0.));
#31472=DIRECTION('',(0.,-1.,0.));
#31473=DIRECTION('center_axis',(1.,0.,0.));
#31474=DIRECTION('ref_axis',(0.,0.,1.));
#31475=DIRECTION('center_axis',(1.,0.,0.));
#31476=DIRECTION('ref_axis',(0.,0.,1.));
#31477=DIRECTION('',(1.,0.,0.));
#31478=DIRECTION('center_axis',(-1.,0.,0.));
#31479=DIRECTION('ref_axis',(0.,0.,1.));
#31480=DIRECTION('center_axis',(-1.,0.,0.));
#31481=DIRECTION('ref_axis',(0.,0.,1.));
#31482=DIRECTION('center_axis',(1.,0.,0.));
#31483=DIRECTION('ref_axis',(0.,-1.,0.));
#31484=DIRECTION('center_axis',(1.,0.,0.));
#31485=DIRECTION('ref_axis',(0.,-1.,0.));
#31486=DIRECTION('center_axis',(1.,0.,0.));
#31487=DIRECTION('ref_axis',(0.,0.,1.));
#31488=DIRECTION('center_axis',(1.,0.,0.));
#31489=DIRECTION('ref_axis',(0.,0.,1.));
#31490=DIRECTION('',(1.,0.,0.));
#31491=DIRECTION('center_axis',(-1.,0.,0.));
#31492=DIRECTION('ref_axis',(0.,0.,1.));
#31493=DIRECTION('center_axis',(-1.,0.,0.));
#31494=DIRECTION('ref_axis',(0.,0.,1.));
#31495=DIRECTION('center_axis',(1.,0.,0.));
#31496=DIRECTION('ref_axis',(0.,0.,1.));
#31497=DIRECTION('center_axis',(1.,0.,0.));
#31498=DIRECTION('ref_axis',(0.,0.,1.));
#31499=DIRECTION('',(1.,0.,0.));
#31500=DIRECTION('center_axis',(-1.,0.,0.));
#31501=DIRECTION('ref_axis',(0.,0.,1.));
#31502=DIRECTION('center_axis',(1.,0.,0.));
#31503=DIRECTION('ref_axis',(0.,-0.912870929175277,0.408248290463863));
#31504=DIRECTION('center_axis',(1.,0.,0.));
#31505=DIRECTION('ref_axis',(0.,0.,1.));
#31506=DIRECTION('',(1.,0.,0.));
#31507=DIRECTION('center_axis',(1.,0.,0.));
#31508=DIRECTION('ref_axis',(0.,0.,1.));
#31509=DIRECTION('',(1.,0.,0.));
#31510=DIRECTION('center_axis',(0.,0.,1.));
#31511=DIRECTION('ref_axis',(0.,-1.,0.));
#31512=DIRECTION('',(0.,-1.,0.));
#31513=DIRECTION('',(1.,0.,0.));
#31514=DIRECTION('',(0.,-1.,0.));
#31515=DIRECTION('center_axis',(1.,0.,0.));
#31516=DIRECTION('ref_axis',(0.,0.912870929175277,0.408248290463863));
#31517=DIRECTION('center_axis',(1.,0.,0.));
#31518=DIRECTION('ref_axis',(0.,0.,1.));
#31519=DIRECTION('',(1.,0.,0.));
#31520=DIRECTION('center_axis',(1.,0.,0.));
#31521=DIRECTION('ref_axis',(0.,0.,1.));
#31522=DIRECTION('center_axis',(0.,1.,0.));
#31523=DIRECTION('ref_axis',(0.,0.,1.));
#31524=DIRECTION('',(0.,0.,1.));
#31525=DIRECTION('',(0.,0.,1.));
#31526=DIRECTION('center_axis',(0.,-1.,0.));
#31527=DIRECTION('ref_axis',(0.,0.,-1.));
#31528=DIRECTION('',(0.,0.,-1.));
#31529=DIRECTION('',(0.,0.,-1.));
#31530=DIRECTION('center_axis',(-1.,0.,0.));
#31531=DIRECTION('ref_axis',(0.,0.,1.));
#31532=DIRECTION('center_axis',(-1.,0.,0.));
#31533=DIRECTION('ref_axis',(0.,0.,1.));
#31534=DIRECTION('center_axis',(-1.,0.,0.));
#31535=DIRECTION('ref_axis',(0.,0.,1.));
#31536=DIRECTION('center_axis',(0.,-1.,0.));
#31537=DIRECTION('ref_axis',(0.,0.,-1.));
#31538=DIRECTION('',(0.,0.,-1.));
#31539=DIRECTION('',(1.,0.,0.));
#31540=DIRECTION('',(0.,0.,-1.));
#31541=DIRECTION('',(1.,0.,0.));
#31542=DIRECTION('center_axis',(0.,0.,1.));
#31543=DIRECTION('ref_axis',(0.,-1.,0.));
#31544=DIRECTION('',(0.,-1.,0.));
#31545=DIRECTION('',(1.,0.,0.));
#31546=DIRECTION('',(0.,-1.,0.));
#31547=DIRECTION('center_axis',(0.,-0.894427190999916,-0.447213595499958));
#31548=DIRECTION('ref_axis',(0.,0.447213595499958,-0.894427190999916));
#31549=DIRECTION('',(0.,0.447213595499958,-0.894427190999916));
#31550=DIRECTION('',(1.,0.,0.));
#31551=DIRECTION('',(0.,0.447213595499958,-0.894427190999916));
#31552=DIRECTION('center_axis',(0.,0.894427190999916,-0.447213595499958));
#31553=DIRECTION('ref_axis',(0.,0.447213595499958,0.894427190999916));
#31554=DIRECTION('',(0.,0.447213595499958,0.894427190999916));
#31555=DIRECTION('',(1.,0.,0.));
#31556=DIRECTION('',(0.,0.447213595499958,0.894427190999916));
#31557=DIRECTION('center_axis',(0.,0.,1.));
#31558=DIRECTION('ref_axis',(0.,-1.,0.));
#31559=DIRECTION('',(0.,-1.,0.));
#31560=DIRECTION('',(1.,0.,0.));
#31561=DIRECTION('',(0.,-1.,0.));
#31562=DIRECTION('center_axis',(0.,1.,0.));
#31563=DIRECTION('ref_axis',(0.,0.,1.));
#31564=DIRECTION('',(0.,0.,1.));
#31565=DIRECTION('',(1.,0.,0.));
#31566=DIRECTION('',(0.,0.,1.));
#31567=DIRECTION('center_axis',(0.,0.,1.));
#31568=DIRECTION('ref_axis',(0.,-1.,0.));
#31569=DIRECTION('',(0.,-1.,0.));
#31570=DIRECTION('',(0.,-1.,0.));
#31571=DIRECTION('center_axis',(1.,0.,0.));
#31572=DIRECTION('ref_axis',(0.,0.,1.));
#31573=DIRECTION('center_axis',(1.,0.,0.));
#31574=DIRECTION('ref_axis',(0.,0.,1.));
#31575=DIRECTION('',(1.,0.,0.));
#31576=DIRECTION('center_axis',(1.,0.,0.));
#31577=DIRECTION('ref_axis',(0.,0.,1.));
#31578=DIRECTION('center_axis',(-1.,0.,0.));
#31579=DIRECTION('ref_axis',(0.,0.,1.));
#31580=DIRECTION('center_axis',(0.,0.,-1.));
#31581=DIRECTION('ref_axis',(0.,1.,0.));
#31582=DIRECTION('',(0.,1.,0.));
#31583=DIRECTION('',(1.,0.,0.));
#31584=DIRECTION('',(0.,1.,0.));
#31585=DIRECTION('',(1.,0.,0.));
#31586=DIRECTION('center_axis',(0.,1.,0.));
#31587=DIRECTION('ref_axis',(0.,0.,1.));
#31588=DIRECTION('',(0.,0.,1.));
#31589=DIRECTION('',(1.,0.,0.));
#31590=DIRECTION('',(0.,0.,1.));
#31591=DIRECTION('center_axis',(0.,0.,-1.));
#31592=DIRECTION('ref_axis',(0.,1.,0.));
#31593=DIRECTION('',(0.,1.,0.));
#31594=DIRECTION('',(1.,0.,0.));
#31595=DIRECTION('',(0.,1.,0.));
#31596=DIRECTION('center_axis',(0.,0.894427190999916,0.447213595499957));
#31597=DIRECTION('ref_axis',(0.,-0.447213595499957,0.894427190999916));
#31598=DIRECTION('',(0.,-0.447213595499957,0.894427190999916));
#31599=DIRECTION('',(1.,0.,0.));
#31600=DIRECTION('',(0.,-0.447213595499957,0.894427190999916));
#31601=DIRECTION('center_axis',(0.,-0.894427190999916,0.447213595499957));
#31602=DIRECTION('ref_axis',(0.,-0.447213595499957,-0.894427190999916));
#31603=DIRECTION('',(0.,-0.447213595499957,-0.894427190999916));
#31604=DIRECTION('',(1.,0.,0.));
#31605=DIRECTION('',(0.,-0.447213595499957,-0.894427190999916));
#31606=DIRECTION('center_axis',(0.,0.,-1.));
#31607=DIRECTION('ref_axis',(0.,1.,0.));
#31608=DIRECTION('',(0.,1.,0.));
#31609=DIRECTION('',(1.,0.,0.));
#31610=DIRECTION('',(0.,1.,0.));
#31611=DIRECTION('center_axis',(0.,-1.,0.));
#31612=DIRECTION('ref_axis',(0.,0.,-1.));
#31613=DIRECTION('',(0.,0.,-1.));
#31614=DIRECTION('',(0.,0.,-1.));
#31615=DIRECTION('center_axis',(1.,0.,0.));
#31616=DIRECTION('ref_axis',(0.,0.,1.));
#31617=DIRECTION('center_axis',(1.,0.,0.));
#31618=DIRECTION('ref_axis',(0.,0.,1.));
#31619=DIRECTION('',(1.,0.,0.));
#31620=DIRECTION('center_axis',(1.,0.,0.));
#31621=DIRECTION('ref_axis',(0.,0.,1.));
#31622=DIRECTION('center_axis',(-1.,0.,0.));
#31623=DIRECTION('ref_axis',(0.,0.,1.));
#31624=DIRECTION('center_axis',(-1.,0.,0.));
#31625=DIRECTION('ref_axis',(0.,1.,0.));
#31626=DIRECTION('center_axis',(-1.,0.,0.));
#31627=DIRECTION('ref_axis',(0.,1.,0.));
#31628=DIRECTION('center_axis',(-1.,0.,0.));
#31629=DIRECTION('ref_axis',(0.,1.,0.));
#31630=DIRECTION('',(0.,0.,-1.));
#31631=DIRECTION('',(0.,-1.,0.));
#31632=DIRECTION('',(0.,0.,-1.));
#31633=DIRECTION('center_axis',(-1.,0.,0.));
#31634=DIRECTION('ref_axis',(0.,0.,1.));
#31635=DIRECTION('center_axis',(1.,0.,0.));
#31636=DIRECTION('ref_axis',(0.,0.,1.));
#31637=DIRECTION('',(1.,0.,0.));
#31638=DIRECTION('center_axis',(1.,0.,0.));
#31639=DIRECTION('ref_axis',(0.,0.,1.));
#31640=DIRECTION('center_axis',(-1.,0.,0.));
#31641=DIRECTION('ref_axis',(0.,0.,1.));
#31642=DIRECTION('center_axis',(1.,0.,0.));
#31643=DIRECTION('ref_axis',(0.,0.,1.));
#31644=DIRECTION('',(1.,0.,0.));
#31645=DIRECTION('center_axis',(1.,0.,0.));
#31646=DIRECTION('ref_axis',(0.,0.,1.));
#31647=DIRECTION('center_axis',(-1.,0.,0.));
#31648=DIRECTION('ref_axis',(0.,0.,1.));
#31649=DIRECTION('center_axis',(0.,0.,1.));
#31650=DIRECTION('ref_axis',(1.,0.,0.));
#31651=DIRECTION('',(0.,0.,1.));
#31652=DIRECTION('center_axis',(0.,0.,1.));
#31653=DIRECTION('ref_axis',(1.,0.,0.));
#31654=DIRECTION('center_axis',(0.,0.,-1.));
#31655=DIRECTION('ref_axis',(-1.,0.,0.));
#31656=DIRECTION('center_axis',(0.,0.,1.));
#31657=DIRECTION('ref_axis',(1.,0.,0.));
#31658=DIRECTION('',(0.,0.,1.));
#31659=DIRECTION('center_axis',(0.,0.,1.));
#31660=DIRECTION('ref_axis',(1.,0.,0.));
#31661=DIRECTION('center_axis',(0.,0.,-1.));
#31662=DIRECTION('ref_axis',(-1.,0.,0.));
#31663=DIRECTION('center_axis',(1.,0.,0.));
#31664=DIRECTION('ref_axis',(0.,-1.,0.));
#31665=DIRECTION('',(0.,0.,-1.));
#31666=DIRECTION('',(0.,1.,0.));
#31667=DIRECTION('center_axis',(0.,0.,-1.));
#31668=DIRECTION('ref_axis',(0.914708142118334,0.404115100859181,0.));
#31669=DIRECTION('center_axis',(0.,0.,1.));
#31670=DIRECTION('ref_axis',(0.914708142118334,0.404115100859181,0.));
#31671=DIRECTION('center_axis',(0.,0.,-1.));
#31672=DIRECTION('ref_axis',(0.,1.,0.));
#31673=DIRECTION('center_axis',(0.,0.,1.));
#31674=DIRECTION('ref_axis',(0.,1.,0.));
#31675=DIRECTION('',(0.,0.,-1.));
#31676=DIRECTION('center_axis',(0.,-1.,0.));
#31677=DIRECTION('ref_axis',(-1.,0.,0.));
#31678=DIRECTION('',(1.,0.,0.));
#31679=DIRECTION('',(0.,0.,-1.));
#31680=DIRECTION('center_axis',(0.,0.,-1.));
#31681=DIRECTION('ref_axis',(0.,-1.,0.));
#31682=DIRECTION('center_axis',(0.,0.,1.));
#31683=DIRECTION('ref_axis',(0.,-1.,0.));
#31684=DIRECTION('',(0.,0.,-1.));
#31685=DIRECTION('center_axis',(1.,0.,0.));
#31686=DIRECTION('ref_axis',(0.,-1.,0.));
#31687=DIRECTION('',(0.,1.,0.));
#31688=DIRECTION('',(0.,0.,-1.));
#31689=DIRECTION('center_axis',(0.,0.,-1.));
#31690=DIRECTION('ref_axis',(1.,0.,0.));
#31691=DIRECTION('center_axis',(0.,0.,1.));
#31692=DIRECTION('ref_axis',(1.,0.,0.));
#31693=DIRECTION('',(0.,0.,-1.));
#31694=DIRECTION('center_axis',(-0.160285849379284,0.987070639057186,0.));
#31695=DIRECTION('ref_axis',(0.987070639057186,0.160285849379284,0.));
#31696=DIRECTION('',(-0.987070639057186,-0.160285849379284,0.));
#31697=DIRECTION('',(0.,0.,-1.));
#31698=DIRECTION('center_axis',(0.,0.,-1.));
#31699=DIRECTION('ref_axis',(0.,1.,0.));
#31700=DIRECTION('center_axis',(0.,0.,1.));
#31701=DIRECTION('ref_axis',(0.,1.,0.));
#31702=DIRECTION('center_axis',(0.,0.,-1.));
#31703=DIRECTION('ref_axis',(-1.,0.,0.));
#31704=DIRECTION('center_axis',(0.,0.,1.));
#31705=DIRECTION('ref_axis',(-1.,0.,0.));
#31706=DIRECTION('',(0.,0.,-1.));
#31707=DIRECTION('center_axis',(-3.69197497485193E-16,-1.,0.));
#31708=DIRECTION('ref_axis',(-1.,3.69197497485193E-16,0.));
#31709=DIRECTION('',(1.,-3.69197497485193E-16,0.));
#31710=DIRECTION('',(0.,0.,-1.));
#31711=DIRECTION('center_axis',(0.,0.,-1.));
#31712=DIRECTION('ref_axis',(0.,-1.,0.));
#31713=DIRECTION('center_axis',(0.,0.,1.));
#31714=DIRECTION('ref_axis',(0.,-1.,0.));
#31715=DIRECTION('',(0.,0.,-1.));
#31716=DIRECTION('center_axis',(1.,0.,0.));
#31717=DIRECTION('ref_axis',(0.,-1.,0.));
#31718=DIRECTION('',(0.,0.,-1.));
#31719=DIRECTION('',(0.,-1.,0.));
#31720=DIRECTION('center_axis',(0.,0.,-1.));
#31721=DIRECTION('ref_axis',(1.,4.44089209850062E-16,0.));
#31722=DIRECTION('center_axis',(0.,0.,1.));
#31723=DIRECTION('ref_axis',(1.,4.44089209850062E-16,0.));
#31724=DIRECTION('',(0.,0.,-1.));
#31725=DIRECTION('center_axis',(0.160285849379284,0.987070639057186,0.));
#31726=DIRECTION('ref_axis',(0.987070639057186,-0.160285849379284,0.));
#31727=DIRECTION('',(0.987070639057186,-0.160285849379284,0.));
#31728=DIRECTION('',(0.,0.,-1.));
#31729=DIRECTION('center_axis',(0.,0.,-1.));
#31730=DIRECTION('ref_axis',(0.,1.,0.));
#31731=DIRECTION('center_axis',(0.,0.,1.));
#31732=DIRECTION('ref_axis',(0.,1.,0.));
#31733=DIRECTION('',(0.,0.,-1.));
#31734=DIRECTION('center_axis',(-1.,0.,0.));
#31735=DIRECTION('ref_axis',(0.,1.,0.));
#31736=DIRECTION('',(0.,1.,0.));
#31737=DIRECTION('',(0.,0.,-1.));
#31738=DIRECTION('center_axis',(0.,0.,-1.));
#31739=DIRECTION('ref_axis',(-1.,0.,0.));
#31740=DIRECTION('center_axis',(0.,0.,1.));
#31741=DIRECTION('ref_axis',(-1.,0.,0.));
#31742=DIRECTION('',(0.,0.,-1.));
#31743=DIRECTION('center_axis',(0.,-1.,0.));
#31744=DIRECTION('ref_axis',(-1.,0.,0.));
#31745=DIRECTION('',(-1.,0.,0.));
#31746=DIRECTION('',(0.,0.,-1.));
#31747=DIRECTION('center_axis',(0.,0.,-1.));
#31748=DIRECTION('ref_axis',(1.,0.,0.));
#31749=DIRECTION('center_axis',(0.,0.,1.));
#31750=DIRECTION('ref_axis',(1.,0.,0.));
#31751=DIRECTION('',(0.,0.,-1.));
#31752=DIRECTION('center_axis',(-1.,0.,0.));
#31753=DIRECTION('ref_axis',(0.,1.,0.));
#31754=DIRECTION('',(0.,0.,-1.));
#31755=DIRECTION('',(0.,1.,0.));
#31756=DIRECTION('center_axis',(0.,0.,-1.));
#31757=DIRECTION('ref_axis',(-0.374029024133323,0.927416998499529,0.));
#31758=DIRECTION('center_axis',(0.,0.,1.));
#31759=DIRECTION('ref_axis',(-0.374029024133323,0.927416998499529,0.));
#31760=DIRECTION('center_axis',(0.,0.,1.));
#31761=DIRECTION('ref_axis',(1.,0.,0.));
#31762=DIRECTION('axis',(0.,0.,1.));
#31763=DIRECTION('refdir',(1.,0.,0.));
#31764=DIRECTION('axis',(0.,0.,1.));
#31765=DIRECTION('refdir',(1.,0.,0.));
#31766=DIRECTION('center_axis',(1.,6.57957785206009E-13,0.));
#31767=DIRECTION('ref_axis',(0.,0.,1.));
#31768=DIRECTION('center_axis',(1.,6.58286732145141E-13,0.));
#31769=DIRECTION('ref_axis',(0.,0.,1.));
#31770=DIRECTION('',(1.,6.57957785206009E-13,0.));
#31771=DIRECTION('center_axis',(-1.,3.28954970259306E-16,0.));
#31772=DIRECTION('ref_axis',(0.,0.,1.));
#31773=DIRECTION('center_axis',(-1.,-6.58286732145141E-13,0.));
#31774=DIRECTION('ref_axis',(0.,0.,1.));
#31775=DIRECTION('center_axis',(0.999999999362884,-3.56963971004376E-5,
0.));
#31776=DIRECTION('ref_axis',(0.,0.,1.));
#31777=DIRECTION('center_axis',(0.999999999362884,-3.56963971007665E-5,
0.));
#31778=DIRECTION('ref_axis',(0.,0.,1.));
#31779=DIRECTION('',(0.999999999362884,-3.56963971004376E-5,0.));
#31780=DIRECTION('center_axis',(0.999999999362884,-3.56963971007665E-5,
0.));
#31781=DIRECTION('ref_axis',(0.,0.,1.));
#31782=DIRECTION('center_axis',(-0.999999999362884,3.56963971007665E-5,
0.));
#31783=DIRECTION('ref_axis',(0.,0.,1.));
#31784=DIRECTION('center_axis',(-0.999999999362884,3.56963971010297E-5,
0.));
#31785=DIRECTION('ref_axis',(-2.52411644540658E-5,-0.707106780736035,0.707106781186551));
#31786=DIRECTION('',(0.999999999362884,-3.56963971010297E-5,0.));
#31787=DIRECTION('center_axis',(-0.999999999362884,3.56963970959969E-5,
0.));
#31788=DIRECTION('ref_axis',(-3.56963970959969E-5,-0.999999999362884,0.));
#31789=DIRECTION('',(-0.999999999362884,3.56963971010297E-5,0.));
#31790=DIRECTION('center_axis',(0.970304361397857,0.24188725938399,0.));
#31791=DIRECTION('ref_axis',(0.24188725938399,-0.970304361397857,0.));
#31792=DIRECTION('center_axis',(0.999999999840721,-1.7848198553344E-5,0.));
#31793=DIRECTION('ref_axis',(-1.26205822290334E-5,-0.707106781073918,0.70710678118655));
#31794=DIRECTION('',(0.999999999840721,-1.7848198553344E-5,0.));
#31795=DIRECTION('center_axis',(-0.999999999840721,1.78481985546597E-5,
0.));
#31796=DIRECTION('ref_axis',(-1.78481985546597E-5,-0.999999999840721,0.));
#31797=DIRECTION('',(-0.999999999840721,1.7848198553344E-5,0.));
#31798=DIRECTION('center_axis',(0.,-1.,0.));
#31799=DIRECTION('ref_axis',(0.707106781186548,0.,0.707106781186548));
#31800=DIRECTION('center_axis',(0.,-1.,0.));
#31801=DIRECTION('ref_axis',(1.,0.,0.));
#31802=DIRECTION('',(0.,-1.,0.));
#31803=DIRECTION('center_axis',(0.,1.,0.));
#31804=DIRECTION('ref_axis',(0.,0.,1.));
#31805=DIRECTION('',(0.,1.,0.));
#31806=DIRECTION('center_axis',(0.,0.,-1.));
#31807=DIRECTION('ref_axis',(-1.,0.,0.));
#31808=DIRECTION('center_axis',(-1.,0.,0.));
#31809=DIRECTION('ref_axis',(0.,0.,1.));
#31810=DIRECTION('center_axis',(0.,0.,-1.));
#31811=DIRECTION('ref_axis',(-0.707106781186545,-0.70710678118655,0.));
#31812=DIRECTION('center_axis',(0.,0.,1.));
#31813=DIRECTION('ref_axis',(-0.707106781186545,-0.70710678118655,0.));
#31814=DIRECTION('center_axis',(1.,0.,0.));
#31815=DIRECTION('ref_axis',(0.,0.707106781186548,0.707106781186548));
#31816=DIRECTION('center_axis',(-1.,0.,0.));
#31817=DIRECTION('ref_axis',(0.,0.,1.));
#31818=DIRECTION('',(-1.,0.,0.));
#31819=DIRECTION('',(1.,0.,0.));
#31820=DIRECTION('center_axis',(0.,0.,-1.));
#31821=DIRECTION('ref_axis',(-1.,0.,0.));
#31822=DIRECTION('center_axis',(-0.707106781186545,0.70710678118655,0.));
#31823=DIRECTION('ref_axis',(0.,0.,1.));
#31824=DIRECTION('center_axis',(0.,0.,1.));
#31825=DIRECTION('ref_axis',(0.382683432365091,0.923879532511286,0.));
#31826=DIRECTION('center_axis',(0.,0.,-1.));
#31827=DIRECTION('ref_axis',(0.382683432365091,0.923879532511286,0.));
#31828=DIRECTION('center_axis',(0.707106781186548,-0.707106781186547,0.));
#31829=DIRECTION('ref_axis',(0.5,0.500000000000001,0.707106781186547));
#31830=DIRECTION('center_axis',(-0.707106781186548,0.707106781186548,0.));
#31831=DIRECTION('ref_axis',(0.,0.,1.));
#31832=DIRECTION('',(-0.707106781186548,0.707106781186547,0.));
#31833=DIRECTION('',(0.707106781186548,-0.707106781186547,0.));
#31834=DIRECTION('center_axis',(0.,0.,-1.));
#31835=DIRECTION('ref_axis',(-1.,0.,0.));
#31836=DIRECTION('center_axis',(0.,1.,0.));
#31837=DIRECTION('ref_axis',(0.,0.,1.));
#31838=DIRECTION('center_axis',(0.,0.,1.));
#31839=DIRECTION('ref_axis',(0.923879532511287,0.38268343236509,0.));
#31840=DIRECTION('center_axis',(0.,0.,-1.));
#31841=DIRECTION('ref_axis',(0.923879532511287,0.38268343236509,0.));
#31842=DIRECTION('center_axis',(-3.28954970259306E-16,-1.,0.));
#31843=DIRECTION('ref_axis',(0.707106781186548,-2.32606290175374E-16,0.707106781186548));
#31844=DIRECTION('center_axis',(0.,1.,0.));
#31845=DIRECTION('ref_axis',(0.,0.,1.));
#31846=DIRECTION('',(3.28954970259306E-16,1.,0.));
#31847=DIRECTION('',(-3.28954970259306E-16,-1.,0.));
#31848=DIRECTION('center_axis',(1.,0.,0.));
#31849=DIRECTION('ref_axis',(0.,0.,1.));
#31850=DIRECTION('center_axis',(0.,0.,1.));
#31851=DIRECTION('ref_axis',(0.707106781186546,-0.707106781186549,0.));
#31852=DIRECTION('center_axis',(0.,0.,-1.));
#31853=DIRECTION('ref_axis',(0.707106781186547,-0.707106781186548,0.));
#31854=DIRECTION('center_axis',(-1.,0.,0.));
#31855=DIRECTION('ref_axis',(0.,-0.707106781186548,0.707106781186548));
#31856=DIRECTION('',(1.,0.,0.));
#31857=DIRECTION('',(-1.,0.,0.));
#31858=DIRECTION('center_axis',(0.92387953251129,-0.382683432365083,0.));
#31859=DIRECTION('ref_axis',(0.382683432365083,0.92387953251129,0.));
#31860=DIRECTION('center_axis',(-0.707106781186548,0.707106781186547,0.));
#31861=DIRECTION('ref_axis',(-0.499999999999999,-0.499999999999999,0.707106781186549));
#31862=DIRECTION('',(0.707106781186548,-0.707106781186547,0.));
#31863=DIRECTION('',(-0.707106781186548,0.707106781186547,0.));
#31864=DIRECTION('center_axis',(0.382683432365083,-0.92387953251129,0.));
#31865=DIRECTION('ref_axis',(0.92387953251129,0.382683432365083,0.));
#31866=DIRECTION('center_axis',(0.,1.,0.));
#31867=DIRECTION('ref_axis',(-0.707106781186551,0.,0.707106781186544));
#31868=DIRECTION('',(0.,1.,0.));
#31869=DIRECTION('center_axis',(0.,-1.,0.));
#31870=DIRECTION('ref_axis',(0.,0.,1.));
#31871=DIRECTION('',(0.,-1.,0.));
#31872=DIRECTION('center_axis',(0.,0.,-1.));
#31873=DIRECTION('ref_axis',(-1.,0.,0.));
#31874=DIRECTION('center_axis',(0.88294759285893,-0.469471562785885,0.));
#31875=DIRECTION('ref_axis',(0.,0.,1.));
#31876=DIRECTION('center_axis',(0.,0.,-1.));
#31877=DIRECTION('ref_axis',(0.857167300702112,0.515038074910055,0.));
#31878=DIRECTION('center_axis',(0.,0.,1.));
#31879=DIRECTION('ref_axis',(0.857167300702112,0.515038074910055,0.));
#31880=DIRECTION('center_axis',(-0.882947592858928,0.46947156278589,0.));
#31881=DIRECTION('ref_axis',(-0.331966525620151,-0.624338230342891,0.707106781186542));
#31882=DIRECTION('',(0.882947592858928,-0.46947156278589,0.));
#31883=DIRECTION('',(-0.882947592858928,0.46947156278589,0.));
#31884=DIRECTION('center_axis',(0.970295726275989,-0.241921895599697,0.));
#31885=DIRECTION('ref_axis',(-0.241921895599697,-0.970295726275989,0.));
#31886=DIRECTION('center_axis',(-1.,0.,0.));
#31887=DIRECTION('ref_axis',(0.,-0.707106781186548,0.707106781186548));
#31888=DIRECTION('',(1.,0.,0.));
#31889=DIRECTION('',(-1.,0.,0.));
#31890=DIRECTION('center_axis',(-0.882964350739721,-0.469440044438886,0.));
#31891=DIRECTION('ref_axis',(0.331944238783253,-0.624350079954038,0.707106781186543));
#31892=DIRECTION('',(-0.882964350739721,-0.469440044438886,0.));
#31893=DIRECTION('center_axis',(0.882964350739719,0.46944004443889,0.));
#31894=DIRECTION('ref_axis',(0.,0.,1.));
#31895=DIRECTION('',(0.882964350739721,0.469440044438886,0.));
#31896=DIRECTION('center_axis',(0.,0.,-1.));
#31897=DIRECTION('ref_axis',(-1.,0.,0.));
#31898=DIRECTION('center_axis',(3.56963971004376E-5,0.999999999362884,0.));
#31899=DIRECTION('ref_axis',(0.,0.,1.));
#31900=DIRECTION('center_axis',(0.,0.,-1.));
#31901=DIRECTION('ref_axis',(-0.857148915152355,0.51506867236626,0.));
#31902=DIRECTION('center_axis',(0.,0.,1.));
#31903=DIRECTION('ref_axis',(-0.857148915152355,0.51506867236626,0.));
#31904=DIRECTION('center_axis',(-3.56963971014961E-5,-0.999999999362884,
0.));
#31905=DIRECTION('ref_axis',(0.707106780736038,-2.52411644543957E-5,0.707106781186548));
#31906=DIRECTION('',(3.56963971014961E-5,0.999999999362884,0.));
#31907=DIRECTION('',(-3.56963971014961E-5,-0.999999999362884,0.));
#31908=DIRECTION('center_axis',(0.382716411291948,0.9238658715029,0.));
#31909=DIRECTION('ref_axis',(-0.9238658715029,0.382716411291948,0.));
#31910=DIRECTION('center_axis',(-0.707132021900493,-0.707081539571584,0.));
#31911=DIRECTION('ref_axis',(0.499982151482891,-0.500017847879993,0.707106781186548));
#31912=DIRECTION('',(-0.707132021900493,-0.707081539571584,0.));
#31913=DIRECTION('center_axis',(0.923893192342431,0.382650452950617,-6.50651058246798E-15));
#31914=DIRECTION('ref_axis',(-0.382650452950617,0.923893192342431,1.57081060919186E-14));
#31915=DIRECTION('',(0.707132021900493,0.707081539571584,0.));
#31916=DIRECTION('center_axis',(-0.999999999362884,3.5696397100931E-5,0.));
#31917=DIRECTION('ref_axis',(-2.52411644539961E-5,-0.707106780736038,0.707106781186548));
#31918=DIRECTION('',(-0.999999999362884,3.5696397100931E-5,0.));
#31919=DIRECTION('center_axis',(0.999999999362884,-3.56963971004377E-5,
0.));
#31920=DIRECTION('ref_axis',(0.,0.,1.));
#31921=DIRECTION('',(0.999999999362884,-3.5696397100931E-5,0.));
#31922=DIRECTION('center_axis',(-3.56963971048783E-5,-0.999999999362884,
0.));
#31923=DIRECTION('ref_axis',(0.,0.,1.));
#31924=DIRECTION('center_axis',(0.,0.,1.));
#31925=DIRECTION('ref_axis',(-0.707132021900492,-0.707081539571584,0.));
#31926=DIRECTION('center_axis',(0.,0.,-1.));
#31927=DIRECTION('ref_axis',(-0.707132021900492,-0.707081539571584,0.));
#31928=DIRECTION('center_axis',(3.56963971007665E-5,0.999999999362884,0.));
#31929=DIRECTION('ref_axis',(-0.707106780736035,2.52411644538797E-5,0.707106781186551));
#31930=DIRECTION('center_axis',(-3.56963971004377E-5,-0.999999999362884,
0.));
#31931=DIRECTION('ref_axis',(0.,0.,1.));
#31932=DIRECTION('',(-3.56963971007665E-5,-0.999999999362884,0.));
#31933=DIRECTION('',(3.56963971007665E-5,0.999999999362884,0.));
#31934=DIRECTION('center_axis',(0.,0.,-1.));
#31935=DIRECTION('ref_axis',(-1.,0.,0.));
#31936=DIRECTION('center_axis',(-0.707132021900495,-0.707081539571582,0.));
#31937=DIRECTION('ref_axis',(0.,0.,1.));
#31938=DIRECTION('center_axis',(0.,0.,1.));
#31939=DIRECTION('ref_axis',(-0.923865871502902,0.382716411291943,0.));
#31940=DIRECTION('center_axis',(0.,0.,-1.));
#31941=DIRECTION('ref_axis',(-0.923865871502902,0.382716411291943,0.));
#31942=DIRECTION('center_axis',(0.707132021900493,0.707081539571584,0.));
#31943=DIRECTION('ref_axis',(-0.499982151482891,0.500017847879993,0.707106781186548));
#31944=DIRECTION('center_axis',(-0.70713202190049,-0.707081539571586,0.));
#31945=DIRECTION('ref_axis',(0.,0.,1.));
#31946=DIRECTION('',(-0.707132021900493,-0.707081539571584,0.));
#31947=DIRECTION('',(0.707132021900493,0.707081539571584,0.));
#31948=DIRECTION('center_axis',(0.,0.,-1.));
#31949=DIRECTION('ref_axis',(-1.,0.,0.));
#31950=DIRECTION('center_axis',(-0.999999999362884,3.56963971004377E-5,
0.));
#31951=DIRECTION('ref_axis',(0.,0.,1.));
#31952=DIRECTION('center_axis',(0.,0.,1.));
#31953=DIRECTION('ref_axis',(-0.382650452950611,0.923893192342433,0.));
#31954=DIRECTION('center_axis',(0.,0.,-1.));
#31955=DIRECTION('ref_axis',(-0.382650452950611,0.923893192342433,0.));
#31956=DIRECTION('center_axis',(0.999999999362884,-3.56963971021026E-5,
0.));
#31957=DIRECTION('ref_axis',(2.52411644548245E-5,0.707106780736035,0.707106781186551));
#31958=DIRECTION('center_axis',(-0.999999999362884,3.5696397104879E-5,0.));
#31959=DIRECTION('ref_axis',(0.,0.,1.));
#31960=DIRECTION('',(-0.999999999362884,3.56963971021026E-5,0.));
#31961=DIRECTION('',(0.999999999362884,-3.56963971021026E-5,0.));
#31962=DIRECTION('center_axis',(0.,0.,-1.));
#31963=DIRECTION('ref_axis',(-1.,0.,0.));
#31964=DIRECTION('center_axis',(-3.56963971004376E-5,-0.999999999362884,
0.));
#31965=DIRECTION('ref_axis',(0.,0.,1.));
#31966=DIRECTION('center_axis',(0.,0.,-1.));
#31967=DIRECTION('ref_axis',(0.707081539571587,-0.70713202190049,0.));
#31968=DIRECTION('center_axis',(0.,0.,1.));
#31969=DIRECTION('ref_axis',(0.707081539571586,-0.70713202190049,0.));
#31970=DIRECTION('center_axis',(3.56963971011028E-5,0.999999999362884,0.));
#31971=DIRECTION('ref_axis',(-0.707106780736038,2.52411644541176E-5,0.707106781186548));
#31972=DIRECTION('center_axis',(-3.56963970915558E-5,-0.999999999362884,
0.));
#31973=DIRECTION('ref_axis',(0.,0.,1.));
#31974=DIRECTION('',(-3.56963971011028E-5,-0.999999999362884,0.));
#31975=DIRECTION('',(3.56963971011028E-5,0.999999999362884,0.));
#31976=DIRECTION('center_axis',(1.,0.,0.));
#31977=DIRECTION('ref_axis',(0.,0.707106781186554,0.707106781186541));
#31978=DIRECTION('center_axis',(1.,0.,0.));
#31979=DIRECTION('ref_axis',(0.,1.,0.));
#31980=DIRECTION('',(1.,0.,0.));
#31981=DIRECTION('center_axis',(-1.,0.,0.));
#31982=DIRECTION('ref_axis',(0.,0.,1.));
#31983=DIRECTION('',(-1.,0.,0.));
#31984=DIRECTION('center_axis',(-0.999999999840721,1.78481985534681E-5,
0.));
#31985=DIRECTION('ref_axis',(1.26205822291212E-5,0.707106781073918,0.70710678118655));
#31986=DIRECTION('',(-0.999999999840721,1.78481985534681E-5,0.));
#31987=DIRECTION('center_axis',(0.999999999840721,-1.78481985546596E-5,
0.));
#31988=DIRECTION('ref_axis',(1.78481985546596E-5,0.999999999840721,0.));
#31989=DIRECTION('',(0.999999999840721,-1.78481985534681E-5,0.));
#31990=DIRECTION('center_axis',(0.999999999362884,-3.56963971040562E-5,
0.));
#31991=DIRECTION('ref_axis',(2.52411644562058E-5,0.707106780736035,0.707106781186551));
#31992=DIRECTION('',(-0.999999999362884,3.56963971040562E-5,0.));
#31993=DIRECTION('center_axis',(0.999999999362884,-3.5696397104879E-5,0.));
#31994=DIRECTION('ref_axis',(3.5696397104879E-5,0.999999999362884,0.));
#31995=DIRECTION('',(0.999999999362884,-3.56963971040562E-5,0.));
#31996=DIRECTION('center_axis',(-0.816511153790762,-0.408241003122002,-0.408226431169298));
#31997=DIRECTION('ref_axis',(-0.577329659497308,0.577370878146268,0.577350269189622));
#31998=DIRECTION('center_axis',(0.,0.,1.));
#31999=DIRECTION('ref_axis',(-0.999999999362884,3.56963970915558E-5,0.));
#32000=DIRECTION('center_axis',(0.408248290463868,-0.816496580927721,0.408248290463868));
#32001=DIRECTION('ref_axis',(0.577350269189616,0.577350269189634,0.577350269189627));
#32002=DIRECTION('center_axis',(0.,0.,1.));
#32003=DIRECTION('ref_axis',(-4.44089209850064E-15,1.,0.));
#32004=DIRECTION('center_axis',(0.469440044438886,-0.882964350739721,0.));
#32005=DIRECTION('ref_axis',(-0.882964350739721,-0.469440044438886,0.));
#32006=DIRECTION('',(0.,0.,-1.));
#32007=DIRECTION('',(-0.882964350739721,-0.469440044438886,0.));
#32008=DIRECTION('',(0.,0.,-1.));
#32009=DIRECTION('center_axis',(0.,0.,-1.));
#32010=DIRECTION('ref_axis',(-0.999999999362884,3.56963971004376E-5,0.));
#32011=DIRECTION('',(0.,0.,-1.));
#32012=DIRECTION('center_axis',(0.,0.,1.));
#32013=DIRECTION('ref_axis',(-0.857148915152355,0.51506867236626,0.));
#32014=DIRECTION('center_axis',(0.999999999362884,-3.56963971014961E-5,
0.));
#32015=DIRECTION('ref_axis',(-3.56963971014961E-5,-0.999999999362884,0.));
#32016=DIRECTION('',(0.,0.,-1.));
#32017=DIRECTION('',(-3.56963971014961E-5,-0.999999999362884,0.));
#32018=DIRECTION('center_axis',(0.707081539571584,-0.707132021900493,0.));
#32019=DIRECTION('ref_axis',(-0.707132021900493,-0.707081539571584,0.));
#32020=DIRECTION('',(0.,0.,-1.));
#32021=DIRECTION('',(-0.707132021900493,-0.707081539571584,0.));
#32022=DIRECTION('center_axis',(-3.5696397100931E-5,-0.999999999362884,
0.));
#32023=DIRECTION('ref_axis',(-0.999999999362884,3.5696397100931E-5,0.));
#32024=DIRECTION('',(0.,0.,-1.));
#32025=DIRECTION('',(-0.999999999362884,3.5696397100931E-5,0.));
#32026=DIRECTION('center_axis',(0.,0.,-1.));
#32027=DIRECTION('ref_axis',(-3.56963971004376E-5,-0.999999999362884,0.));
#32028=DIRECTION('',(0.,0.,-1.));
#32029=DIRECTION('center_axis',(0.,0.,-1.));
#32030=DIRECTION('ref_axis',(-0.707132021900492,-0.707081539571584,0.));
#32031=DIRECTION('center_axis',(-0.999999999362884,3.56963971007665E-5,
0.));
#32032=DIRECTION('ref_axis',(3.56963971007665E-5,0.999999999362884,0.));
#32033=DIRECTION('',(0.,0.,-1.));
#32034=DIRECTION('',(3.56963971007665E-5,0.999999999362884,0.));
#32035=DIRECTION('center_axis',(0.,0.,-1.));
#32036=DIRECTION('ref_axis',(-0.999999999362884,3.56963971013258E-5,0.));
#32037=DIRECTION('',(0.,0.,-1.));
#32038=DIRECTION('center_axis',(0.,0.,-1.));
#32039=DIRECTION('ref_axis',(-0.923865871502902,0.382716411291943,0.));
#32040=DIRECTION('center_axis',(-0.707081539571584,0.707132021900493,0.));
#32041=DIRECTION('ref_axis',(0.707132021900493,0.707081539571584,0.));
#32042=DIRECTION('',(0.,0.,-1.));
#32043=DIRECTION('',(0.707132021900493,0.707081539571584,0.));
#32044=DIRECTION('center_axis',(0.,0.,-1.));
#32045=DIRECTION('ref_axis',(-0.707081539571585,0.707132021900492,0.));
#32046=DIRECTION('',(0.,0.,-1.));
#32047=DIRECTION('center_axis',(0.,0.,1.));
#32048=DIRECTION('ref_axis',(-0.707081539571585,0.707132021900492,0.));
#32049=DIRECTION('',(0.,0.,-1.));
#32050=DIRECTION('center_axis',(0.,0.,-1.));
#32051=DIRECTION('ref_axis',(-0.674257203707391,0.738496596639883,0.));
#32052=DIRECTION('center_axis',(3.56963971021026E-5,0.999999999362884,0.));
#32053=DIRECTION('ref_axis',(0.999999999362884,-3.56963971021026E-5,0.));
#32054=DIRECTION('',(0.,0.,-1.));
#32055=DIRECTION('',(-0.999999999362884,3.56963971021026E-5,0.));
#32056=DIRECTION('center_axis',(0.,0.,-1.));
#32057=DIRECTION('ref_axis',(0.999999999362884,-3.56963970980596E-5,0.));
#32058=DIRECTION('',(0.,0.,-1.));
#32059=DIRECTION('center_axis',(0.,0.,-1.));
#32060=DIRECTION('ref_axis',(0.999999999362884,-3.56963970980596E-5,0.));
#32061=DIRECTION('center_axis',(-0.999999999362884,3.56963971011028E-5,
0.));
#32062=DIRECTION('ref_axis',(3.56963971011028E-5,0.999999999362884,0.));
#32063=DIRECTION('',(0.,0.,-1.));
#32064=DIRECTION('',(3.56963971011028E-5,0.999999999362884,0.));
#32065=DIRECTION('',(0.,0.,1.));
#32066=DIRECTION('',(-3.56963971011028E-5,-0.999999999362884,0.));
#32067=DIRECTION('center_axis',(0.,0.,-1.));
#32068=DIRECTION('ref_axis',(-0.999999999362884,3.56963970915558E-5,0.));
#32069=DIRECTION('',(0.,0.,-1.));
#32070=DIRECTION('center_axis',(0.,0.,-1.));
#32071=DIRECTION('ref_axis',(-0.999999999362884,3.56963970915558E-5,0.));
#32072=DIRECTION('center_axis',(3.56963971040562E-5,0.999999999362884,0.));
#32073=DIRECTION('ref_axis',(0.999999999362884,-3.56963971040562E-5,0.));
#32074=DIRECTION('',(0.,0.,-1.));
#32075=DIRECTION('',(0.999999999362884,-3.56963971040562E-5,0.));
#32076=DIRECTION('center_axis',(1.78481985534681E-5,0.999999999840721,0.));
#32077=DIRECTION('ref_axis',(0.999999999840721,-1.78481985534681E-5,0.));
#32078=DIRECTION('',(0.,0.,-1.));
#32079=DIRECTION('',(0.999999999840721,-1.78481985534681E-5,0.));
#32080=DIRECTION('center_axis',(0.,1.,0.));
#32081=DIRECTION('ref_axis',(1.,0.,0.));
#32082=DIRECTION('',(0.,0.,-1.));
#32083=DIRECTION('',(1.,0.,0.));
#32084=DIRECTION('center_axis',(0.,0.,-1.));
#32085=DIRECTION('ref_axis',(-1.,0.,0.));
#32086=DIRECTION('center_axis',(3.56963971011028E-5,0.999999999362884,0.));
#32087=DIRECTION('ref_axis',(-0.707106780736038,2.52411644541176E-5,-0.707106781186548));
#32088=DIRECTION('center_axis',(-3.56963970915558E-5,-0.999999999362884,
0.));
#32089=DIRECTION('ref_axis',(-0.999999999362884,3.56963970915558E-5,0.));
#32090=DIRECTION('',(-3.56963971011028E-5,-0.999999999362884,0.));
#32091=DIRECTION('center_axis',(0.,0.,1.));
#32092=DIRECTION('ref_axis',(1.,0.,0.));
#32093=DIRECTION('center_axis',(0.,0.,-1.));
#32094=DIRECTION('ref_axis',(0.880581945986775,-0.473893908382608,0.));
#32095=DIRECTION('center_axis',(0.,0.,1.));
#32096=DIRECTION('ref_axis',(0.880581945986775,-0.473893908382608,0.));
#32097=DIRECTION('center_axis',(0.999999999362884,-3.56963971040562E-5,
0.));
#32098=DIRECTION('ref_axis',(2.52411644562058E-5,0.707106780736035,-0.707106781186551));
#32099=DIRECTION('center_axis',(-0.999999999362884,3.56963971004374E-5,
0.));
#32100=DIRECTION('ref_axis',(3.56963971004374E-5,0.999999999362884,0.));
#32101=DIRECTION('',(-0.999999999362884,3.56963971040562E-5,0.));
#32102=DIRECTION('center_axis',(0.999999999362884,-3.56963971048783E-5,
0.));
#32103=DIRECTION('ref_axis',(0.,0.,-1.));
#32104=DIRECTION('center_axis',(0.999999999840721,-1.78481985534681E-5,
0.));
#32105=DIRECTION('ref_axis',(1.26205822291212E-5,0.707106781073918,-0.70710678118655));
#32106=DIRECTION('center_axis',(-0.999999999840721,1.78481985457778E-5,
0.));
#32107=DIRECTION('ref_axis',(1.78481985457778E-5,0.999999999840721,0.));
#32108=DIRECTION('',(-0.999999999840721,1.78481985534681E-5,0.));
#32109=DIRECTION('center_axis',(1.,0.,0.));
#32110=DIRECTION('ref_axis',(0.,0.707106781186554,-0.707106781186541));
#32111=DIRECTION('center_axis',(-1.,0.,0.));
#32112=DIRECTION('ref_axis',(0.,1.,0.));
#32113=DIRECTION('',(-1.,0.,0.));
#32114=DIRECTION('center_axis',(-0.816511153790763,-0.408241003122,0.408226431169296));
#32115=DIRECTION('ref_axis',(-0.57732965949731,0.577370878146255,-0.577350269189634));
#32116=DIRECTION('center_axis',(0.,0.,1.));
#32117=DIRECTION('ref_axis',(-0.836963911810301,-0.547258083839059,0.));
#32118=DIRECTION('center_axis',(0.,0.,1.));
#32119=DIRECTION('ref_axis',(-0.880598861730879,-0.473862474477859,0.));
#32120=DIRECTION('center_axis',(0.,0.,-1.));
#32121=DIRECTION('ref_axis',(-0.88059886173088,-0.473862474477859,0.));
#32122=DIRECTION('center_axis',(0.,-1.,0.));
#32123=DIRECTION('ref_axis',(0.707106781186548,0.,-0.707106781186548));
#32124=DIRECTION('',(0.,1.,0.));
#32125=DIRECTION('center_axis',(0.,-1.,0.));
#32126=DIRECTION('ref_axis',(0.,0.,-1.));
#32127=DIRECTION('',(0.,-1.,0.));
#32128=DIRECTION('center_axis',(0.408248290463864,-0.816496580927721,-0.408248290463871));
#32129=DIRECTION('ref_axis',(0.577350269189621,0.577350269189625,-0.577350269189632));
#32130=DIRECTION('center_axis',(0.,0.,-1.));
#32131=DIRECTION('ref_axis',(-4.44089209850064E-15,1.,0.));
#32132=DIRECTION('center_axis',(0.707132021900493,0.707081539571584,0.));
#32133=DIRECTION('ref_axis',(-0.499982151482891,0.500017847879993,-0.707106781186548));
#32134=DIRECTION('',(-0.707132021900493,-0.707081539571584,0.));
#32135=DIRECTION('center_axis',(-0.707132021900495,-0.707081539571582,0.));
#32136=DIRECTION('ref_axis',(-0.707081539571582,0.707132021900495,0.));
#32137=DIRECTION('center_axis',(-0.70713202190049,-0.707081539571586,0.));
#32138=DIRECTION('ref_axis',(-0.707081539571586,0.70713202190049,0.));
#32139=DIRECTION('center_axis',(0.,0.,-1.));
#32140=DIRECTION('ref_axis',(-1.,0.,0.));
#32141=DIRECTION('',(-0.707106781186548,0.707106781186547,0.));
#32142=DIRECTION('center_axis',(0.,0.,1.));
#32143=DIRECTION('ref_axis',(0.923879532511287,0.38268343236509,0.));
#32144=DIRECTION('',(3.28954970259306E-16,1.,0.));
#32145=DIRECTION('center_axis',(0.,0.,1.));
#32146=DIRECTION('ref_axis',(0.707106781186547,-0.707106781186548,0.));
#32147=DIRECTION('',(1.,0.,0.));
#32148=DIRECTION('',(0.707106781186548,-0.707106781186547,0.));
#32149=DIRECTION('',(0.,-1.,0.));
#32150=DIRECTION('center_axis',(0.,0.,-1.));
#32151=DIRECTION('ref_axis',(0.857167300702112,0.515038074910055,0.));
#32152=DIRECTION('',(0.882947592858928,-0.46947156278589,0.));
#32153=DIRECTION('',(1.,0.,0.));
#32154=DIRECTION('',(0.999999999840721,-1.7848198553344E-5,0.));
#32155=DIRECTION('',(0.999999999362884,-3.56963971010297E-5,0.));
#32156=DIRECTION('',(0.882964350739721,0.469440044438886,0.));
#32157=DIRECTION('center_axis',(0.,0.,-1.));
#32158=DIRECTION('ref_axis',(-0.857148915152355,0.51506867236626,0.));
#32159=DIRECTION('',(3.56963971014961E-5,0.999999999362884,0.));
#32160=DIRECTION('',(0.707132021900493,0.707081539571584,0.));
#32161=DIRECTION('',(0.999999999362884,-3.5696397100931E-5,0.));
#32162=DIRECTION('center_axis',(0.,0.,1.));
#32163=DIRECTION('ref_axis',(-0.707132021900492,-0.707081539571584,0.));
#32164=DIRECTION('',(-3.56963971007665E-5,-0.999999999362884,0.));
#32165=DIRECTION('center_axis',(0.,0.,1.));
#32166=DIRECTION('ref_axis',(-0.923865871502902,0.382716411291943,0.));
#32167=DIRECTION('center_axis',(0.707106781186548,-0.707106781186547,0.));
#32168=DIRECTION('ref_axis',(0.5,0.500000000000001,-0.707106781186547));
#32169=DIRECTION('center_axis',(-0.707106781186548,0.707106781186548,0.));
#32170=DIRECTION('ref_axis',(0.707106781186548,0.707106781186548,0.));
#32171=DIRECTION('',(0.707106781186548,-0.707106781186547,0.));
#32172=DIRECTION('center_axis',(-0.707106781186548,0.707106781186548,0.));
#32173=DIRECTION('ref_axis',(0.707106781186548,0.707106781186548,0.));
#32174=DIRECTION('center_axis',(0.,0.,-1.));
#32175=DIRECTION('ref_axis',(-1.,0.,0.));
#32176=DIRECTION('center_axis',(0.,0.,-1.));
#32177=DIRECTION('ref_axis',(0.674283564945582,0.738472527616483,0.));
#32178=DIRECTION('center_axis',(-0.999999999362884,3.5696397100931E-5,0.));
#32179=DIRECTION('ref_axis',(-2.52411644539961E-5,-0.707106780736038,-0.707106781186548));
#32180=DIRECTION('center_axis',(0.999999999362884,-3.56963971004376E-5,
0.));
#32181=DIRECTION('ref_axis',(-3.56963971004376E-5,-0.999999999362884,0.));
#32182=DIRECTION('center_axis',(-0.923893192342434,-0.38265045295061,-1.69930937299605E-15));
#32183=DIRECTION('ref_axis',(0.38265045295061,-0.923893192342434,-4.10249573495478E-15));
#32184=DIRECTION('center_axis',(-3.56963971048783E-5,-0.999999999362884,
0.));
#32185=DIRECTION('ref_axis',(-0.999999999362884,3.56963971048783E-5,0.));
#32186=DIRECTION('center_axis',(3.56963971007665E-5,0.999999999362884,0.));
#32187=DIRECTION('ref_axis',(-0.707106780736035,2.52411644538797E-5,-0.707106781186551));
#32188=DIRECTION('center_axis',(-3.56963971004377E-5,-0.999999999362884,
0.));
#32189=DIRECTION('ref_axis',(-0.999999999362884,3.56963971004377E-5,0.));
#32190=DIRECTION('center_axis',(0.,0.,-1.));
#32191=DIRECTION('ref_axis',(-1.,0.,0.));
#32192=DIRECTION('center_axis',(0.,0.,-1.));
#32193=DIRECTION('ref_axis',(-1.,0.,0.));
#32194=DIRECTION('center_axis',(-0.707132021900493,-0.707081539571584,0.));
#32195=DIRECTION('ref_axis',(0.499982151482891,-0.500017847879993,-0.707106781186548));
#32196=DIRECTION('center_axis',(-0.382716411291948,-0.9238658715029,-4.10278864883162E-15));
#32197=DIRECTION('ref_axis',(0.9238658715029,-0.382716411291948,-9.90500799955984E-15));
#32198=DIRECTION('center_axis',(-0.882964350739721,-0.469440044438886,0.));
#32199=DIRECTION('ref_axis',(0.33194423878325,-0.624350079954033,-0.707106781186549));
#32200=DIRECTION('center_axis',(0.88296435073972,0.469440044438887,0.));
#32201=DIRECTION('ref_axis',(0.469440044438887,-0.88296435073972,0.));
#32202=DIRECTION('center_axis',(-0.970304361397861,-0.241887259383973,0.));
#32203=DIRECTION('ref_axis',(-0.241887259383973,0.970304361397861,0.));
#32204=DIRECTION('center_axis',(0.,0.,1.));
#32205=DIRECTION('ref_axis',(1.,0.,0.));
#32206=DIRECTION('center_axis',(3.56963971004376E-5,0.999999999362884,0.));
#32207=DIRECTION('ref_axis',(0.999999999362884,-3.56963971004376E-5,0.));
#32208=DIRECTION('center_axis',(-3.56963971014961E-5,-0.999999999362884,
0.));
#32209=DIRECTION('ref_axis',(0.707106780736038,-2.52411644543957E-5,-0.707106781186548));
#32210=DIRECTION('center_axis',(-1.,0.,0.));
#32211=DIRECTION('ref_axis',(0.,-0.707106781186548,-0.707106781186548));
#32212=DIRECTION('',(-1.,0.,0.));
#32213=DIRECTION('center_axis',(1.,0.,0.));
#32214=DIRECTION('ref_axis',(0.,-1.,0.));
#32215=DIRECTION('center_axis',(-0.970295726275993,0.241921895599681,0.));
#32216=DIRECTION('ref_axis',(0.241921895599681,0.970295726275993,0.));
#32217=DIRECTION('center_axis',(-0.999999999840721,1.7848198553344E-5,0.));
#32218=DIRECTION('ref_axis',(-1.26205822290334E-5,-0.707106781073918,-0.70710678118655));
#32219=DIRECTION('center_axis',(0.999999999840721,-1.78481985502188E-5,
0.));
#32220=DIRECTION('ref_axis',(-1.78481985502188E-5,-0.999999999840721,0.));
#32221=DIRECTION('',(-0.999999999840721,1.7848198553344E-5,0.));
#32222=DIRECTION('center_axis',(-0.999999999362884,3.56963971010297E-5,
0.));
#32223=DIRECTION('ref_axis',(-2.52411644540658E-5,-0.707106780736035,-0.707106781186551));
#32224=DIRECTION('',(-0.999999999362884,3.56963971010297E-5,0.));
#32225=DIRECTION('center_axis',(0.,1.,0.));
#32226=DIRECTION('ref_axis',(-0.707106781186551,0.,-0.707106781186544));
#32227=DIRECTION('',(0.,1.,0.));
#32228=DIRECTION('center_axis',(0.,-1.,0.));
#32229=DIRECTION('ref_axis',(-1.,0.,0.));
#32230=DIRECTION('center_axis',(-0.382683432365083,0.92387953251129,0.));
#32231=DIRECTION('ref_axis',(-0.92387953251129,-0.382683432365083,0.));
#32232=DIRECTION('center_axis',(0.,0.,1.));
#32233=DIRECTION('ref_axis',(1.,0.,0.));
#32234=DIRECTION('center_axis',(0.88294759285893,-0.469471562785885,0.));
#32235=DIRECTION('ref_axis',(-0.469471562785885,-0.88294759285893,0.));
#32236=DIRECTION('center_axis',(0.,0.,1.));
#32237=DIRECTION('ref_axis',(0.857167300702112,0.515038074910055,0.));
#32238=DIRECTION('center_axis',(-0.882947592858928,0.46947156278589,0.));
#32239=DIRECTION('ref_axis',(-0.331966525620151,-0.624338230342891,-0.707106781186542));
#32240=DIRECTION('',(-0.882947592858928,0.46947156278589,0.));
#32241=DIRECTION('center_axis',(-0.707106781186548,0.707106781186547,0.));
#32242=DIRECTION('ref_axis',(-0.5,-0.500000000000001,-0.707106781186547));
#32243=DIRECTION('',(-0.707106781186548,0.707106781186547,0.));
#32244=DIRECTION('center_axis',(-0.92387953251129,0.382683432365083,0.));
#32245=DIRECTION('ref_axis',(-0.382683432365083,-0.92387953251129,0.));
#32246=DIRECTION('center_axis',(0.,0.,-1.));
#32247=DIRECTION('ref_axis',(-1.,0.,0.));
#32248=DIRECTION('center_axis',(0.,1.,0.));
#32249=DIRECTION('ref_axis',(1.,0.,0.));
#32250=DIRECTION('center_axis',(0.,0.,-1.));
#32251=DIRECTION('ref_axis',(0.923879532511287,0.38268343236509,0.));
#32252=DIRECTION('center_axis',(-3.28954970259306E-16,-1.,0.));
#32253=DIRECTION('ref_axis',(0.707106781186548,-2.32606290175374E-16,-0.707106781186548));
#32254=DIRECTION('center_axis',(0.,1.,0.));
#32255=DIRECTION('ref_axis',(1.,0.,0.));
#32256=DIRECTION('',(-3.28954970259306E-16,-1.,0.));
#32257=DIRECTION('center_axis',(1.,0.,0.));
#32258=DIRECTION('ref_axis',(0.,-1.,0.));
#32259=DIRECTION('center_axis',(0.,0.,-1.));
#32260=DIRECTION('ref_axis',(0.707106781186546,-0.707106781186549,0.));
#32261=DIRECTION('center_axis',(-1.,0.,0.));
#32262=DIRECTION('ref_axis',(0.,-0.707106781186548,-0.707106781186548));
#32263=DIRECTION('',(-1.,0.,0.));
#32264=DIRECTION('center_axis',(-3.56963971010297E-5,-0.999999999362884,
0.));
#32265=DIRECTION('ref_axis',(-0.999999999362884,3.56963971010297E-5,0.));
#32266=DIRECTION('',(0.,0.,-1.));
#32267=DIRECTION('center_axis',(-1.7848198553344E-5,-0.999999999840721,
0.));
#32268=DIRECTION('ref_axis',(-0.999999999840721,1.7848198553344E-5,0.));
#32269=DIRECTION('',(0.,0.,-1.));
#32270=DIRECTION('center_axis',(0.,-1.,0.));
#32271=DIRECTION('ref_axis',(-1.,0.,0.));
#32272=DIRECTION('',(0.,0.,-1.));
#32273=DIRECTION('center_axis',(-0.46947156278589,-0.882947592858928,0.));
#32274=DIRECTION('ref_axis',(-0.882947592858928,0.46947156278589,0.));
#32275=DIRECTION('',(0.,0.,-1.));
#32276=DIRECTION('center_axis',(0.,0.,-1.));
#32277=DIRECTION('ref_axis',(0.469471562785885,0.88294759285893,0.));
#32278=DIRECTION('',(0.,0.,-1.));
#32279=DIRECTION('center_axis',(-1.,0.,0.));
#32280=DIRECTION('ref_axis',(0.,1.,0.));
#32281=DIRECTION('',(0.,0.,-1.));
#32282=DIRECTION('center_axis',(-0.707106781186547,-0.707106781186548,0.));
#32283=DIRECTION('ref_axis',(-0.707106781186548,0.707106781186547,0.));
#32284=DIRECTION('',(0.,0.,-1.));
#32285=DIRECTION('center_axis',(0.,-1.,0.));
#32286=DIRECTION('ref_axis',(-1.,0.,0.));
#32287=DIRECTION('',(0.,0.,-1.));
#32288=DIRECTION('center_axis',(0.,0.,-1.));
#32289=DIRECTION('ref_axis',(1.,0.,0.));
#32290=DIRECTION('',(0.,0.,-1.));
#32291=DIRECTION('center_axis',(1.,-3.28954970259306E-16,0.));
#32292=DIRECTION('ref_axis',(-3.28954970259306E-16,-1.,0.));
#32293=DIRECTION('',(0.,0.,-1.));
#32294=DIRECTION('center_axis',(0.,0.,-1.));
#32295=DIRECTION('ref_axis',(0.707106781186547,0.707106781186548,0.));
#32296=DIRECTION('',(0.,0.,-1.));
#32297=DIRECTION('center_axis',(0.707106781186547,0.707106781186548,0.));
#32298=DIRECTION('ref_axis',(0.707106781186548,-0.707106781186547,0.));
#32299=DIRECTION('',(0.,0.,-1.));
#32300=DIRECTION('center_axis',(0.,0.,-1.));
#32301=DIRECTION('ref_axis',(1.48029736616687E-15,1.,0.));
#32302=DIRECTION('',(0.,0.,1.));
#32303=DIRECTION('center_axis',(0.,0.,1.));
#32304=DIRECTION('ref_axis',(1.48029736616687E-15,1.,0.));
#32305=DIRECTION('',(0.,0.,-1.));
#32306=DIRECTION('center_axis',(0.,0.,1.));
#32307=DIRECTION('ref_axis',(-1.,0.,0.));
#32308=DIRECTION('',(0.,0.,-1.));
#32309=DIRECTION('center_axis',(0.,0.,1.));
#32310=DIRECTION('ref_axis',(-1.,0.,0.));
#32311=DIRECTION('center_axis',(0.,0.,1.));
#32312=DIRECTION('ref_axis',(0.836944376135179,-0.547287960086548,0.));
#32313=DIRECTION('center_axis',(0.,0.,1.));
#32314=DIRECTION('ref_axis',(-1.,0.,0.));
#32315=DIRECTION('center_axis',(0.,0.,-1.));
#32316=DIRECTION('ref_axis',(-1.,0.,0.));
#32317=DIRECTION('center_axis',(0.,0.,-1.));
#32318=DIRECTION('ref_axis',(-1.,0.,0.));
#32319=DIRECTION('',(-1.,0.,0.));
#32320=DIRECTION('',(0.,1.,0.));
#32321=DIRECTION('center_axis',(0.,0.,-1.));
#32322=DIRECTION('ref_axis',(0.,-1.,0.));
#32323=DIRECTION('center_axis',(0.,1.,0.));
#32324=DIRECTION('ref_axis',(1.,0.,0.));
#32325=DIRECTION('',(0.,0.,-1.));
#32326=DIRECTION('center_axis',(0.,0.,-1.));
#32327=DIRECTION('ref_axis',(0.,-1.,0.));
#32328=DIRECTION('',(0.,0.,-1.));
#32329=DIRECTION('center_axis',(1.,0.,0.));
#32330=DIRECTION('ref_axis',(0.,-1.,0.));
#32331=DIRECTION('',(0.,0.,-1.));
#32332=DIRECTION('center_axis',(0.,0.,-1.));
#32333=DIRECTION('ref_axis',(-4.44089209850064E-15,1.,0.));
#32334=DIRECTION('axis',(0.,0.,1.));
#32335=DIRECTION('refdir',(1.,0.,0.));
#32336=DIRECTION('center_axis',(-1.,-6.57957785206009E-13,0.));
#32337=DIRECTION('ref_axis',(0.,0.,-1.));
#32338=DIRECTION('center_axis',(1.,-3.28954970259306E-16,0.));
#32339=DIRECTION('ref_axis',(0.,0.,-1.));
#32340=DIRECTION('',(-1.,-6.57957785206009E-13,0.));
#32341=DIRECTION('center_axis',(-1.,-6.58286732145141E-13,0.));
#32342=DIRECTION('ref_axis',(0.,0.,-1.));
#32343=DIRECTION('center_axis',(1.,6.58286732145141E-13,0.));
#32344=DIRECTION('ref_axis',(0.,0.,-1.));
#32345=DIRECTION('center_axis',(-0.999999999362884,3.56963971004376E-5,
0.));
#32346=DIRECTION('ref_axis',(0.,0.,-1.));
#32347=DIRECTION('center_axis',(-0.999999999362884,3.56963971007665E-5,
0.));
#32348=DIRECTION('ref_axis',(0.,0.,-1.));
#32349=DIRECTION('',(-0.999999999362884,3.56963971004376E-5,0.));
#32350=DIRECTION('center_axis',(-0.999999999362884,3.56963971007665E-5,
0.));
#32351=DIRECTION('ref_axis',(0.,0.,-1.));
#32352=DIRECTION('center_axis',(0.999999999362884,-3.56963971007665E-5,
0.));
#32353=DIRECTION('ref_axis',(0.,0.,-1.));
#32354=DIRECTION('center_axis',(0.999999999362884,-3.56963971010297E-5,
0.));
#32355=DIRECTION('ref_axis',(-2.52411644540658E-5,-0.707106780736035,-0.707106781186551));
#32356=DIRECTION('',(0.999999999362884,-3.56963971010297E-5,0.));
#32357=DIRECTION('center_axis',(-0.970304361397857,-0.24188725938399,0.));
#32358=DIRECTION('ref_axis',(0.24188725938399,-0.970304361397857,0.));
#32359=DIRECTION('',(-0.999999999362884,3.56963971010297E-5,0.));
#32360=DIRECTION('center_axis',(0.999999999362884,-3.56963970959969E-5,
0.));
#32361=DIRECTION('ref_axis',(-3.56963970959969E-5,-0.999999999362884,0.));
#32362=DIRECTION('center_axis',(-0.999999999840721,1.7848198553344E-5,0.));
#32363=DIRECTION('ref_axis',(-1.26205822290334E-5,-0.707106781073918,-0.70710678118655));
#32364=DIRECTION('',(-0.999999999840721,1.7848198553344E-5,0.));
#32365=DIRECTION('center_axis',(0.999999999840721,-1.78481985546597E-5,
0.));
#32366=DIRECTION('ref_axis',(-1.78481985546597E-5,-0.999999999840721,0.));
#32367=DIRECTION('',(0.999999999840721,-1.7848198553344E-5,0.));
#32368=DIRECTION('center_axis',(0.,1.,0.));
#32369=DIRECTION('ref_axis',(0.707106781186548,0.,-0.707106781186548));
#32370=DIRECTION('center_axis',(0.,1.,0.));
#32371=DIRECTION('ref_axis',(1.,0.,0.));
#32372=DIRECTION('',(0.,1.,0.));
#32373=DIRECTION('center_axis',(0.,-1.,0.));
#32374=DIRECTION('ref_axis',(0.,0.,-1.));
#32375=DIRECTION('',(0.,-1.,0.));
#32376=DIRECTION('center_axis',(0.,0.,1.));
#32377=DIRECTION('ref_axis',(-1.,0.,0.));
#32378=DIRECTION('center_axis',(1.,0.,0.));
#32379=DIRECTION('ref_axis',(0.,0.,-1.));
#32380=DIRECTION('center_axis',(0.,0.,1.));
#32381=DIRECTION('ref_axis',(-0.707106781186545,-0.70710678118655,0.));
#32382=DIRECTION('center_axis',(0.,0.,-1.));
#32383=DIRECTION('ref_axis',(-0.707106781186545,-0.70710678118655,0.));
#32384=DIRECTION('center_axis',(-1.,0.,0.));
#32385=DIRECTION('ref_axis',(0.,0.707106781186548,-0.707106781186548));
#32386=DIRECTION('center_axis',(1.,0.,0.));
#32387=DIRECTION('ref_axis',(0.,0.,-1.));
#32388=DIRECTION('',(1.,0.,0.));
#32389=DIRECTION('',(-1.,0.,0.));
#32390=DIRECTION('center_axis',(0.,0.,1.));
#32391=DIRECTION('ref_axis',(-1.,0.,0.));
#32392=DIRECTION('center_axis',(0.707106781186545,-0.70710678118655,0.));
#32393=DIRECTION('ref_axis',(0.,0.,-1.));
#32394=DIRECTION('center_axis',(0.,0.,-1.));
#32395=DIRECTION('ref_axis',(0.382683432365091,0.923879532511286,0.));
#32396=DIRECTION('center_axis',(0.,0.,1.));
#32397=DIRECTION('ref_axis',(0.382683432365091,0.923879532511286,0.));
#32398=DIRECTION('center_axis',(-0.707106781186548,0.707106781186547,0.));
#32399=DIRECTION('ref_axis',(0.5,0.500000000000001,-0.707106781186547));
#32400=DIRECTION('center_axis',(0.707106781186548,-0.707106781186548,0.));
#32401=DIRECTION('ref_axis',(0.,0.,-1.));
#32402=DIRECTION('',(0.707106781186548,-0.707106781186547,0.));
#32403=DIRECTION('',(-0.707106781186548,0.707106781186547,0.));
#32404=DIRECTION('center_axis',(0.,0.,1.));
#32405=DIRECTION('ref_axis',(-1.,0.,0.));
#32406=DIRECTION('center_axis',(0.,-1.,0.));
#32407=DIRECTION('ref_axis',(0.,0.,-1.));
#32408=DIRECTION('center_axis',(0.,0.,-1.));
#32409=DIRECTION('ref_axis',(0.923879532511287,0.38268343236509,0.));
#32410=DIRECTION('center_axis',(0.,0.,1.));
#32411=DIRECTION('ref_axis',(0.923879532511287,0.38268343236509,0.));
#32412=DIRECTION('center_axis',(3.28954970259306E-16,1.,0.));
#32413=DIRECTION('ref_axis',(0.707106781186548,-2.32606290175374E-16,-0.707106781186548));
#32414=DIRECTION('center_axis',(0.,-1.,0.));
#32415=DIRECTION('ref_axis',(0.,0.,-1.));
#32416=DIRECTION('',(-3.28954970259306E-16,-1.,0.));
#32417=DIRECTION('',(3.28954970259306E-16,1.,0.));
#32418=DIRECTION('center_axis',(-1.,0.,0.));
#32419=DIRECTION('ref_axis',(0.,0.,-1.));
#32420=DIRECTION('center_axis',(0.,0.,-1.));
#32421=DIRECTION('ref_axis',(0.707106781186547,-0.707106781186548,0.));
#32422=DIRECTION('center_axis',(0.,0.,1.));
#32423=DIRECTION('ref_axis',(0.707106781186546,-0.707106781186549,0.));
#32424=DIRECTION('center_axis',(1.,0.,0.));
#32425=DIRECTION('ref_axis',(0.,-0.707106781186548,-0.707106781186548));
#32426=DIRECTION('',(1.,0.,0.));
#32427=DIRECTION('center_axis',(-0.92387953251129,0.382683432365083,0.));
#32428=DIRECTION('ref_axis',(0.382683432365083,0.92387953251129,0.));
#32429=DIRECTION('',(-1.,0.,0.));
#32430=DIRECTION('center_axis',(0.707106781186548,-0.707106781186547,0.));
#32431=DIRECTION('ref_axis',(-0.499999999999999,-0.499999999999999,-0.707106781186549));
#32432=DIRECTION('',(0.707106781186548,-0.707106781186547,0.));
#32433=DIRECTION('center_axis',(-0.382683432365083,0.92387953251129,0.));
#32434=DIRECTION('ref_axis',(0.92387953251129,0.382683432365083,0.));
#32435=DIRECTION('',(-0.707106781186548,0.707106781186547,0.));
#32436=DIRECTION('center_axis',(0.,-1.,0.));
#32437=DIRECTION('ref_axis',(-0.707106781186551,0.,-0.707106781186544));
#32438=DIRECTION('',(0.,1.,0.));
#32439=DIRECTION('',(0.,-1.,0.));
#32440=DIRECTION('center_axis',(0.,1.,0.));
#32441=DIRECTION('ref_axis',(0.,0.,-1.));
#32442=DIRECTION('center_axis',(0.,0.,1.));
#32443=DIRECTION('ref_axis',(-1.,0.,0.));
#32444=DIRECTION('center_axis',(-0.88294759285893,0.469471562785885,0.));
#32445=DIRECTION('ref_axis',(0.,0.,-1.));
#32446=DIRECTION('center_axis',(0.,0.,1.));
#32447=DIRECTION('ref_axis',(0.857167300702112,0.515038074910055,0.));
#32448=DIRECTION('center_axis',(0.,0.,-1.));
#32449=DIRECTION('ref_axis',(0.857167300702112,0.515038074910055,0.));
#32450=DIRECTION('center_axis',(0.882947592858928,-0.46947156278589,0.));
#32451=DIRECTION('ref_axis',(-0.331966525620151,-0.624338230342891,-0.707106781186542));
#32452=DIRECTION('',(0.882947592858928,-0.46947156278589,0.));
#32453=DIRECTION('center_axis',(-0.970295726275989,0.241921895599697,0.));
#32454=DIRECTION('ref_axis',(-0.241921895599697,-0.970295726275989,0.));
#32455=DIRECTION('',(-0.882947592858928,0.46947156278589,0.));
#32456=DIRECTION('center_axis',(1.,0.,0.));
#32457=DIRECTION('ref_axis',(0.,-0.707106781186548,-0.707106781186548));
#32458=DIRECTION('',(-1.,0.,0.));
#32459=DIRECTION('',(1.,0.,0.));
#32460=DIRECTION('center_axis',(0.882964350739721,0.469440044438886,0.));
#32461=DIRECTION('ref_axis',(0.331944238783253,-0.624350079954038,-0.707106781186543));
#32462=DIRECTION('',(-0.882964350739721,-0.469440044438886,0.));
#32463=DIRECTION('',(0.882964350739721,0.469440044438886,0.));
#32464=DIRECTION('center_axis',(-0.882964350739719,-0.46944004443889,0.));
#32465=DIRECTION('ref_axis',(0.,0.,-1.));
#32466=DIRECTION('center_axis',(0.,0.,1.));
#32467=DIRECTION('ref_axis',(-1.,0.,0.));
#32468=DIRECTION('center_axis',(-3.56963971004376E-5,-0.999999999362884,
0.));
#32469=DIRECTION('ref_axis',(0.,0.,-1.));
#32470=DIRECTION('center_axis',(0.,0.,1.));
#32471=DIRECTION('ref_axis',(-0.857148915152355,0.51506867236626,0.));
#32472=DIRECTION('center_axis',(0.,0.,-1.));
#32473=DIRECTION('ref_axis',(-0.857148915152355,0.51506867236626,0.));
#32474=DIRECTION('center_axis',(3.56963971014961E-5,0.999999999362884,0.));
#32475=DIRECTION('ref_axis',(0.707106780736038,-2.52411644543957E-5,-0.707106781186548));
#32476=DIRECTION('',(3.56963971014961E-5,0.999999999362884,0.));
#32477=DIRECTION('center_axis',(-0.382716411291948,-0.9238658715029,0.));
#32478=DIRECTION('ref_axis',(-0.9238658715029,0.382716411291948,0.));
#32479=DIRECTION('',(-3.56963971014961E-5,-0.999999999362884,0.));
#32480=DIRECTION('center_axis',(0.707132021900493,0.707081539571584,0.));
#32481=DIRECTION('ref_axis',(0.499982151482891,-0.500017847879993,-0.707106781186548));
#32482=DIRECTION('',(-0.707132021900493,-0.707081539571584,0.));
#32483=DIRECTION('',(0.707132021900493,0.707081539571584,0.));
#32484=DIRECTION('center_axis',(-0.923893192342431,-0.382650452950617,-6.50651058246798E-15));
#32485=DIRECTION('ref_axis',(-0.382650452950617,0.923893192342431,-1.57081060919186E-14));
#32486=DIRECTION('center_axis',(0.999999999362884,-3.5696397100931E-5,0.));
#32487=DIRECTION('ref_axis',(-2.52411644539961E-5,-0.707106780736038,-0.707106781186548));
#32488=DIRECTION('',(-0.999999999362884,3.5696397100931E-5,0.));
#32489=DIRECTION('',(0.999999999362884,-3.5696397100931E-5,0.));
#32490=DIRECTION('center_axis',(-0.999999999362884,3.56963971004377E-5,
0.));
#32491=DIRECTION('ref_axis',(0.,0.,-1.));
#32492=DIRECTION('center_axis',(3.56963971048783E-5,0.999999999362884,0.));
#32493=DIRECTION('ref_axis',(0.,0.,-1.));
#32494=DIRECTION('center_axis',(0.,0.,-1.));
#32495=DIRECTION('ref_axis',(-0.707132021900492,-0.707081539571584,0.));
#32496=DIRECTION('center_axis',(0.,0.,1.));
#32497=DIRECTION('ref_axis',(-0.707132021900492,-0.707081539571584,0.));
#32498=DIRECTION('center_axis',(-3.56963971007665E-5,-0.999999999362884,
0.));
#32499=DIRECTION('ref_axis',(-0.707106780736035,2.52411644538797E-5,-0.707106781186551));
#32500=DIRECTION('center_axis',(3.56963971004377E-5,0.999999999362884,0.));
#32501=DIRECTION('ref_axis',(0.,0.,-1.));
#32502=DIRECTION('',(3.56963971007665E-5,0.999999999362884,0.));
#32503=DIRECTION('',(-3.56963971007665E-5,-0.999999999362884,0.));
#32504=DIRECTION('center_axis',(0.,0.,1.));
#32505=DIRECTION('ref_axis',(-1.,0.,0.));
#32506=DIRECTION('center_axis',(0.707132021900495,0.707081539571582,0.));
#32507=DIRECTION('ref_axis',(0.,0.,-1.));
#32508=DIRECTION('center_axis',(0.,0.,-1.));
#32509=DIRECTION('ref_axis',(-0.923865871502902,0.382716411291943,0.));
#32510=DIRECTION('center_axis',(0.,0.,1.));
#32511=DIRECTION('ref_axis',(-0.923865871502902,0.382716411291943,0.));
#32512=DIRECTION('center_axis',(-0.707132021900493,-0.707081539571584,0.));
#32513=DIRECTION('ref_axis',(-0.499982151482891,0.500017847879993,-0.707106781186548));
#32514=DIRECTION('center_axis',(0.70713202190049,0.707081539571586,0.));
#32515=DIRECTION('ref_axis',(0.,0.,-1.));
#32516=DIRECTION('',(0.707132021900493,0.707081539571584,0.));
#32517=DIRECTION('',(-0.707132021900493,-0.707081539571584,0.));
#32518=DIRECTION('center_axis',(0.,0.,1.));
#32519=DIRECTION('ref_axis',(-1.,0.,0.));
#32520=DIRECTION('center_axis',(0.999999999362884,-3.56963971004377E-5,
0.));
#32521=DIRECTION('ref_axis',(0.,0.,-1.));
#32522=DIRECTION('center_axis',(0.,0.,-1.));
#32523=DIRECTION('ref_axis',(-0.382650452950611,0.923893192342433,0.));
#32524=DIRECTION('center_axis',(0.,0.,1.));
#32525=DIRECTION('ref_axis',(-0.382650452950611,0.923893192342433,0.));
#32526=DIRECTION('center_axis',(-0.999999999362884,3.56963971021026E-5,
0.));
#32527=DIRECTION('ref_axis',(2.52411644548245E-5,0.707106780736035,-0.707106781186551));
#32528=DIRECTION('center_axis',(0.999999999362884,-3.5696397104879E-5,0.));
#32529=DIRECTION('ref_axis',(0.,0.,-1.));
#32530=DIRECTION('',(0.999999999362884,-3.56963971021026E-5,0.));
#32531=DIRECTION('',(-0.999999999362884,3.56963971021026E-5,0.));
#32532=DIRECTION('center_axis',(0.,0.,1.));
#32533=DIRECTION('ref_axis',(-1.,0.,0.));
#32534=DIRECTION('center_axis',(3.56963971004376E-5,0.999999999362884,0.));
#32535=DIRECTION('ref_axis',(0.,0.,-1.));
#32536=DIRECTION('center_axis',(0.,0.,1.));
#32537=DIRECTION('ref_axis',(0.707081539571586,-0.70713202190049,0.));
#32538=DIRECTION('center_axis',(0.,0.,-1.));
#32539=DIRECTION('ref_axis',(0.707081539571587,-0.70713202190049,0.));
#32540=DIRECTION('center_axis',(-3.56963971011028E-5,-0.999999999362884,
0.));
#32541=DIRECTION('ref_axis',(-0.707106780736038,2.52411644541176E-5,-0.707106781186548));
#32542=DIRECTION('center_axis',(3.56963970915558E-5,0.999999999362884,0.));
#32543=DIRECTION('ref_axis',(0.,0.,-1.));
#32544=DIRECTION('',(3.56963971011028E-5,0.999999999362884,0.));
#32545=DIRECTION('',(-3.56963971011028E-5,-0.999999999362884,0.));
#32546=DIRECTION('center_axis',(-1.,0.,0.));
#32547=DIRECTION('ref_axis',(0.,0.707106781186554,-0.707106781186541));
#32548=DIRECTION('center_axis',(-1.,0.,0.));
#32549=DIRECTION('ref_axis',(0.,1.,0.));
#32550=DIRECTION('',(-1.,0.,0.));
#32551=DIRECTION('center_axis',(1.,0.,0.));
#32552=DIRECTION('ref_axis',(0.,0.,-1.));
#32553=DIRECTION('',(1.,0.,0.));
#32554=DIRECTION('center_axis',(0.999999999840721,-1.78481985534681E-5,
0.));
#32555=DIRECTION('ref_axis',(1.26205822291212E-5,0.707106781073918,-0.70710678118655));
#32556=DIRECTION('',(0.999999999840721,-1.78481985534681E-5,0.));
#32557=DIRECTION('center_axis',(-0.999999999840721,1.78481985546596E-5,
0.));
#32558=DIRECTION('ref_axis',(1.78481985546596E-5,0.999999999840721,0.));
#32559=DIRECTION('',(-0.999999999840721,1.78481985534681E-5,0.));
#32560=DIRECTION('center_axis',(-0.999999999362884,3.56963971040562E-5,
0.));
#32561=DIRECTION('ref_axis',(2.52411644562058E-5,0.707106780736035,-0.707106781186551));
#32562=DIRECTION('',(0.999999999362884,-3.56963971040562E-5,0.));
#32563=DIRECTION('center_axis',(-0.999999999362884,3.5696397104879E-5,0.));
#32564=DIRECTION('ref_axis',(3.5696397104879E-5,0.999999999362884,0.));
#32565=DIRECTION('',(-0.999999999362884,3.56963971040562E-5,0.));
#32566=DIRECTION('center_axis',(-0.816511153790762,-0.408241003122002,0.408226431169298));
#32567=DIRECTION('ref_axis',(-0.577329659497308,0.577370878146268,-0.577350269189622));
#32568=DIRECTION('center_axis',(0.,0.,1.));
#32569=DIRECTION('ref_axis',(-0.999999999362884,3.56963970915558E-5,0.));
#32570=DIRECTION('center_axis',(0.408248290463868,-0.816496580927721,-0.408248290463868));
#32571=DIRECTION('ref_axis',(0.577350269189616,0.577350269189634,-0.577350269189627));
#32572=DIRECTION('center_axis',(0.,0.,1.));
#32573=DIRECTION('ref_axis',(-4.44089209850064E-15,1.,0.));
#32574=DIRECTION('center_axis',(-0.469440044438886,0.882964350739721,0.));
#32575=DIRECTION('ref_axis',(-0.882964350739721,-0.469440044438886,0.));
#32576=DIRECTION('',(0.,0.,1.));
#32577=DIRECTION('',(-0.882964350739721,-0.469440044438886,0.));
#32578=DIRECTION('',(0.,0.,1.));
#32579=DIRECTION('center_axis',(0.,0.,-1.));
#32580=DIRECTION('ref_axis',(-0.999999999362884,3.56963971004376E-5,0.));
#32581=DIRECTION('center_axis',(0.,0.,1.));
#32582=DIRECTION('ref_axis',(-0.857148915152355,0.51506867236626,0.));
#32583=DIRECTION('',(0.,0.,1.));
#32584=DIRECTION('center_axis',(-0.999999999362884,3.56963971014961E-5,
0.));
#32585=DIRECTION('ref_axis',(-3.56963971014961E-5,-0.999999999362884,0.));
#32586=DIRECTION('',(-3.56963971014961E-5,-0.999999999362884,0.));
#32587=DIRECTION('',(0.,0.,1.));
#32588=DIRECTION('center_axis',(-0.707081539571584,0.707132021900493,0.));
#32589=DIRECTION('ref_axis',(-0.707132021900493,-0.707081539571584,0.));
#32590=DIRECTION('',(-0.707132021900493,-0.707081539571584,0.));
#32591=DIRECTION('',(0.,0.,1.));
#32592=DIRECTION('center_axis',(3.5696397100931E-5,0.999999999362884,0.));
#32593=DIRECTION('ref_axis',(-0.999999999362884,3.5696397100931E-5,0.));
#32594=DIRECTION('',(-0.999999999362884,3.5696397100931E-5,0.));
#32595=DIRECTION('',(0.,0.,1.));
#32596=DIRECTION('center_axis',(0.,0.,-1.));
#32597=DIRECTION('ref_axis',(-3.56963971004376E-5,-0.999999999362884,0.));
#32598=DIRECTION('center_axis',(0.,0.,-1.));
#32599=DIRECTION('ref_axis',(-0.707132021900492,-0.707081539571584,0.));
#32600=DIRECTION('',(0.,0.,1.));
#32601=DIRECTION('center_axis',(0.999999999362884,-3.56963971007665E-5,
0.));
#32602=DIRECTION('ref_axis',(3.56963971007665E-5,0.999999999362884,0.));
#32603=DIRECTION('',(3.56963971007665E-5,0.999999999362884,0.));
#32604=DIRECTION('',(0.,0.,1.));
#32605=DIRECTION('center_axis',(0.,0.,-1.));
#32606=DIRECTION('ref_axis',(-0.999999999362884,3.56963971013258E-5,0.));
#32607=DIRECTION('center_axis',(0.,0.,-1.));
#32608=DIRECTION('ref_axis',(-0.923865871502902,0.382716411291943,0.));
#32609=DIRECTION('',(0.,0.,1.));
#32610=DIRECTION('center_axis',(0.707081539571584,-0.707132021900493,0.));
#32611=DIRECTION('ref_axis',(0.707132021900493,0.707081539571584,0.));
#32612=DIRECTION('',(0.707132021900493,0.707081539571584,0.));
#32613=DIRECTION('',(0.,0.,1.));
#32614=DIRECTION('center_axis',(0.,0.,-1.));
#32615=DIRECTION('ref_axis',(-0.707081539571585,0.707132021900492,0.));
#32616=DIRECTION('center_axis',(0.,0.,-1.));
#32617=DIRECTION('ref_axis',(-0.674257203707391,0.738496596639883,0.));
#32618=DIRECTION('',(0.,0.,1.));
#32619=DIRECTION('center_axis',(0.,0.,1.));
#32620=DIRECTION('ref_axis',(-0.707081539571585,0.707132021900492,0.));
#32621=DIRECTION('',(0.,0.,1.));
#32622=DIRECTION('center_axis',(-3.56963971021026E-5,-0.999999999362884,
0.));
#32623=DIRECTION('ref_axis',(0.999999999362884,-3.56963971021026E-5,0.));
#32624=DIRECTION('',(-0.999999999362884,3.56963971021026E-5,0.));
#32625=DIRECTION('',(0.,0.,1.));
#32626=DIRECTION('center_axis',(0.,0.,-1.));
#32627=DIRECTION('ref_axis',(0.999999999362884,-3.56963970980596E-5,0.));
#32628=DIRECTION('center_axis',(0.,0.,-1.));
#32629=DIRECTION('ref_axis',(0.999999999362884,-3.56963970980596E-5,0.));
#32630=DIRECTION('',(0.,0.,1.));
#32631=DIRECTION('center_axis',(0.999999999362884,-3.56963971011028E-5,
0.));
#32632=DIRECTION('ref_axis',(3.56963971011028E-5,0.999999999362884,0.));
#32633=DIRECTION('',(-3.56963971011028E-5,-0.999999999362884,0.));
#32634=DIRECTION('',(0.,0.,-1.));
#32635=DIRECTION('',(3.56963971011028E-5,0.999999999362884,0.));
#32636=DIRECTION('',(0.,0.,1.));
#32637=DIRECTION('center_axis',(0.,0.,-1.));
#32638=DIRECTION('ref_axis',(-0.999999999362884,3.56963970915558E-5,0.));
#32639=DIRECTION('center_axis',(0.,0.,-1.));
#32640=DIRECTION('ref_axis',(-0.999999999362884,3.56963970915558E-5,0.));
#32641=DIRECTION('',(0.,0.,1.));
#32642=DIRECTION('center_axis',(-3.56963971040562E-5,-0.999999999362884,
0.));
#32643=DIRECTION('ref_axis',(0.999999999362884,-3.56963971040562E-5,0.));
#32644=DIRECTION('',(0.999999999362884,-3.56963971040562E-5,0.));
#32645=DIRECTION('',(0.,0.,1.));
#32646=DIRECTION('center_axis',(-1.78481985534681E-5,-0.999999999840721,
0.));
#32647=DIRECTION('ref_axis',(0.999999999840721,-1.78481985534681E-5,0.));
#32648=DIRECTION('',(0.999999999840721,-1.78481985534681E-5,0.));
#32649=DIRECTION('',(0.,0.,1.));
#32650=DIRECTION('center_axis',(0.,-1.,0.));
#32651=DIRECTION('ref_axis',(1.,0.,0.));
#32652=DIRECTION('',(1.,0.,0.));
#32653=DIRECTION('',(0.,0.,1.));
#32654=DIRECTION('center_axis',(0.,0.,-1.));
#32655=DIRECTION('ref_axis',(-1.,0.,0.));
#32656=DIRECTION('center_axis',(-3.56963971011028E-5,-0.999999999362884,
0.));
#32657=DIRECTION('ref_axis',(-0.707106780736038,2.52411644541176E-5,0.707106781186548));
#32658=DIRECTION('',(-3.56963971011028E-5,-0.999999999362884,0.));
#32659=DIRECTION('center_axis',(3.56963970915558E-5,0.999999999362884,0.));
#32660=DIRECTION('ref_axis',(-0.999999999362884,3.56963970915558E-5,0.));
#32661=DIRECTION('center_axis',(0.,0.,-1.));
#32662=DIRECTION('ref_axis',(1.,0.,0.));
#32663=DIRECTION('center_axis',(0.,0.,-1.));
#32664=DIRECTION('ref_axis',(0.880581945986775,-0.473893908382608,0.));
#32665=DIRECTION('center_axis',(0.,0.,1.));
#32666=DIRECTION('ref_axis',(0.880581945986775,-0.473893908382608,0.));
#32667=DIRECTION('center_axis',(-0.999999999362884,3.56963971040562E-5,
0.));
#32668=DIRECTION('ref_axis',(2.52411644562058E-5,0.707106780736035,0.707106781186551));
#32669=DIRECTION('center_axis',(0.999999999362884,-3.56963971004374E-5,
0.));
#32670=DIRECTION('ref_axis',(3.56963971004374E-5,0.999999999362884,0.));
#32671=DIRECTION('center_axis',(-0.999999999362884,3.56963971048783E-5,
0.));
#32672=DIRECTION('ref_axis',(0.,0.,1.));
#32673=DIRECTION('',(-0.999999999362884,3.56963971040562E-5,0.));
#32674=DIRECTION('center_axis',(-0.999999999840721,1.78481985534681E-5,
0.));
#32675=DIRECTION('ref_axis',(1.26205822291212E-5,0.707106781073918,0.70710678118655));
#32676=DIRECTION('center_axis',(0.999999999840721,-1.78481985457778E-5,
0.));
#32677=DIRECTION('ref_axis',(1.78481985457778E-5,0.999999999840721,0.));
#32678=DIRECTION('',(-0.999999999840721,1.78481985534681E-5,0.));
#32679=DIRECTION('center_axis',(-1.,0.,0.));
#32680=DIRECTION('ref_axis',(0.,0.707106781186554,0.707106781186541));
#32681=DIRECTION('',(-1.,0.,0.));
#32682=DIRECTION('center_axis',(1.,0.,0.));
#32683=DIRECTION('ref_axis',(0.,1.,0.));
#32684=DIRECTION('center_axis',(-0.816511153790763,-0.408241003122,-0.408226431169296));
#32685=DIRECTION('ref_axis',(-0.57732965949731,0.577370878146255,0.577350269189634));
#32686=DIRECTION('center_axis',(0.,0.,-1.));
#32687=DIRECTION('ref_axis',(-0.836963911810301,-0.54725808383906,0.));
#32688=DIRECTION('center_axis',(0.,0.,1.));
#32689=DIRECTION('ref_axis',(-0.880598861730879,-0.473862474477859,0.));
#32690=DIRECTION('center_axis',(0.,0.,-1.));
#32691=DIRECTION('ref_axis',(-0.88059886173088,-0.473862474477859,0.));
#32692=DIRECTION('center_axis',(0.,1.,0.));
#32693=DIRECTION('ref_axis',(0.707106781186548,0.,0.707106781186548));
#32694=DIRECTION('',(0.,1.,0.));
#32695=DIRECTION('',(0.,-1.,0.));
#32696=DIRECTION('center_axis',(0.,1.,0.));
#32697=DIRECTION('ref_axis',(0.,0.,1.));
#32698=DIRECTION('center_axis',(0.408248290463864,-0.816496580927721,0.408248290463871));
#32699=DIRECTION('ref_axis',(0.577350269189621,0.577350269189625,0.577350269189632));
#32700=DIRECTION('center_axis',(0.,0.,-1.));
#32701=DIRECTION('ref_axis',(-4.44089209850064E-15,1.,0.));
#32702=DIRECTION('center_axis',(-0.707132021900493,-0.707081539571584,0.));
#32703=DIRECTION('ref_axis',(-0.499982151482891,0.500017847879993,0.707106781186548));
#32704=DIRECTION('center_axis',(0.70713202190049,0.707081539571586,0.));
#32705=DIRECTION('ref_axis',(-0.707081539571586,0.70713202190049,0.));
#32706=DIRECTION('center_axis',(0.707132021900495,0.707081539571582,0.));
#32707=DIRECTION('ref_axis',(-0.707081539571582,0.707132021900495,0.));
#32708=DIRECTION('',(-0.707132021900493,-0.707081539571584,0.));
#32709=DIRECTION('center_axis',(0.,0.,-1.));
#32710=DIRECTION('ref_axis',(-1.,0.,0.));
#32711=DIRECTION('center_axis',(0.,0.,1.));
#32712=DIRECTION('ref_axis',(-0.923865871502902,0.382716411291943,0.));
#32713=DIRECTION('',(-3.56963971007665E-5,-0.999999999362884,0.));
#32714=DIRECTION('center_axis',(0.,0.,1.));
#32715=DIRECTION('ref_axis',(-0.707132021900492,-0.707081539571584,0.));
#32716=DIRECTION('',(0.999999999362884,-3.5696397100931E-5,0.));
#32717=DIRECTION('',(0.707132021900493,0.707081539571584,0.));
#32718=DIRECTION('',(3.56963971014961E-5,0.999999999362884,0.));
#32719=DIRECTION('center_axis',(0.,0.,-1.));
#32720=DIRECTION('ref_axis',(-0.857148915152355,0.51506867236626,0.));
#32721=DIRECTION('',(0.882964350739721,0.469440044438886,0.));
#32722=DIRECTION('',(0.999999999362884,-3.56963971010297E-5,0.));
#32723=DIRECTION('',(0.999999999840721,-1.7848198553344E-5,0.));
#32724=DIRECTION('',(1.,0.,0.));
#32725=DIRECTION('',(0.882947592858928,-0.46947156278589,0.));
#32726=DIRECTION('center_axis',(0.,0.,-1.));
#32727=DIRECTION('ref_axis',(0.857167300702112,0.515038074910055,0.));
#32728=DIRECTION('',(0.,-1.,0.));
#32729=DIRECTION('',(0.707106781186548,-0.707106781186547,0.));
#32730=DIRECTION('',(1.,0.,0.));
#32731=DIRECTION('center_axis',(0.,0.,1.));
#32732=DIRECTION('ref_axis',(0.707106781186547,-0.707106781186548,0.));
#32733=DIRECTION('',(3.28954970259306E-16,1.,0.));
#32734=DIRECTION('center_axis',(0.,0.,1.));
#32735=DIRECTION('ref_axis',(0.923879532511287,0.38268343236509,0.));
#32736=DIRECTION('',(-0.707106781186548,0.707106781186547,0.));
#32737=DIRECTION('center_axis',(-0.707106781186548,0.707106781186547,0.));
#32738=DIRECTION('ref_axis',(0.5,0.500000000000001,0.707106781186547));
#32739=DIRECTION('center_axis',(0.707106781186548,-0.707106781186548,0.));
#32740=DIRECTION('ref_axis',(0.707106781186548,0.707106781186548,0.));
#32741=DIRECTION('',(0.707106781186548,-0.707106781186547,0.));
#32742=DIRECTION('center_axis',(0.707106781186548,-0.707106781186548,0.));
#32743=DIRECTION('ref_axis',(0.707106781186548,0.707106781186548,0.));
#32744=DIRECTION('center_axis',(0.,0.,1.));
#32745=DIRECTION('ref_axis',(-1.,0.,0.));
#32746=DIRECTION('center_axis',(0.,0.,-1.));
#32747=DIRECTION('ref_axis',(0.674283564945582,0.738472527616483,0.));
#32748=DIRECTION('center_axis',(0.999999999362884,-3.5696397100931E-5,0.));
#32749=DIRECTION('ref_axis',(-2.52411644539961E-5,-0.707106780736038,0.707106781186548));
#32750=DIRECTION('center_axis',(0.923893192342434,0.38265045295061,-1.69930937299605E-15));
#32751=DIRECTION('ref_axis',(0.38265045295061,-0.923893192342434,4.10249573495478E-15));
#32752=DIRECTION('center_axis',(-0.999999999362884,3.56963971004376E-5,
0.));
#32753=DIRECTION('ref_axis',(-3.56963971004376E-5,-0.999999999362884,0.));
#32754=DIRECTION('center_axis',(3.56963971048783E-5,0.999999999362884,0.));
#32755=DIRECTION('ref_axis',(-0.999999999362884,3.56963971048783E-5,0.));
#32756=DIRECTION('center_axis',(-3.56963971007665E-5,-0.999999999362884,
0.));
#32757=DIRECTION('ref_axis',(-0.707106780736035,2.52411644538797E-5,0.707106781186551));
#32758=DIRECTION('center_axis',(3.56963971004377E-5,0.999999999362884,0.));
#32759=DIRECTION('ref_axis',(-0.999999999362884,3.56963971004377E-5,0.));
#32760=DIRECTION('center_axis',(0.,0.,1.));
#32761=DIRECTION('ref_axis',(-1.,0.,0.));
#32762=DIRECTION('center_axis',(0.,0.,1.));
#32763=DIRECTION('ref_axis',(-1.,0.,0.));
#32764=DIRECTION('center_axis',(0.707132021900493,0.707081539571584,0.));
#32765=DIRECTION('ref_axis',(0.499982151482891,-0.500017847879993,0.707106781186548));
#32766=DIRECTION('center_axis',(0.382716411291948,0.9238658715029,-4.10278864883162E-15));
#32767=DIRECTION('ref_axis',(0.9238658715029,-0.382716411291948,9.90500799955984E-15));
#32768=DIRECTION('center_axis',(0.882964350739721,0.469440044438886,0.));
#32769=DIRECTION('ref_axis',(0.33194423878325,-0.624350079954033,0.707106781186549));
#32770=DIRECTION('center_axis',(0.970304361397861,0.241887259383973,0.));
#32771=DIRECTION('ref_axis',(-0.241887259383973,0.970304361397861,0.));
#32772=DIRECTION('center_axis',(-0.88296435073972,-0.469440044438887,0.));
#32773=DIRECTION('ref_axis',(0.469440044438887,-0.88296435073972,0.));
#32774=DIRECTION('center_axis',(0.,0.,-1.));
#32775=DIRECTION('ref_axis',(1.,0.,0.));
#32776=DIRECTION('center_axis',(-3.56963971004376E-5,-0.999999999362884,
0.));
#32777=DIRECTION('ref_axis',(0.999999999362884,-3.56963971004376E-5,0.));
#32778=DIRECTION('center_axis',(3.56963971014961E-5,0.999999999362884,0.));
#32779=DIRECTION('ref_axis',(0.707106780736038,-2.52411644543957E-5,0.707106781186548));
#32780=DIRECTION('center_axis',(1.,0.,0.));
#32781=DIRECTION('ref_axis',(0.,-0.707106781186548,0.707106781186548));
#32782=DIRECTION('',(-1.,0.,0.));
#32783=DIRECTION('center_axis',(0.970295726275993,-0.241921895599681,0.));
#32784=DIRECTION('ref_axis',(0.241921895599681,0.970295726275993,0.));
#32785=DIRECTION('center_axis',(-1.,0.,0.));
#32786=DIRECTION('ref_axis',(0.,-1.,0.));
#32787=DIRECTION('center_axis',(0.999999999840721,-1.7848198553344E-5,0.));
#32788=DIRECTION('ref_axis',(-1.26205822290334E-5,-0.707106781073918,0.70710678118655));
#32789=DIRECTION('center_axis',(-0.999999999840721,1.78481985502188E-5,
0.));
#32790=DIRECTION('ref_axis',(-1.78481985502188E-5,-0.999999999840721,0.));
#32791=DIRECTION('',(-0.999999999840721,1.7848198553344E-5,0.));
#32792=DIRECTION('center_axis',(0.999999999362884,-3.56963971010297E-5,
0.));
#32793=DIRECTION('ref_axis',(-2.52411644540658E-5,-0.707106780736035,0.707106781186551));
#32794=DIRECTION('',(-0.999999999362884,3.56963971010297E-5,0.));
#32795=DIRECTION('center_axis',(0.,-1.,0.));
#32796=DIRECTION('ref_axis',(-0.707106781186551,0.,0.707106781186544));
#32797=DIRECTION('',(0.,1.,0.));
#32798=DIRECTION('center_axis',(0.382683432365083,-0.92387953251129,0.));
#32799=DIRECTION('ref_axis',(-0.92387953251129,-0.382683432365083,0.));
#32800=DIRECTION('center_axis',(0.,1.,0.));
#32801=DIRECTION('ref_axis',(-1.,0.,0.));
#32802=DIRECTION('center_axis',(0.,0.,-1.));
#32803=DIRECTION('ref_axis',(1.,0.,0.));
#32804=DIRECTION('center_axis',(-0.88294759285893,0.469471562785885,0.));
#32805=DIRECTION('ref_axis',(-0.469471562785885,-0.88294759285893,0.));
#32806=DIRECTION('center_axis',(0.,0.,1.));
#32807=DIRECTION('ref_axis',(0.857167300702112,0.515038074910055,0.));
#32808=DIRECTION('center_axis',(0.882947592858928,-0.46947156278589,0.));
#32809=DIRECTION('ref_axis',(-0.331966525620151,-0.624338230342891,0.707106781186542));
#32810=DIRECTION('',(-0.882947592858928,0.46947156278589,0.));
#32811=DIRECTION('center_axis',(0.707106781186548,-0.707106781186547,0.));
#32812=DIRECTION('ref_axis',(-0.5,-0.500000000000001,0.707106781186547));
#32813=DIRECTION('',(-0.707106781186548,0.707106781186547,0.));
#32814=DIRECTION('center_axis',(0.92387953251129,-0.382683432365083,0.));
#32815=DIRECTION('ref_axis',(-0.382683432365083,-0.92387953251129,0.));
#32816=DIRECTION('center_axis',(0.,0.,1.));
#32817=DIRECTION('ref_axis',(-1.,0.,0.));
#32818=DIRECTION('center_axis',(0.,-1.,0.));
#32819=DIRECTION('ref_axis',(1.,0.,0.));
#32820=DIRECTION('center_axis',(0.,0.,-1.));
#32821=DIRECTION('ref_axis',(0.923879532511287,0.38268343236509,0.));
#32822=DIRECTION('center_axis',(3.28954970259306E-16,1.,0.));
#32823=DIRECTION('ref_axis',(0.707106781186548,-2.32606290175374E-16,0.707106781186548));
#32824=DIRECTION('center_axis',(0.,-1.,0.));
#32825=DIRECTION('ref_axis',(1.,0.,0.));
#32826=DIRECTION('',(-3.28954970259306E-16,-1.,0.));
#32827=DIRECTION('center_axis',(-1.,0.,0.));
#32828=DIRECTION('ref_axis',(0.,-1.,0.));
#32829=DIRECTION('center_axis',(0.,0.,-1.));
#32830=DIRECTION('ref_axis',(0.707106781186546,-0.707106781186549,0.));
#32831=DIRECTION('center_axis',(1.,0.,0.));
#32832=DIRECTION('ref_axis',(0.,-0.707106781186548,0.707106781186548));
#32833=DIRECTION('',(-1.,0.,0.));
#32834=DIRECTION('center_axis',(3.56963971010297E-5,0.999999999362884,0.));
#32835=DIRECTION('ref_axis',(-0.999999999362884,3.56963971010297E-5,0.));
#32836=DIRECTION('',(0.,0.,1.));
#32837=DIRECTION('center_axis',(1.7848198553344E-5,0.999999999840721,0.));
#32838=DIRECTION('ref_axis',(-0.999999999840721,1.7848198553344E-5,0.));
#32839=DIRECTION('',(0.,0.,1.));
#32840=DIRECTION('center_axis',(0.,1.,0.));
#32841=DIRECTION('ref_axis',(-1.,0.,0.));
#32842=DIRECTION('',(0.,0.,1.));
#32843=DIRECTION('center_axis',(0.46947156278589,0.882947592858928,0.));
#32844=DIRECTION('ref_axis',(-0.882947592858928,0.46947156278589,0.));
#32845=DIRECTION('',(0.,0.,1.));
#32846=DIRECTION('center_axis',(0.,0.,-1.));
#32847=DIRECTION('ref_axis',(0.469471562785885,0.88294759285893,0.));
#32848=DIRECTION('',(0.,0.,1.));
#32849=DIRECTION('center_axis',(1.,0.,0.));
#32850=DIRECTION('ref_axis',(0.,1.,0.));
#32851=DIRECTION('',(0.,0.,1.));
#32852=DIRECTION('center_axis',(0.707106781186547,0.707106781186548,0.));
#32853=DIRECTION('ref_axis',(-0.707106781186548,0.707106781186547,0.));
#32854=DIRECTION('',(0.,0.,1.));
#32855=DIRECTION('center_axis',(0.,1.,0.));
#32856=DIRECTION('ref_axis',(-1.,0.,0.));
#32857=DIRECTION('',(0.,0.,1.));
#32858=DIRECTION('center_axis',(0.,0.,-1.));
#32859=DIRECTION('ref_axis',(1.,0.,0.));
#32860=DIRECTION('',(0.,0.,1.));
#32861=DIRECTION('center_axis',(-1.,3.28954970259306E-16,0.));
#32862=DIRECTION('ref_axis',(-3.28954970259306E-16,-1.,0.));
#32863=DIRECTION('',(0.,0.,1.));
#32864=DIRECTION('center_axis',(0.,0.,-1.));
#32865=DIRECTION('ref_axis',(0.707106781186547,0.707106781186548,0.));
#32866=DIRECTION('',(0.,0.,1.));
#32867=DIRECTION('center_axis',(-0.707106781186547,-0.707106781186548,0.));
#32868=DIRECTION('ref_axis',(0.707106781186548,-0.707106781186547,0.));
#32869=DIRECTION('',(0.,0.,1.));
#32870=DIRECTION('center_axis',(0.,0.,-1.));
#32871=DIRECTION('ref_axis',(1.48029736616687E-15,1.,0.));
#32872=DIRECTION('',(0.,0.,1.));
#32873=DIRECTION('center_axis',(0.,0.,1.));
#32874=DIRECTION('ref_axis',(1.48029736616687E-15,1.,0.));
#32875=DIRECTION('',(0.,0.,-1.));
#32876=DIRECTION('center_axis',(0.,0.,1.));
#32877=DIRECTION('ref_axis',(-1.,0.,0.));
#32878=DIRECTION('center_axis',(0.,0.,1.));
#32879=DIRECTION('ref_axis',(-1.,0.,0.));
#32880=DIRECTION('',(0.,0.,1.));
#32881=DIRECTION('center_axis',(0.,0.,1.));
#32882=DIRECTION('ref_axis',(0.836944376135179,-0.547287960086548,0.));
#32883=DIRECTION('center_axis',(0.,0.,1.));
#32884=DIRECTION('ref_axis',(-1.,0.,0.));
#32885=DIRECTION('center_axis',(0.,0.,-1.));
#32886=DIRECTION('ref_axis',(-1.,0.,0.));
#32887=DIRECTION('center_axis',(0.,0.,-1.));
#32888=DIRECTION('ref_axis',(-1.,0.,0.));
#32889=DIRECTION('',(-1.,0.,0.));
#32890=DIRECTION('center_axis',(0.,0.,-1.));
#32891=DIRECTION('ref_axis',(0.,-1.,0.));
#32892=DIRECTION('',(0.,1.,0.));
#32893=DIRECTION('center_axis',(0.,-1.,0.));
#32894=DIRECTION('ref_axis',(1.,0.,0.));
#32895=DIRECTION('',(0.,0.,1.));
#32896=DIRECTION('center_axis',(0.,0.,-1.));
#32897=DIRECTION('ref_axis',(0.,-1.,0.));
#32898=DIRECTION('',(0.,0.,1.));
#32899=DIRECTION('center_axis',(-1.,0.,0.));
#32900=DIRECTION('ref_axis',(0.,-1.,0.));
#32901=DIRECTION('',(0.,0.,1.));
#32902=DIRECTION('center_axis',(0.,0.,-1.));
#32903=DIRECTION('ref_axis',(-4.44089209850064E-15,1.,0.));
#32904=DIRECTION('center_axis',(-3.56963957938316E-5,-0.999999999362884,
0.));
#32905=DIRECTION('ref_axis',(0.,0.,-1.));
#32906=DIRECTION('center_axis',(0.,-1.,0.));
#32907=DIRECTION('ref_axis',(1.,0.,0.));
#32908=DIRECTION('center_axis',(-3.56963971012317E-5,-0.999999999362884,
0.));
#32909=DIRECTION('ref_axis',(0.,0.,-1.));
#32910=DIRECTION('',(-3.56963957938316E-5,-0.999999999362884,0.));
#32911=DIRECTION('center_axis',(-3.56963957938316E-5,-0.999999999362884,
0.));
#32912=DIRECTION('ref_axis',(0.,0.,-1.));
#32913=DIRECTION('center_axis',(3.56963957938316E-5,0.999999999362884,0.));
#32914=DIRECTION('ref_axis',(0.,0.,-1.));
#32915=DIRECTION('center_axis',(-3.56963957938316E-5,-0.999999999362884,
0.));
#32916=DIRECTION('ref_axis',(0.,0.,-1.));
#32917=DIRECTION('center_axis',(0.,-1.,0.));
#32918=DIRECTION('ref_axis',(1.,0.,0.));
#32919=DIRECTION('center_axis',(-3.56963971012317E-5,-0.999999999362884,
0.));
#32920=DIRECTION('ref_axis',(0.,0.,-1.));
#32921=DIRECTION('',(-3.56963957938316E-5,-0.999999999362884,0.));
#32922=DIRECTION('center_axis',(-3.56963957938316E-5,-0.999999999362884,
0.));
#32923=DIRECTION('ref_axis',(0.,0.,-1.));
#32924=DIRECTION('center_axis',(3.56963957938316E-5,0.999999999362884,0.));
#32925=DIRECTION('ref_axis',(0.,0.,-1.));
#32926=DIRECTION('center_axis',(0.,1.,0.));
#32927=DIRECTION('ref_axis',(-1.,0.,0.));
#32928=DIRECTION('',(0.,0.,1.));
#32929=DIRECTION('',(0.,0.,1.));
#32930=DIRECTION('',(-1.,0.,0.));
#32931=DIRECTION('',(0.,0.,1.));
#32932=DIRECTION('',(-1.,0.,0.));
#32933=DIRECTION('',(0.,0.,1.));
#32934=DIRECTION('center_axis',(-0.999999999362884,3.56963971012317E-5,
0.));
#32935=DIRECTION('ref_axis',(0.,0.,1.));
#32936=DIRECTION('',(0.,0.,1.));
#32937=DIRECTION('center_axis',(0.999999999362884,-3.56963971012317E-5,
0.));
#32938=DIRECTION('ref_axis',(0.,0.,1.));
#32939=DIRECTION('center_axis',(0.999999999362884,-3.56963971012835E-5,
0.));
#32940=DIRECTION('ref_axis',(0.,0.,1.));
#32941=DIRECTION('center_axis',(0.999999999362884,-3.56963971012317E-5,
0.));
#32942=DIRECTION('ref_axis',(0.,0.,1.));
#32943=DIRECTION('',(0.999999999362884,-3.56963971012835E-5,0.));
#32944=DIRECTION('center_axis',(-0.999999999362884,3.56963971012317E-5,
0.));
#32945=DIRECTION('ref_axis',(0.,0.,1.));
#32946=DIRECTION('',(-0.999999999362884,3.56963971012835E-5,0.));
#32947=DIRECTION('',(0.999999999362884,-3.56963971012835E-5,0.));
#32948=DIRECTION('center_axis',(-0.999999999362884,3.56963971012317E-5,
0.));
#32949=DIRECTION('ref_axis',(0.,0.,1.));
#32950=DIRECTION('center_axis',(-0.707132021900494,-0.707081539571582,0.));
#32951=DIRECTION('ref_axis',(0.707081539571582,-0.707132021900494,0.));
#32952=DIRECTION('',(-0.999999999362884,3.56963971012835E-5,0.));
#32953=DIRECTION('center_axis',(0.707081539571582,-0.707132021900494,0.));
#32954=DIRECTION('ref_axis',(-0.707132021900494,-0.707081539571582,0.));
#32955=DIRECTION('',(0.999999999362884,-3.56963971012835E-5,0.));
#32956=DIRECTION('',(-0.999999999362884,3.56963971012835E-5,0.));
#32957=DIRECTION('center_axis',(0.707081539571582,-0.707132021900494,0.));
#32958=DIRECTION('ref_axis',(-0.707132021900494,-0.707081539571582,0.));
#32959=DIRECTION('',(0.999999999362884,-3.56963971012835E-5,0.));
#32960=DIRECTION('center_axis',(-0.707106781186546,-0.707106781186549,0.));
#32961=DIRECTION('ref_axis',(0.707106781186549,-0.707106781186546,0.));
#32962=DIRECTION('',(-0.999999996715682,-1.14900183283708E-14,-8.104711771334E-5));
#32963=DIRECTION('',(0.999999996715682,1.14900183283708E-14,-8.104711771334E-5));
#32964=DIRECTION('center_axis',(-0.707106781186546,-0.707106781186549,0.));
#32965=DIRECTION('ref_axis',(0.707106781186549,-0.707106781186546,0.));
#32966=DIRECTION('',(-0.999999999639016,-4.22740799323897E-15,-2.68694483879996E-5));
#32967=DIRECTION('center_axis',(0.707106781186549,-0.707106781186546,0.));
#32968=DIRECTION('ref_axis',(-0.707106781186546,-0.707106781186549,0.));
#32969=DIRECTION('center_axis',(1.,0.,0.));
#32970=DIRECTION('ref_axis',(0.,-1.,0.));
#32971=DIRECTION('',(0.999999996701292,0.,-8.12244748976037E-5));
#32972=DIRECTION('',(-0.999999996701292,0.,-8.12244748976037E-5));
#32973=DIRECTION('center_axis',(1.,0.,0.));
#32974=DIRECTION('ref_axis',(0.,-1.,0.));
#32975=DIRECTION('',(0.999999999362884,-3.56963971012835E-5,0.));
#32976=DIRECTION('center_axis',(-1.,0.,0.));
#32977=DIRECTION('ref_axis',(0.,-1.,0.));
#32978=DIRECTION('center_axis',(-1.,0.,0.));
#32979=DIRECTION('ref_axis',(0.,-1.,0.));
#32980=DIRECTION('center_axis',(0.707106781186549,-0.707106781186546,0.));
#32981=DIRECTION('ref_axis',(-0.707106781186546,-0.707106781186549,0.));
#32982=DIRECTION('',(0.999999999639016,4.22740799323897E-15,-2.68694483879996E-5));
#32983=DIRECTION('center_axis',(-0.707106781186546,-0.707106781186549,0.));
#32984=DIRECTION('ref_axis',(0.707106781186549,-0.707106781186546,0.));
#32985=DIRECTION('center_axis',(0.707081539571582,-0.707132021900494,0.));
#32986=DIRECTION('ref_axis',(-0.707132021900494,-0.707081539571582,0.));
#32987=DIRECTION('',(0.999999999362884,-3.56963971012835E-5,0.));
#32988=DIRECTION('center_axis',(-0.707132021900494,-0.707081539571582,0.));
#32989=DIRECTION('ref_axis',(0.707081539571582,-0.707132021900494,0.));
#32990=DIRECTION('center_axis',(-0.999999999362884,3.56963971012317E-5,
0.));
#32991=DIRECTION('ref_axis',(0.,0.,1.));
#32992=DIRECTION('',(0.,0.,1.));
#32993=DIRECTION('center_axis',(0.999999999362884,-3.56963971012317E-5,
0.));
#32994=DIRECTION('ref_axis',(0.,0.,1.));
#32995=DIRECTION('center_axis',(0.999999999362884,-3.56963971012835E-5,
0.));
#32996=DIRECTION('ref_axis',(0.,0.,1.));
#32997=DIRECTION('center_axis',(0.999999999362884,-3.56963971012317E-5,
0.));
#32998=DIRECTION('ref_axis',(0.,0.,1.));
#32999=DIRECTION('',(0.999999999362884,-3.56963971012835E-5,0.));
#33000=DIRECTION('center_axis',(-0.999999999362884,3.56963971012317E-5,
0.));
#33001=DIRECTION('ref_axis',(0.,0.,1.));
#33002=DIRECTION('',(-0.999999999362884,3.56963971012835E-5,0.));
#33003=DIRECTION('',(0.999999999362884,-3.56963971012835E-5,0.));
#33004=DIRECTION('center_axis',(-0.999999999362884,3.56963971012317E-5,
0.));
#33005=DIRECTION('ref_axis',(0.,0.,1.));
#33006=DIRECTION('center_axis',(-0.707132021900494,-0.707081539571582,0.));
#33007=DIRECTION('ref_axis',(0.707081539571582,-0.707132021900494,0.));
#33008=DIRECTION('',(-0.999999999362884,3.56963971012835E-5,0.));
#33009=DIRECTION('center_axis',(0.707081539571582,-0.707132021900494,0.));
#33010=DIRECTION('ref_axis',(-0.707132021900494,-0.707081539571582,0.));
#33011=DIRECTION('',(0.999999999362884,-3.56963971012835E-5,0.));
#33012=DIRECTION('',(-0.999999999362884,3.56963971012835E-5,0.));
#33013=DIRECTION('center_axis',(0.707081539571582,-0.707132021900494,0.));
#33014=DIRECTION('ref_axis',(-0.707132021900494,-0.707081539571582,0.));
#33015=DIRECTION('',(0.999999999362884,-3.56963971012835E-5,0.));
#33016=DIRECTION('center_axis',(-0.707106781186546,-0.707106781186549,0.));
#33017=DIRECTION('ref_axis',(0.707106781186549,-0.707106781186546,0.));
#33018=DIRECTION('',(-0.999999996715682,-1.14900183283708E-14,-8.104711771334E-5));
#33019=DIRECTION('',(0.999999996715682,1.14900183283708E-14,-8.104711771334E-5));
#33020=DIRECTION('center_axis',(-0.707106781186546,-0.707106781186549,0.));
#33021=DIRECTION('ref_axis',(0.707106781186549,-0.707106781186546,0.));
#33022=DIRECTION('',(-0.999999999639016,-4.22740799323897E-15,-2.68694483879996E-5));
#33023=DIRECTION('center_axis',(0.707106781186549,-0.707106781186546,0.));
#33024=DIRECTION('ref_axis',(-0.707106781186546,-0.707106781186549,0.));
#33025=DIRECTION('center_axis',(1.,0.,0.));
#33026=DIRECTION('ref_axis',(0.,-1.,0.));
#33027=DIRECTION('',(0.999999996701292,0.,-8.12244748976037E-5));
#33028=DIRECTION('',(-0.999999996701292,0.,-8.12244748976037E-5));
#33029=DIRECTION('center_axis',(1.,0.,0.));
#33030=DIRECTION('ref_axis',(0.,-1.,0.));
#33031=DIRECTION('',(0.999999999362884,-3.56963971012835E-5,0.));
#33032=DIRECTION('center_axis',(-1.,0.,0.));
#33033=DIRECTION('ref_axis',(0.,-1.,0.));
#33034=DIRECTION('center_axis',(-1.,0.,0.));
#33035=DIRECTION('ref_axis',(0.,-1.,0.));
#33036=DIRECTION('center_axis',(0.707106781186549,-0.707106781186546,0.));
#33037=DIRECTION('ref_axis',(-0.707106781186546,-0.707106781186549,0.));
#33038=DIRECTION('',(0.999999999639016,4.22740799323897E-15,-2.68694483879996E-5));
#33039=DIRECTION('center_axis',(-0.707106781186546,-0.707106781186549,0.));
#33040=DIRECTION('ref_axis',(0.707106781186549,-0.707106781186546,0.));
#33041=DIRECTION('center_axis',(0.707081539571582,-0.707132021900494,0.));
#33042=DIRECTION('ref_axis',(-0.707132021900494,-0.707081539571582,0.));
#33043=DIRECTION('',(0.999999999362884,-3.56963971012835E-5,0.));
#33044=DIRECTION('center_axis',(-0.707132021900494,-0.707081539571582,0.));
#33045=DIRECTION('ref_axis',(0.707081539571582,-0.707132021900494,0.));
#33046=DIRECTION('center_axis',(-0.999999999362884,3.56963971012317E-5,
0.));
#33047=DIRECTION('ref_axis',(0.,0.,1.));
#33048=DIRECTION('',(0.,0.,1.));
#33049=DIRECTION('center_axis',(0.999999999362884,-3.56963971012317E-5,
0.));
#33050=DIRECTION('ref_axis',(0.,0.,1.));
#33051=DIRECTION('center_axis',(0.999999999362884,-3.56963971012835E-5,
0.));
#33052=DIRECTION('ref_axis',(0.,0.,1.));
#33053=DIRECTION('center_axis',(0.999999999362884,-3.56963971012317E-5,
0.));
#33054=DIRECTION('ref_axis',(0.,0.,1.));
#33055=DIRECTION('',(0.999999999362884,-3.56963971012835E-5,0.));
#33056=DIRECTION('center_axis',(-0.999999999362884,3.56963971012317E-5,
0.));
#33057=DIRECTION('ref_axis',(0.,0.,1.));
#33058=DIRECTION('',(-0.999999999362884,3.56963971012835E-5,0.));
#33059=DIRECTION('',(0.999999999362884,-3.56963971012835E-5,0.));
#33060=DIRECTION('center_axis',(-0.999999999362884,3.56963971012317E-5,
0.));
#33061=DIRECTION('ref_axis',(0.,0.,1.));
#33062=DIRECTION('center_axis',(-0.707132021900494,-0.707081539571582,0.));
#33063=DIRECTION('ref_axis',(0.707081539571582,-0.707132021900494,0.));
#33064=DIRECTION('',(-0.999999999362884,3.56963971012835E-5,0.));
#33065=DIRECTION('center_axis',(0.707081539571582,-0.707132021900494,0.));
#33066=DIRECTION('ref_axis',(-0.707132021900494,-0.707081539571582,0.));
#33067=DIRECTION('',(0.999999999362884,-3.56963971012835E-5,0.));
#33068=DIRECTION('',(-0.999999999362884,3.56963971012835E-5,0.));
#33069=DIRECTION('center_axis',(0.707081539571582,-0.707132021900494,0.));
#33070=DIRECTION('ref_axis',(-0.707132021900494,-0.707081539571582,0.));
#33071=DIRECTION('',(0.999999999362884,-3.56963971012835E-5,0.));
#33072=DIRECTION('center_axis',(-0.707106781186546,-0.707106781186549,0.));
#33073=DIRECTION('ref_axis',(0.707106781186549,-0.707106781186546,0.));
#33074=DIRECTION('',(-0.999999996715682,-1.14900183283708E-14,-8.10471177095101E-5));
#33075=DIRECTION('',(0.999999996715682,1.14900183283708E-14,-8.10471177095101E-5));
#33076=DIRECTION('center_axis',(-0.707106781186546,-0.707106781186549,0.));
#33077=DIRECTION('ref_axis',(0.707106781186549,-0.707106781186546,0.));
#33078=DIRECTION('',(-0.999999999639016,-4.22740799323898E-15,-2.6869448392227E-5));
#33079=DIRECTION('center_axis',(0.707106781186549,-0.707106781186546,0.));
#33080=DIRECTION('ref_axis',(-0.707106781186546,-0.707106781186549,0.));
#33081=DIRECTION('center_axis',(1.,0.,0.));
#33082=DIRECTION('ref_axis',(0.,-1.,0.));
#33083=DIRECTION('',(0.999999996701292,0.,-8.12244748976037E-5));
#33084=DIRECTION('',(-0.999999996701292,0.,-8.12244748976037E-5));
#33085=DIRECTION('center_axis',(1.,0.,0.));
#33086=DIRECTION('ref_axis',(0.,-1.,0.));
#33087=DIRECTION('',(0.999999999362884,-3.56963971012835E-5,0.));
#33088=DIRECTION('center_axis',(-1.,0.,0.));
#33089=DIRECTION('ref_axis',(0.,-1.,0.));
#33090=DIRECTION('center_axis',(-1.,0.,0.));
#33091=DIRECTION('ref_axis',(0.,-1.,0.));
#33092=DIRECTION('center_axis',(0.707106781186549,-0.707106781186546,0.));
#33093=DIRECTION('ref_axis',(-0.707106781186546,-0.707106781186549,0.));
#33094=DIRECTION('',(0.999999999639016,4.22740799323898E-15,-2.6869448392227E-5));
#33095=DIRECTION('center_axis',(-0.707106781186546,-0.707106781186549,0.));
#33096=DIRECTION('ref_axis',(0.707106781186549,-0.707106781186546,0.));
#33097=DIRECTION('center_axis',(0.707081539571582,-0.707132021900494,0.));
#33098=DIRECTION('ref_axis',(-0.707132021900494,-0.707081539571582,0.));
#33099=DIRECTION('',(0.999999999362884,-3.56963971012835E-5,0.));
#33100=DIRECTION('center_axis',(-0.707132021900494,-0.707081539571582,0.));
#33101=DIRECTION('ref_axis',(0.707081539571582,-0.707132021900494,0.));
#33102=DIRECTION('center_axis',(0.,0.,-1.));
#33103=DIRECTION('ref_axis',(0.999999999362884,-3.56963971012317E-5,0.));
#33104=DIRECTION('',(0.,0.,1.));
#33105=DIRECTION('center_axis',(0.,0.,-1.));
#33106=DIRECTION('ref_axis',(0.999999999362884,-3.56963971012317E-5,0.));
#33107=DIRECTION('',(0.,0.,1.));
#33108=DIRECTION('center_axis',(0.,0.,-1.));
#33109=DIRECTION('ref_axis',(0.999999999362884,-3.56963971012317E-5,0.));
#33110=DIRECTION('',(0.,0.,1.));
#33111=DIRECTION('',(0.,0.,1.));
#33112=DIRECTION('',(0.,0.,1.));
#33113=DIRECTION('center_axis',(3.56963971012317E-5,0.999999999362884,0.));
#33114=DIRECTION('ref_axis',(-0.999999999362884,3.56963971012317E-5,0.));
#33115=DIRECTION('',(0.,0.,1.));
#33116=DIRECTION('',(-0.999999999362884,3.56963971012317E-5,0.));
#33117=DIRECTION('center_axis',(3.56963971012317E-5,0.999999999362884,0.));
#33118=DIRECTION('ref_axis',(-0.999999999362884,3.56963971012317E-5,0.));
#33119=DIRECTION('',(-0.999999999362884,3.56963971012317E-5,0.));
#33120=DIRECTION('',(0.,0.,1.));
#33121=DIRECTION('center_axis',(3.56963971012317E-5,0.999999999362884,0.));
#33122=DIRECTION('ref_axis',(-0.999999999362884,3.56963971012317E-5,0.));
#33123=DIRECTION('',(0.,0.,1.));
#33124=DIRECTION('center_axis',(0.,0.,-1.));
#33125=DIRECTION('ref_axis',(-0.999999999362884,3.56963971012317E-5,0.));
#33126=DIRECTION('',(0.,0.,1.));
#33127=DIRECTION('center_axis',(0.,0.,-1.));
#33128=DIRECTION('ref_axis',(-0.999999999362884,3.56963971012317E-5,0.));
#33129=DIRECTION('center_axis',(0.,0.,-1.));
#33130=DIRECTION('ref_axis',(-0.999999999362884,3.56963971012317E-5,0.));
#33131=DIRECTION('center_axis',(0.,0.,1.));
#33132=DIRECTION('ref_axis',(-0.999999999362884,3.56963971012317E-5,0.));
#33133=DIRECTION('',(0.,0.,1.));
#33134=DIRECTION('center_axis',(0.,0.,-1.));
#33135=DIRECTION('ref_axis',(-0.999999999362884,3.56963971012317E-5,0.));
#33136=DIRECTION('',(0.,0.,1.));
#33137=DIRECTION('center_axis',(-0.999999999362884,3.56963971012317E-5,
0.));
#33138=DIRECTION('ref_axis',(-3.56963971012317E-5,-0.999999999362884,0.));
#33139=DIRECTION('',(0.,0.,1.));
#33140=DIRECTION('',(-3.56963971012317E-5,-0.999999999362884,0.));
#33141=DIRECTION('center_axis',(-0.999999999362884,3.56963971012317E-5,
0.));
#33142=DIRECTION('ref_axis',(-3.56963971012317E-5,-0.999999999362884,0.));
#33143=DIRECTION('',(-3.56963971012317E-5,-0.999999999362884,0.));
#33144=DIRECTION('',(0.,0.,1.));
#33145=DIRECTION('center_axis',(-0.999999999362884,3.56963971012317E-5,
0.));
#33146=DIRECTION('ref_axis',(-3.56963971012317E-5,-0.999999999362884,0.));
#33147=DIRECTION('',(0.,0.,1.));
#33148=DIRECTION('center_axis',(0.,0.,-1.));
#33149=DIRECTION('ref_axis',(-0.707132021900495,-0.707081539571582,0.));
#33150=DIRECTION('',(0.,0.,1.));
#33151=DIRECTION('center_axis',(0.,0.,-1.));
#33152=DIRECTION('ref_axis',(-0.707132021900495,-0.707081539571582,0.));
#33153=DIRECTION('center_axis',(0.,0.,-1.));
#33154=DIRECTION('ref_axis',(-0.707132021900495,-0.707081539571582,0.));
#33155=DIRECTION('center_axis',(0.,0.,1.));
#33156=DIRECTION('ref_axis',(-0.707132021900495,-0.707081539571582,0.));
#33157=DIRECTION('',(0.,0.,1.));
#33158=DIRECTION('center_axis',(0.,0.,-1.));
#33159=DIRECTION('ref_axis',(-0.707132021900495,-0.707081539571582,0.));
#33160=DIRECTION('',(0.,0.,1.));
#33161=DIRECTION('center_axis',(-0.707132021900494,-0.707081539571582,0.));
#33162=DIRECTION('ref_axis',(0.707081539571582,-0.707132021900494,0.));
#33163=DIRECTION('',(0.,0.,1.));
#33164=DIRECTION('',(0.707081539571582,-0.707132021900494,0.));
#33165=DIRECTION('center_axis',(-0.707132021900494,-0.707081539571582,0.));
#33166=DIRECTION('ref_axis',(0.707081539571582,-0.707132021900494,0.));
#33167=DIRECTION('',(0.707081539571582,-0.707132021900494,0.));
#33168=DIRECTION('',(0.,0.,1.));
#33169=DIRECTION('center_axis',(-0.707132021900494,-0.707081539571582,0.));
#33170=DIRECTION('ref_axis',(0.707081539571582,-0.707132021900494,0.));
#33171=DIRECTION('',(0.,0.,1.));
#33172=DIRECTION('center_axis',(0.,0.,-1.));
#33173=DIRECTION('ref_axis',(-3.56963971045624E-5,-0.999999999362884,0.));
#33174=DIRECTION('',(0.,0.,1.));
#33175=DIRECTION('center_axis',(0.,0.,-1.));
#33176=DIRECTION('ref_axis',(-3.56963971045624E-5,-0.999999999362884,0.));
#33177=DIRECTION('center_axis',(0.,0.,-1.));
#33178=DIRECTION('ref_axis',(-3.56963971045624E-5,-0.999999999362884,0.));
#33179=DIRECTION('center_axis',(0.,0.,1.));
#33180=DIRECTION('ref_axis',(-3.56963971045624E-5,-0.999999999362884,0.));
#33181=DIRECTION('',(0.,0.,1.));
#33182=DIRECTION('center_axis',(0.,0.,-1.));
#33183=DIRECTION('ref_axis',(-3.56963971045624E-5,-0.999999999362884,0.));
#33184=DIRECTION('',(0.,0.,1.));
#33185=DIRECTION('center_axis',(-3.56963971054591E-5,-0.999999999362884,
0.));
#33186=DIRECTION('ref_axis',(0.999999999362884,-3.56963971054591E-5,0.));
#33187=DIRECTION('',(0.,0.,1.));
#33188=DIRECTION('',(0.999999999362884,-3.56963971054591E-5,0.));
#33189=DIRECTION('center_axis',(-3.56963971054591E-5,-0.999999999362884,
0.));
#33190=DIRECTION('ref_axis',(0.999999999362884,-3.56963971054591E-5,0.));
#33191=DIRECTION('',(0.999999999362884,-3.56963971054591E-5,0.));
#33192=DIRECTION('',(0.,0.,1.));
#33193=DIRECTION('center_axis',(-3.56963971054591E-5,-0.999999999362884,
0.));
#33194=DIRECTION('ref_axis',(0.999999999362884,-3.56963971054591E-5,0.));
#33195=DIRECTION('',(0.,0.,1.));
#33196=DIRECTION('center_axis',(0.,0.,-1.));
#33197=DIRECTION('ref_axis',(0.707081539571582,-0.707132021900495,0.));
#33198=DIRECTION('',(0.,0.,1.));
#33199=DIRECTION('center_axis',(0.,0.,-1.));
#33200=DIRECTION('ref_axis',(0.707081539571582,-0.707132021900495,0.));
#33201=DIRECTION('center_axis',(0.,0.,-1.));
#33202=DIRECTION('ref_axis',(0.707081539571582,-0.707132021900495,0.));
#33203=DIRECTION('center_axis',(0.,0.,1.));
#33204=DIRECTION('ref_axis',(0.707081539571582,-0.707132021900495,0.));
#33205=DIRECTION('',(0.,0.,1.));
#33206=DIRECTION('center_axis',(0.,0.,-1.));
#33207=DIRECTION('ref_axis',(0.707081539571582,-0.707132021900495,0.));
#33208=DIRECTION('',(0.,0.,1.));
#33209=DIRECTION('center_axis',(0.707081539571582,-0.707132021900494,0.));
#33210=DIRECTION('ref_axis',(0.707132021900494,0.707081539571582,0.));
#33211=DIRECTION('',(0.,0.,1.));
#33212=DIRECTION('',(0.707132021900494,0.707081539571582,0.));
#33213=DIRECTION('center_axis',(0.707081539571582,-0.707132021900494,0.));
#33214=DIRECTION('ref_axis',(0.707132021900494,0.707081539571582,0.));
#33215=DIRECTION('',(0.707132021900494,0.707081539571582,0.));
#33216=DIRECTION('',(0.,0.,1.));
#33217=DIRECTION('center_axis',(0.707081539571582,-0.707132021900494,0.));
#33218=DIRECTION('ref_axis',(0.707132021900494,0.707081539571582,0.));
#33219=DIRECTION('',(0.,0.,1.));
#33220=DIRECTION('center_axis',(0.,0.,-1.));
#33221=DIRECTION('ref_axis',(3.56963971074767E-5,0.999999999362884,0.));
#33222=DIRECTION('',(0.,0.,1.));
#33223=DIRECTION('center_axis',(0.,0.,-1.));
#33224=DIRECTION('ref_axis',(3.56963971074767E-5,0.999999999362884,0.));
#33225=DIRECTION('center_axis',(0.,0.,-1.));
#33226=DIRECTION('ref_axis',(3.56963971074767E-5,0.999999999362884,0.));
#33227=DIRECTION('center_axis',(0.,0.,1.));
#33228=DIRECTION('ref_axis',(3.56963971074767E-5,0.999999999362884,0.));
#33229=DIRECTION('',(0.,0.,1.));
#33230=DIRECTION('center_axis',(0.,0.,-1.));
#33231=DIRECTION('ref_axis',(3.56963971074767E-5,0.999999999362884,0.));
#33232=DIRECTION('',(0.,0.,1.));
#33233=DIRECTION('center_axis',(3.56963971088917E-5,0.999999999362884,0.));
#33234=DIRECTION('ref_axis',(-0.999999999362884,3.56963971088917E-5,0.));
#33235=DIRECTION('',(0.,0.,1.));
#33236=DIRECTION('',(-0.999999999362884,3.56963971088917E-5,0.));
#33237=DIRECTION('center_axis',(3.56963971088917E-5,0.999999999362884,0.));
#33238=DIRECTION('ref_axis',(-0.999999999362884,3.56963971088917E-5,0.));
#33239=DIRECTION('',(-0.999999999362884,3.56963971088917E-5,0.));
#33240=DIRECTION('',(0.,0.,1.));
#33241=DIRECTION('center_axis',(3.56963971088917E-5,0.999999999362884,0.));
#33242=DIRECTION('ref_axis',(-0.999999999362884,3.56963971088917E-5,0.));
#33243=DIRECTION('',(0.,0.,1.));
#33244=DIRECTION('center_axis',(0.,0.,1.));
#33245=DIRECTION('ref_axis',(-1.,0.,0.));
#33246=DIRECTION('',(0.,0.,1.));
#33247=DIRECTION('',(0.,0.,1.));
#33248=DIRECTION('',(0.,0.,1.));
#33249=DIRECTION('center_axis',(0.,0.,1.));
#33250=DIRECTION('ref_axis',(-1.,0.,0.));
#33251=DIRECTION('',(0.,0.,1.));
#33252=DIRECTION('center_axis',(0.,0.,1.));
#33253=DIRECTION('ref_axis',(-1.,0.,0.));
#33254=DIRECTION('',(0.,0.,1.));
#33255=DIRECTION('center_axis',(0.,-1.,0.));
#33256=DIRECTION('ref_axis',(1.,0.,0.));
#33257=DIRECTION('',(0.,0.,1.));
#33258=DIRECTION('',(1.,0.,0.));
#33259=DIRECTION('center_axis',(0.,-1.,0.));
#33260=DIRECTION('ref_axis',(1.,0.,0.));
#33261=DIRECTION('',(0.,0.,1.));
#33262=DIRECTION('center_axis',(0.,-1.,0.));
#33263=DIRECTION('ref_axis',(1.,0.,0.));
#33264=DIRECTION('',(0.,0.,1.));
#33265=DIRECTION('center_axis',(0.,0.,1.));
#33266=DIRECTION('ref_axis',(1.,0.,0.));
#33267=DIRECTION('',(0.,0.,1.));
#33268=DIRECTION('center_axis',(0.,0.,-1.));
#33269=DIRECTION('ref_axis',(1.,0.,0.));
#33270=DIRECTION('center_axis',(0.,0.,1.));
#33271=DIRECTION('ref_axis',(1.,0.,0.));
#33272=DIRECTION('',(0.,0.,1.));
#33273=DIRECTION('center_axis',(0.,0.,1.));
#33274=DIRECTION('ref_axis',(1.,0.,0.));
#33275=DIRECTION('',(0.,0.,1.));
#33276=DIRECTION('center_axis',(-1.,0.,0.));
#33277=DIRECTION('ref_axis',(0.,-1.,0.));
#33278=DIRECTION('',(0.,0.,1.));
#33279=DIRECTION('',(0.,-1.,0.));
#33280=DIRECTION('center_axis',(-1.,0.,0.));
#33281=DIRECTION('ref_axis',(0.,-1.,0.));
#33282=DIRECTION('',(0.,0.,1.));
#33283=DIRECTION('center_axis',(-1.,0.,0.));
#33284=DIRECTION('ref_axis',(0.,-1.,0.));
#33285=DIRECTION('',(0.,0.,1.));
#33286=DIRECTION('center_axis',(0.,0.,1.));
#33287=DIRECTION('ref_axis',(0.70710678118655,-0.707106781186545,0.));
#33288=DIRECTION('',(0.,0.,1.));
#33289=DIRECTION('center_axis',(0.,0.,-1.));
#33290=DIRECTION('ref_axis',(0.70710678118655,-0.707106781186545,0.));
#33291=DIRECTION('center_axis',(0.,0.,1.));
#33292=DIRECTION('ref_axis',(0.70710678118655,-0.707106781186545,0.));
#33293=DIRECTION('',(0.,0.,1.));
#33294=DIRECTION('center_axis',(0.,0.,1.));
#33295=DIRECTION('ref_axis',(0.70710678118655,-0.707106781186545,0.));
#33296=DIRECTION('',(0.,0.,1.));
#33297=DIRECTION('center_axis',(-0.707106781186549,0.707106781186546,0.));
#33298=DIRECTION('ref_axis',(-0.707106781186546,-0.707106781186549,0.));
#33299=DIRECTION('',(0.,0.,1.));
#33300=DIRECTION('',(-0.707106781186546,-0.707106781186549,0.));
#33301=DIRECTION('center_axis',(-0.707106781186549,0.707106781186546,0.));
#33302=DIRECTION('ref_axis',(-0.707106781186546,-0.707106781186549,0.));
#33303=DIRECTION('',(0.,0.,1.));
#33304=DIRECTION('center_axis',(-0.707106781186549,0.707106781186546,0.));
#33305=DIRECTION('ref_axis',(-0.707106781186546,-0.707106781186549,0.));
#33306=DIRECTION('',(0.,0.,1.));
#33307=DIRECTION('center_axis',(0.,0.,1.));
#33308=DIRECTION('ref_axis',(3.33066907387547E-15,-1.,0.));
#33309=DIRECTION('',(0.,0.,1.));
#33310=DIRECTION('center_axis',(0.,0.,-1.));
#33311=DIRECTION('ref_axis',(3.33066907387547E-15,-1.,0.));
#33312=DIRECTION('center_axis',(0.,0.,1.));
#33313=DIRECTION('ref_axis',(3.33066907387547E-15,-1.,0.));
#33314=DIRECTION('',(0.,0.,1.));
#33315=DIRECTION('center_axis',(0.,0.,1.));
#33316=DIRECTION('ref_axis',(3.33066907387547E-15,-1.,0.));
#33317=DIRECTION('',(0.,0.,1.));
#33318=DIRECTION('center_axis',(-4.22740799476499E-15,1.,0.));
#33319=DIRECTION('ref_axis',(-1.,-4.22740799476499E-15,0.));
#33320=DIRECTION('',(0.,0.,1.));
#33321=DIRECTION('',(-1.,-4.22740799476499E-15,0.));
#33322=DIRECTION('center_axis',(-4.22740799476499E-15,1.,0.));
#33323=DIRECTION('ref_axis',(-1.,-4.22740799476499E-15,0.));
#33324=DIRECTION('',(0.,0.,1.));
#33325=DIRECTION('center_axis',(-4.22740799476499E-15,1.,0.));
#33326=DIRECTION('ref_axis',(-1.,-4.22740799476499E-15,0.));
#33327=DIRECTION('',(0.,0.,1.));
#33328=DIRECTION('center_axis',(0.,0.,1.));
#33329=DIRECTION('ref_axis',(-0.707106781186545,-0.70710678118655,0.));
#33330=DIRECTION('',(0.,0.,1.));
#33331=DIRECTION('center_axis',(0.,0.,-1.));
#33332=DIRECTION('ref_axis',(-0.707106781186545,-0.70710678118655,0.));
#33333=DIRECTION('center_axis',(0.,0.,1.));
#33334=DIRECTION('ref_axis',(-0.707106781186545,-0.70710678118655,0.));
#33335=DIRECTION('',(0.,0.,1.));
#33336=DIRECTION('center_axis',(0.,0.,1.));
#33337=DIRECTION('ref_axis',(-0.707106781186545,-0.70710678118655,0.));
#33338=DIRECTION('',(0.,0.,1.));
#33339=DIRECTION('center_axis',(0.707106781186546,0.707106781186549,0.));
#33340=DIRECTION('ref_axis',(-0.707106781186549,0.707106781186546,0.));
#33341=DIRECTION('',(0.,0.,1.));
#33342=DIRECTION('',(-0.707106781186549,0.707106781186546,0.));
#33343=DIRECTION('center_axis',(0.707106781186546,0.707106781186549,0.));
#33344=DIRECTION('ref_axis',(-0.707106781186549,0.707106781186546,0.));
#33345=DIRECTION('',(0.,0.,1.));
#33346=DIRECTION('center_axis',(0.707106781186546,0.707106781186549,0.));
#33347=DIRECTION('ref_axis',(-0.707106781186549,0.707106781186546,0.));
#33348=DIRECTION('',(0.,0.,1.));
#33349=DIRECTION('center_axis',(0.,0.,1.));
#33350=DIRECTION('ref_axis',(-6.2450045135165E-15,1.,0.));
#33351=DIRECTION('',(0.,0.,1.));
#33352=DIRECTION('center_axis',(0.,0.,-1.));
#33353=DIRECTION('ref_axis',(-6.2450045135165E-15,1.,0.));
#33354=DIRECTION('center_axis',(0.,0.,1.));
#33355=DIRECTION('ref_axis',(-6.2450045135165E-15,1.,0.));
#33356=DIRECTION('',(0.,0.,1.));
#33357=DIRECTION('center_axis',(0.,0.,1.));
#33358=DIRECTION('ref_axis',(-6.2450045135165E-15,1.,0.));
#33359=DIRECTION('',(0.,0.,1.));
#33360=DIRECTION('center_axis',(7.6600122440718E-15,-1.,0.));
#33361=DIRECTION('ref_axis',(1.,7.6600122440718E-15,0.));
#33362=DIRECTION('',(0.,0.,1.));
#33363=DIRECTION('',(1.,7.6600122440718E-15,0.));
#33364=DIRECTION('center_axis',(7.6600122440718E-15,-1.,0.));
#33365=DIRECTION('ref_axis',(1.,7.6600122440718E-15,0.));
#33366=DIRECTION('',(0.,0.,1.));
#33367=DIRECTION('center_axis',(7.6600122440718E-15,-1.,0.));
#33368=DIRECTION('ref_axis',(1.,7.6600122440718E-15,0.));
#33369=DIRECTION('',(0.,0.,1.));
#33370=DIRECTION('center_axis',(0.999999999362884,-3.56963971013892E-5,
0.));
#33371=DIRECTION('ref_axis',(0.,0.,1.));
#33372=DIRECTION('center_axis',(0.999999999362884,-3.56963971012317E-5,
0.));
#33373=DIRECTION('ref_axis',(0.,0.,1.));
#33374=DIRECTION('',(0.999999999362884,-3.56963971013892E-5,0.));
#33375=DIRECTION('center_axis',(-0.999999999362884,3.56963971012317E-5,
0.));
#33376=DIRECTION('ref_axis',(0.,0.,1.));
#33377=DIRECTION('center_axis',(0.999999999362884,-3.56963971013892E-5,
0.));
#33378=DIRECTION('ref_axis',(0.,0.,1.));
#33379=DIRECTION('center_axis',(0.999999999362884,-3.56963971012317E-5,
0.));
#33380=DIRECTION('ref_axis',(0.,0.,1.));
#33381=DIRECTION('',(0.999999999362884,-3.56963971013892E-5,0.));
#33382=DIRECTION('center_axis',(-0.999999999362884,3.56963971012317E-5,
0.));
#33383=DIRECTION('ref_axis',(0.,0.,1.));
#33384=DIRECTION('center_axis',(0.999999999362884,-3.56963971013892E-5,
0.));
#33385=DIRECTION('ref_axis',(0.,0.,1.));
#33386=DIRECTION('center_axis',(0.999999999362884,-3.56963971012317E-5,
0.));
#33387=DIRECTION('ref_axis',(0.,0.,1.));
#33388=DIRECTION('',(0.999999999362884,-3.56963971013892E-5,0.));
#33389=DIRECTION('center_axis',(-0.999999999362884,3.56963971012317E-5,
0.));
#33390=DIRECTION('ref_axis',(0.,0.,1.));
#33391=DIRECTION('center_axis',(3.56963971012317E-5,0.999999999362884,0.));
#33392=DIRECTION('ref_axis',(-0.999999999362884,3.56963971012317E-5,0.));
#33393=DIRECTION('',(0.999999999362884,-3.56963971012317E-5,0.));
#33394=DIRECTION('',(0.,0.,1.));
#33395=DIRECTION('',(-0.999999999362884,3.56963971012317E-5,0.));
#33396=DIRECTION('',(0.,0.,1.));
#33397=DIRECTION('center_axis',(-3.56963971012317E-5,-0.999999999362884,
0.));
#33398=DIRECTION('ref_axis',(0.999999999362884,-3.56963971012317E-5,0.));
#33399=DIRECTION('',(0.999999999362884,-3.56963971012317E-5,0.));
#33400=DIRECTION('',(0.,0.,1.));
#33401=DIRECTION('',(0.999999999362884,-3.56963971012317E-5,0.));
#33402=DIRECTION('center_axis',(0.,0.,-1.));
#33403=DIRECTION('ref_axis',(-0.999999999362884,3.56963971012317E-5,0.));
#33404=DIRECTION('center_axis',(0.,0.,-1.));
#33405=DIRECTION('ref_axis',(-0.999999999362884,3.56963971012317E-5,0.));
#33406=DIRECTION('',(0.,0.,1.));
#33407=DIRECTION('center_axis',(0.,0.,-1.));
#33408=DIRECTION('ref_axis',(-0.999999999362884,3.56963971012317E-5,0.));
#33409=DIRECTION('center_axis',(0.999999999362884,-3.56963971012317E-5,
0.));
#33410=DIRECTION('ref_axis',(3.56963971012317E-5,0.999999999362884,0.));
#33411=DIRECTION('',(3.56963971012317E-5,0.999999999362884,0.));
#33412=DIRECTION('',(0.,0.,1.));
#33413=DIRECTION('',(3.56963971012317E-5,0.999999999362884,0.));
#33414=DIRECTION('center_axis',(0.,0.,-1.));
#33415=DIRECTION('ref_axis',(-3.56963971086332E-5,-0.999999999362884,0.));
#33416=DIRECTION('',(0.,0.,1.));
#33417=DIRECTION('center_axis',(0.,0.,-1.));
#33418=DIRECTION('ref_axis',(-3.56963971086332E-5,-0.999999999362884,0.));
#33419=DIRECTION('center_axis',(0.,0.,-1.));
#33420=DIRECTION('ref_axis',(-3.56963971086332E-5,-0.999999999362884,0.));
#33421=DIRECTION('center_axis',(3.56963971088917E-5,0.999999999362884,0.));
#33422=DIRECTION('ref_axis',(-0.999999999362884,3.56963971088917E-5,0.));
#33423=DIRECTION('',(0.,0.,1.));
#33424=DIRECTION('center_axis',(0.,0.,-1.));
#33425=DIRECTION('ref_axis',(3.56963971074767E-5,0.999999999362884,0.));
#33426=DIRECTION('',(0.,0.,1.));
#33427=DIRECTION('center_axis',(0.707081539571582,-0.707132021900494,0.));
#33428=DIRECTION('ref_axis',(0.707132021900494,0.707081539571582,0.));
#33429=DIRECTION('',(0.,0.,1.));
#33430=DIRECTION('center_axis',(0.,0.,-1.));
#33431=DIRECTION('ref_axis',(0.707081539571582,-0.707132021900495,0.));
#33432=DIRECTION('',(0.,0.,1.));
#33433=DIRECTION('center_axis',(-3.56963971054591E-5,-0.999999999362884,
0.));
#33434=DIRECTION('ref_axis',(0.999999999362884,-3.56963971054591E-5,0.));
#33435=DIRECTION('',(0.,0.,1.));
#33436=DIRECTION('center_axis',(0.,0.,-1.));
#33437=DIRECTION('ref_axis',(-3.56963971045624E-5,-0.999999999362884,0.));
#33438=DIRECTION('',(0.,0.,1.));
#33439=DIRECTION('center_axis',(-0.707132021900494,-0.707081539571582,0.));
#33440=DIRECTION('ref_axis',(0.707081539571582,-0.707132021900494,0.));
#33441=DIRECTION('',(0.,0.,1.));
#33442=DIRECTION('center_axis',(0.,0.,-1.));
#33443=DIRECTION('ref_axis',(-0.707132021900495,-0.707081539571582,0.));
#33444=DIRECTION('',(0.,0.,1.));
#33445=DIRECTION('center_axis',(-0.999999999362884,3.56963971012317E-5,
0.));
#33446=DIRECTION('ref_axis',(-3.56963971012317E-5,-0.999999999362884,0.));
#33447=DIRECTION('',(0.,0.,1.));
#33448=DIRECTION('center_axis',(0.,0.,-1.));
#33449=DIRECTION('ref_axis',(-0.999999999362884,3.56963971012317E-5,0.));
#33450=DIRECTION('',(0.,0.,1.));
#33451=DIRECTION('center_axis',(3.56963971012317E-5,0.999999999362884,0.));
#33452=DIRECTION('ref_axis',(-0.999999999362884,3.56963971012317E-5,0.));
#33453=DIRECTION('center_axis',(-0.999999999362884,3.56963971012317E-5,
0.));
#33454=DIRECTION('ref_axis',(-3.56963971012317E-5,-0.999999999362884,0.));
#33455=DIRECTION('',(-3.56963971012317E-5,-0.999999999362884,0.));
#33456=DIRECTION('',(0.,0.,1.));
#33457=DIRECTION('',(-3.56963971012317E-5,-0.999999999362884,0.));
#33458=DIRECTION('center_axis',(0.,0.,-1.));
#33459=DIRECTION('ref_axis',(3.56963971012317E-5,0.999999999362884,0.));
#33460=DIRECTION('center_axis',(0.,0.,-1.));
#33461=DIRECTION('ref_axis',(3.56963971012317E-5,0.999999999362884,0.));
#33462=DIRECTION('',(0.,0.,1.));
#33463=DIRECTION('center_axis',(0.,0.,-1.));
#33464=DIRECTION('ref_axis',(3.56963971012317E-5,0.999999999362884,0.));
#33465=DIRECTION('center_axis',(-3.56963971012317E-5,-0.999999999362884,
0.));
#33466=DIRECTION('ref_axis',(0.999999999362884,-3.56963971012317E-5,0.));
#33467=DIRECTION('',(0.999999999362884,-3.56963971012317E-5,0.));
#33468=DIRECTION('',(0.,0.,1.));
#33469=DIRECTION('',(0.999999999362884,-3.56963971012317E-5,0.));
#33470=DIRECTION('center_axis',(0.,0.,-1.));
#33471=DIRECTION('ref_axis',(-0.999999999362884,3.56963971012317E-5,0.));
#33472=DIRECTION('center_axis',(0.,0.,-1.));
#33473=DIRECTION('ref_axis',(-0.999999999362884,3.56963971012317E-5,0.));
#33474=DIRECTION('',(0.,0.,1.));
#33475=DIRECTION('center_axis',(0.,0.,-1.));
#33476=DIRECTION('ref_axis',(-0.999999999362884,3.56963971012317E-5,0.));
#33477=DIRECTION('center_axis',(0.999999999362884,-3.56963971012317E-5,
0.));
#33478=DIRECTION('ref_axis',(3.56963971012317E-5,0.999999999362884,0.));
#33479=DIRECTION('',(3.56963971012317E-5,0.999999999362884,0.));
#33480=DIRECTION('',(0.,0.,1.));
#33481=DIRECTION('',(3.56963971012317E-5,0.999999999362884,0.));
#33482=DIRECTION('center_axis',(0.,0.,-1.));
#33483=DIRECTION('ref_axis',(0.999999999362884,-3.56963971012317E-5,0.));
#33484=DIRECTION('center_axis',(0.,0.,-1.));
#33485=DIRECTION('ref_axis',(0.999999999362884,-3.56963971012317E-5,0.));
#33486=DIRECTION('',(0.,0.,1.));
#33487=DIRECTION('center_axis',(0.,0.,1.));
#33488=DIRECTION('ref_axis',(0.999999999362884,-3.56963971012317E-5,0.));
#33489=DIRECTION('center_axis',(-3.56963971012317E-5,-0.999999999362884,
0.));
#33490=DIRECTION('ref_axis',(0.999999999362884,-3.56963971012317E-5,0.));
#33491=DIRECTION('',(0.999999999362884,-3.56963971012317E-5,0.));
#33492=DIRECTION('',(0.,0.,1.));
#33493=DIRECTION('',(0.999999999362884,-3.56963971012317E-5,0.));
#33494=DIRECTION('center_axis',(0.,0.,-1.));
#33495=DIRECTION('ref_axis',(-0.707081539571584,0.707132021900492,0.));
#33496=DIRECTION('center_axis',(0.,0.,-1.));
#33497=DIRECTION('ref_axis',(-0.707081539571584,0.707132021900492,0.));
#33498=DIRECTION('',(0.,0.,1.));
#33499=DIRECTION('center_axis',(0.,0.,-1.));
#33500=DIRECTION('ref_axis',(-0.707081539571584,0.707132021900492,0.));
#33501=DIRECTION('center_axis',(0.707081539571584,-0.707132021900493,0.));
#33502=DIRECTION('ref_axis',(0.707132021900493,0.707081539571584,0.));
#33503=DIRECTION('',(0.707132021900493,0.707081539571584,0.));
#33504=DIRECTION('',(0.,0.,1.));
#33505=DIRECTION('',(0.707132021900493,0.707081539571584,0.));
#33506=DIRECTION('center_axis',(0.,0.,-1.));
#33507=DIRECTION('ref_axis',(-0.999999999362884,3.56963971012317E-5,0.));
#33508=DIRECTION('center_axis',(0.,0.,-1.));
#33509=DIRECTION('ref_axis',(-0.999999999362884,3.56963971012317E-5,0.));
#33510=DIRECTION('',(0.,0.,1.));
#33511=DIRECTION('center_axis',(0.,0.,-1.));
#33512=DIRECTION('ref_axis',(-0.999999999362884,3.56963971012317E-5,0.));
#33513=DIRECTION('center_axis',(0.999999999362884,-3.56963971012317E-5,
0.));
#33514=DIRECTION('ref_axis',(3.56963971012317E-5,0.999999999362884,0.));
#33515=DIRECTION('',(3.56963971012317E-5,0.999999999362884,0.));
#33516=DIRECTION('',(0.,0.,1.));
#33517=DIRECTION('',(3.56963971012317E-5,0.999999999362884,0.));
#33518=DIRECTION('center_axis',(0.,0.,-1.));
#33519=DIRECTION('ref_axis',(-3.56963971012317E-5,-0.999999999362884,0.));
#33520=DIRECTION('center_axis',(0.,0.,-1.));
#33521=DIRECTION('ref_axis',(-3.56963971012317E-5,-0.999999999362884,0.));
#33522=DIRECTION('',(0.,0.,1.));
#33523=DIRECTION('center_axis',(0.,0.,-1.));
#33524=DIRECTION('ref_axis',(-3.56963971012317E-5,-0.999999999362884,0.));
#33525=DIRECTION('center_axis',(3.56963971012317E-5,0.999999999362884,0.));
#33526=DIRECTION('ref_axis',(-0.999999999362884,3.56963971012317E-5,0.));
#33527=DIRECTION('',(-0.999999999362884,3.56963971012317E-5,0.));
#33528=DIRECTION('',(0.,0.,1.));
#33529=DIRECTION('',(-0.999999999362884,3.56963971012317E-5,0.));
#33530=DIRECTION('center_axis',(-0.707081539571583,0.707132021900493,0.));
#33531=DIRECTION('ref_axis',(-0.707132021900493,-0.707081539571583,0.));
#33532=DIRECTION('',(-0.707132021900493,-0.707081539571583,0.));
#33533=DIRECTION('',(0.,0.,1.));
#33534=DIRECTION('',(-0.707132021900493,-0.707081539571583,0.));
#33535=DIRECTION('center_axis',(-0.999999999362884,3.56963971012317E-5,
0.));
#33536=DIRECTION('ref_axis',(-3.56963971012317E-5,-0.999999999362884,0.));
#33537=DIRECTION('',(-3.56963971012317E-5,-0.999999999362884,0.));
#33538=DIRECTION('',(0.,0.,1.));
#33539=DIRECTION('',(-3.56963971012317E-5,-0.999999999362884,0.));
#33540=DIRECTION('center_axis',(0.,0.,-1.));
#33541=DIRECTION('ref_axis',(-0.999999999362884,3.56963971012317E-5,0.));
#33542=DIRECTION('center_axis',(0.,0.,-1.));
#33543=DIRECTION('ref_axis',(-0.999999999362884,3.56963971012317E-5,0.));
#33544=DIRECTION('',(0.,0.,1.));
#33545=DIRECTION('center_axis',(0.,0.,1.));
#33546=DIRECTION('ref_axis',(-0.999999999362884,3.56963971012317E-5,0.));
#33547=DIRECTION('center_axis',(-0.469440044438888,0.88296435073972,0.));
#33548=DIRECTION('ref_axis',(-0.88296435073972,-0.469440044438888,0.));
#33549=DIRECTION('',(-0.88296435073972,-0.469440044438887,0.));
#33550=DIRECTION('',(0.,0.,1.));
#33551=DIRECTION('',(-0.88296435073972,-0.469440044438887,0.));
#33552=DIRECTION('center_axis',(3.56963971012317E-5,0.999999999362884,0.));
#33553=DIRECTION('ref_axis',(-0.999999999362884,3.56963971012317E-5,0.));
#33554=DIRECTION('',(-0.999999999362884,3.56963971012317E-5,0.));
#33555=DIRECTION('',(0.,0.,1.));
#33556=DIRECTION('',(-0.999999999362884,3.56963971012317E-5,0.));
#33557=DIRECTION('center_axis',(-0.999999999362884,3.56963971012317E-5,
0.));
#33558=DIRECTION('ref_axis',(-3.56963971012317E-5,-0.999999999362884,0.));
#33559=DIRECTION('',(-3.56963971012317E-5,-0.999999999362884,0.));
#33560=DIRECTION('',(-3.56963971012317E-5,-0.999999999362884,0.));
#33561=DIRECTION('center_axis',(0.,-1.,0.));
#33562=DIRECTION('ref_axis',(1.,0.,0.));
#33563=DIRECTION('',(-1.,0.,0.));
#33564=DIRECTION('',(0.,0.,1.));
#33565=DIRECTION('',(1.,0.,0.));
#33566=DIRECTION('center_axis',(0.,0.,1.));
#33567=DIRECTION('ref_axis',(1.,0.,0.));
#33568=DIRECTION('center_axis',(0.,0.,1.));
#33569=DIRECTION('ref_axis',(1.,0.,0.));
#33570=DIRECTION('center_axis',(0.,0.,1.));
#33571=DIRECTION('ref_axis',(1.,0.,0.));
#33572=DIRECTION('',(0.,0.,1.));
#33573=DIRECTION('center_axis',(1.,0.,0.));
#33574=DIRECTION('ref_axis',(0.,1.,0.));
#33575=DIRECTION('',(0.,1.,0.));
#33576=DIRECTION('',(0.,1.,0.));
#33577=DIRECTION('',(0.,0.,1.));
#33578=DIRECTION('center_axis',(0.,0.,1.));
#33579=DIRECTION('ref_axis',(7.40148683083432E-15,-1.,0.));
#33580=DIRECTION('',(0.,0.,1.));
#33581=DIRECTION('center_axis',(0.,0.,1.));
#33582=DIRECTION('ref_axis',(7.40148683083432E-15,-1.,0.));
#33583=DIRECTION('center_axis',(0.,0.,1.));
#33584=DIRECTION('ref_axis',(7.40148683083432E-15,-1.,0.));
#33585=DIRECTION('center_axis',(7.6600122440718E-15,-1.,0.));
#33586=DIRECTION('ref_axis',(1.,7.6600122440718E-15,0.));
#33587=DIRECTION('',(0.,0.,1.));
#33588=DIRECTION('',(1.,7.6600122440718E-15,0.));
#33589=DIRECTION('center_axis',(0.,0.,1.));
#33590=DIRECTION('ref_axis',(-6.2450045135165E-15,1.,0.));
#33591=DIRECTION('',(0.,0.,1.));
#33592=DIRECTION('center_axis',(0.,0.,1.));
#33593=DIRECTION('ref_axis',(-6.2450045135165E-15,1.,0.));
#33594=DIRECTION('center_axis',(0.707106781186546,0.707106781186549,0.));
#33595=DIRECTION('ref_axis',(-0.707106781186549,0.707106781186546,0.));
#33596=DIRECTION('',(0.,0.,1.));
#33597=DIRECTION('',(-0.707106781186549,0.707106781186546,0.));
#33598=DIRECTION('center_axis',(0.,0.,1.));
#33599=DIRECTION('ref_axis',(-0.707106781186545,-0.70710678118655,0.));
#33600=DIRECTION('',(0.,0.,1.));
#33601=DIRECTION('center_axis',(0.,0.,1.));
#33602=DIRECTION('ref_axis',(-0.707106781186545,-0.70710678118655,0.));
#33603=DIRECTION('center_axis',(-4.22740799476499E-15,1.,0.));
#33604=DIRECTION('ref_axis',(-1.,-4.22740799476499E-15,0.));
#33605=DIRECTION('',(0.,0.,1.));
#33606=DIRECTION('',(-1.,-4.22740799476499E-15,0.));
#33607=DIRECTION('center_axis',(0.,0.,1.));
#33608=DIRECTION('ref_axis',(3.33066907387547E-15,-1.,0.));
#33609=DIRECTION('',(0.,0.,1.));
#33610=DIRECTION('center_axis',(0.,0.,1.));
#33611=DIRECTION('ref_axis',(3.33066907387547E-15,-1.,0.));
#33612=DIRECTION('center_axis',(-0.707106781186549,0.707106781186546,0.));
#33613=DIRECTION('ref_axis',(-0.707106781186546,-0.707106781186549,0.));
#33614=DIRECTION('',(0.,0.,1.));
#33615=DIRECTION('',(-0.707106781186546,-0.707106781186549,0.));
#33616=DIRECTION('center_axis',(0.,0.,1.));
#33617=DIRECTION('ref_axis',(0.70710678118655,-0.707106781186545,0.));
#33618=DIRECTION('',(0.,0.,1.));
#33619=DIRECTION('center_axis',(0.,0.,1.));
#33620=DIRECTION('ref_axis',(0.70710678118655,-0.707106781186545,0.));
#33621=DIRECTION('center_axis',(-1.,0.,0.));
#33622=DIRECTION('ref_axis',(0.,-1.,0.));
#33623=DIRECTION('',(0.,0.,1.));
#33624=DIRECTION('',(0.,-1.,0.));
#33625=DIRECTION('center_axis',(0.,0.,1.));
#33626=DIRECTION('ref_axis',(1.,0.,0.));
#33627=DIRECTION('',(0.,0.,1.));
#33628=DIRECTION('center_axis',(0.,0.,1.));
#33629=DIRECTION('ref_axis',(1.,0.,0.));
#33630=DIRECTION('center_axis',(0.,-1.,0.));
#33631=DIRECTION('ref_axis',(1.,0.,0.));
#33632=DIRECTION('',(1.,0.,0.));
#33633=DIRECTION('center_axis',(-1.,0.,0.));
#33634=DIRECTION('ref_axis',(0.,-1.,0.));
#33635=DIRECTION('',(0.,-1.,0.));
#33636=DIRECTION('',(0.,-1.,0.));
#33637=DIRECTION('',(0.,0.,1.));
#33638=DIRECTION('center_axis',(0.,0.,1.));
#33639=DIRECTION('ref_axis',(0.,1.,0.));
#33640=DIRECTION('center_axis',(0.,0.,1.));
#33641=DIRECTION('ref_axis',(0.,1.,0.));
#33642=DIRECTION('center_axis',(0.,0.,1.));
#33643=DIRECTION('ref_axis',(0.,1.,0.));
#33644=DIRECTION('',(0.,0.,1.));
#33645=DIRECTION('center_axis',(0.,1.,0.));
#33646=DIRECTION('ref_axis',(-1.,0.,0.));
#33647=DIRECTION('',(-1.,0.,0.));
#33648=DIRECTION('',(-1.,0.,0.));
#33649=DIRECTION('',(0.,0.,1.));
#33650=DIRECTION('center_axis',(0.,0.,1.));
#33651=DIRECTION('ref_axis',(1.,0.,0.));
#33652=DIRECTION('center_axis',(0.,0.,1.));
#33653=DIRECTION('ref_axis',(1.,0.,0.));
#33654=DIRECTION('center_axis',(0.,0.,1.));
#33655=DIRECTION('ref_axis',(1.,0.,0.));
#33656=DIRECTION('',(0.,0.,1.));
#33657=DIRECTION('center_axis',(1.,0.,0.));
#33658=DIRECTION('ref_axis',(0.,1.,0.));
#33659=DIRECTION('',(0.,1.,0.));
#33660=DIRECTION('',(0.,1.,0.));
#33661=DIRECTION('',(0.,0.,1.));
#33662=DIRECTION('center_axis',(0.,0.,1.));
#33663=DIRECTION('ref_axis',(-1.,0.,0.));
#33664=DIRECTION('center_axis',(0.,0.,1.));
#33665=DIRECTION('ref_axis',(-1.,0.,0.));
#33666=DIRECTION('center_axis',(0.,0.,-1.));
#33667=DIRECTION('ref_axis',(-1.,0.,0.));
#33668=DIRECTION('',(0.,0.,1.));
#33669=DIRECTION('center_axis',(0.,1.,0.));
#33670=DIRECTION('ref_axis',(-1.,0.,0.));
#33671=DIRECTION('',(-1.,0.,0.));
#33672=DIRECTION('',(-1.,0.,0.));
#33673=DIRECTION('',(0.,0.,1.));
#33674=DIRECTION('center_axis',(0.,0.,1.));
#33675=DIRECTION('ref_axis',(0.707106781186548,0.707106781186547,0.));
#33676=DIRECTION('center_axis',(0.,0.,1.));
#33677=DIRECTION('ref_axis',(0.707106781186548,0.707106781186547,0.));
#33678=DIRECTION('center_axis',(0.,0.,1.));
#33679=DIRECTION('ref_axis',(0.707106781186548,0.707106781186547,0.));
#33680=DIRECTION('',(0.,0.,1.));
#33681=DIRECTION('center_axis',(0.707106781186547,0.707106781186548,0.));
#33682=DIRECTION('ref_axis',(-0.707106781186548,0.707106781186547,0.));
#33683=DIRECTION('',(-0.707106781186548,0.707106781186547,0.));
#33684=DIRECTION('',(-0.707106781186548,0.707106781186547,0.));
#33685=DIRECTION('',(0.,0.,1.));
#33686=DIRECTION('center_axis',(0.,0.,1.));
#33687=DIRECTION('ref_axis',(1.,0.,0.));
#33688=DIRECTION('center_axis',(0.,0.,1.));
#33689=DIRECTION('ref_axis',(1.,0.,0.));
#33690=DIRECTION('center_axis',(0.,0.,1.));
#33691=DIRECTION('ref_axis',(1.,0.,0.));
#33692=DIRECTION('',(0.,0.,1.));
#33693=DIRECTION('center_axis',(1.,0.,0.));
#33694=DIRECTION('ref_axis',(0.,1.,0.));
#33695=DIRECTION('',(0.,1.,0.));
#33696=DIRECTION('',(0.,1.,0.));
#33697=DIRECTION('',(0.,0.,1.));
#33698=DIRECTION('center_axis',(0.,0.,1.));
#33699=DIRECTION('ref_axis',(0.,-1.,0.));
#33700=DIRECTION('center_axis',(0.,0.,1.));
#33701=DIRECTION('ref_axis',(0.,-1.,0.));
#33702=DIRECTION('center_axis',(0.,0.,1.));
#33703=DIRECTION('ref_axis',(0.,-1.,0.));
#33704=DIRECTION('',(0.,0.,1.));
#33705=DIRECTION('center_axis',(0.,-1.,0.));
#33706=DIRECTION('ref_axis',(1.,0.,0.));
#33707=DIRECTION('',(1.,0.,0.));
#33708=DIRECTION('',(1.,0.,0.));
#33709=DIRECTION('',(0.,0.,1.));
#33710=DIRECTION('center_axis',(-0.707106781186547,-0.707106781186548,0.));
#33711=DIRECTION('ref_axis',(0.707106781186548,-0.707106781186547,0.));
#33712=DIRECTION('',(0.707106781186548,-0.707106781186547,0.));
#33713=DIRECTION('',(0.707106781186548,-0.707106781186547,0.));
#33714=DIRECTION('',(0.,0.,1.));
#33715=DIRECTION('center_axis',(-1.,0.,0.));
#33716=DIRECTION('ref_axis',(0.,-1.,0.));
#33717=DIRECTION('',(0.,-1.,0.));
#33718=DIRECTION('',(0.,-1.,0.));
#33719=DIRECTION('',(0.,0.,1.));
#33720=DIRECTION('center_axis',(0.,0.,1.));
#33721=DIRECTION('ref_axis',(1.,0.,0.));
#33722=DIRECTION('center_axis',(0.,0.,1.));
#33723=DIRECTION('ref_axis',(1.,0.,0.));
#33724=DIRECTION('center_axis',(0.,0.,-1.));
#33725=DIRECTION('ref_axis',(1.,0.,0.));
#33726=DIRECTION('',(0.,0.,1.));
#33727=DIRECTION('center_axis',(-0.46947156278589,-0.882947592858928,0.));
#33728=DIRECTION('ref_axis',(0.882947592858928,-0.46947156278589,0.));
#33729=DIRECTION('',(0.882947592858928,-0.46947156278589,0.));
#33730=DIRECTION('',(0.882947592858928,-0.46947156278589,0.));
#33731=DIRECTION('',(0.,0.,1.));
#33732=DIRECTION('center_axis',(0.,-1.,0.));
#33733=DIRECTION('ref_axis',(1.,0.,0.));
#33734=DIRECTION('',(1.,0.,0.));
#33735=DIRECTION('',(1.,0.,0.));
#33736=DIRECTION('',(0.,0.,1.));
#33737=DIRECTION('center_axis',(-1.,0.,0.));
#33738=DIRECTION('ref_axis',(0.,-1.,0.));
#33739=DIRECTION('',(0.,-1.,0.));
#33740=DIRECTION('',(0.,-1.,0.));
#33741=DIRECTION('center_axis',(0.,0.,1.));
#33742=DIRECTION('ref_axis',(1.,0.,0.));
#33743=DIRECTION('center_axis',(0.,0.,1.));
#33744=DIRECTION('ref_axis',(1.,0.,0.));
#33745=DIRECTION('',(0.,0.,1.));
#33746=DIRECTION('',(1.,0.,0.));
#33747=DIRECTION('',(0.,0.,1.));
#33748=DIRECTION('',(1.,0.,0.));
#33749=DIRECTION('axis',(0.,0.,1.));
#33750=DIRECTION('refdir',(1.,0.,0.));
#33751=DIRECTION('center_axis',(0.,0.,-1.));
#33752=DIRECTION('ref_axis',(-1.,0.,0.));
#33753=DIRECTION('',(0.0182661827191965,-0.999833159366536,0.));
#33754=DIRECTION('',(1.,0.,0.));
#33755=DIRECTION('center_axis',(0.,0.,1.));
#33756=DIRECTION('ref_axis',(0.966963946635808,-0.254913173269844,0.));
#33757=DIRECTION('center_axis',(0.,0.,-1.));
#33758=DIRECTION('ref_axis',(-1.,0.,0.));
#33759=DIRECTION('',(0.,1.,0.));
#33760=DIRECTION('center_axis',(0.,0.,1.));
#33761=DIRECTION('ref_axis',(-0.406016680407563,0.913865665856215,0.));
#33762=DIRECTION('',(1.,0.,0.));
#33763=DIRECTION('center_axis',(0.,0.,-1.));
#33764=DIRECTION('ref_axis',(-1.,0.,0.));
#33765=DIRECTION('center_axis',(0.,0.,1.));
#33766=DIRECTION('ref_axis',(0.966963946635808,-0.254913173269844,0.));
#33767=DIRECTION('',(0.0182661827191965,-0.999833159366536,0.));
#33768=DIRECTION('center_axis',(1.,0.,0.));
#33769=DIRECTION('ref_axis',(0.,1.,0.));
#33770=DIRECTION('',(0.,0.,1.));
#33771=DIRECTION('',(0.,1.,0.));
#33772=DIRECTION('',(0.,0.,1.));
#33773=DIRECTION('',(0.,1.,0.));
#33774=DIRECTION('center_axis',(0.,0.,1.));
#33775=DIRECTION('ref_axis',(1.,0.,0.));
#33776=DIRECTION('center_axis',(0.,0.,-1.));
#33777=DIRECTION('ref_axis',(-0.406016680407563,0.913865665856215,0.));
#33778=DIRECTION('',(0.,-1.,0.));
#33779=DIRECTION('',(1.,0.,0.));
#33780=DIRECTION('',(-0.0182661827191965,0.999833159366536,0.));
#33781=DIRECTION('center_axis',(0.,0.,-1.));
#33782=DIRECTION('ref_axis',(0.966963946635808,-0.254913173269844,0.));
#33783=DIRECTION('center_axis',(0.,0.,1.));
#33784=DIRECTION('ref_axis',(-0.866549484750265,-0.499091164497079,0.));
#33785=DIRECTION('',(1.,0.,0.));
#33786=DIRECTION('center_axis',(0.,0.,1.));
#33787=DIRECTION('ref_axis',(0.,-1.,0.));
#33788=DIRECTION('',(0.,1.,0.));
#33789=DIRECTION('',(1.,0.,0.));
#33790=DIRECTION('',(0.,-1.,0.));
#33791=DIRECTION('center_axis',(0.,0.,1.));
#33792=DIRECTION('ref_axis',(-1.,0.,0.));
#33793=DIRECTION('',(1.,0.,0.));
#33794=DIRECTION('',(0.,-1.,0.));
#33795=DIRECTION('center_axis',(0.,0.,1.));
#33796=DIRECTION('ref_axis',(0.866549484750267,-0.499091164497075,0.));
#33797=DIRECTION('center_axis',(0.,0.,-1.));
#33798=DIRECTION('ref_axis',(0.866549484750267,-0.499091164497075,0.));
#33799=DIRECTION('center_axis',(0.,0.,1.));
#33800=DIRECTION('ref_axis',(0.866549484750267,-0.499091164497075,0.));
#33801=DIRECTION('',(0.,0.,-1.));
#33802=DIRECTION('',(0.,0.,1.));
#33803=DIRECTION('center_axis',(-1.,0.,0.));
#33804=DIRECTION('ref_axis',(0.,-1.,0.));
#33805=DIRECTION('',(0.,0.,1.));
#33806=DIRECTION('',(0.,-1.,0.));
#33807=DIRECTION('center_axis',(0.,0.,1.));
#33808=DIRECTION('ref_axis',(1.,0.,0.));
#33809=DIRECTION('',(1.,0.,0.));
#33810=DIRECTION('center_axis',(0.,0.,1.));
#33811=DIRECTION('ref_axis',(-1.,0.,0.));
#33812=DIRECTION('',(0.,-1.,0.));
#33813=DIRECTION('',(1.,0.,0.));
#33814=DIRECTION('',(0.,1.,0.));
#33815=DIRECTION('center_axis',(0.,0.,1.));
#33816=DIRECTION('ref_axis',(0.,-1.,0.));
#33817=DIRECTION('',(1.,0.,0.));
#33818=DIRECTION('center_axis',(0.,0.,1.));
#33819=DIRECTION('ref_axis',(-0.866549484750265,-0.499091164497079,0.));
#33820=DIRECTION('center_axis',(0.,0.,1.));
#33821=DIRECTION('ref_axis',(0.966963946635808,-0.254913173269844,0.));
#33822=DIRECTION('',(-1.,0.,0.));
#33823=DIRECTION('center_axis',(0.,0.,-1.));
#33824=DIRECTION('ref_axis',(0.,-1.,0.));
#33825=DIRECTION('',(0.,-1.,0.));
#33826=DIRECTION('center_axis',(0.,0.,1.));
#33827=DIRECTION('ref_axis',(0.,1.,0.));
#33828=DIRECTION('',(-1.,0.,0.));
#33829=DIRECTION('center_axis',(0.,0.,1.));
#33830=DIRECTION('ref_axis',(1.,0.,0.));
#33831=DIRECTION('',(0.,1.,0.));
#33832=DIRECTION('center_axis',(0.,0.,-1.));
#33833=DIRECTION('ref_axis',(-1.,0.,0.));
#33834=DIRECTION('',(-1.,0.,0.));
#33835=DIRECTION('center_axis',(0.,0.,1.));
#33836=DIRECTION('ref_axis',(-0.406016680407563,0.913865665856215,0.));
#33837=DIRECTION('center_axis',(0.,0.,-1.));
#33838=DIRECTION('ref_axis',(-0.866549484750265,-0.499091164497079,0.));
#33839=DIRECTION('',(0.,0.,-1.));
#33840=DIRECTION('center_axis',(0.,-1.,0.));
#33841=DIRECTION('ref_axis',(1.,0.,0.));
#33842=DIRECTION('',(0.,0.,1.));
#33843=DIRECTION('center_axis',(0.,-1.,0.));
#33844=DIRECTION('ref_axis',(1.,0.,0.));
#33845=DIRECTION('',(0.,0.,1.));
#33846=DIRECTION('',(0.,0.,1.));
#33847=DIRECTION('',(1.,0.,0.));
#33848=DIRECTION('',(-1.08845394571094E-16,0.,1.));
#33849=DIRECTION('',(-1.,0.,0.));
#33850=DIRECTION('',(-1.08845394571094E-16,0.,-1.));
#33851=DIRECTION('center_axis',(-1.,0.,0.));
#33852=DIRECTION('ref_axis',(0.,-1.,0.));
#33853=DIRECTION('',(0.,0.,1.));
#33854=DIRECTION('center_axis',(1.,0.,0.));
#33855=DIRECTION('ref_axis',(0.,1.,0.));
#33856=DIRECTION('',(0.,0.,1.));
#33857=DIRECTION('center_axis',(0.,-1.,0.));
#33858=DIRECTION('ref_axis',(1.,0.,0.));
#33859=DIRECTION('',(0.,0.,1.));
#33860=DIRECTION('center_axis',(0.,0.,1.));
#33861=DIRECTION('ref_axis',(-0.406016680407563,0.913865665856215,0.));
#33862=DIRECTION('',(0.,0.,-1.));
#33863=DIRECTION('',(0.,0.,-1.));
#33864=DIRECTION('center_axis',(0.,0.,1.));
#33865=DIRECTION('ref_axis',(0.966963946635808,-0.254913173269844,0.));
#33866=DIRECTION('',(0.,0.,1.));
#33867=DIRECTION('',(0.,0.,1.));
#33868=DIRECTION('center_axis',(0.,0.,1.));
#33869=DIRECTION('ref_axis',(-1.,0.,0.));
#33870=DIRECTION('',(0.,-1.,0.));
#33871=DIRECTION('',(-1.,0.,0.));
#33872=DIRECTION('',(0.,-1.,0.));
#33873=DIRECTION('center_axis',(-1.,0.,-1.08845394571094E-16));
#33874=DIRECTION('ref_axis',(1.08845394571094E-16,0.,-1.));
#33875=DIRECTION('',(1.08845394571094E-16,0.,-1.));
#33876=DIRECTION('',(0.,-1.,0.));
#33877=DIRECTION('center_axis',(0.,0.,-1.));
#33878=DIRECTION('ref_axis',(1.,0.,0.));
#33879=DIRECTION('',(1.,0.,0.));
#33880=DIRECTION('',(0.,-1.,0.));
#33881=DIRECTION('center_axis',(1.,0.,-1.08845394571094E-16));
#33882=DIRECTION('ref_axis',(1.08845394571094E-16,0.,1.));
#33883=DIRECTION('',(1.08845394571094E-16,0.,1.));
#33884=DIRECTION('center_axis',(0.,1.,0.));
#33885=DIRECTION('ref_axis',(0.,0.,1.));
#33886=DIRECTION('center_axis',(0.,0.,1.));
#33887=DIRECTION('ref_axis',(1.,0.,0.));
#33888=DIRECTION('',(0.,1.,0.));
#33889=DIRECTION('center_axis',(0.,0.,1.));
#33890=DIRECTION('ref_axis',(-1.,0.,0.));
#33891=DIRECTION('',(0.,-1.,0.));
#33892=DIRECTION('center_axis',(0.,0.,1.));
#33893=DIRECTION('ref_axis',(1.,0.,0.));
#33894=DIRECTION('',(-1.,0.,0.));
#33895=DIRECTION('center_axis',(0.,0.,1.));
#33896=DIRECTION('ref_axis',(1.,0.,0.));
#33897=DIRECTION('',(0.,-1.,0.));
#33898=DIRECTION('',(-1.,0.,0.));
#33899=DIRECTION('center_axis',(0.,0.,1.));
#33900=DIRECTION('ref_axis',(0.,1.,0.));
#33901=DIRECTION('',(0.,-1.,0.));
#33902=DIRECTION('center_axis',(0.,0.,1.));
#33903=DIRECTION('ref_axis',(0.,-1.,0.));
#33904=DIRECTION('center_axis',(0.,0.,-1.));
#33905=DIRECTION('ref_axis',(1.,0.,0.));
#33906=DIRECTION('',(0.,0.,1.));
#33907=DIRECTION('',(0.,0.,1.));
#33908=DIRECTION('center_axis',(1.,0.,0.));
#33909=DIRECTION('ref_axis',(0.,1.,0.));
#33910=DIRECTION('',(0.,0.,1.));
#33911=DIRECTION('center_axis',(0.,0.,-1.));
#33912=DIRECTION('ref_axis',(-1.,0.,0.));
#33913=DIRECTION('',(0.,0.,1.));
#33914=DIRECTION('center_axis',(0.,0.,-1.));
#33915=DIRECTION('ref_axis',(-1.,0.,0.));
#33916=DIRECTION('center_axis',(0.,0.,-1.));
#33917=DIRECTION('ref_axis',(0.,-1.,0.));
#33918=DIRECTION('center_axis',(0.,0.,-1.));
#33919=DIRECTION('ref_axis',(0.,-1.,0.));
#33920=DIRECTION('',(0.,0.,1.));
#33921=DIRECTION('',(0.,0.,1.));
#33922=DIRECTION('center_axis',(-1.,0.,0.));
#33923=DIRECTION('ref_axis',(0.,-1.,0.));
#33924=DIRECTION('',(0.,0.,1.));
#33925=DIRECTION('center_axis',(0.,0.,-1.));
#33926=DIRECTION('ref_axis',(0.,1.,0.));
#33927=DIRECTION('',(0.,0.,1.));
#33928=DIRECTION('center_axis',(0.,0.,-1.));
#33929=DIRECTION('ref_axis',(-1.,0.,0.));
#33930=DIRECTION('',(0.0182661827191965,-0.999833159366536,0.));
#33931=DIRECTION('center_axis',(0.,0.,1.));
#33932=DIRECTION('ref_axis',(0.966963946635808,-0.254913173269844,0.));
#33933=DIRECTION('',(1.,0.,0.));
#33934=DIRECTION('center_axis',(0.,0.,-1.));
#33935=DIRECTION('ref_axis',(-1.,0.,0.));
#33936=DIRECTION('',(0.,1.,0.));
#33937=DIRECTION('',(1.,0.,0.));
#33938=DIRECTION('center_axis',(0.,0.,1.));
#33939=DIRECTION('ref_axis',(-0.406016680407563,0.913865665856215,0.));
#33940=DIRECTION('center_axis',(0.,0.,-1.));
#33941=DIRECTION('ref_axis',(-1.,0.,0.));
#33942=DIRECTION('center_axis',(0.,0.,1.));
#33943=DIRECTION('ref_axis',(0.966963946635808,-0.254913173269844,0.));
#33944=DIRECTION('',(0.0182661827191965,-0.999833159366536,0.));
#33945=DIRECTION('center_axis',(1.,0.,0.));
#33946=DIRECTION('ref_axis',(0.,1.,0.));
#33947=DIRECTION('',(0.,0.,1.));
#33948=DIRECTION('',(0.,-1.,0.));
#33949=DIRECTION('',(0.,0.,1.));
#33950=DIRECTION('',(0.,0.,-1.));
#33951=DIRECTION('center_axis',(-1.,0.,0.));
#33952=DIRECTION('ref_axis',(0.,1.,0.));
#33953=DIRECTION('',(0.,0.,-1.));
#33954=DIRECTION('',(0.,1.,0.));
#33955=DIRECTION('',(0.,0.,-1.));
#33956=DIRECTION('',(0.,1.,0.));
#33957=DIRECTION('center_axis',(0.,0.,1.));
#33958=DIRECTION('ref_axis',(1.,0.,0.));
#33959=DIRECTION('center_axis',(0.,0.,-1.));
#33960=DIRECTION('ref_axis',(-0.406016680407563,0.913865665856215,0.));
#33961=DIRECTION('center_axis',(0.,0.,1.));
#33962=DIRECTION('ref_axis',(0.866549484750267,-0.499091164497075,0.));
#33963=DIRECTION('',(0.,-1.,0.));
#33964=DIRECTION('',(1.,0.,0.));
#33965=DIRECTION('center_axis',(0.,0.,1.));
#33966=DIRECTION('ref_axis',(-1.,0.,0.));
#33967=DIRECTION('',(0.,-1.,0.));
#33968=DIRECTION('',(1.,0.,0.));
#33969=DIRECTION('',(0.,1.,0.));
#33970=DIRECTION('center_axis',(0.,0.,1.));
#33971=DIRECTION('ref_axis',(0.,-1.,0.));
#33972=DIRECTION('',(1.,0.,0.));
#33973=DIRECTION('center_axis',(0.,0.,1.));
#33974=DIRECTION('ref_axis',(-0.866549484750265,-0.499091164497079,0.));
#33975=DIRECTION('center_axis',(0.,0.,-1.));
#33976=DIRECTION('ref_axis',(0.966963946635808,-0.254913173269844,0.));
#33977=DIRECTION('',(-0.0182661827191965,0.999833159366536,0.));
#33978=DIRECTION('',(1.,0.,0.));
#33979=DIRECTION('center_axis',(-0.999833159366536,-0.0182661827191965,
0.));
#33980=DIRECTION('ref_axis',(0.0182661827191965,-0.999833159366536,0.));
#33981=DIRECTION('',(0.,0.,-1.));
#33982=DIRECTION('',(0.,0.,1.));
#33983=DIRECTION('',(0.,0.,-1.));
#33984=DIRECTION('center_axis',(0.,0.,-1.));
#33985=DIRECTION('ref_axis',(0.866549484750267,-0.499091164497075,0.));
#33986=DIRECTION('center_axis',(0.,0.,1.));
#33987=DIRECTION('ref_axis',(0.866549484750267,-0.499091164497075,0.));
#33988=DIRECTION('',(0.,0.,-1.));
#33989=DIRECTION('',(0.,0.,1.));
#33990=DIRECTION('center_axis',(1.,0.,0.));
#33991=DIRECTION('ref_axis',(0.,-1.,0.));
#33992=DIRECTION('',(0.,-1.,0.));
#33993=DIRECTION('',(0.,0.,-1.));
#33994=DIRECTION('center_axis',(0.,0.,1.));
#33995=DIRECTION('ref_axis',(1.,0.,0.));
#33996=DIRECTION('center_axis',(0.,0.,1.));
#33997=DIRECTION('ref_axis',(-0.406016680407563,0.913865665856215,0.));
#33998=DIRECTION('',(-1.,0.,0.));
#33999=DIRECTION('center_axis',(0.,0.,-1.));
#34000=DIRECTION('ref_axis',(-1.,0.,0.));
#34001=DIRECTION('',(0.,1.,0.));
#34002=DIRECTION('center_axis',(0.,0.,1.));
#34003=DIRECTION('ref_axis',(1.,0.,0.));
#34004=DIRECTION('',(-1.,0.,0.));
#34005=DIRECTION('center_axis',(0.,0.,1.));
#34006=DIRECTION('ref_axis',(0.,1.,0.));
#34007=DIRECTION('',(0.,-1.,0.));
#34008=DIRECTION('center_axis',(0.,0.,-1.));
#34009=DIRECTION('ref_axis',(0.,-1.,0.));
#34010=DIRECTION('',(-1.,0.,0.));
#34011=DIRECTION('center_axis',(0.,0.,1.));
#34012=DIRECTION('ref_axis',(0.966963946635808,-0.254913173269844,0.));
#34013=DIRECTION('center_axis',(0.,0.,1.));
#34014=DIRECTION('ref_axis',(-0.866549484750265,-0.499091164497079,0.));
#34015=DIRECTION('',(1.,0.,0.));
#34016=DIRECTION('center_axis',(0.,0.,1.));
#34017=DIRECTION('ref_axis',(0.,-1.,0.));
#34018=DIRECTION('',(0.,1.,0.));
#34019=DIRECTION('',(1.,0.,0.));
#34020=DIRECTION('',(0.,-1.,0.));
#34021=DIRECTION('center_axis',(0.,0.,1.));
#34022=DIRECTION('ref_axis',(-1.,0.,0.));
#34023=DIRECTION('',(1.,0.,0.));
#34024=DIRECTION('center_axis',(0.,-1.,0.));
#34025=DIRECTION('ref_axis',(-1.,0.,0.));
#34026=DIRECTION('',(0.,0.,1.));
#34027=DIRECTION('',(0.,0.,-1.));
#34028=DIRECTION('',(0.,0.,1.));
#34029=DIRECTION('center_axis',(0.,0.,-1.));
#34030=DIRECTION('ref_axis',(-0.866549484750265,-0.499091164497079,0.));
#34031=DIRECTION('',(0.,0.,1.));
#34032=DIRECTION('center_axis',(0.,1.,0.));
#34033=DIRECTION('ref_axis',(1.,0.,0.));
#34034=DIRECTION('',(0.,0.,-1.));
#34035=DIRECTION('center_axis',(0.,1.,0.));
#34036=DIRECTION('ref_axis',(1.,0.,0.));
#34037=DIRECTION('',(0.,0.,-1.));
#34038=DIRECTION('',(0.,0.,-1.));
#34039=DIRECTION('',(1.,0.,0.));
#34040=DIRECTION('',(-1.08845394571094E-16,0.,1.));
#34041=DIRECTION('',(-1.,0.,0.));
#34042=DIRECTION('',(-1.08845394571094E-16,0.,-1.));
#34043=DIRECTION('center_axis',(1.,0.,0.));
#34044=DIRECTION('ref_axis',(0.,-1.,0.));
#34045=DIRECTION('',(0.,0.,-1.));
#34046=DIRECTION('center_axis',(-1.,0.,0.));
#34047=DIRECTION('ref_axis',(0.,1.,0.));
#34048=DIRECTION('',(0.,0.,-1.));
#34049=DIRECTION('center_axis',(0.,1.,0.));
#34050=DIRECTION('ref_axis',(1.,0.,0.));
#34051=DIRECTION('',(0.,0.,-1.));
#34052=DIRECTION('center_axis',(0.,0.,1.));
#34053=DIRECTION('ref_axis',(-0.406016680407563,0.913865665856215,0.));
#34054=DIRECTION('center_axis',(0.,0.,1.));
#34055=DIRECTION('ref_axis',(0.966963946635808,-0.254913173269844,0.));
#34056=DIRECTION('',(0.,0.,-1.));
#34057=DIRECTION('center_axis',(0.,0.,1.));
#34058=DIRECTION('ref_axis',(-1.,0.,0.));
#34059=DIRECTION('',(0.,-1.,0.));
#34060=DIRECTION('',(-1.,0.,0.));
#34061=DIRECTION('',(0.,-1.,0.));
#34062=DIRECTION('center_axis',(1.,0.,-1.08845394571094E-16));
#34063=DIRECTION('ref_axis',(1.08845394571094E-16,0.,1.));
#34064=DIRECTION('',(0.,-1.,0.));
#34065=DIRECTION('',(1.08845394571094E-16,0.,1.));
#34066=DIRECTION('center_axis',(0.,0.,-1.));
#34067=DIRECTION('ref_axis',(1.,0.,0.));
#34068=DIRECTION('',(0.,-1.,0.));
#34069=DIRECTION('',(1.,0.,0.));
#34070=DIRECTION('center_axis',(-1.,0.,-1.08845394571094E-16));
#34071=DIRECTION('ref_axis',(1.08845394571094E-16,0.,-1.));
#34072=DIRECTION('',(1.08845394571094E-16,0.,-1.));
#34073=DIRECTION('center_axis',(0.,-1.,0.));
#34074=DIRECTION('ref_axis',(0.,0.,-1.));
#34075=DIRECTION('center_axis',(0.,1.,0.));
#34076=DIRECTION('ref_axis',(-1.,0.,0.));
#34077=DIRECTION('center_axis',(-1.,0.,0.));
#34078=DIRECTION('ref_axis',(0.,-1.,0.));
#34079=DIRECTION('',(0.,1.,0.));
#34080=DIRECTION('',(0.,0.,-1.));
#34081=DIRECTION('center_axis',(1.,0.,0.));
#34082=DIRECTION('ref_axis',(0.,1.,0.));
#34083=DIRECTION('',(0.,-1.,0.));
#34084=DIRECTION('',(0.,0.,-1.));
#34085=DIRECTION('',(0.,0.,1.));
#34086=DIRECTION('center_axis',(0.,0.,1.));
#34087=DIRECTION('ref_axis',(1.,0.,0.));
#34088=DIRECTION('',(-1.,0.,0.));
#34089=DIRECTION('center_axis',(0.,0.,1.));
#34090=DIRECTION('ref_axis',(1.,0.,0.));
#34091=DIRECTION('',(0.,-1.,0.));
#34092=DIRECTION('center_axis',(0.,0.,1.));
#34093=DIRECTION('ref_axis',(-1.,0.,0.));
#34094=DIRECTION('center_axis',(0.,0.,1.));
#34095=DIRECTION('ref_axis',(1.,0.,0.));
#34096=DIRECTION('center_axis',(0.,0.,1.));
#34097=DIRECTION('ref_axis',(0.,-1.,0.));
#34098=DIRECTION('',(0.,-1.,0.));
#34099=DIRECTION('center_axis',(0.,0.,1.));
#34100=DIRECTION('ref_axis',(0.,1.,0.));
#34101=DIRECTION('',(-1.,0.,0.));
#34102=DIRECTION('center_axis',(0.,-1.,0.));
#34103=DIRECTION('ref_axis',(-1.,0.,0.));
#34104=DIRECTION('',(0.,0.,-1.));
#34105=DIRECTION('center_axis',(0.,-1.,0.));
#34106=DIRECTION('ref_axis',(-1.,0.,0.));
#34107=DIRECTION('',(0.,0.,-1.));
#34108=DIRECTION('',(0.,0.,-1.));
#34109=DIRECTION('center_axis',(0.,0.,-1.));
#34110=DIRECTION('ref_axis',(1.,0.,0.));
#34111=DIRECTION('',(0.,0.,-1.));
#34112=DIRECTION('center_axis',(-1.,0.,0.));
#34113=DIRECTION('ref_axis',(0.,1.,0.));
#34114=DIRECTION('',(0.,0.,-1.));
#34115=DIRECTION('center_axis',(0.,0.,-1.));
#34116=DIRECTION('ref_axis',(-1.,0.,0.));
#34117=DIRECTION('center_axis',(0.,0.,-1.));
#34118=DIRECTION('ref_axis',(-1.,0.,0.));
#34119=DIRECTION('center_axis',(0.,0.,-1.));
#34120=DIRECTION('ref_axis',(0.,-1.,0.));
#34121=DIRECTION('center_axis',(0.,0.,-1.));
#34122=DIRECTION('ref_axis',(0.,-1.,0.));
#34123=DIRECTION('',(0.,0.,-1.));
#34124=DIRECTION('center_axis',(1.,0.,0.));
#34125=DIRECTION('ref_axis',(0.,-1.,0.));
#34126=DIRECTION('',(0.,0.,-1.));
#34127=DIRECTION('center_axis',(0.,0.,-1.));
#34128=DIRECTION('ref_axis',(0.,1.,0.));
#34129=DIRECTION('axis',(0.,0.,1.));
#34130=DIRECTION('refdir',(1.,0.,0.));
#34131=DIRECTION('center_axis',(0.,0.,1.));
#34132=DIRECTION('ref_axis',(1.,0.,0.));
#34133=DIRECTION('center_axis',(0.,0.,-1.));
#34134=DIRECTION('ref_axis',(1.,0.,0.));
#34135=DIRECTION('',(0.,0.,1.));
#34136=DIRECTION('center_axis',(0.,0.,-1.));
#34137=DIRECTION('ref_axis',(1.,0.,0.));
#34138=DIRECTION('center_axis',(0.,0.,1.));
#34139=DIRECTION('ref_axis',(1.76313947997109E-5,-0.999999999844567,0.));
#34140=DIRECTION('center_axis',(0.,0.,1.));
#34141=DIRECTION('ref_axis',(1.76313947997109E-5,-0.999999999844567,0.));
#34142=DIRECTION('',(0.,0.,1.));
#34143=DIRECTION('center_axis',(0.,0.,1.));
#34144=DIRECTION('ref_axis',(1.76313947997109E-5,-0.999999999844567,0.));
#34145=DIRECTION('',(0.,0.,1.));
#34146=DIRECTION('center_axis',(0.000247476788645072,-0.999999969377619,
0.));
#34147=DIRECTION('ref_axis',(0.999999969377619,0.000247476788645072,0.));
#34148=DIRECTION('',(-0.999999969377619,-0.000247476788645072,0.));
#34149=DIRECTION('',(0.999999969377619,0.000247476788645072,0.));
#34150=DIRECTION('',(0.,0.,1.));
#34151=DIRECTION('center_axis',(-0.965913556273921,-0.258864833081411,0.));
#34152=DIRECTION('ref_axis',(0.258864833081411,-0.965913556273921,0.));
#34153=DIRECTION('',(0.258864833081411,-0.965913556273921,0.));
#34154=DIRECTION('',(0.258864833081411,-0.965913556273921,0.));
#34155=DIRECTION('',(0.,0.,1.));
#34156=DIRECTION('center_axis',(0.,-1.,0.));
#34157=DIRECTION('ref_axis',(1.,0.,0.));
#34158=DIRECTION('',(1.,0.,0.));
#34159=DIRECTION('',(1.,0.,0.));
#34160=DIRECTION('',(0.,0.,1.));
#34161=DIRECTION('center_axis',(0.965913556273921,-0.258864833081411,0.));
#34162=DIRECTION('ref_axis',(0.258864833081411,0.965913556273921,0.));
#34163=DIRECTION('',(-0.258864833081411,-0.965913556273921,0.));
#34164=DIRECTION('',(0.258864833081411,0.965913556273921,0.));
#34165=DIRECTION('',(0.,0.,1.));
#34166=DIRECTION('center_axis',(-0.000247476788645237,-0.999999969377619,
0.));
#34167=DIRECTION('ref_axis',(0.999999969377619,-0.000247476788645237,0.));
#34168=DIRECTION('',(0.999999969377619,-0.000247476788645237,0.));
#34169=DIRECTION('',(0.999999969377619,-0.000247476788645237,0.));
#34170=DIRECTION('',(0.,0.,1.));
#34171=DIRECTION('center_axis',(0.,0.,1.));
#34172=DIRECTION('ref_axis',(-0.999999999844567,1.76313947908291E-5,0.));
#34173=DIRECTION('center_axis',(0.,0.,1.));
#34174=DIRECTION('ref_axis',(-0.999999999844567,1.76313947908291E-5,0.));
#34175=DIRECTION('center_axis',(0.,0.,1.));
#34176=DIRECTION('ref_axis',(-0.999999999844567,1.76313947908291E-5,0.));
#34177=DIRECTION('',(0.,0.,1.));
#34178=DIRECTION('center_axis',(-0.999999999844567,1.76313948019314E-5,
0.));
#34179=DIRECTION('ref_axis',(-1.76313948019314E-5,-0.999999999844567,0.));
#34180=DIRECTION('',(1.76313948019314E-5,0.999999999844567,0.));
#34181=DIRECTION('',(-1.76313948019314E-5,-0.999999999844567,0.));
#34182=DIRECTION('',(0.,0.,1.));
#34183=DIRECTION('center_axis',(-0.707094313797817,0.707119248355463,0.));
#34184=DIRECTION('ref_axis',(-0.707119248355463,-0.707094313797817,0.));
#34185=DIRECTION('',(0.707119248355463,0.707094313797817,0.));
#34186=DIRECTION('',(-0.707119248355463,-0.707094313797817,0.));
#34187=DIRECTION('',(0.,0.,1.));
#34188=DIRECTION('center_axis',(0.,0.,1.));
#34189=DIRECTION('ref_axis',(0.586386638808598,0.81003130175738,0.));
#34190=DIRECTION('center_axis',(0.,0.,1.));
#34191=DIRECTION('ref_axis',(0.586386638808598,0.81003130175738,0.));
#34192=DIRECTION('center_axis',(0.,0.,1.));
#34193=DIRECTION('ref_axis',(0.586386638808598,0.81003130175738,0.));
#34194=DIRECTION('',(0.,0.,1.));
#34195=DIRECTION('center_axis',(0.,0.,1.));
#34196=DIRECTION('ref_axis',(0.999993170091859,0.00369591255780612,0.));
#34197=DIRECTION('center_axis',(0.,0.,1.));
#34198=DIRECTION('ref_axis',(-0.586386638808589,-0.810031301757386,0.));
#34199=DIRECTION('center_axis',(0.,0.,-1.));
#34200=DIRECTION('ref_axis',(-0.586386638808589,-0.810031301757386,0.));
#34201=DIRECTION('',(0.,0.,1.));
#34202=DIRECTION('center_axis',(0.,0.,1.));
#34203=DIRECTION('ref_axis',(-0.707119248355468,-0.707094313797812,0.));
#34204=DIRECTION('center_axis',(0.,0.,1.));
#34205=DIRECTION('ref_axis',(-0.707119248355468,-0.707094313797812,0.));
#34206=DIRECTION('center_axis',(0.,0.,1.));
#34207=DIRECTION('ref_axis',(-0.707119248355468,-0.707094313797812,0.));
#34208=DIRECTION('',(0.,0.,1.));
#34209=DIRECTION('center_axis',(-0.707119248355465,-0.707094313797815,0.));
#34210=DIRECTION('ref_axis',(0.707094313797815,-0.707119248355465,0.));
#34211=DIRECTION('',(0.707094313797815,-0.707119248355465,0.));
#34212=DIRECTION('',(0.707094313797815,-0.707119248355465,0.));
#34213=DIRECTION('',(0.,0.,1.));
#34214=DIRECTION('center_axis',(-0.999999999844567,1.76313948004511E-5,
0.));
#34215=DIRECTION('ref_axis',(-1.76313948004511E-5,-0.999999999844567,0.));
#34216=DIRECTION('',(1.76313948004511E-5,0.999999999844567,0.));
#34217=DIRECTION('',(-1.76313948004511E-5,-0.999999999844567,0.));
#34218=DIRECTION('',(0.,0.,1.));
#34219=DIRECTION('center_axis',(-0.707119248355464,-0.707094313797816,0.));
#34220=DIRECTION('ref_axis',(0.707094313797816,-0.707119248355464,0.));
#34221=DIRECTION('',(-0.707094313797816,0.707119248355464,0.));
#34222=DIRECTION('',(0.707094313797816,-0.707119248355464,0.));
#34223=DIRECTION('',(0.,0.,1.));
#34224=DIRECTION('center_axis',(0.,0.,1.));
#34225=DIRECTION('ref_axis',(0.707119248355461,0.707094313797818,0.));
#34226=DIRECTION('center_axis',(0.,0.,1.));
#34227=DIRECTION('ref_axis',(0.707119248355461,0.707094313797818,0.));
#34228=DIRECTION('center_axis',(0.,0.,-1.));
#34229=DIRECTION('ref_axis',(0.707119248355461,0.707094313797818,0.));
#34230=DIRECTION('',(0.,0.,1.));
#34231=DIRECTION('center_axis',(-1.76313948097558E-5,-0.999999999844567,
0.));
#34232=DIRECTION('ref_axis',(0.999999999844567,-1.76313948097558E-5,0.));
#34233=DIRECTION('',(-0.999999999844567,1.76313948097558E-5,0.));
#34234=DIRECTION('',(0.999999999844567,-1.76313948097558E-5,0.));
#34235=DIRECTION('',(0.,0.,1.));
#34236=DIRECTION('center_axis',(0.,0.,1.));
#34237=DIRECTION('ref_axis',(-0.999999999844567,1.76313948019314E-5,0.));
#34238=DIRECTION('center_axis',(0.,0.,1.));
#34239=DIRECTION('ref_axis',(-0.999999999844567,1.76313948019314E-5,0.));
#34240=DIRECTION('center_axis',(0.,0.,1.));
#34241=DIRECTION('ref_axis',(-0.999999999844567,1.76313948019314E-5,0.));
#34242=DIRECTION('',(0.,0.,1.));
#34243=DIRECTION('center_axis',(-0.999999999844567,1.76313947990255E-5,
0.));
#34244=DIRECTION('ref_axis',(-1.76313947990255E-5,-0.999999999844567,0.));
#34245=DIRECTION('',(1.76313947990255E-5,0.999999999844567,0.));
#34246=DIRECTION('',(-1.76313947990255E-5,-0.999999999844567,0.));
#34247=DIRECTION('',(0.,0.,1.));
#34248=DIRECTION('center_axis',(0.,0.,1.));
#34249=DIRECTION('ref_axis',(1.76313947886088E-5,0.999999999844567,0.));
#34250=DIRECTION('center_axis',(0.,0.,1.));
#34251=DIRECTION('ref_axis',(1.76313947886088E-5,0.999999999844567,0.));
#34252=DIRECTION('center_axis',(0.,0.,1.));
#34253=DIRECTION('ref_axis',(1.76313947886088E-5,0.999999999844567,0.));
#34254=DIRECTION('',(0.,0.,1.));
#34255=DIRECTION('center_axis',(1.76313947987393E-5,0.999999999844567,0.));
#34256=DIRECTION('ref_axis',(-0.999999999844567,1.76313947987393E-5,0.));
#34257=DIRECTION('',(0.999999999844567,-1.76313947987393E-5,0.));
#34258=DIRECTION('',(-0.999999999844567,1.76313947987393E-5,0.));
#34259=DIRECTION('',(0.,0.,1.));
#34260=DIRECTION('center_axis',(0.469487130310524,0.882939315283213,0.));
#34261=DIRECTION('ref_axis',(-0.882939315283213,0.469487130310524,0.));
#34262=DIRECTION('',(0.882939315283213,-0.469487130310524,0.));
#34263=DIRECTION('',(-0.882939315283213,0.469487130310524,0.));
#34264=DIRECTION('',(0.,0.,1.));
#34265=DIRECTION('center_axis',(0.999999999844567,-1.76313947965879E-5,
0.));
#34266=DIRECTION('ref_axis',(1.76313947965879E-5,0.999999999844567,0.));
#34267=DIRECTION('',(-1.76313947965879E-5,-0.999999999844567,0.));
#34268=DIRECTION('',(1.76313947965879E-5,0.999999999844567,0.));
#34269=DIRECTION('',(0.,0.,1.));
#34270=DIRECTION('center_axis',(0.,0.,1.));
#34271=DIRECTION('ref_axis',(-0.999999999844567,1.76313947986007E-5,0.));
#34272=DIRECTION('center_axis',(0.,0.,1.));
#34273=DIRECTION('ref_axis',(-0.999999999844567,1.76313947986007E-5,0.));
#34274=DIRECTION('center_axis',(0.,0.,-1.));
#34275=DIRECTION('ref_axis',(-0.999999999844567,1.76313947986007E-5,0.));
#34276=DIRECTION('',(0.,0.,1.));
#34277=DIRECTION('center_axis',(-0.707100547519659,0.707113014798482,0.));
#34278=DIRECTION('ref_axis',(-0.707113014798482,-0.707100547519659,0.));
#34279=DIRECTION('',(0.707113014798482,0.707100547519659,0.));
#34280=DIRECTION('',(-0.707113014798482,-0.707100547519659,0.));
#34281=DIRECTION('',(0.,0.,1.));
#34282=DIRECTION('center_axis',(0.,0.,1.));
#34283=DIRECTION('ref_axis',(0.707100547519658,-0.707113014798483,0.));
#34284=DIRECTION('center_axis',(0.,0.,1.));
#34285=DIRECTION('ref_axis',(0.707100547519658,-0.707113014798483,0.));
#34286=DIRECTION('center_axis',(0.,0.,-1.));
#34287=DIRECTION('ref_axis',(0.707100547519658,-0.707113014798483,0.));
#34288=DIRECTION('',(0.,0.,1.));
#34289=DIRECTION('center_axis',(-0.999999999961142,8.81569739766863E-6,
0.));
#34290=DIRECTION('ref_axis',(-8.81569739766863E-6,-0.999999999961142,0.));
#34291=DIRECTION('',(-8.81569739766863E-6,-0.999999999961142,0.));
#34292=DIRECTION('',(-8.81569739766863E-6,-0.999999999961142,0.));
#34293=DIRECTION('',(0.,0.,1.));
#34294=DIRECTION('center_axis',(0.,0.,1.));
#34295=DIRECTION('ref_axis',(0.999999999961142,-8.8156974001885E-6,0.));
#34296=DIRECTION('center_axis',(0.,0.,1.));
#34297=DIRECTION('ref_axis',(0.999999999961142,-8.8156974001885E-6,0.));
#34298=DIRECTION('center_axis',(0.,0.,-1.));
#34299=DIRECTION('ref_axis',(0.999999999961142,-8.8156974001885E-6,0.));
#34300=DIRECTION('',(0.,0.,1.));
#34301=DIRECTION('center_axis',(-0.707113014798484,-0.707100547519657,0.));
#34302=DIRECTION('ref_axis',(0.707100547519657,-0.707113014798484,0.));
#34303=DIRECTION('',(0.707100547519657,-0.707113014798484,0.));
#34304=DIRECTION('',(0.707100547519657,-0.707113014798484,0.));
#34305=DIRECTION('',(0.,0.,1.));
#34306=DIRECTION('center_axis',(0.,0.,1.));
#34307=DIRECTION('ref_axis',(0.707113014798483,0.707100547519659,0.));
#34308=DIRECTION('center_axis',(0.,0.,1.));
#34309=DIRECTION('ref_axis',(0.707113014798483,0.707100547519659,0.));
#34310=DIRECTION('center_axis',(0.,0.,-1.));
#34311=DIRECTION('ref_axis',(0.707113014798483,0.707100547519659,0.));
#34312=DIRECTION('',(0.,0.,1.));
#34313=DIRECTION('center_axis',(1.,0.,0.));
#34314=DIRECTION('ref_axis',(0.,1.,0.));
#34315=DIRECTION('',(0.,1.,0.));
#34316=DIRECTION('',(0.,1.,0.));
#34317=DIRECTION('',(0.,0.,1.));
#34318=DIRECTION('center_axis',(0.469471562785889,-0.882947592858928,0.));
#34319=DIRECTION('ref_axis',(0.882947592858928,0.469471562785889,0.));
#34320=DIRECTION('',(0.882947592858928,0.469471562785889,0.));
#34321=DIRECTION('',(0.882947592858928,0.469471562785889,0.));
#34322=DIRECTION('',(0.,0.,1.));
#34323=DIRECTION('center_axis',(0.,-1.,0.));
#34324=DIRECTION('ref_axis',(1.,0.,0.));
#34325=DIRECTION('',(1.,0.,0.));
#34326=DIRECTION('',(1.,0.,0.));
#34327=DIRECTION('',(0.,0.,1.));
#34328=DIRECTION('center_axis',(0.,0.,1.));
#34329=DIRECTION('ref_axis',(-1.,0.,0.));
#34330=DIRECTION('center_axis',(0.,0.,1.));
#34331=DIRECTION('ref_axis',(-1.,0.,0.));
#34332=DIRECTION('center_axis',(0.,0.,1.));
#34333=DIRECTION('ref_axis',(-1.,0.,0.));
#34334=DIRECTION('',(0.,0.,1.));
#34335=DIRECTION('center_axis',(-1.,0.,0.));
#34336=DIRECTION('ref_axis',(0.,-1.,0.));
#34337=DIRECTION('',(0.,-1.,0.));
#34338=DIRECTION('',(0.,-1.,0.));
#34339=DIRECTION('',(0.,0.,1.));
#34340=DIRECTION('center_axis',(0.,0.,1.));
#34341=DIRECTION('ref_axis',(0.,1.,0.));
#34342=DIRECTION('center_axis',(0.,0.,1.));
#34343=DIRECTION('ref_axis',(0.,1.,0.));
#34344=DIRECTION('center_axis',(0.,0.,1.));
#34345=DIRECTION('ref_axis',(0.,1.,0.));
#34346=DIRECTION('',(0.,0.,1.));
#34347=DIRECTION('center_axis',(0.,1.,0.));
#34348=DIRECTION('ref_axis',(-1.,0.,0.));
#34349=DIRECTION('',(-1.,0.,0.));
#34350=DIRECTION('',(-1.,0.,0.));
#34351=DIRECTION('',(0.,0.,1.));
#34352=DIRECTION('center_axis',(0.,0.,1.));
#34353=DIRECTION('ref_axis',(0.,-1.,0.));
#34354=DIRECTION('center_axis',(0.,0.,1.));
#34355=DIRECTION('ref_axis',(0.,-1.,0.));
#34356=DIRECTION('center_axis',(0.,0.,-1.));
#34357=DIRECTION('ref_axis',(0.,-1.,0.));
#34358=DIRECTION('',(0.,0.,1.));
#34359=DIRECTION('center_axis',(-0.707106781186547,0.707106781186548,0.));
#34360=DIRECTION('ref_axis',(-0.707106781186548,-0.707106781186547,0.));
#34361=DIRECTION('',(-0.707106781186548,-0.707106781186547,0.));
#34362=DIRECTION('',(-0.707106781186548,-0.707106781186547,0.));
#34363=DIRECTION('',(0.,0.,1.));
#34364=DIRECTION('center_axis',(-1.,0.,0.));
#34365=DIRECTION('ref_axis',(0.,-1.,0.));
#34366=DIRECTION('',(0.,-1.,0.));
#34367=DIRECTION('',(0.,-1.,0.));
#34368=DIRECTION('',(0.,0.,1.));
#34369=DIRECTION('center_axis',(-0.707106781186548,0.707106781186548,0.));
#34370=DIRECTION('ref_axis',(-0.707106781186548,-0.707106781186548,0.));
#34371=DIRECTION('',(0.707106781186547,0.707106781186547,0.));
#34372=DIRECTION('',(-0.707106781186547,-0.707106781186547,0.));
#34373=DIRECTION('',(0.,0.,1.));
#34374=DIRECTION('center_axis',(0.,0.,1.));
#34375=DIRECTION('ref_axis',(0.586372356735787,0.810041640445797,0.));
#34376=DIRECTION('center_axis',(0.,0.,1.));
#34377=DIRECTION('ref_axis',(0.586372356735787,0.810041640445797,0.));
#34378=DIRECTION('center_axis',(0.,0.,1.));
#34379=DIRECTION('ref_axis',(0.586372356735787,0.810041640445797,0.));
#34380=DIRECTION('',(0.,0.,1.));
#34381=DIRECTION('center_axis',(0.,0.,1.));
#34382=DIRECTION('ref_axis',(0.999993104732582,-0.0037135545358805,0.));
#34383=DIRECTION('center_axis',(0.,0.,1.));
#34384=DIRECTION('ref_axis',(-0.592372410147205,-0.805664277287004,0.));
#34385=DIRECTION('center_axis',(0.,0.,-1.));
#34386=DIRECTION('ref_axis',(-0.592372410147205,-0.805664277287004,0.));
#34387=DIRECTION('',(0.,0.,1.));
#34388=DIRECTION('center_axis',(0.,0.,1.));
#34389=DIRECTION('ref_axis',(-0.707106781186548,-0.707106781186548,0.));
#34390=DIRECTION('center_axis',(0.,0.,1.));
#34391=DIRECTION('ref_axis',(-0.707106781186548,-0.707106781186548,0.));
#34392=DIRECTION('center_axis',(0.,0.,1.));
#34393=DIRECTION('ref_axis',(-0.707106781186548,-0.707106781186548,0.));
#34394=DIRECTION('',(0.,0.,1.));
#34395=DIRECTION('center_axis',(-0.707106781186548,-0.707106781186548,0.));
#34396=DIRECTION('ref_axis',(0.707106781186548,-0.707106781186548,0.));
#34397=DIRECTION('',(0.707106781186547,-0.707106781186547,0.));
#34398=DIRECTION('',(0.707106781186547,-0.707106781186547,0.));
#34399=DIRECTION('',(0.,0.,1.));
#34400=DIRECTION('center_axis',(-1.,0.,0.));
#34401=DIRECTION('ref_axis',(0.,-1.,0.));
#34402=DIRECTION('',(0.,-1.,0.));
#34403=DIRECTION('',(0.,-1.,0.));
#34404=DIRECTION('',(0.,0.,1.));
#34405=DIRECTION('center_axis',(0.,0.,1.));
#34406=DIRECTION('ref_axis',(0.,1.,0.));
#34407=DIRECTION('center_axis',(0.,0.,1.));
#34408=DIRECTION('ref_axis',(0.,1.,0.));
#34409=DIRECTION('center_axis',(0.,0.,1.));
#34410=DIRECTION('ref_axis',(0.,1.,0.));
#34411=DIRECTION('',(0.,0.,1.));
#34412=DIRECTION('center_axis',(0.,1.,0.));
#34413=DIRECTION('ref_axis',(-1.,0.,0.));
#34414=DIRECTION('',(-1.,0.,0.));
#34415=DIRECTION('',(-1.,0.,0.));
#34416=DIRECTION('',(0.,0.,1.));
#34417=DIRECTION('center_axis',(1.,0.,0.));
#34418=DIRECTION('ref_axis',(0.,1.,0.));
#34419=DIRECTION('',(0.,1.,0.));
#34420=DIRECTION('',(0.,1.,0.));
#34421=DIRECTION('',(0.,0.,1.));
#34422=DIRECTION('center_axis',(0.,1.,0.));
#34423=DIRECTION('ref_axis',(-1.,0.,0.));
#34424=DIRECTION('',(1.,0.,0.));
#34425=DIRECTION('',(-1.,0.,0.));
#34426=DIRECTION('',(0.,0.,1.));
#34427=DIRECTION('center_axis',(-1.,0.,0.));
#34428=DIRECTION('ref_axis',(0.,-1.,0.));
#34429=DIRECTION('',(0.,1.,0.));
#34430=DIRECTION('',(0.,-1.,0.));
#34431=DIRECTION('',(0.,0.,1.));
#34432=DIRECTION('center_axis',(0.,1.,0.));
#34433=DIRECTION('ref_axis',(-1.,0.,0.));
#34434=DIRECTION('',(1.,0.,0.));
#34435=DIRECTION('',(-1.,0.,0.));
#34436=DIRECTION('',(0.,0.,1.));
#34437=DIRECTION('center_axis',(0.,0.,1.));
#34438=DIRECTION('ref_axis',(1.,8.88178419700124E-15,0.));
#34439=DIRECTION('center_axis',(0.,0.,1.));
#34440=DIRECTION('ref_axis',(1.,8.88178419700124E-15,0.));
#34441=DIRECTION('center_axis',(0.,0.,1.));
#34442=DIRECTION('ref_axis',(1.,8.88178419700124E-15,0.));
#34443=DIRECTION('',(0.,0.,1.));
#34444=DIRECTION('center_axis',(1.,0.,0.));
#34445=DIRECTION('ref_axis',(0.,1.,0.));
#34446=DIRECTION('',(0.,-1.,0.));
#34447=DIRECTION('',(0.,1.,0.));
#34448=DIRECTION('',(0.,0.,1.));
#34449=DIRECTION('center_axis',(0.707106781186548,-0.707106781186548,0.));
#34450=DIRECTION('ref_axis',(0.707106781186548,0.707106781186548,0.));
#34451=DIRECTION('',(-0.707106781186547,-0.707106781186547,0.));
#34452=DIRECTION('',(0.707106781186547,0.707106781186547,0.));
#34453=DIRECTION('',(0.,0.,1.));
#34454=DIRECTION('center_axis',(0.,0.,1.));
#34455=DIRECTION('ref_axis',(-0.586372356735787,-0.810041640445797,0.));
#34456=DIRECTION('center_axis',(0.,0.,1.));
#34457=DIRECTION('ref_axis',(-0.586372356735787,-0.810041640445797,0.));
#34458=DIRECTION('center_axis',(0.,0.,1.));
#34459=DIRECTION('ref_axis',(-0.586372356735787,-0.810041640445797,0.));
#34460=DIRECTION('',(0.,0.,1.));
#34461=DIRECTION('center_axis',(0.,0.,1.));
#34462=DIRECTION('ref_axis',(-0.999993104772333,-0.00371354383159855,0.));
#34463=DIRECTION('center_axis',(0.,0.,1.));
#34464=DIRECTION('ref_axis',(0.586372356735787,0.810041640445797,0.));
#34465=DIRECTION('center_axis',(0.,0.,-1.));
#34466=DIRECTION('ref_axis',(0.586372356735787,0.810041640445797,0.));
#34467=DIRECTION('',(0.,0.,1.));
#34468=DIRECTION('center_axis',(0.,0.,1.));
#34469=DIRECTION('ref_axis',(0.707106781186548,0.707106781186548,0.));
#34470=DIRECTION('center_axis',(0.,0.,1.));
#34471=DIRECTION('ref_axis',(0.707106781186548,0.707106781186548,0.));
#34472=DIRECTION('center_axis',(0.,0.,1.));
#34473=DIRECTION('ref_axis',(0.707106781186548,0.707106781186548,0.));
#34474=DIRECTION('',(0.,0.,1.));
#34475=DIRECTION('center_axis',(0.707106781186548,0.707106781186548,0.));
#34476=DIRECTION('ref_axis',(-0.707106781186548,0.707106781186548,0.));
#34477=DIRECTION('',(-0.707106781186547,0.707106781186547,0.));
#34478=DIRECTION('',(-0.707106781186547,0.707106781186547,0.));
#34479=DIRECTION('',(0.,0.,1.));
#34480=DIRECTION('center_axis',(1.,0.,0.));
#34481=DIRECTION('ref_axis',(0.,1.,0.));
#34482=DIRECTION('',(0.,-1.,0.));
#34483=DIRECTION('',(0.,1.,0.));
#34484=DIRECTION('',(0.,0.,1.));
#34485=DIRECTION('center_axis',(0.707106781186547,0.707106781186548,0.));
#34486=DIRECTION('ref_axis',(-0.707106781186548,0.707106781186547,0.));
#34487=DIRECTION('',(0.707106781186548,-0.707106781186547,0.));
#34488=DIRECTION('',(-0.707106781186548,0.707106781186547,0.));
#34489=DIRECTION('',(0.,0.,1.));
#34490=DIRECTION('center_axis',(0.,0.,1.));
#34491=DIRECTION('ref_axis',(-0.707106781186546,-0.707106781186549,0.));
#34492=DIRECTION('center_axis',(0.,0.,1.));
#34493=DIRECTION('ref_axis',(-0.707106781186546,-0.707106781186549,0.));
#34494=DIRECTION('center_axis',(0.,0.,-1.));
#34495=DIRECTION('ref_axis',(-0.707106781186546,-0.707106781186549,0.));
#34496=DIRECTION('',(0.,0.,1.));
#34497=DIRECTION('center_axis',(0.,1.,0.));
#34498=DIRECTION('ref_axis',(-1.,0.,0.));
#34499=DIRECTION('',(1.,0.,0.));
#34500=DIRECTION('',(-1.,0.,0.));
#34501=DIRECTION('',(0.,0.,1.));
#34502=DIRECTION('center_axis',(0.,0.,1.));
#34503=DIRECTION('ref_axis',(1.,0.,0.));
#34504=DIRECTION('center_axis',(0.,0.,1.));
#34505=DIRECTION('ref_axis',(1.,0.,0.));
#34506=DIRECTION('center_axis',(0.,0.,1.));
#34507=DIRECTION('ref_axis',(1.,0.,0.));
#34508=DIRECTION('',(0.,0.,1.));
#34509=DIRECTION('center_axis',(1.,0.,0.));
#34510=DIRECTION('ref_axis',(0.,1.,0.));
#34511=DIRECTION('',(0.,-1.,0.));
#34512=DIRECTION('',(0.,1.,0.));
#34513=DIRECTION('',(0.,0.,1.));
#34514=DIRECTION('center_axis',(0.,0.,1.));
#34515=DIRECTION('ref_axis',(0.,-1.,0.));
#34516=DIRECTION('center_axis',(0.,0.,1.));
#34517=DIRECTION('ref_axis',(0.,-1.,0.));
#34518=DIRECTION('center_axis',(0.,0.,1.));
#34519=DIRECTION('ref_axis',(0.,-1.,0.));
#34520=DIRECTION('',(0.,0.,1.));
#34521=DIRECTION('center_axis',(0.,-1.,0.));
#34522=DIRECTION('ref_axis',(1.,0.,0.));
#34523=DIRECTION('',(-1.,0.,0.));
#34524=DIRECTION('',(1.,0.,0.));
#34525=DIRECTION('',(0.,0.,1.));
#34526=DIRECTION('center_axis',(-0.469471562785891,-0.882947592858927,0.));
#34527=DIRECTION('ref_axis',(0.882947592858927,-0.469471562785891,0.));
#34528=DIRECTION('',(-0.882947592858927,0.469471562785891,0.));
#34529=DIRECTION('',(0.882947592858927,-0.469471562785891,0.));
#34530=DIRECTION('',(0.,0.,1.));
#34531=DIRECTION('center_axis',(-1.,0.,0.));
#34532=DIRECTION('ref_axis',(0.,-1.,0.));
#34533=DIRECTION('',(0.,1.,0.));
#34534=DIRECTION('',(0.,-1.,0.));
#34535=DIRECTION('',(0.,0.,1.));
#34536=DIRECTION('center_axis',(0.,0.,1.));
#34537=DIRECTION('ref_axis',(1.,0.,0.));
#34538=DIRECTION('center_axis',(0.,0.,1.));
#34539=DIRECTION('ref_axis',(1.,0.,0.));
#34540=DIRECTION('center_axis',(0.,0.,-1.));
#34541=DIRECTION('ref_axis',(1.,0.,0.));
#34542=DIRECTION('',(0.,0.,1.));
#34543=DIRECTION('center_axis',(0.707113014798485,-0.707100547519656,0.));
#34544=DIRECTION('ref_axis',(0.707100547519656,0.707113014798485,0.));
#34545=DIRECTION('',(-0.707100547519656,-0.707113014798485,0.));
#34546=DIRECTION('',(0.707100547519656,0.707113014798485,0.));
#34547=DIRECTION('',(0.,0.,1.));
#34548=DIRECTION('center_axis',(0.,0.,1.));
#34549=DIRECTION('ref_axis',(-0.707113014798483,0.707100547519658,0.));
#34550=DIRECTION('center_axis',(0.,0.,1.));
#34551=DIRECTION('ref_axis',(-0.707113014798483,0.707100547519658,0.));
#34552=DIRECTION('center_axis',(0.,0.,-1.));
#34553=DIRECTION('ref_axis',(-0.707113014798483,0.707100547519658,0.));
#34554=DIRECTION('',(0.,0.,1.));
#34555=DIRECTION('center_axis',(0.999999999961142,8.81569739766863E-6,0.));
#34556=DIRECTION('ref_axis',(-8.81569739766863E-6,0.999999999961142,0.));
#34557=DIRECTION('',(8.81569739766863E-6,-0.999999999961142,0.));
#34558=DIRECTION('',(-8.81569739766863E-6,0.999999999961142,0.));
#34559=DIRECTION('',(0.,0.,1.));
#34560=DIRECTION('center_axis',(0.,0.,1.));
#34561=DIRECTION('ref_axis',(-0.999999999961142,-8.81569739996647E-6,0.));
#34562=DIRECTION('center_axis',(0.,0.,1.));
#34563=DIRECTION('ref_axis',(-0.999999999961142,-8.81569739996647E-6,0.));
#34564=DIRECTION('center_axis',(0.,0.,-1.));
#34565=DIRECTION('ref_axis',(-0.999999999961142,-8.81569739996647E-6,0.));
#34566=DIRECTION('',(0.,0.,1.));
#34567=DIRECTION('center_axis',(0.707100547519659,0.707113014798482,0.));
#34568=DIRECTION('ref_axis',(-0.707113014798482,0.707100547519659,0.));
#34569=DIRECTION('',(-0.707113014798482,0.707100547519659,0.));
#34570=DIRECTION('',(-0.707113014798482,0.707100547519659,0.));
#34571=DIRECTION('',(0.,0.,1.));
#34572=DIRECTION('center_axis',(0.,0.,1.));
#34573=DIRECTION('ref_axis',(-0.707100547519656,-0.707113014798485,0.));
#34574=DIRECTION('center_axis',(0.,0.,1.));
#34575=DIRECTION('ref_axis',(-0.707100547519656,-0.707113014798485,0.));
#34576=DIRECTION('center_axis',(0.,0.,-1.));
#34577=DIRECTION('ref_axis',(-0.707100547519656,-0.707113014798485,0.));
#34578=DIRECTION('',(0.,0.,1.));
#34579=DIRECTION('center_axis',(-0.999999999844567,-1.76313947965879E-5,
0.));
#34580=DIRECTION('ref_axis',(1.76313947965879E-5,-0.999999999844567,0.));
#34581=DIRECTION('',(1.76313947965879E-5,-0.999999999844567,0.));
#34582=DIRECTION('',(1.76313947965879E-5,-0.999999999844567,0.));
#34583=DIRECTION('',(0.,0.,1.));
#34584=DIRECTION('center_axis',(-0.469487130310524,0.882939315283213,0.));
#34585=DIRECTION('ref_axis',(-0.882939315283213,-0.469487130310524,0.));
#34586=DIRECTION('',(-0.882939315283213,-0.469487130310524,0.));
#34587=DIRECTION('',(-0.882939315283213,-0.469487130310524,0.));
#34588=DIRECTION('',(0.,0.,1.));
#34589=DIRECTION('center_axis',(-1.76313947987393E-5,0.999999999844567,
0.));
#34590=DIRECTION('ref_axis',(-0.999999999844567,-1.76313947987393E-5,0.));
#34591=DIRECTION('',(-0.999999999844567,-1.76313947987393E-5,0.));
#34592=DIRECTION('',(-0.999999999844567,-1.76313947987393E-5,0.));
#34593=DIRECTION('',(0.,0.,1.));
#34594=DIRECTION('center_axis',(0.,0.,1.));
#34595=DIRECTION('ref_axis',(0.999999999844567,1.76313947978603E-5,0.));
#34596=DIRECTION('center_axis',(0.,0.,1.));
#34597=DIRECTION('ref_axis',(0.999999999844567,1.76313947978603E-5,0.));
#34598=DIRECTION('center_axis',(0.,0.,1.));
#34599=DIRECTION('ref_axis',(0.999999999844567,1.76313947978603E-5,0.));
#34600=DIRECTION('',(0.,0.,1.));
#34601=DIRECTION('center_axis',(0.999999999844567,1.76313947990255E-5,0.));
#34602=DIRECTION('ref_axis',(-1.76313947990255E-5,0.999999999844567,0.));
#34603=DIRECTION('',(-1.76313947990255E-5,0.999999999844567,0.));
#34604=DIRECTION('',(-1.76313947990255E-5,0.999999999844567,0.));
#34605=DIRECTION('',(0.,0.,1.));
#34606=DIRECTION('center_axis',(0.,0.,1.));
#34607=DIRECTION('ref_axis',(1.76313947974904E-5,-0.999999999844567,0.));
#34608=DIRECTION('center_axis',(0.,0.,1.));
#34609=DIRECTION('ref_axis',(1.76313947974904E-5,-0.999999999844567,0.));
#34610=DIRECTION('center_axis',(0.,0.,1.));
#34611=DIRECTION('ref_axis',(1.76313947974904E-5,-0.999999999844567,0.));
#34612=DIRECTION('',(0.,0.,1.));
#34613=DIRECTION('center_axis',(1.76313948097558E-5,-0.999999999844567,
0.));
#34614=DIRECTION('ref_axis',(0.999999999844567,1.76313948097558E-5,0.));
#34615=DIRECTION('',(0.999999999844567,1.76313948097558E-5,0.));
#34616=DIRECTION('',(0.999999999844567,1.76313948097558E-5,0.));
#34617=DIRECTION('',(0.,0.,1.));
#34618=DIRECTION('center_axis',(0.,0.,1.));
#34619=DIRECTION('ref_axis',(-1.76313947930495E-5,0.999999999844567,0.));
#34620=DIRECTION('center_axis',(0.,0.,1.));
#34621=DIRECTION('ref_axis',(-1.76313947930495E-5,0.999999999844567,0.));
#34622=DIRECTION('center_axis',(0.,0.,-1.));
#34623=DIRECTION('ref_axis',(-1.76313947930495E-5,0.999999999844567,0.));
#34624=DIRECTION('',(0.,0.,1.));
#34625=DIRECTION('center_axis',(0.707119248355464,-0.707094313797816,0.));
#34626=DIRECTION('ref_axis',(0.707094313797816,0.707119248355464,0.));
#34627=DIRECTION('',(0.707094313797816,0.707119248355464,0.));
#34628=DIRECTION('',(0.707094313797816,0.707119248355464,0.));
#34629=DIRECTION('',(0.,0.,1.));
#34630=DIRECTION('center_axis',(0.999999999844567,1.76313948004511E-5,0.));
#34631=DIRECTION('ref_axis',(-1.76313948004511E-5,0.999999999844567,0.));
#34632=DIRECTION('',(-1.76313948004511E-5,0.999999999844567,0.));
#34633=DIRECTION('',(-1.76313948004511E-5,0.999999999844567,0.));
#34634=DIRECTION('',(0.,0.,1.));
#34635=DIRECTION('center_axis',(0.707119248355465,-0.707094313797815,0.));
#34636=DIRECTION('ref_axis',(0.707094313797815,0.707119248355465,0.));
#34637=DIRECTION('',(-0.707094313797815,-0.707119248355465,0.));
#34638=DIRECTION('',(0.707094313797815,0.707119248355465,0.));
#34639=DIRECTION('',(0.,0.,1.));
#34640=DIRECTION('center_axis',(0.,0.,1.));
#34641=DIRECTION('ref_axis',(-0.586358074480661,-0.810051978882424,0.));
#34642=DIRECTION('center_axis',(0.,0.,1.));
#34643=DIRECTION('ref_axis',(-0.586358074480661,-0.810051978882424,0.));
#34644=DIRECTION('center_axis',(0.,0.,1.));
#34645=DIRECTION('ref_axis',(-0.586358074480661,-0.810051978882424,0.));
#34646=DIRECTION('',(0.,0.,1.));
#34647=DIRECTION('center_axis',(0.,0.,1.));
#34648=DIRECTION('ref_axis',(-0.999993170052296,0.00369592326208568,0.));
#34649=DIRECTION('center_axis',(0.,0.,1.));
#34650=DIRECTION('ref_axis',(0.592358205070174,0.805674721513615,0.));
#34651=DIRECTION('center_axis',(0.,0.,-1.));
#34652=DIRECTION('ref_axis',(0.592358205070174,0.805674721513615,0.));
#34653=DIRECTION('',(0.,0.,1.));
#34654=DIRECTION('center_axis',(0.,0.,1.));
#34655=DIRECTION('ref_axis',(0.707094313797827,0.707119248355453,0.));
#34656=DIRECTION('center_axis',(0.,0.,1.));
#34657=DIRECTION('ref_axis',(0.707094313797827,0.707119248355453,0.));
#34658=DIRECTION('center_axis',(0.,0.,1.));
#34659=DIRECTION('ref_axis',(0.707094313797827,0.707119248355453,0.));
#34660=DIRECTION('',(0.,0.,1.));
#34661=DIRECTION('center_axis',(0.707094313797817,0.707119248355463,0.));
#34662=DIRECTION('ref_axis',(-0.707119248355463,0.707094313797817,0.));
#34663=DIRECTION('',(-0.707119248355463,0.707094313797817,0.));
#34664=DIRECTION('',(-0.707119248355463,0.707094313797817,0.));
#34665=DIRECTION('',(0.,0.,1.));
#34666=DIRECTION('center_axis',(0.999999999844567,1.76313948019314E-5,0.));
#34667=DIRECTION('ref_axis',(-1.76313948019314E-5,0.999999999844567,0.));
#34668=DIRECTION('',(-1.76313948019314E-5,0.999999999844567,0.));
#34669=DIRECTION('',(-1.76313948019314E-5,0.999999999844567,0.));
#34670=DIRECTION('center_axis',(0.,0.,1.));
#34671=DIRECTION('ref_axis',(1.,0.,0.));
#34672=DIRECTION('center_axis',(0.,0.,1.));
#34673=DIRECTION('ref_axis',(1.,0.,0.));
#34674=DIRECTION('axis',(0.,0.,1.));
#34675=DIRECTION('refdir',(1.,0.,0.));
#34676=DIRECTION('center_axis',(-1.,0.,0.));
#34677=DIRECTION('ref_axis',(0.,0.878663232865503,-0.477442062673936));
#34678=DIRECTION('',(-1.,0.,0.));
#34679=DIRECTION('center_axis',(-1.,0.,0.));
#34680=DIRECTION('ref_axis',(0.,-1.74186785585433E-15,-1.));
#34681=DIRECTION('center_axis',(-1.,0.,0.));
#34682=DIRECTION('ref_axis',(0.,0.878663232865503,-0.477442062673936));
#34683=DIRECTION('',(-1.,0.,0.));
#34684=DIRECTION('center_axis',(-1.,0.,0.));
#34685=DIRECTION('ref_axis',(0.,0.878663232865503,-0.477442062673936));
#34686=DIRECTION('',(-1.,0.,0.));
#34687=DIRECTION('center_axis',(-1.,0.,0.));
#34688=DIRECTION('ref_axis',(0.,0.878663232865503,-0.477442062673936));
#34689=DIRECTION('',(-1.,0.,0.));
#34690=DIRECTION('center_axis',(1.,0.,0.));
#34691=DIRECTION('ref_axis',(0.,-0.878663231892279,-0.477442064465015));
#34692=DIRECTION('',(1.,0.,0.));
#34693=DIRECTION('center_axis',(1.,0.,0.));
#34694=DIRECTION('ref_axis',(0.,-1.74186785585433E-15,-1.));
#34695=DIRECTION('center_axis',(1.,0.,0.));
#34696=DIRECTION('ref_axis',(0.,-0.878663231892279,-0.477442064465015));
#34697=DIRECTION('',(1.,0.,0.));
#34698=DIRECTION('center_axis',(1.,0.,0.));
#34699=DIRECTION('ref_axis',(0.,-0.878663231892279,-0.477442064465015));
#34700=DIRECTION('',(1.,0.,0.));
#34701=DIRECTION('center_axis',(1.,0.,0.));
#34702=DIRECTION('ref_axis',(0.,-0.878663231892279,-0.477442064465015));
#34703=DIRECTION('',(1.,0.,0.));
#34704=DIRECTION('center_axis',(0.,0.,-1.));
#34705=DIRECTION('ref_axis',(-0.609193659724225,0.793021490851165,0.));
#34706=DIRECTION('',(0.,0.,-1.));
#34707=DIRECTION('center_axis',(0.,0.,-1.));
#34708=DIRECTION('ref_axis',(1.,8.06646416329218E-14,0.));
#34709=DIRECTION('center_axis',(0.,0.,-1.));
#34710=DIRECTION('ref_axis',(-0.609193659724225,0.793021490851165,0.));
#34711=DIRECTION('',(0.,0.,-1.));
#34712=DIRECTION('center_axis',(0.,0.,-1.));
#34713=DIRECTION('ref_axis',(-0.609193659724225,0.793021490851165,0.));
#34714=DIRECTION('',(0.,0.,-1.));
#34715=DIRECTION('center_axis',(0.,0.,-1.));
#34716=DIRECTION('ref_axis',(-0.609193659724225,0.793021490851165,0.));
#34717=DIRECTION('',(0.,0.,-1.));
#34718=DIRECTION('center_axis',(0.,0.,-1.));
#34719=DIRECTION('ref_axis',(-0.609193659724225,0.793021490851165,0.));
#34720=DIRECTION('',(0.,0.,-1.));
#34721=DIRECTION('center_axis',(0.,0.,-1.));
#34722=DIRECTION('ref_axis',(-0.609193659724225,0.793021490851165,0.));
#34723=DIRECTION('',(0.,0.,-1.));
#34724=DIRECTION('center_axis',(0.,0.,-1.));
#34725=DIRECTION('ref_axis',(-0.609193659724225,0.793021490851165,0.));
#34726=DIRECTION('',(0.,0.,-1.));
#34727=DIRECTION('center_axis',(0.,0.,-1.));
#34728=DIRECTION('ref_axis',(-0.609193659724225,0.793021490851165,0.));
#34729=DIRECTION('',(0.,0.,-1.));
#34730=DIRECTION('center_axis',(0.,0.,-1.));
#34731=DIRECTION('ref_axis',(-0.609193659724225,0.793021490851165,0.));
#34732=DIRECTION('',(0.,0.,-1.));
#34733=DIRECTION('center_axis',(0.,0.,-1.));
#34734=DIRECTION('ref_axis',(-0.609193659724225,0.793021490851165,0.));
#34735=DIRECTION('',(0.,0.,-1.));
#34736=DIRECTION('center_axis',(0.,0.,-1.));
#34737=DIRECTION('ref_axis',(-0.609193659724225,0.793021490851165,0.));
#34738=DIRECTION('',(0.,0.,-1.));
#34739=DIRECTION('center_axis',(0.,0.,-1.));
#34740=DIRECTION('ref_axis',(-0.609193659724225,0.793021490851165,0.));
#34741=DIRECTION('',(0.,0.,-1.));
#34742=DIRECTION('center_axis',(0.,0.,-1.));
#34743=DIRECTION('ref_axis',(-0.609193659724225,0.793021490851165,0.));
#34744=DIRECTION('',(0.,0.,-1.));
#34745=DIRECTION('center_axis',(0.,0.,-1.));
#34746=DIRECTION('ref_axis',(-0.609193659724225,0.793021490851165,0.));
#34747=DIRECTION('',(0.,0.,-1.));
#34748=DIRECTION('center_axis',(0.,0.,-1.));
#34749=DIRECTION('ref_axis',(-0.609193659724225,0.793021490851165,0.));
#34750=DIRECTION('',(0.,0.,-1.));
#34751=DIRECTION('center_axis',(0.,0.,-1.));
#34752=DIRECTION('ref_axis',(-0.609193659724225,0.793021490851165,0.));
#34753=DIRECTION('',(0.,0.,-1.));
#34754=DIRECTION('center_axis',(0.,0.,-1.));
#34755=DIRECTION('ref_axis',(-0.609193659724225,0.793021490851165,0.));
#34756=DIRECTION('',(0.,0.,-1.));
#34757=DIRECTION('center_axis',(0.,0.,-1.));
#34758=DIRECTION('ref_axis',(-0.609193659724225,0.793021490851165,0.));
#34759=DIRECTION('',(0.,0.,-1.));
#34760=DIRECTION('center_axis',(0.,0.,-1.));
#34761=DIRECTION('ref_axis',(-0.609193659724225,0.793021490851165,0.));
#34762=DIRECTION('',(0.,0.,-1.));
#34763=DIRECTION('center_axis',(0.,0.,-1.));
#34764=DIRECTION('ref_axis',(-0.609193659724225,0.793021490851165,0.));
#34765=DIRECTION('',(0.,0.,-1.));
#34766=DIRECTION('center_axis',(0.,0.,-1.));
#34767=DIRECTION('ref_axis',(-0.609193659724225,0.793021490851165,0.));
#34768=DIRECTION('',(0.,0.,-1.));
#34769=DIRECTION('center_axis',(0.,0.,-1.));
#34770=DIRECTION('ref_axis',(-0.609193659724225,0.793021490851165,0.));
#34771=DIRECTION('',(0.,0.,-1.));
#34772=DIRECTION('center_axis',(0.,0.,-1.));
#34773=DIRECTION('ref_axis',(-0.609193659724225,0.793021490851165,0.));
#34774=DIRECTION('',(0.,0.,-1.));
#34775=DIRECTION('center_axis',(0.,0.,-1.));
#34776=DIRECTION('ref_axis',(-0.609193659724225,0.793021490851165,0.));
#34777=DIRECTION('',(0.,0.,-1.));
#34778=DIRECTION('center_axis',(0.,0.,-1.));
#34779=DIRECTION('ref_axis',(-0.609193659724225,0.793021490851165,0.));
#34780=DIRECTION('',(0.,0.,-1.));
#34781=DIRECTION('center_axis',(0.,0.,-1.));
#34782=DIRECTION('ref_axis',(-0.609193659724225,0.793021490851165,0.));
#34783=DIRECTION('',(0.,0.,-1.));
#34784=DIRECTION('center_axis',(0.,0.,-1.));
#34785=DIRECTION('ref_axis',(-0.609193659724225,0.793021490851165,0.));
#34786=DIRECTION('',(0.,0.,-1.));
#34787=DIRECTION('center_axis',(0.,0.,-1.));
#34788=DIRECTION('ref_axis',(-0.609193645039877,0.793021502131581,0.));
#34789=DIRECTION('',(0.,0.,-1.));
#34790=DIRECTION('center_axis',(0.,0.,-1.));
#34791=DIRECTION('ref_axis',(1.,8.15320033709099E-14,0.));
#34792=DIRECTION('center_axis',(0.,0.,-1.));
#34793=DIRECTION('ref_axis',(-0.609193645039877,0.793021502131581,0.));
#34794=DIRECTION('',(0.,0.,-1.));
#34795=DIRECTION('center_axis',(0.,0.,-1.));
#34796=DIRECTION('ref_axis',(-0.609193645039877,0.793021502131581,0.));
#34797=DIRECTION('',(0.,0.,-1.));
#34798=DIRECTION('center_axis',(0.,0.,-1.));
#34799=DIRECTION('ref_axis',(-0.609193645039877,0.793021502131581,0.));
#34800=DIRECTION('',(0.,0.,-1.));
#34801=DIRECTION('center_axis',(0.,0.,-1.));
#34802=DIRECTION('ref_axis',(-0.609193645039877,0.793021502131581,0.));
#34803=DIRECTION('',(0.,0.,-1.));
#34804=DIRECTION('center_axis',(0.,0.,-1.));
#34805=DIRECTION('ref_axis',(-0.609193645039877,0.793021502131581,0.));
#34806=DIRECTION('',(0.,0.,-1.));
#34807=DIRECTION('center_axis',(0.,0.,-1.));
#34808=DIRECTION('ref_axis',(-0.609193645039877,0.793021502131581,0.));
#34809=DIRECTION('',(0.,0.,-1.));
#34810=DIRECTION('center_axis',(0.,0.,-1.));
#34811=DIRECTION('ref_axis',(-0.609193645039877,0.793021502131581,0.));
#34812=DIRECTION('',(0.,0.,-1.));
#34813=DIRECTION('center_axis',(0.,0.,-1.));
#34814=DIRECTION('ref_axis',(-0.609193645039877,0.793021502131581,0.));
#34815=DIRECTION('',(0.,0.,-1.));
#34816=DIRECTION('center_axis',(0.,0.,-1.));
#34817=DIRECTION('ref_axis',(-0.609193645039877,0.793021502131581,0.));
#34818=DIRECTION('',(0.,0.,-1.));
#34819=DIRECTION('center_axis',(0.,0.,-1.));
#34820=DIRECTION('ref_axis',(-0.609193645039877,0.793021502131581,0.));
#34821=DIRECTION('',(0.,0.,-1.));
#34822=DIRECTION('center_axis',(0.,0.,-1.));
#34823=DIRECTION('ref_axis',(-0.609193645039877,0.793021502131581,0.));
#34824=DIRECTION('',(0.,0.,-1.));
#34825=DIRECTION('center_axis',(0.,0.,-1.));
#34826=DIRECTION('ref_axis',(-0.609193645039877,0.793021502131581,0.));
#34827=DIRECTION('',(0.,0.,-1.));
#34828=DIRECTION('center_axis',(0.,0.,-1.));
#34829=DIRECTION('ref_axis',(-0.609193645039877,0.793021502131581,0.));
#34830=DIRECTION('',(0.,0.,-1.));
#34831=DIRECTION('center_axis',(0.,0.,-1.));
#34832=DIRECTION('ref_axis',(-0.609193645039877,0.793021502131581,0.));
#34833=DIRECTION('',(0.,0.,-1.));
#34834=DIRECTION('center_axis',(0.,0.,-1.));
#34835=DIRECTION('ref_axis',(-0.609193645039877,0.793021502131581,0.));
#34836=DIRECTION('',(0.,0.,-1.));
#34837=DIRECTION('center_axis',(0.,0.,-1.));
#34838=DIRECTION('ref_axis',(-0.609193645039877,0.793021502131581,0.));
#34839=DIRECTION('',(0.,0.,-1.));
#34840=DIRECTION('center_axis',(0.,0.,-1.));
#34841=DIRECTION('ref_axis',(-0.609193645039877,0.793021502131581,0.));
#34842=DIRECTION('',(0.,0.,-1.));
#34843=DIRECTION('center_axis',(0.,0.,-1.));
#34844=DIRECTION('ref_axis',(-0.609193645039877,0.793021502131581,0.));
#34845=DIRECTION('',(0.,0.,-1.));
#34846=DIRECTION('center_axis',(0.,0.,-1.));
#34847=DIRECTION('ref_axis',(-0.609193645039877,0.793021502131581,0.));
#34848=DIRECTION('',(0.,0.,-1.));
#34849=DIRECTION('center_axis',(0.,0.,-1.));
#34850=DIRECTION('ref_axis',(-0.609193645039877,0.793021502131581,0.));
#34851=DIRECTION('',(0.,0.,-1.));
#34852=DIRECTION('center_axis',(0.,0.,-1.));
#34853=DIRECTION('ref_axis',(-0.609193645039877,0.793021502131581,0.));
#34854=DIRECTION('',(0.,0.,-1.));
#34855=DIRECTION('center_axis',(0.,0.,-1.));
#34856=DIRECTION('ref_axis',(-0.609193645039877,0.793021502131581,0.));
#34857=DIRECTION('',(0.,0.,-1.));
#34858=DIRECTION('center_axis',(0.,0.,-1.));
#34859=DIRECTION('ref_axis',(-0.609193645039877,0.793021502131581,0.));
#34860=DIRECTION('',(0.,0.,-1.));
#34861=DIRECTION('center_axis',(0.,0.,-1.));
#34862=DIRECTION('ref_axis',(-0.609193645039877,0.793021502131581,0.));
#34863=DIRECTION('',(0.,0.,-1.));
#34864=DIRECTION('center_axis',(0.,0.,-1.));
#34865=DIRECTION('ref_axis',(-0.609193645039877,0.793021502131581,0.));
#34866=DIRECTION('',(0.,0.,-1.));
#34867=DIRECTION('center_axis',(0.,0.,-1.));
#34868=DIRECTION('ref_axis',(-0.609193645039877,0.793021502131581,0.));
#34869=DIRECTION('',(0.,0.,-1.));
#34870=DIRECTION('center_axis',(0.,0.,-1.));
#34871=DIRECTION('ref_axis',(-0.609193651103488,0.793021497473556,0.));
#34872=DIRECTION('',(0.,0.,-1.));
#34873=DIRECTION('center_axis',(0.,0.,-1.));
#34874=DIRECTION('ref_axis',(1.,7.80625564189563E-14,0.));
#34875=DIRECTION('center_axis',(0.,0.,-1.));
#34876=DIRECTION('ref_axis',(-0.609193651103488,0.793021497473556,0.));
#34877=DIRECTION('',(0.,0.,-1.));
#34878=DIRECTION('center_axis',(0.,0.,-1.));
#34879=DIRECTION('ref_axis',(-0.609193651103488,0.793021497473556,0.));
#34880=DIRECTION('',(0.,0.,-1.));
#34881=DIRECTION('center_axis',(0.,0.,-1.));
#34882=DIRECTION('ref_axis',(-0.609193651103488,0.793021497473556,0.));
#34883=DIRECTION('',(0.,0.,-1.));
#34884=DIRECTION('center_axis',(0.,0.,-1.));
#34885=DIRECTION('ref_axis',(-0.609193651103488,0.793021497473556,0.));
#34886=DIRECTION('',(0.,0.,-1.));
#34887=DIRECTION('center_axis',(0.,0.,-1.));
#34888=DIRECTION('ref_axis',(-0.609193651103488,0.793021497473556,0.));
#34889=DIRECTION('',(0.,0.,-1.));
#34890=DIRECTION('center_axis',(0.,0.,-1.));
#34891=DIRECTION('ref_axis',(-0.609193651103488,0.793021497473556,0.));
#34892=DIRECTION('',(0.,0.,-1.));
#34893=DIRECTION('center_axis',(0.,0.,-1.));
#34894=DIRECTION('ref_axis',(-0.609193651103488,0.793021497473556,0.));
#34895=DIRECTION('',(0.,0.,-1.));
#34896=DIRECTION('center_axis',(0.,0.,-1.));
#34897=DIRECTION('ref_axis',(-0.609193651103488,0.793021497473556,0.));
#34898=DIRECTION('',(0.,0.,-1.));
#34899=DIRECTION('center_axis',(0.,0.,-1.));
#34900=DIRECTION('ref_axis',(-0.609193651103488,0.793021497473556,0.));
#34901=DIRECTION('',(0.,0.,-1.));
#34902=DIRECTION('center_axis',(0.,0.,-1.));
#34903=DIRECTION('ref_axis',(-0.609193651103488,0.793021497473556,0.));
#34904=DIRECTION('',(0.,0.,-1.));
#34905=DIRECTION('center_axis',(0.,0.,-1.));
#34906=DIRECTION('ref_axis',(-0.609193651103488,0.793021497473556,0.));
#34907=DIRECTION('',(0.,0.,-1.));
#34908=DIRECTION('center_axis',(0.,0.,-1.));
#34909=DIRECTION('ref_axis',(-0.609193651103488,0.793021497473556,0.));
#34910=DIRECTION('',(0.,0.,-1.));
#34911=DIRECTION('center_axis',(0.,0.,-1.));
#34912=DIRECTION('ref_axis',(-0.609193651103488,0.793021497473556,0.));
#34913=DIRECTION('',(0.,0.,-1.));
#34914=DIRECTION('center_axis',(0.,0.,-1.));
#34915=DIRECTION('ref_axis',(-0.609193651103488,0.793021497473556,0.));
#34916=DIRECTION('',(0.,0.,-1.));
#34917=DIRECTION('center_axis',(0.,0.,-1.));
#34918=DIRECTION('ref_axis',(-0.609193651103488,0.793021497473556,0.));
#34919=DIRECTION('',(0.,0.,-1.));
#34920=DIRECTION('center_axis',(0.,0.,-1.));
#34921=DIRECTION('ref_axis',(-0.609193651103488,0.793021497473556,0.));
#34922=DIRECTION('',(0.,0.,-1.));
#34923=DIRECTION('center_axis',(0.,0.,-1.));
#34924=DIRECTION('ref_axis',(-0.609193651103488,0.793021497473556,0.));
#34925=DIRECTION('',(0.,0.,-1.));
#34926=DIRECTION('center_axis',(0.,0.,-1.));
#34927=DIRECTION('ref_axis',(-0.609193651103488,0.793021497473556,0.));
#34928=DIRECTION('',(0.,0.,-1.));
#34929=DIRECTION('center_axis',(0.,0.,-1.));
#34930=DIRECTION('ref_axis',(-0.609193651103488,0.793021497473556,0.));
#34931=DIRECTION('',(0.,0.,-1.));
#34932=DIRECTION('center_axis',(0.,0.,-1.));
#34933=DIRECTION('ref_axis',(-0.609193651103488,0.793021497473556,0.));
#34934=DIRECTION('',(0.,0.,-1.));
#34935=DIRECTION('center_axis',(0.,0.,-1.));
#34936=DIRECTION('ref_axis',(-0.609193651103488,0.793021497473556,0.));
#34937=DIRECTION('',(0.,0.,-1.));
#34938=DIRECTION('center_axis',(0.,0.,-1.));
#34939=DIRECTION('ref_axis',(-0.609193651103488,0.793021497473556,0.));
#34940=DIRECTION('',(0.,0.,-1.));
#34941=DIRECTION('center_axis',(0.,0.,-1.));
#34942=DIRECTION('ref_axis',(-0.609193651103488,0.793021497473556,0.));
#34943=DIRECTION('',(0.,0.,-1.));
#34944=DIRECTION('center_axis',(0.,0.,-1.));
#34945=DIRECTION('ref_axis',(-0.609193651103488,0.793021497473556,0.));
#34946=DIRECTION('',(0.,0.,-1.));
#34947=DIRECTION('center_axis',(0.,0.,-1.));
#34948=DIRECTION('ref_axis',(-0.609193651103488,0.793021497473556,0.));
#34949=DIRECTION('',(0.,0.,-1.));
#34950=DIRECTION('center_axis',(0.,0.,-1.));
#34951=DIRECTION('ref_axis',(-0.609193651103488,0.793021497473556,0.));
#34952=DIRECTION('',(0.,0.,-1.));
#34953=DIRECTION('center_axis',(0.,0.,-1.));
#34954=DIRECTION('ref_axis',(-0.609193695218696,0.793021463584555,0.));
#34955=DIRECTION('',(0.,0.,-1.));
#34956=DIRECTION('center_axis',(0.,0.,-1.));
#34957=DIRECTION('ref_axis',(1.,7.89299181569448E-14,0.));
#34958=DIRECTION('center_axis',(0.,0.,-1.));
#34959=DIRECTION('ref_axis',(-0.609193695218696,0.793021463584555,0.));
#34960=DIRECTION('',(0.,0.,-1.));
#34961=DIRECTION('center_axis',(0.,0.,-1.));
#34962=DIRECTION('ref_axis',(-0.609193695218696,0.793021463584555,0.));
#34963=DIRECTION('',(0.,0.,-1.));
#34964=DIRECTION('center_axis',(0.,0.,-1.));
#34965=DIRECTION('ref_axis',(-0.609193695218696,0.793021463584555,0.));
#34966=DIRECTION('',(0.,0.,-1.));
#34967=DIRECTION('center_axis',(0.,0.,-1.));
#34968=DIRECTION('ref_axis',(-0.609193695218696,0.793021463584555,0.));
#34969=DIRECTION('',(0.,0.,-1.));
#34970=DIRECTION('center_axis',(0.,0.,-1.));
#34971=DIRECTION('ref_axis',(-0.609193695218696,0.793021463584555,0.));
#34972=DIRECTION('',(0.,0.,-1.));
#34973=DIRECTION('center_axis',(0.,0.,-1.));
#34974=DIRECTION('ref_axis',(-0.609193695218696,0.793021463584555,0.));
#34975=DIRECTION('',(0.,0.,-1.));
#34976=DIRECTION('center_axis',(0.,0.,-1.));
#34977=DIRECTION('ref_axis',(-0.609193695218696,0.793021463584555,0.));
#34978=DIRECTION('',(0.,0.,-1.));
#34979=DIRECTION('center_axis',(0.,0.,-1.));
#34980=DIRECTION('ref_axis',(-0.609193695218696,0.793021463584555,0.));
#34981=DIRECTION('',(0.,0.,-1.));
#34982=DIRECTION('center_axis',(0.,0.,-1.));
#34983=DIRECTION('ref_axis',(-0.609193695218696,0.793021463584555,0.));
#34984=DIRECTION('',(0.,0.,-1.));
#34985=DIRECTION('center_axis',(0.,0.,-1.));
#34986=DIRECTION('ref_axis',(-0.609193695218696,0.793021463584555,0.));
#34987=DIRECTION('',(0.,0.,-1.));
#34988=DIRECTION('center_axis',(0.,0.,-1.));
#34989=DIRECTION('ref_axis',(-0.609193695218696,0.793021463584555,0.));
#34990=DIRECTION('',(0.,0.,-1.));
#34991=DIRECTION('center_axis',(0.,0.,-1.));
#34992=DIRECTION('ref_axis',(-0.609193695218696,0.793021463584555,0.));
#34993=DIRECTION('',(0.,0.,-1.));
#34994=DIRECTION('center_axis',(0.,0.,-1.));
#34995=DIRECTION('ref_axis',(-0.609193695218696,0.793021463584555,0.));
#34996=DIRECTION('',(0.,0.,-1.));
#34997=DIRECTION('center_axis',(0.,0.,-1.));
#34998=DIRECTION('ref_axis',(-0.609193695218696,0.793021463584555,0.));
#34999=DIRECTION('',(0.,0.,-1.));
#35000=DIRECTION('center_axis',(0.,0.,-1.));
#35001=DIRECTION('ref_axis',(-0.609193695218696,0.793021463584555,0.));
#35002=DIRECTION('',(0.,0.,-1.));
#35003=DIRECTION('center_axis',(0.,0.,-1.));
#35004=DIRECTION('ref_axis',(-0.609193695218696,0.793021463584555,0.));
#35005=DIRECTION('',(0.,0.,-1.));
#35006=DIRECTION('center_axis',(0.,0.,-1.));
#35007=DIRECTION('ref_axis',(-0.609193695218696,0.793021463584555,0.));
#35008=DIRECTION('',(0.,0.,-1.));
#35009=DIRECTION('center_axis',(0.,0.,-1.));
#35010=DIRECTION('ref_axis',(-0.609193695218696,0.793021463584555,0.));
#35011=DIRECTION('',(0.,0.,-1.));
#35012=DIRECTION('center_axis',(0.,0.,-1.));
#35013=DIRECTION('ref_axis',(-0.609193695218696,0.793021463584555,0.));
#35014=DIRECTION('',(0.,0.,-1.));
#35015=DIRECTION('center_axis',(0.,0.,-1.));
#35016=DIRECTION('ref_axis',(-0.609193695218696,0.793021463584555,0.));
#35017=DIRECTION('',(0.,0.,-1.));
#35018=DIRECTION('center_axis',(0.,0.,-1.));
#35019=DIRECTION('ref_axis',(-0.609193695218696,0.793021463584555,0.));
#35020=DIRECTION('',(0.,0.,-1.));
#35021=DIRECTION('center_axis',(0.,0.,-1.));
#35022=DIRECTION('ref_axis',(-0.609193695218696,0.793021463584555,0.));
#35023=DIRECTION('',(0.,0.,-1.));
#35024=DIRECTION('center_axis',(0.,0.,-1.));
#35025=DIRECTION('ref_axis',(-0.609193695218696,0.793021463584555,0.));
#35026=DIRECTION('',(0.,0.,-1.));
#35027=DIRECTION('center_axis',(0.,0.,-1.));
#35028=DIRECTION('ref_axis',(-0.609193695218696,0.793021463584555,0.));
#35029=DIRECTION('',(0.,0.,-1.));
#35030=DIRECTION('center_axis',(0.,0.,-1.));
#35031=DIRECTION('ref_axis',(-0.609193695218696,0.793021463584555,0.));
#35032=DIRECTION('',(0.,0.,-1.));
#35033=DIRECTION('center_axis',(0.,0.,-1.));
#35034=DIRECTION('ref_axis',(-0.609193695218696,0.793021463584555,0.));
#35035=DIRECTION('',(0.,0.,-1.));
#35036=DIRECTION('center_axis',(-1.,0.,0.));
#35037=DIRECTION('ref_axis',(0.,0.,-1.));
#35038=DIRECTION('',(-1.,0.,0.));
#35039=DIRECTION('center_axis',(1.,0.,0.));
#35040=DIRECTION('ref_axis',(0.,0.,-1.));
#35041=DIRECTION('center_axis',(-1.,0.,0.));
#35042=DIRECTION('ref_axis',(0.,0.,-1.));
#35043=DIRECTION('',(-1.,0.,0.));
#35044=DIRECTION('center_axis',(1.,0.,0.));
#35045=DIRECTION('ref_axis',(0.,0.,-1.));
#35046=DIRECTION('center_axis',(-1.,0.,0.));
#35047=DIRECTION('ref_axis',(0.,0.,-1.));
#35048=DIRECTION('',(-1.,0.,0.));
#35049=DIRECTION('center_axis',(-1.,0.,0.));
#35050=DIRECTION('ref_axis',(0.,0.,-1.));
#35051=DIRECTION('',(-1.,0.,0.));
#35052=DIRECTION('center_axis',(-1.,0.,0.));
#35053=DIRECTION('ref_axis',(0.,0.,-1.));
#35054=DIRECTION('',(-1.,0.,0.));
#35055=DIRECTION('center_axis',(-1.,0.,0.));
#35056=DIRECTION('ref_axis',(0.,0.,-1.));
#35057=DIRECTION('center_axis',(-1.,0.,0.));
#35058=DIRECTION('ref_axis',(0.,0.,-1.));
#35059=DIRECTION('',(-1.,0.,0.));
#35060=DIRECTION('center_axis',(-1.,0.,0.));
#35061=DIRECTION('ref_axis',(0.,0.,-1.));
#35062=DIRECTION('',(-1.,0.,0.));
#35063=DIRECTION('center_axis',(-1.,0.,0.));
#35064=DIRECTION('ref_axis',(0.,0.,-1.));
#35065=DIRECTION('',(-1.,0.,0.));
#35066=DIRECTION('center_axis',(-1.,0.,0.));
#35067=DIRECTION('ref_axis',(0.,0.,-1.));
#35068=DIRECTION('center_axis',(0.,0.,-1.));
#35069=DIRECTION('ref_axis',(0.939338957847042,-0.34299026556279,0.));
#35070=DIRECTION('',(0.,0.,-1.));
#35071=DIRECTION('center_axis',(0.,0.,1.));
#35072=DIRECTION('ref_axis',(1.,0.,0.));
#35073=DIRECTION('center_axis',(0.,0.,-1.));
#35074=DIRECTION('ref_axis',(0.939338957847042,-0.34299026556279,0.));
#35075=DIRECTION('',(0.,0.,-1.));
#35076=DIRECTION('center_axis',(0.,0.,-1.));
#35077=DIRECTION('ref_axis',(0.939338957847042,-0.34299026556279,0.));
#35078=DIRECTION('',(0.,0.,-1.));
#35079=DIRECTION('center_axis',(0.,0.,-1.));
#35080=DIRECTION('ref_axis',(0.939338957847042,-0.34299026556279,0.));
#35081=DIRECTION('',(0.,0.,-1.));
#35082=DIRECTION('center_axis',(0.,0.,-1.));
#35083=DIRECTION('ref_axis',(0.939338957847042,-0.34299026556279,0.));
#35084=DIRECTION('',(0.,0.,-1.));
#35085=DIRECTION('center_axis',(0.,0.,-1.));
#35086=DIRECTION('ref_axis',(0.939338957847042,-0.34299026556279,0.));
#35087=DIRECTION('',(0.,0.,-1.));
#35088=DIRECTION('center_axis',(0.,0.,-1.));
#35089=DIRECTION('ref_axis',(0.939338957847042,-0.34299026556279,0.));
#35090=DIRECTION('',(0.,0.,-1.));
#35091=DIRECTION('center_axis',(0.,0.,-1.));
#35092=DIRECTION('ref_axis',(0.939338957847042,-0.34299026556279,0.));
#35093=DIRECTION('',(0.,0.,-1.));
#35094=DIRECTION('center_axis',(0.,0.,-1.));
#35095=DIRECTION('ref_axis',(0.939338957847042,-0.34299026556279,0.));
#35096=DIRECTION('',(0.,0.,-1.));
#35097=DIRECTION('center_axis',(0.,0.,-1.));
#35098=DIRECTION('ref_axis',(0.939338957847042,-0.34299026556279,0.));
#35099=DIRECTION('',(0.,0.,-1.));
#35100=DIRECTION('center_axis',(0.,0.,-1.));
#35101=DIRECTION('ref_axis',(0.939338957847042,-0.34299026556279,0.));
#35102=DIRECTION('',(0.,0.,-1.));
#35103=DIRECTION('center_axis',(0.,0.,-1.));
#35104=DIRECTION('ref_axis',(0.939338957847042,-0.34299026556279,0.));
#35105=DIRECTION('',(0.,0.,-1.));
#35106=DIRECTION('center_axis',(0.,0.,-1.));
#35107=DIRECTION('ref_axis',(0.939338957847042,-0.34299026556279,0.));
#35108=DIRECTION('',(0.,0.,-1.));
#35109=DIRECTION('center_axis',(0.,0.,-1.));
#35110=DIRECTION('ref_axis',(0.939338957847042,-0.34299026556279,0.));
#35111=DIRECTION('',(0.,0.,-1.));
#35112=DIRECTION('center_axis',(0.,0.,-1.));
#35113=DIRECTION('ref_axis',(0.939338957847042,-0.34299026556279,0.));
#35114=DIRECTION('',(0.,0.,-1.));
#35115=DIRECTION('center_axis',(0.,0.,-1.));
#35116=DIRECTION('ref_axis',(0.939338957847042,-0.34299026556279,0.));
#35117=DIRECTION('',(0.,0.,-1.));
#35118=DIRECTION('center_axis',(0.,0.,-1.));
#35119=DIRECTION('ref_axis',(0.939338957847042,-0.34299026556279,0.));
#35120=DIRECTION('',(0.,0.,-1.));
#35121=DIRECTION('center_axis',(0.,0.,-1.));
#35122=DIRECTION('ref_axis',(0.939338957847042,-0.34299026556279,0.));
#35123=DIRECTION('',(0.,0.,-1.));
#35124=DIRECTION('center_axis',(0.,0.,-1.));
#35125=DIRECTION('ref_axis',(0.939338957847042,-0.34299026556279,0.));
#35126=DIRECTION('',(0.,0.,-1.));
#35127=DIRECTION('center_axis',(0.,0.,-1.));
#35128=DIRECTION('ref_axis',(0.939338957847042,-0.34299026556279,0.));
#35129=DIRECTION('',(0.,0.,-1.));
#35130=DIRECTION('center_axis',(0.,0.,-1.));
#35131=DIRECTION('ref_axis',(0.939338957847042,-0.34299026556279,0.));
#35132=DIRECTION('',(0.,0.,-1.));
#35133=DIRECTION('center_axis',(0.,0.,-1.));
#35134=DIRECTION('ref_axis',(0.939338957847042,-0.34299026556279,0.));
#35135=DIRECTION('',(0.,0.,-1.));
#35136=DIRECTION('center_axis',(0.,0.,-1.));
#35137=DIRECTION('ref_axis',(0.939338957847042,-0.34299026556279,0.));
#35138=DIRECTION('',(0.,0.,-1.));
#35139=DIRECTION('center_axis',(0.,0.,-1.));
#35140=DIRECTION('ref_axis',(0.939338957847042,-0.34299026556279,0.));
#35141=DIRECTION('',(0.,0.,-1.));
#35142=DIRECTION('center_axis',(0.,0.,-1.));
#35143=DIRECTION('ref_axis',(0.939338957847042,-0.34299026556279,0.));
#35144=DIRECTION('',(0.,0.,-1.));
#35145=DIRECTION('center_axis',(0.,0.,-1.));
#35146=DIRECTION('ref_axis',(0.939338957847042,-0.34299026556279,0.));
#35147=DIRECTION('',(0.,0.,-1.));
#35148=DIRECTION('center_axis',(0.,0.,-1.));
#35149=DIRECTION('ref_axis',(0.939338957847042,-0.34299026556279,0.));
#35150=DIRECTION('',(0.,0.,-1.));
#35151=DIRECTION('center_axis',(0.,0.,-1.));
#35152=DIRECTION('ref_axis',(0.939338984774712,-0.342990191816636,0.));
#35153=DIRECTION('',(0.,0.,-1.));
#35154=DIRECTION('center_axis',(0.,0.,1.));
#35155=DIRECTION('ref_axis',(1.,0.,0.));
#35156=DIRECTION('center_axis',(0.,0.,-1.));
#35157=DIRECTION('ref_axis',(0.939338984774712,-0.342990191816636,0.));
#35158=DIRECTION('',(0.,0.,-1.));
#35159=DIRECTION('center_axis',(0.,0.,-1.));
#35160=DIRECTION('ref_axis',(0.939338984774712,-0.342990191816636,0.));
#35161=DIRECTION('',(0.,0.,-1.));
#35162=DIRECTION('center_axis',(0.,0.,-1.));
#35163=DIRECTION('ref_axis',(0.939338984774712,-0.342990191816636,0.));
#35164=DIRECTION('',(0.,0.,-1.));
#35165=DIRECTION('center_axis',(0.,0.,-1.));
#35166=DIRECTION('ref_axis',(0.939338984774712,-0.342990191816636,0.));
#35167=DIRECTION('',(0.,0.,-1.));
#35168=DIRECTION('center_axis',(0.,0.,-1.));
#35169=DIRECTION('ref_axis',(0.939338984774712,-0.342990191816636,0.));
#35170=DIRECTION('',(0.,0.,-1.));
#35171=DIRECTION('center_axis',(0.,0.,-1.));
#35172=DIRECTION('ref_axis',(0.939338984774712,-0.342990191816636,0.));
#35173=DIRECTION('',(0.,0.,-1.));
#35174=DIRECTION('center_axis',(0.,0.,-1.));
#35175=DIRECTION('ref_axis',(0.939338984774712,-0.342990191816636,0.));
#35176=DIRECTION('',(0.,0.,-1.));
#35177=DIRECTION('center_axis',(0.,0.,-1.));
#35178=DIRECTION('ref_axis',(0.939338984774712,-0.342990191816636,0.));
#35179=DIRECTION('',(0.,0.,-1.));
#35180=DIRECTION('center_axis',(0.,0.,-1.));
#35181=DIRECTION('ref_axis',(0.939338984774712,-0.342990191816636,0.));
#35182=DIRECTION('',(0.,0.,-1.));
#35183=DIRECTION('center_axis',(0.,0.,-1.));
#35184=DIRECTION('ref_axis',(0.939338984774712,-0.342990191816636,0.));
#35185=DIRECTION('',(0.,0.,-1.));
#35186=DIRECTION('center_axis',(0.,0.,-1.));
#35187=DIRECTION('ref_axis',(0.939338984774712,-0.342990191816636,0.));
#35188=DIRECTION('',(0.,0.,-1.));
#35189=DIRECTION('center_axis',(0.,0.,-1.));
#35190=DIRECTION('ref_axis',(0.939338984774712,-0.342990191816636,0.));
#35191=DIRECTION('',(0.,0.,-1.));
#35192=DIRECTION('center_axis',(0.,0.,-1.));
#35193=DIRECTION('ref_axis',(0.939338984774712,-0.342990191816636,0.));
#35194=DIRECTION('',(0.,0.,-1.));
#35195=DIRECTION('center_axis',(0.,0.,-1.));
#35196=DIRECTION('ref_axis',(0.939338984774712,-0.342990191816636,0.));
#35197=DIRECTION('',(0.,0.,-1.));
#35198=DIRECTION('center_axis',(0.,0.,-1.));
#35199=DIRECTION('ref_axis',(0.939338984774712,-0.342990191816636,0.));
#35200=DIRECTION('',(0.,0.,-1.));
#35201=DIRECTION('center_axis',(0.,0.,-1.));
#35202=DIRECTION('ref_axis',(0.939338984774712,-0.342990191816636,0.));
#35203=DIRECTION('',(0.,0.,-1.));
#35204=DIRECTION('center_axis',(0.,0.,-1.));
#35205=DIRECTION('ref_axis',(0.939338984774712,-0.342990191816636,0.));
#35206=DIRECTION('',(0.,0.,-1.));
#35207=DIRECTION('center_axis',(0.,0.,-1.));
#35208=DIRECTION('ref_axis',(0.939338984774712,-0.342990191816636,0.));
#35209=DIRECTION('',(0.,0.,-1.));
#35210=DIRECTION('center_axis',(0.,0.,-1.));
#35211=DIRECTION('ref_axis',(0.939338984774712,-0.342990191816636,0.));
#35212=DIRECTION('',(0.,0.,-1.));
#35213=DIRECTION('center_axis',(0.,0.,-1.));
#35214=DIRECTION('ref_axis',(0.939338984774712,-0.342990191816636,0.));
#35215=DIRECTION('',(0.,0.,-1.));
#35216=DIRECTION('center_axis',(0.,0.,-1.));
#35217=DIRECTION('ref_axis',(0.939338984774712,-0.342990191816636,0.));
#35218=DIRECTION('',(0.,0.,-1.));
#35219=DIRECTION('center_axis',(0.,0.,-1.));
#35220=DIRECTION('ref_axis',(0.939338984774712,-0.342990191816636,0.));
#35221=DIRECTION('',(0.,0.,-1.));
#35222=DIRECTION('center_axis',(0.,0.,-1.));
#35223=DIRECTION('ref_axis',(0.939338984774712,-0.342990191816636,0.));
#35224=DIRECTION('',(0.,0.,-1.));
#35225=DIRECTION('center_axis',(0.,0.,-1.));
#35226=DIRECTION('ref_axis',(0.939338984774712,-0.342990191816636,0.));
#35227=DIRECTION('',(0.,0.,-1.));
#35228=DIRECTION('center_axis',(0.,0.,-1.));
#35229=DIRECTION('ref_axis',(0.939338984774712,-0.342990191816636,0.));
#35230=DIRECTION('',(0.,0.,-1.));
#35231=DIRECTION('center_axis',(0.,0.,-1.));
#35232=DIRECTION('ref_axis',(0.939338984774712,-0.342990191816636,0.));
#35233=DIRECTION('',(0.,0.,-1.));
#35234=DIRECTION('center_axis',(0.,0.,-1.));
#35235=DIRECTION('ref_axis',(0.939338988036949,-0.342990182882426,0.));
#35236=DIRECTION('',(0.,0.,-1.));
#35237=DIRECTION('center_axis',(0.,0.,1.));
#35238=DIRECTION('ref_axis',(1.,0.,0.));
#35239=DIRECTION('center_axis',(0.,0.,-1.));
#35240=DIRECTION('ref_axis',(0.939338988036949,-0.342990182882426,0.));
#35241=DIRECTION('',(0.,0.,-1.));
#35242=DIRECTION('center_axis',(0.,0.,-1.));
#35243=DIRECTION('ref_axis',(0.939338988036949,-0.342990182882426,0.));
#35244=DIRECTION('',(0.,0.,-1.));
#35245=DIRECTION('center_axis',(0.,0.,-1.));
#35246=DIRECTION('ref_axis',(0.939338988036949,-0.342990182882426,0.));
#35247=DIRECTION('',(0.,0.,-1.));
#35248=DIRECTION('center_axis',(0.,0.,-1.));
#35249=DIRECTION('ref_axis',(0.939338988036949,-0.342990182882426,0.));
#35250=DIRECTION('',(0.,0.,-1.));
#35251=DIRECTION('center_axis',(0.,0.,-1.));
#35252=DIRECTION('ref_axis',(0.939338988036949,-0.342990182882426,0.));
#35253=DIRECTION('',(0.,0.,-1.));
#35254=DIRECTION('center_axis',(0.,0.,-1.));
#35255=DIRECTION('ref_axis',(0.939338988036949,-0.342990182882426,0.));
#35256=DIRECTION('',(0.,0.,-1.));
#35257=DIRECTION('center_axis',(0.,0.,-1.));
#35258=DIRECTION('ref_axis',(0.939338988036949,-0.342990182882426,0.));
#35259=DIRECTION('',(0.,0.,-1.));
#35260=DIRECTION('center_axis',(0.,0.,-1.));
#35261=DIRECTION('ref_axis',(0.939338988036949,-0.342990182882426,0.));
#35262=DIRECTION('',(0.,0.,-1.));
#35263=DIRECTION('center_axis',(0.,0.,-1.));
#35264=DIRECTION('ref_axis',(0.939338988036949,-0.342990182882426,0.));
#35265=DIRECTION('',(0.,0.,-1.));
#35266=DIRECTION('center_axis',(0.,0.,-1.));
#35267=DIRECTION('ref_axis',(0.939338988036949,-0.342990182882426,0.));
#35268=DIRECTION('',(0.,0.,-1.));
#35269=DIRECTION('center_axis',(0.,0.,-1.));
#35270=DIRECTION('ref_axis',(0.939338988036949,-0.342990182882426,0.));
#35271=DIRECTION('',(0.,0.,-1.));
#35272=DIRECTION('center_axis',(0.,0.,-1.));
#35273=DIRECTION('ref_axis',(0.939338988036949,-0.342990182882426,0.));
#35274=DIRECTION('',(0.,0.,-1.));
#35275=DIRECTION('center_axis',(0.,0.,-1.));
#35276=DIRECTION('ref_axis',(0.939338988036949,-0.342990182882426,0.));
#35277=DIRECTION('',(0.,0.,-1.));
#35278=DIRECTION('center_axis',(0.,0.,-1.));
#35279=DIRECTION('ref_axis',(0.939338988036949,-0.342990182882426,0.));
#35280=DIRECTION('',(0.,0.,-1.));
#35281=DIRECTION('center_axis',(0.,0.,-1.));
#35282=DIRECTION('ref_axis',(0.939338988036949,-0.342990182882426,0.));
#35283=DIRECTION('',(0.,0.,-1.));
#35284=DIRECTION('center_axis',(0.,0.,-1.));
#35285=DIRECTION('ref_axis',(0.939338988036949,-0.342990182882426,0.));
#35286=DIRECTION('',(0.,0.,-1.));
#35287=DIRECTION('center_axis',(0.,0.,-1.));
#35288=DIRECTION('ref_axis',(0.939338988036949,-0.342990182882426,0.));
#35289=DIRECTION('',(0.,0.,-1.));
#35290=DIRECTION('center_axis',(0.,0.,-1.));
#35291=DIRECTION('ref_axis',(0.939338988036949,-0.342990182882426,0.));
#35292=DIRECTION('',(0.,0.,-1.));
#35293=DIRECTION('center_axis',(0.,0.,-1.));
#35294=DIRECTION('ref_axis',(0.939338988036949,-0.342990182882426,0.));
#35295=DIRECTION('',(0.,0.,-1.));
#35296=DIRECTION('center_axis',(0.,0.,-1.));
#35297=DIRECTION('ref_axis',(0.939338988036949,-0.342990182882426,0.));
#35298=DIRECTION('',(0.,0.,-1.));
#35299=DIRECTION('center_axis',(0.,0.,-1.));
#35300=DIRECTION('ref_axis',(0.939338988036949,-0.342990182882426,0.));
#35301=DIRECTION('',(0.,0.,-1.));
#35302=DIRECTION('center_axis',(0.,0.,-1.));
#35303=DIRECTION('ref_axis',(0.939338988036949,-0.342990182882426,0.));
#35304=DIRECTION('',(0.,0.,-1.));
#35305=DIRECTION('center_axis',(0.,0.,-1.));
#35306=DIRECTION('ref_axis',(0.939338988036949,-0.342990182882426,0.));
#35307=DIRECTION('',(0.,0.,-1.));
#35308=DIRECTION('center_axis',(0.,0.,-1.));
#35309=DIRECTION('ref_axis',(0.939338988036949,-0.342990182882426,0.));
#35310=DIRECTION('',(0.,0.,-1.));
#35311=DIRECTION('center_axis',(0.,0.,-1.));
#35312=DIRECTION('ref_axis',(0.939338988036949,-0.342990182882426,0.));
#35313=DIRECTION('',(0.,0.,-1.));
#35314=DIRECTION('center_axis',(0.,0.,-1.));
#35315=DIRECTION('ref_axis',(0.939338988036949,-0.342990182882426,0.));
#35316=DIRECTION('',(0.,0.,-1.));
#35317=DIRECTION('center_axis',(0.,0.,-1.));
#35318=DIRECTION('ref_axis',(0.939338973287599,-0.342990223276114,0.));
#35319=DIRECTION('',(0.,0.,-1.));
#35320=DIRECTION('center_axis',(0.,0.,1.));
#35321=DIRECTION('ref_axis',(1.,0.,0.));
#35322=DIRECTION('center_axis',(0.,0.,-1.));
#35323=DIRECTION('ref_axis',(0.939338973287599,-0.342990223276114,0.));
#35324=DIRECTION('',(0.,0.,-1.));
#35325=DIRECTION('center_axis',(0.,0.,-1.));
#35326=DIRECTION('ref_axis',(0.939338973287599,-0.342990223276114,0.));
#35327=DIRECTION('',(0.,0.,-1.));
#35328=DIRECTION('center_axis',(0.,0.,-1.));
#35329=DIRECTION('ref_axis',(0.939338973287599,-0.342990223276114,0.));
#35330=DIRECTION('',(0.,0.,-1.));
#35331=DIRECTION('center_axis',(0.,0.,-1.));
#35332=DIRECTION('ref_axis',(0.939338973287599,-0.342990223276114,0.));
#35333=DIRECTION('',(0.,0.,-1.));
#35334=DIRECTION('center_axis',(0.,0.,-1.));
#35335=DIRECTION('ref_axis',(0.939338973287599,-0.342990223276114,0.));
#35336=DIRECTION('',(0.,0.,-1.));
#35337=DIRECTION('center_axis',(0.,0.,-1.));
#35338=DIRECTION('ref_axis',(0.939338973287599,-0.342990223276114,0.));
#35339=DIRECTION('',(0.,0.,-1.));
#35340=DIRECTION('center_axis',(0.,0.,-1.));
#35341=DIRECTION('ref_axis',(0.939338973287599,-0.342990223276114,0.));
#35342=DIRECTION('',(0.,0.,-1.));
#35343=DIRECTION('center_axis',(0.,0.,-1.));
#35344=DIRECTION('ref_axis',(0.939338973287599,-0.342990223276114,0.));
#35345=DIRECTION('',(0.,0.,-1.));
#35346=DIRECTION('center_axis',(0.,0.,-1.));
#35347=DIRECTION('ref_axis',(0.939338973287599,-0.342990223276114,0.));
#35348=DIRECTION('',(0.,0.,-1.));
#35349=DIRECTION('center_axis',(0.,0.,-1.));
#35350=DIRECTION('ref_axis',(0.939338973287599,-0.342990223276114,0.));
#35351=DIRECTION('',(0.,0.,-1.));
#35352=DIRECTION('center_axis',(0.,0.,-1.));
#35353=DIRECTION('ref_axis',(0.939338973287599,-0.342990223276114,0.));
#35354=DIRECTION('',(0.,0.,-1.));
#35355=DIRECTION('center_axis',(0.,0.,-1.));
#35356=DIRECTION('ref_axis',(0.939338973287599,-0.342990223276114,0.));
#35357=DIRECTION('',(0.,0.,-1.));
#35358=DIRECTION('center_axis',(0.,0.,-1.));
#35359=DIRECTION('ref_axis',(0.939338973287599,-0.342990223276114,0.));
#35360=DIRECTION('',(0.,0.,-1.));
#35361=DIRECTION('center_axis',(0.,0.,-1.));
#35362=DIRECTION('ref_axis',(0.939338973287599,-0.342990223276114,0.));
#35363=DIRECTION('',(0.,0.,-1.));
#35364=DIRECTION('center_axis',(0.,0.,-1.));
#35365=DIRECTION('ref_axis',(0.939338973287599,-0.342990223276114,0.));
#35366=DIRECTION('',(0.,0.,-1.));
#35367=DIRECTION('center_axis',(0.,0.,-1.));
#35368=DIRECTION('ref_axis',(0.939338973287599,-0.342990223276114,0.));
#35369=DIRECTION('',(0.,0.,-1.));
#35370=DIRECTION('center_axis',(0.,0.,-1.));
#35371=DIRECTION('ref_axis',(0.939338973287599,-0.342990223276114,0.));
#35372=DIRECTION('',(0.,0.,-1.));
#35373=DIRECTION('center_axis',(0.,0.,-1.));
#35374=DIRECTION('ref_axis',(0.939338973287599,-0.342990223276114,0.));
#35375=DIRECTION('',(0.,0.,-1.));
#35376=DIRECTION('center_axis',(0.,0.,-1.));
#35377=DIRECTION('ref_axis',(0.939338973287599,-0.342990223276114,0.));
#35378=DIRECTION('',(0.,0.,-1.));
#35379=DIRECTION('center_axis',(0.,0.,-1.));
#35380=DIRECTION('ref_axis',(0.939338973287599,-0.342990223276114,0.));
#35381=DIRECTION('',(0.,0.,-1.));
#35382=DIRECTION('center_axis',(0.,0.,-1.));
#35383=DIRECTION('ref_axis',(0.939338973287599,-0.342990223276114,0.));
#35384=DIRECTION('',(0.,0.,-1.));
#35385=DIRECTION('center_axis',(0.,0.,-1.));
#35386=DIRECTION('ref_axis',(0.939338973287599,-0.342990223276114,0.));
#35387=DIRECTION('',(0.,0.,-1.));
#35388=DIRECTION('center_axis',(0.,0.,-1.));
#35389=DIRECTION('ref_axis',(0.939338973287599,-0.342990223276114,0.));
#35390=DIRECTION('',(0.,0.,-1.));
#35391=DIRECTION('center_axis',(0.,0.,-1.));
#35392=DIRECTION('ref_axis',(0.939338973287599,-0.342990223276114,0.));
#35393=DIRECTION('',(0.,0.,-1.));
#35394=DIRECTION('center_axis',(0.,0.,-1.));
#35395=DIRECTION('ref_axis',(0.939338973287599,-0.342990223276114,0.));
#35396=DIRECTION('',(0.,0.,-1.));
#35397=DIRECTION('center_axis',(0.,0.,-1.));
#35398=DIRECTION('ref_axis',(0.939338973287599,-0.342990223276114,0.));
#35399=DIRECTION('',(0.,0.,-1.));
#35400=DIRECTION('center_axis',(0.,0.,-1.));
#35401=DIRECTION('ref_axis',(0.939338973287599,-0.342990223276114,0.));
#35402=DIRECTION('center_axis',(0.,0.,1.));
#35403=DIRECTION('ref_axis',(1.,0.,0.));
#35404=DIRECTION('center_axis',(0.,0.,-1.));
#35405=DIRECTION('ref_axis',(0.939338988036949,-0.342990182882426,0.));
#35406=DIRECTION('center_axis',(0.,0.,1.));
#35407=DIRECTION('ref_axis',(1.,0.,0.));
#35408=DIRECTION('center_axis',(0.,0.,-1.));
#35409=DIRECTION('ref_axis',(0.939338984774712,-0.342990191816636,0.));
#35410=DIRECTION('center_axis',(0.,0.,1.));
#35411=DIRECTION('ref_axis',(1.,0.,0.));
#35412=DIRECTION('center_axis',(0.,0.,-1.));
#35413=DIRECTION('ref_axis',(0.939338957847042,-0.34299026556279,0.));
#35414=DIRECTION('center_axis',(0.,0.,1.));
#35415=DIRECTION('ref_axis',(1.,0.,0.));
#35416=DIRECTION('center_axis',(-1.,0.,0.));
#35417=DIRECTION('ref_axis',(0.,0.,-1.));
#35418=DIRECTION('center_axis',(-1.,0.,0.));
#35419=DIRECTION('ref_axis',(0.,0.,-1.));
#35420=DIRECTION('center_axis',(-1.,0.,0.));
#35421=DIRECTION('ref_axis',(0.,0.,-1.));
#35422=DIRECTION('center_axis',(1.,0.,0.));
#35423=DIRECTION('ref_axis',(0.,0.,-1.));
#35424=DIRECTION('center_axis',(0.,0.,-1.));
#35425=DIRECTION('ref_axis',(-0.609193695218696,0.793021463584555,0.));
#35426=DIRECTION('center_axis',(0.,0.,1.));
#35427=DIRECTION('ref_axis',(1.,7.89299181569448E-14,0.));
#35428=DIRECTION('center_axis',(0.,0.,-1.));
#35429=DIRECTION('ref_axis',(-0.609193651103488,0.793021497473556,0.));
#35430=DIRECTION('center_axis',(0.,0.,1.));
#35431=DIRECTION('ref_axis',(1.,7.80625564189562E-14,0.));
#35432=DIRECTION('center_axis',(0.,0.,-1.));
#35433=DIRECTION('ref_axis',(-0.609193645039877,0.793021502131581,0.));
#35434=DIRECTION('center_axis',(0.,0.,1.));
#35435=DIRECTION('ref_axis',(1.,8.15320033709099E-14,0.));
#35436=DIRECTION('center_axis',(0.,0.,-1.));
#35437=DIRECTION('ref_axis',(-0.609193659724225,0.793021490851165,0.));
#35438=DIRECTION('center_axis',(0.,0.,1.));
#35439=DIRECTION('ref_axis',(1.,8.06646416329218E-14,0.));
#35440=DIRECTION('center_axis',(1.,0.,0.));
#35441=DIRECTION('ref_axis',(0.,-0.878663231892279,-0.477442064465015));
#35442=DIRECTION('center_axis',(-1.,0.,0.));
#35443=DIRECTION('ref_axis',(0.,-1.74186785585433E-15,-1.));
#35444=DIRECTION('center_axis',(-1.,0.,0.));
#35445=DIRECTION('ref_axis',(0.,0.878663232865503,-0.477442062673936));
#35446=DIRECTION('center_axis',(1.,0.,0.));
#35447=DIRECTION('ref_axis',(0.,-1.74186785585433E-15,-1.));
#35448=DIRECTION('center_axis',(0.,0.,1.));
#35449=DIRECTION('ref_axis',(1.,0.,0.));
#35450=DIRECTION('center_axis',(0.,0.,1.));
#35451=DIRECTION('ref_axis',(1.,0.,0.));
#35452=DIRECTION('',(0.,0.,1.));
#35453=DIRECTION('center_axis',(0.,0.,1.));
#35454=DIRECTION('ref_axis',(1.,0.,0.));
#35455=DIRECTION('center_axis',(0.,0.,-1.));
#35456=DIRECTION('ref_axis',(-1.,0.,0.));
#35457=DIRECTION('center_axis',(0.,0.,1.));
#35458=DIRECTION('ref_axis',(1.,0.,0.));
#35459=DIRECTION('center_axis',(0.,0.,1.));
#35460=DIRECTION('ref_axis',(1.,0.,0.));
#35461=DIRECTION('',(0.,0.,-1.));
#35462=DIRECTION('center_axis',(0.,0.,1.));
#35463=DIRECTION('ref_axis',(1.,0.,0.));
#35464=DIRECTION('',(0.,0.,1.));
#35465=DIRECTION('center_axis',(0.,0.,-1.));
#35466=DIRECTION('ref_axis',(-1.,0.,0.));
#35467=DIRECTION('',(0.,-1.,0.));
#35468=DIRECTION('center_axis',(0.,0.,1.));
#35469=DIRECTION('ref_axis',(-0.374029024133323,0.927416998499529,0.));
#35470=DIRECTION('',(0.,-1.,0.));
#35471=DIRECTION('',(-1.,0.,0.));
#35472=DIRECTION('center_axis',(0.,0.,1.));
#35473=DIRECTION('ref_axis',(1.,0.,0.));
#35474=DIRECTION('center_axis',(0.,0.,1.));
#35475=DIRECTION('ref_axis',(1.,0.,0.));
#35476=DIRECTION('',(0.,0.,1.));
#35477=DIRECTION('center_axis',(0.,0.,1.));
#35478=DIRECTION('ref_axis',(1.,0.,0.));
#35479=DIRECTION('center_axis',(0.,0.,-1.));
#35480=DIRECTION('ref_axis',(-1.,0.,0.));
#35481=DIRECTION('center_axis',(0.,0.,1.));
#35482=DIRECTION('ref_axis',(-0.873226700271574,-0.487314200421882,0.));
#35483=DIRECTION('center_axis',(0.,0.,1.));
#35484=DIRECTION('ref_axis',(1.,0.,0.));
#35485=DIRECTION('',(0.,0.,-1.));
#35486=DIRECTION('center_axis',(0.,0.,1.));
#35487=DIRECTION('ref_axis',(1.,0.,0.));
#35488=DIRECTION('',(0.,0.,1.));
#35489=DIRECTION('center_axis',(0.,0.,-1.));
#35490=DIRECTION('ref_axis',(-1.,0.,0.));
#35491=DIRECTION('',(0.,1.,0.));
#35492=DIRECTION('center_axis',(0.,0.,1.));
#35493=DIRECTION('ref_axis',(0.914708142118334,0.404115100859181,0.));
#35494=DIRECTION('',(0.,1.,0.));
#35495=DIRECTION('',(-1.,0.,0.));
#35496=DIRECTION('center_axis',(0.,0.,1.));
#35497=DIRECTION('ref_axis',(1.,0.,0.));
#35498=DIRECTION('center_axis',(0.,0.,1.));
#35499=DIRECTION('ref_axis',(1.,0.,0.));
#35500=DIRECTION('',(0.,0.,1.));
#35501=DIRECTION('center_axis',(0.,0.,1.));
#35502=DIRECTION('ref_axis',(1.,0.,0.));
#35503=DIRECTION('center_axis',(0.,0.,-1.));
#35504=DIRECTION('ref_axis',(-1.,0.,0.));
#35505=DIRECTION('center_axis',(1.,0.,0.));
#35506=DIRECTION('ref_axis',(0.,1.,0.));
#35507=DIRECTION('',(0.,0.,1.));
#35508=DIRECTION('',(0.,1.,0.));
#35509=DIRECTION('',(0.,0.,1.));
#35510=DIRECTION('center_axis',(-1.,0.,0.));
#35511=DIRECTION('ref_axis',(0.,-1.,0.));
#35512=DIRECTION('',(0.,0.,1.));
#35513=DIRECTION('',(0.,1.,0.));
#35514=DIRECTION('',(0.,0.,1.));
#35515=DIRECTION('',(0.,-1.,0.));
#35516=DIRECTION('center_axis',(0.,-1.,0.));
#35517=DIRECTION('ref_axis',(1.,0.,0.));
#35518=DIRECTION('',(-1.,0.,0.));
#35519=DIRECTION('',(0.,0.,1.));
#35520=DIRECTION('',(1.,0.,0.));
#35521=DIRECTION('center_axis',(0.,0.,1.));
#35522=DIRECTION('ref_axis',(1.,0.,0.));
#35523=DIRECTION('center_axis',(0.,0.,1.));
#35524=DIRECTION('ref_axis',(0.,1.,0.));
#35525=DIRECTION('',(-1.,0.,0.));
#35526=DIRECTION('center_axis',(0.,0.,-1.));
#35527=DIRECTION('ref_axis',(0.,-1.,0.));
#35528=DIRECTION('',(0.,-1.,0.));
#35529=DIRECTION('center_axis',(0.,0.,-1.));
#35530=DIRECTION('ref_axis',(1.,0.,0.));
#35531=DIRECTION('',(0.987070639057186,0.160285849379284,0.));
#35532=DIRECTION('center_axis',(0.,0.,-1.));
#35533=DIRECTION('ref_axis',(0.,1.,0.));
#35534=DIRECTION('',(0.,1.,0.));
#35535=DIRECTION('',(-1.,0.,0.));
#35536=DIRECTION('',(0.,1.,0.));
#35537=DIRECTION('',(1.,0.,0.));
#35538=DIRECTION('',(0.,1.,0.));
#35539=DIRECTION('center_axis',(0.,0.,-1.));
#35540=DIRECTION('ref_axis',(-1.,0.,0.));
#35541=DIRECTION('',(-1.,3.69197497485193E-16,0.));
#35542=DIRECTION('center_axis',(0.,0.,-1.));
#35543=DIRECTION('ref_axis',(0.,-1.,0.));
#35544=DIRECTION('',(0.,-1.,0.));
#35545=DIRECTION('',(1.,0.,0.));
#35546=DIRECTION('',(0.,-1.,0.));
#35547=DIRECTION('',(-1.,0.,0.));
#35548=DIRECTION('',(0.,-1.,0.));
#35549=DIRECTION('center_axis',(0.,0.,-1.));
#35550=DIRECTION('ref_axis',(1.,4.44089209850062E-16,0.));
#35551=DIRECTION('',(0.987070639057186,-0.160285849379284,0.));
#35552=DIRECTION('center_axis',(0.,0.,-1.));
#35553=DIRECTION('ref_axis',(0.,1.,0.));
#35554=DIRECTION('',(0.,1.,0.));
#35555=DIRECTION('center_axis',(0.,0.,-1.));
#35556=DIRECTION('ref_axis',(-1.,0.,0.));
#35557=DIRECTION('',(-1.,0.,0.));
#35558=DIRECTION('center_axis',(0.,0.,1.));
#35559=DIRECTION('ref_axis',(1.,0.,0.));
#35560=DIRECTION('',(0.,1.,0.));
#35561=DIRECTION('center_axis',(0.,0.,1.));
#35562=DIRECTION('ref_axis',(1.,0.,0.));
#35563=DIRECTION('center_axis',(0.,0.,1.));
#35564=DIRECTION('ref_axis',(1.,0.,0.));
#35565=DIRECTION('center_axis',(0.,0.,1.));
#35566=DIRECTION('ref_axis',(0.,1.,0.));
#35567=DIRECTION('',(0.,-1.,0.));
#35568=DIRECTION('',(-1.,0.,0.));
#35569=DIRECTION('',(0.,1.,0.));
#35570=DIRECTION('',(-1.,0.,0.));
#35571=DIRECTION('center_axis',(0.,1.,0.));
#35572=DIRECTION('ref_axis',(0.,0.,-1.));
#35573=DIRECTION('',(0.,0.,1.));
#35574=DIRECTION('',(-1.,0.,0.));
#35575=DIRECTION('',(0.,0.,-1.));
#35576=DIRECTION('center_axis',(0.,0.,1.));
#35577=DIRECTION('ref_axis',(0.,1.,0.));
#35578=DIRECTION('',(0.,-1.,0.));
#35579=DIRECTION('',(-1.,0.,0.));
#35580=DIRECTION('',(0.,1.,0.));
#35581=DIRECTION('center_axis',(0.,0.894427190999916,-0.447213595499957));
#35582=DIRECTION('ref_axis',(0.,-0.447213595499957,-0.894427190999916));
#35583=DIRECTION('',(0.,0.447213595499957,0.894427190999916));
#35584=DIRECTION('',(-1.,0.,0.));
#35585=DIRECTION('',(0.,-0.447213595499957,-0.894427190999916));
#35586=DIRECTION('center_axis',(0.,-0.894427190999916,-0.447213595499957));
#35587=DIRECTION('ref_axis',(0.,-0.447213595499957,0.894427190999916));
#35588=DIRECTION('',(0.,0.447213595499957,-0.894427190999916));
#35589=DIRECTION('',(-1.,0.,0.));
#35590=DIRECTION('',(0.,-0.447213595499957,0.894427190999916));
#35591=DIRECTION('center_axis',(0.,0.,1.));
#35592=DIRECTION('ref_axis',(0.,1.,0.));
#35593=DIRECTION('',(0.,-1.,0.));
#35594=DIRECTION('',(-1.,0.,0.));
#35595=DIRECTION('',(0.,1.,0.));
#35596=DIRECTION('center_axis',(0.,-1.,0.));
#35597=DIRECTION('ref_axis',(0.,0.,1.));
#35598=DIRECTION('',(0.,0.,-1.));
#35599=DIRECTION('',(0.,0.,1.));
#35600=DIRECTION('center_axis',(-1.,0.,0.));
#35601=DIRECTION('ref_axis',(0.,0.,-1.));
#35602=DIRECTION('center_axis',(1.,0.,0.));
#35603=DIRECTION('ref_axis',(0.,0.,-1.));
#35604=DIRECTION('',(-1.,0.,0.));
#35605=DIRECTION('center_axis',(-1.,0.,0.));
#35606=DIRECTION('ref_axis',(0.,0.,-1.));
#35607=DIRECTION('center_axis',(1.,0.,0.));
#35608=DIRECTION('ref_axis',(0.,0.,-1.));
#35609=DIRECTION('center_axis',(-1.,0.,0.));
#35610=DIRECTION('ref_axis',(0.,-0.912870929175277,-0.408248290463863));
#35611=DIRECTION('center_axis',(1.,0.,0.));
#35612=DIRECTION('ref_axis',(0.,0.,-1.));
#35613=DIRECTION('',(-1.,0.,0.));
#35614=DIRECTION('center_axis',(-1.,0.,0.));
#35615=DIRECTION('ref_axis',(0.,0.,-1.));
#35616=DIRECTION('',(-1.,0.,0.));
#35617=DIRECTION('center_axis',(0.,0.,-1.));
#35618=DIRECTION('ref_axis',(0.,-1.,0.));
#35619=DIRECTION('',(0.,1.,0.));
#35620=DIRECTION('',(-1.,0.,0.));
#35621=DIRECTION('',(0.,-1.,0.));
#35622=DIRECTION('center_axis',(-1.,0.,0.));
#35623=DIRECTION('ref_axis',(0.,0.912870929175277,-0.408248290463863));
#35624=DIRECTION('center_axis',(1.,0.,0.));
#35625=DIRECTION('ref_axis',(0.,0.,-1.));
#35626=DIRECTION('',(-1.,0.,0.));
#35627=DIRECTION('center_axis',(-1.,0.,0.));
#35628=DIRECTION('ref_axis',(0.,0.,-1.));
#35629=DIRECTION('center_axis',(0.,1.,0.));
#35630=DIRECTION('ref_axis',(0.,0.,-1.));
#35631=DIRECTION('',(0.,0.,1.));
#35632=DIRECTION('',(0.,0.,-1.));
#35633=DIRECTION('center_axis',(0.,-1.,0.));
#35634=DIRECTION('ref_axis',(0.,0.,1.));
#35635=DIRECTION('',(0.,0.,-1.));
#35636=DIRECTION('',(0.,0.,1.));
#35637=DIRECTION('center_axis',(1.,0.,0.));
#35638=DIRECTION('ref_axis',(0.,0.,-1.));
#35639=DIRECTION('center_axis',(-1.,0.,0.));
#35640=DIRECTION('ref_axis',(0.,0.,-1.));
#35641=DIRECTION('center_axis',(-1.,0.,0.));
#35642=DIRECTION('ref_axis',(0.,0.,-1.));
#35643=DIRECTION('center_axis',(0.,-1.,0.));
#35644=DIRECTION('ref_axis',(0.,0.,1.));
#35645=DIRECTION('',(0.,0.,-1.));
#35646=DIRECTION('',(-1.,0.,0.));
#35647=DIRECTION('',(0.,0.,1.));
#35648=DIRECTION('',(-1.,0.,0.));
#35649=DIRECTION('center_axis',(0.,0.,-1.));
#35650=DIRECTION('ref_axis',(0.,-1.,0.));
#35651=DIRECTION('',(0.,1.,0.));
#35652=DIRECTION('',(-1.,0.,0.));
#35653=DIRECTION('',(0.,-1.,0.));
#35654=DIRECTION('center_axis',(0.,-0.894427190999916,0.447213595499958));
#35655=DIRECTION('ref_axis',(0.,0.447213595499958,0.894427190999916));
#35656=DIRECTION('',(0.,-0.447213595499958,-0.894427190999916));
#35657=DIRECTION('',(-1.,0.,0.));
#35658=DIRECTION('',(0.,0.447213595499958,0.894427190999916));
#35659=DIRECTION('center_axis',(0.,0.894427190999916,0.447213595499958));
#35660=DIRECTION('ref_axis',(0.,0.447213595499958,-0.894427190999916));
#35661=DIRECTION('',(0.,-0.447213595499958,0.894427190999916));
#35662=DIRECTION('',(-1.,0.,0.));
#35663=DIRECTION('',(0.,0.447213595499958,-0.894427190999916));
#35664=DIRECTION('center_axis',(0.,0.,-1.));
#35665=DIRECTION('ref_axis',(0.,-1.,0.));
#35666=DIRECTION('',(0.,1.,0.));
#35667=DIRECTION('',(-1.,0.,0.));
#35668=DIRECTION('',(0.,-1.,0.));
#35669=DIRECTION('center_axis',(0.,1.,0.));
#35670=DIRECTION('ref_axis',(0.,0.,-1.));
#35671=DIRECTION('',(0.,0.,1.));
#35672=DIRECTION('',(-1.,0.,0.));
#35673=DIRECTION('',(0.,0.,-1.));
#35674=DIRECTION('center_axis',(0.,0.,-1.));
#35675=DIRECTION('ref_axis',(0.,-1.,0.));
#35676=DIRECTION('',(0.,1.,0.));
#35677=DIRECTION('',(0.,-1.,0.));
#35678=DIRECTION('center_axis',(-1.,0.,0.));
#35679=DIRECTION('ref_axis',(0.,0.,-1.));
#35680=DIRECTION('center_axis',(1.,0.,0.));
#35681=DIRECTION('ref_axis',(0.,0.,-1.));
#35682=DIRECTION('',(-1.,0.,0.));
#35683=DIRECTION('center_axis',(-1.,0.,0.));
#35684=DIRECTION('ref_axis',(0.,0.,-1.));
#35685=DIRECTION('center_axis',(1.,0.,0.));
#35686=DIRECTION('ref_axis',(0.,0.,-1.));
#35687=DIRECTION('center_axis',(-1.,0.,0.));
#35688=DIRECTION('ref_axis',(0.,-1.,0.));
#35689=DIRECTION('center_axis',(-1.,0.,0.));
#35690=DIRECTION('ref_axis',(0.,-1.,0.));
#35691=DIRECTION('center_axis',(-1.,0.,0.));
#35692=DIRECTION('ref_axis',(0.,0.,-1.));
#35693=DIRECTION('',(-1.,0.,0.));
#35694=DIRECTION('center_axis',(-1.,0.,0.));
#35695=DIRECTION('ref_axis',(0.,0.,-1.));
#35696=DIRECTION('center_axis',(1.,0.,0.));
#35697=DIRECTION('ref_axis',(0.,0.,-1.));
#35698=DIRECTION('center_axis',(1.,0.,0.));
#35699=DIRECTION('ref_axis',(0.,0.,-1.));
#35700=DIRECTION('center_axis',(-1.,0.,0.));
#35701=DIRECTION('ref_axis',(0.,0.,-1.));
#35702=DIRECTION('',(-1.,0.,0.));
#35703=DIRECTION('center_axis',(-1.,0.,0.));
#35704=DIRECTION('ref_axis',(0.,0.,-1.));
#35705=DIRECTION('center_axis',(1.,0.,0.));
#35706=DIRECTION('ref_axis',(0.,0.,-1.));
#35707=DIRECTION('center_axis',(-1.,0.,0.));
#35708=DIRECTION('ref_axis',(0.,-0.912870929175277,-0.408248290463863));
#35709=DIRECTION('center_axis',(-1.,0.,0.));
#35710=DIRECTION('ref_axis',(0.,0.,-1.));
#35711=DIRECTION('',(1.,0.,0.));
#35712=DIRECTION('center_axis',(-1.,0.,0.));
#35713=DIRECTION('ref_axis',(0.,0.,-1.));
#35714=DIRECTION('',(1.,0.,0.));
#35715=DIRECTION('center_axis',(0.,0.,1.));
#35716=DIRECTION('ref_axis',(0.,-1.,0.));
#35717=DIRECTION('',(0.,-1.,0.));
#35718=DIRECTION('',(0.,-1.,0.));
#35719=DIRECTION('',(1.,0.,0.));
#35720=DIRECTION('center_axis',(-1.,0.,0.));
#35721=DIRECTION('ref_axis',(0.,0.912870929175277,-0.408248290463863));
#35722=DIRECTION('center_axis',(-1.,0.,0.));
#35723=DIRECTION('ref_axis',(0.,0.,-1.));
#35724=DIRECTION('center_axis',(-1.,0.,0.));
#35725=DIRECTION('ref_axis',(0.,0.,-1.));
#35726=DIRECTION('',(1.,0.,0.));
#35727=DIRECTION('center_axis',(0.,-1.,0.));
#35728=DIRECTION('ref_axis',(0.,0.,-1.));
#35729=DIRECTION('',(0.,0.,-1.));
#35730=DIRECTION('',(0.,0.,-1.));
#35731=DIRECTION('center_axis',(0.,1.,0.));
#35732=DIRECTION('ref_axis',(0.,0.,1.));
#35733=DIRECTION('',(0.,0.,1.));
#35734=DIRECTION('',(0.,0.,1.));
#35735=DIRECTION('center_axis',(1.,0.,0.));
#35736=DIRECTION('ref_axis',(0.,0.,-1.));
#35737=DIRECTION('center_axis',(1.,0.,0.));
#35738=DIRECTION('ref_axis',(0.,0.,-1.));
#35739=DIRECTION('center_axis',(1.,0.,0.));
#35740=DIRECTION('ref_axis',(0.,0.,-1.));
#35741=DIRECTION('center_axis',(0.,1.,0.));
#35742=DIRECTION('ref_axis',(0.,0.,1.));
#35743=DIRECTION('',(0.,0.,1.));
#35744=DIRECTION('',(1.,0.,0.));
#35745=DIRECTION('',(0.,0.,1.));
#35746=DIRECTION('',(1.,0.,0.));
#35747=DIRECTION('center_axis',(0.,0.,1.));
#35748=DIRECTION('ref_axis',(0.,-1.,0.));
#35749=DIRECTION('',(0.,-1.,0.));
#35750=DIRECTION('',(0.,-1.,0.));
#35751=DIRECTION('',(1.,0.,0.));
#35752=DIRECTION('center_axis',(0.,0.894427190999916,-0.447213595499958));
#35753=DIRECTION('ref_axis',(0.,0.447213595499958,0.894427190999916));
#35754=DIRECTION('',(0.,0.447213595499958,0.894427190999916));
#35755=DIRECTION('',(0.,0.447213595499958,0.894427190999916));
#35756=DIRECTION('',(1.,0.,0.));
#35757=DIRECTION('center_axis',(0.,-0.894427190999916,-0.447213595499958));
#35758=DIRECTION('ref_axis',(0.,0.447213595499958,-0.894427190999916));
#35759=DIRECTION('',(0.,0.447213595499958,-0.894427190999916));
#35760=DIRECTION('',(0.,0.447213595499958,-0.894427190999916));
#35761=DIRECTION('',(1.,0.,0.));
#35762=DIRECTION('center_axis',(0.,0.,1.));
#35763=DIRECTION('ref_axis',(0.,-1.,0.));
#35764=DIRECTION('',(0.,-1.,0.));
#35765=DIRECTION('',(0.,-1.,0.));
#35766=DIRECTION('',(1.,0.,0.));
#35767=DIRECTION('center_axis',(0.,-1.,0.));
#35768=DIRECTION('ref_axis',(0.,0.,-1.));
#35769=DIRECTION('',(0.,0.,-1.));
#35770=DIRECTION('',(0.,0.,-1.));
#35771=DIRECTION('',(1.,0.,0.));
#35772=DIRECTION('center_axis',(0.,0.,1.));
#35773=DIRECTION('ref_axis',(0.,-1.,0.));
#35774=DIRECTION('',(0.,-1.,0.));
#35775=DIRECTION('',(0.,-1.,0.));
#35776=DIRECTION('center_axis',(-1.,0.,0.));
#35777=DIRECTION('ref_axis',(0.,0.,-1.));
#35778=DIRECTION('center_axis',(-1.,0.,0.));
#35779=DIRECTION('ref_axis',(0.,0.,-1.));
#35780=DIRECTION('',(-1.,0.,0.));
#35781=DIRECTION('center_axis',(-1.,0.,0.));
#35782=DIRECTION('ref_axis',(0.,0.,-1.));
#35783=DIRECTION('center_axis',(1.,0.,0.));
#35784=DIRECTION('ref_axis',(0.,0.,-1.));
#35785=DIRECTION('center_axis',(0.,0.,-1.));
#35786=DIRECTION('ref_axis',(0.,1.,0.));
#35787=DIRECTION('',(0.,1.,0.));
#35788=DIRECTION('',(1.,0.,0.));
#35789=DIRECTION('',(0.,1.,0.));
#35790=DIRECTION('',(1.,0.,0.));
#35791=DIRECTION('center_axis',(0.,-1.,0.));
#35792=DIRECTION('ref_axis',(0.,0.,-1.));
#35793=DIRECTION('',(0.,0.,-1.));
#35794=DIRECTION('',(0.,0.,-1.));
#35795=DIRECTION('',(1.,0.,0.));
#35796=DIRECTION('center_axis',(0.,0.,-1.));
#35797=DIRECTION('ref_axis',(0.,1.,0.));
#35798=DIRECTION('',(0.,1.,0.));
#35799=DIRECTION('',(0.,1.,0.));
#35800=DIRECTION('',(1.,0.,0.));
#35801=DIRECTION('center_axis',(0.,-0.894427190999916,0.447213595499957));
#35802=DIRECTION('ref_axis',(0.,-0.447213595499957,-0.894427190999916));
#35803=DIRECTION('',(0.,-0.447213595499957,-0.894427190999916));
#35804=DIRECTION('',(0.,-0.447213595499957,-0.894427190999916));
#35805=DIRECTION('',(1.,0.,0.));
#35806=DIRECTION('center_axis',(0.,0.894427190999916,0.447213595499957));
#35807=DIRECTION('ref_axis',(0.,-0.447213595499957,0.894427190999916));
#35808=DIRECTION('',(0.,-0.447213595499957,0.894427190999916));
#35809=DIRECTION('',(0.,-0.447213595499957,0.894427190999916));
#35810=DIRECTION('',(1.,0.,0.));
#35811=DIRECTION('center_axis',(0.,0.,-1.));
#35812=DIRECTION('ref_axis',(0.,1.,0.));
#35813=DIRECTION('',(0.,1.,0.));
#35814=DIRECTION('',(0.,1.,0.));
#35815=DIRECTION('',(1.,0.,0.));
#35816=DIRECTION('center_axis',(0.,1.,0.));
#35817=DIRECTION('ref_axis',(0.,0.,1.));
#35818=DIRECTION('',(0.,0.,1.));
#35819=DIRECTION('',(0.,0.,1.));
#35820=DIRECTION('center_axis',(-1.,0.,0.));
#35821=DIRECTION('ref_axis',(0.,0.,-1.));
#35822=DIRECTION('center_axis',(-1.,0.,0.));
#35823=DIRECTION('ref_axis',(0.,0.,-1.));
#35824=DIRECTION('',(-1.,0.,0.));
#35825=DIRECTION('center_axis',(-1.,0.,0.));
#35826=DIRECTION('ref_axis',(0.,0.,-1.));
#35827=DIRECTION('center_axis',(1.,0.,0.));
#35828=DIRECTION('ref_axis',(0.,0.,-1.));
#35829=DIRECTION('center_axis',(1.,0.,0.));
#35830=DIRECTION('ref_axis',(0.,1.,0.));
#35831=DIRECTION('center_axis',(1.,0.,0.));
#35832=DIRECTION('ref_axis',(0.,1.,0.));
#35833=DIRECTION('center_axis',(1.,0.,0.));
#35834=DIRECTION('ref_axis',(0.,1.,0.));
#35835=DIRECTION('',(0.,0.,1.));
#35836=DIRECTION('',(0.,-1.,0.));
#35837=DIRECTION('',(0.,0.,1.));
#35838=DIRECTION('center_axis',(1.,0.,0.));
#35839=DIRECTION('ref_axis',(0.,0.,-1.));
#35840=DIRECTION('center_axis',(-1.,0.,0.));
#35841=DIRECTION('ref_axis',(0.,0.,-1.));
#35842=DIRECTION('center_axis',(-1.,0.,0.));
#35843=DIRECTION('ref_axis',(0.,0.,-1.));
#35844=DIRECTION('',(-1.,0.,0.));
#35845=DIRECTION('center_axis',(1.,0.,0.));
#35846=DIRECTION('ref_axis',(0.,0.,-1.));
#35847=DIRECTION('center_axis',(-1.,0.,0.));
#35848=DIRECTION('ref_axis',(0.,0.,-1.));
#35849=DIRECTION('center_axis',(-1.,0.,0.));
#35850=DIRECTION('ref_axis',(0.,0.,-1.));
#35851=DIRECTION('',(-1.,0.,0.));
#35852=DIRECTION('center_axis',(1.,0.,0.));
#35853=DIRECTION('ref_axis',(0.,0.,-1.));
#35854=DIRECTION('center_axis',(0.,0.,1.));
#35855=DIRECTION('ref_axis',(1.,0.,0.));
#35856=DIRECTION('center_axis',(0.,0.,1.));
#35857=DIRECTION('ref_axis',(1.,0.,0.));
#35858=DIRECTION('',(0.,0.,1.));
#35859=DIRECTION('center_axis',(0.,0.,-1.));
#35860=DIRECTION('ref_axis',(-1.,0.,0.));
#35861=DIRECTION('center_axis',(0.,0.,1.));
#35862=DIRECTION('ref_axis',(1.,0.,0.));
#35863=DIRECTION('center_axis',(0.,0.,1.));
#35864=DIRECTION('ref_axis',(1.,0.,0.));
#35865=DIRECTION('',(0.,0.,1.));
#35866=DIRECTION('center_axis',(0.,0.,-1.));
#35867=DIRECTION('ref_axis',(-1.,0.,0.));
#35868=DIRECTION('center_axis',(-1.,0.,0.));
#35869=DIRECTION('ref_axis',(0.,-1.,0.));
#35870=DIRECTION('',(0.,1.,0.));
#35871=DIRECTION('',(0.,0.,1.));
#35872=DIRECTION('center_axis',(0.,0.,-1.));
#35873=DIRECTION('ref_axis',(0.914708142118334,0.404115100859181,0.));
#35874=DIRECTION('center_axis',(0.,0.,1.));
#35875=DIRECTION('ref_axis',(0.914708142118334,0.404115100859181,0.));
#35876=DIRECTION('center_axis',(0.,0.,-1.));
#35877=DIRECTION('ref_axis',(0.,1.,0.));
#35878=DIRECTION('center_axis',(0.,0.,1.));
#35879=DIRECTION('ref_axis',(0.,1.,0.));
#35880=DIRECTION('',(0.,0.,1.));
#35881=DIRECTION('center_axis',(0.,1.,0.));
#35882=DIRECTION('ref_axis',(-1.,0.,0.));
#35883=DIRECTION('',(1.,0.,0.));
#35884=DIRECTION('',(0.,0.,1.));
#35885=DIRECTION('center_axis',(0.,0.,-1.));
#35886=DIRECTION('ref_axis',(0.,-1.,0.));
#35887=DIRECTION('center_axis',(0.,0.,1.));
#35888=DIRECTION('ref_axis',(0.,-1.,0.));
#35889=DIRECTION('',(0.,0.,1.));
#35890=DIRECTION('center_axis',(-1.,0.,0.));
#35891=DIRECTION('ref_axis',(0.,-1.,0.));
#35892=DIRECTION('',(0.,1.,0.));
#35893=DIRECTION('',(0.,0.,1.));
#35894=DIRECTION('center_axis',(0.,0.,-1.));
#35895=DIRECTION('ref_axis',(1.,0.,0.));
#35896=DIRECTION('center_axis',(0.,0.,1.));
#35897=DIRECTION('ref_axis',(1.,0.,0.));
#35898=DIRECTION('',(0.,0.,1.));
#35899=DIRECTION('center_axis',(0.160285849379284,-0.987070639057186,0.));
#35900=DIRECTION('ref_axis',(0.987070639057186,0.160285849379284,0.));
#35901=DIRECTION('',(-0.987070639057186,-0.160285849379284,0.));
#35902=DIRECTION('',(0.,0.,1.));
#35903=DIRECTION('center_axis',(0.,0.,-1.));
#35904=DIRECTION('ref_axis',(0.,1.,0.));
#35905=DIRECTION('center_axis',(0.,0.,1.));
#35906=DIRECTION('ref_axis',(0.,1.,0.));
#35907=DIRECTION('center_axis',(0.,0.,-1.));
#35908=DIRECTION('ref_axis',(-1.,0.,0.));
#35909=DIRECTION('center_axis',(0.,0.,1.));
#35910=DIRECTION('ref_axis',(-1.,0.,0.));
#35911=DIRECTION('',(0.,0.,1.));
#35912=DIRECTION('center_axis',(3.69197497485193E-16,1.,0.));
#35913=DIRECTION('ref_axis',(-1.,3.69197497485193E-16,0.));
#35914=DIRECTION('',(1.,-3.69197497485193E-16,0.));
#35915=DIRECTION('',(0.,0.,1.));
#35916=DIRECTION('center_axis',(0.,0.,-1.));
#35917=DIRECTION('ref_axis',(0.,-1.,0.));
#35918=DIRECTION('center_axis',(0.,0.,1.));
#35919=DIRECTION('ref_axis',(0.,-1.,0.));
#35920=DIRECTION('',(0.,0.,1.));
#35921=DIRECTION('center_axis',(-1.,0.,0.));
#35922=DIRECTION('ref_axis',(0.,-1.,0.));
#35923=DIRECTION('',(0.,-1.,0.));
#35924=DIRECTION('',(0.,0.,1.));
#35925=DIRECTION('center_axis',(0.,0.,-1.));
#35926=DIRECTION('ref_axis',(1.,4.44089209850062E-16,0.));
#35927=DIRECTION('center_axis',(0.,0.,1.));
#35928=DIRECTION('ref_axis',(1.,4.44089209850062E-16,0.));
#35929=DIRECTION('',(0.,0.,1.));
#35930=DIRECTION('center_axis',(-0.160285849379284,-0.987070639057186,0.));
#35931=DIRECTION('ref_axis',(0.987070639057186,-0.160285849379284,0.));
#35932=DIRECTION('',(0.987070639057186,-0.160285849379284,0.));
#35933=DIRECTION('',(0.,0.,1.));
#35934=DIRECTION('center_axis',(0.,0.,-1.));
#35935=DIRECTION('ref_axis',(0.,1.,0.));
#35936=DIRECTION('center_axis',(0.,0.,1.));
#35937=DIRECTION('ref_axis',(0.,1.,0.));
#35938=DIRECTION('',(0.,0.,1.));
#35939=DIRECTION('center_axis',(1.,0.,0.));
#35940=DIRECTION('ref_axis',(0.,1.,0.));
#35941=DIRECTION('',(0.,1.,0.));
#35942=DIRECTION('',(0.,0.,1.));
#35943=DIRECTION('center_axis',(0.,0.,-1.));
#35944=DIRECTION('ref_axis',(-1.,0.,0.));
#35945=DIRECTION('center_axis',(0.,0.,1.));
#35946=DIRECTION('ref_axis',(-1.,0.,0.));
#35947=DIRECTION('',(0.,0.,1.));
#35948=DIRECTION('center_axis',(0.,1.,0.));
#35949=DIRECTION('ref_axis',(-1.,0.,0.));
#35950=DIRECTION('',(-1.,0.,0.));
#35951=DIRECTION('',(0.,0.,1.));
#35952=DIRECTION('center_axis',(0.,0.,-1.));
#35953=DIRECTION('ref_axis',(1.,0.,0.));
#35954=DIRECTION('center_axis',(0.,0.,1.));
#35955=DIRECTION('ref_axis',(1.,0.,0.));
#35956=DIRECTION('',(0.,0.,1.));
#35957=DIRECTION('center_axis',(1.,0.,0.));
#35958=DIRECTION('ref_axis',(0.,1.,0.));
#35959=DIRECTION('',(0.,1.,0.));
#35960=DIRECTION('',(0.,0.,1.));
#35961=DIRECTION('center_axis',(0.,0.,-1.));
#35962=DIRECTION('ref_axis',(-0.374029024133323,0.927416998499529,0.));
#35963=DIRECTION('center_axis',(0.,0.,1.));
#35964=DIRECTION('ref_axis',(-0.374029024133323,0.927416998499529,0.));
#35965=DIRECTION('center_axis',(0.,0.,1.));
#35966=DIRECTION('ref_axis',(1.,0.,0.));
#35967=DIRECTION('',(0.,0.,1.));
#35968=DIRECTION('',(1.,0.,0.));
#35969=DIRECTION('',(0.,0.,1.));
#35970=DIRECTION('',(1.,0.,0.));
#35971=DIRECTION('',(0.,0.,1.));
#35972=DIRECTION('',(1.,0.,0.));
#35973=DIRECTION('',(0.,0.,1.));
#35974=DIRECTION('',(1.,0.,0.));
#35975=DIRECTION('',(0.,0.,1.));
#35976=DIRECTION('',(1.,0.,0.));
#35977=DIRECTION('',(0.,0.,1.));
#35978=DIRECTION('',(1.,0.,0.));
#35979=DIRECTION('',(0.,0.,1.));
#35980=DIRECTION('',(1.,0.,0.));
#35981=CARTESIAN_POINT('',(0.,0.,0.));
#35982=CARTESIAN_POINT('',(0.,0.,0.));
#35983=CARTESIAN_POINT('Origin',(0.,18.7095,-22.));
#35984=CARTESIAN_POINT('',(2.0145,16.8045,-22.));
#35985=CARTESIAN_POINT('',(-2.0145,16.8045,-22.));
#35986=CARTESIAN_POINT('',(-2.0145,16.8045,-22.));
#35987=CARTESIAN_POINT('',(-4.76226713600492,17.1467524890944,-22.));
#35988=CARTESIAN_POINT('',(-2.0145,16.8045,-22.));
#35989=CARTESIAN_POINT('',(-2.86121610856864,17.7902227611999,-22.));
#35990=CARTESIAN_POINT('',(-4.76226713600492,17.1467524890944,-22.));
#35991=CARTESIAN_POINT('',(-2.77493396164202,17.9105472818593,-22.));
#35992=CARTESIAN_POINT('Origin',(-2.90193395837302,17.9105184664736,-22.));
#35993=CARTESIAN_POINT('',(-2.77524548545753,19.2835472465181,-22.));
#35994=CARTESIAN_POINT('',(-2.77493396164202,17.9105472818593,-22.));
#35995=CARTESIAN_POINT('',(-2.50285868490141,19.4743666560534,-22.));
#35996=CARTESIAN_POINT('Origin',(-2.57224549068278,19.2835933057566,-22.));
#35997=CARTESIAN_POINT('',(-1.1157578719061,18.9698596347071,-22.));
#35998=CARTESIAN_POINT('',(-2.50285868490141,19.4743666560534,-22.));
#35999=CARTESIAN_POINT('',(-1.06752374914854,18.9384317981151,-22.));
#36000=CARTESIAN_POINT('Origin',(-1.15916735138508,18.8505088194968,-22.));
#36001=CARTESIAN_POINT('',(-0.749754873669872,18.6072159443625,-22.));
#36002=CARTESIAN_POINT('',(-1.06752374914854,18.9384317981151,-22.));
#36003=CARTESIAN_POINT('',(-0.476019974175079,18.7173288203203,-22.));
#36004=CARTESIAN_POINT('Origin',(-0.635019970082392,18.7172927443649,-22.));
#36005=CARTESIAN_POINT('',(-0.476404103686861,20.4103287767422,-22.));
#36006=CARTESIAN_POINT('',(-0.476019974175079,18.7173288203203,-22.));
#36007=CARTESIAN_POINT('',(-0.27345016815068,20.6133748307555,-22.));
#36008=CARTESIAN_POINT('Origin',(-0.273404108912115,20.4103748359807,-22.));
#36009=CARTESIAN_POINT('',(0.,20.6145,-22.));
#36010=CARTESIAN_POINT('',(-0.27345016815068,20.6133748307555,-22.));
#36011=CARTESIAN_POINT('',(0.27345016815068,20.6133748307555,-22.));
#36012=CARTESIAN_POINT('',(0.27345016815068,20.6133748307555,-22.));
#36013=CARTESIAN_POINT('',(0.47640410368686,20.4103287767422,-22.));
#36014=CARTESIAN_POINT('Origin',(0.273404108912115,20.4103748359807,-22.));
#36015=CARTESIAN_POINT('',(0.476019974175079,18.7173288203203,-22.));
#36016=CARTESIAN_POINT('',(0.476019974175079,18.7173288203203,-22.));
#36017=CARTESIAN_POINT('',(0.749754873669872,18.6072159443625,-22.));
#36018=CARTESIAN_POINT('Origin',(0.635019970082392,18.7172927443649,-22.));
#36019=CARTESIAN_POINT('',(1.06752374914854,18.9384317981151,-22.));
#36020=CARTESIAN_POINT('',(1.06752374914854,18.9384317981151,-22.));
#36021=CARTESIAN_POINT('',(1.1157578719061,18.9698596347071,-22.));
#36022=CARTESIAN_POINT('Origin',(1.15916735138508,18.8505088194968,-22.));
#36023=CARTESIAN_POINT('',(2.50285868490141,19.4743666560534,-22.));
#36024=CARTESIAN_POINT('',(2.50285868490141,19.4743666560534,-22.));
#36025=CARTESIAN_POINT('',(2.77524548545753,19.2835472465181,-22.));
#36026=CARTESIAN_POINT('Origin',(2.57224549068278,19.2835933057566,-22.));
#36027=CARTESIAN_POINT('',(2.77493396164202,17.9105472818593,-22.));
#36028=CARTESIAN_POINT('',(2.77493396164202,17.9105472818593,-22.));
#36029=CARTESIAN_POINT('',(2.86121610856864,17.7902227611999,-22.));
#36030=CARTESIAN_POINT('Origin',(2.90193395837302,17.9105184664736,-22.));
#36031=CARTESIAN_POINT('',(4.76226713600492,17.1467524890944,-22.));
#36032=CARTESIAN_POINT('',(4.76226713600492,17.1467524890944,-22.));
#36033=CARTESIAN_POINT('',(2.0145,16.8045,-22.));
#36034=CARTESIAN_POINT('Origin',(-4.76226713600492,17.1467524890944,0.));
#36035=CARTESIAN_POINT('',(-2.0145,16.8045,422.));
#36036=CARTESIAN_POINT('',(-2.0145,16.8045,0.));
#36037=CARTESIAN_POINT('',(-4.76226713600492,17.1467524890944,422.));
#36038=CARTESIAN_POINT('',(-2.0145,16.8045,422.));
#36039=CARTESIAN_POINT('',(-4.76226713600492,17.1467524890944,0.));
#36040=CARTESIAN_POINT('Origin',(-2.86121610856864,17.7902227611999,0.));
#36041=CARTESIAN_POINT('',(-2.86121610856864,17.7902227611999,422.));
#36042=CARTESIAN_POINT('',(-4.76226713600492,17.1467524890944,422.));
#36043=CARTESIAN_POINT('',(-2.86121610856864,17.7902227611999,0.));
#36044=CARTESIAN_POINT('Origin',(-2.90193395837302,17.9105184664736,0.));
#36045=CARTESIAN_POINT('',(-2.77493396164202,17.9105472818593,422.));
#36046=CARTESIAN_POINT('Origin',(-2.90193395837302,17.9105184664736,422.));
#36047=CARTESIAN_POINT('',(-2.77493396164202,17.9105472818593,0.));
#36048=CARTESIAN_POINT('Origin',(-2.77524548545753,19.2835472465181,0.));
#36049=CARTESIAN_POINT('',(-2.77524548545753,19.2835472465181,422.));
#36050=CARTESIAN_POINT('',(-2.77493396164202,17.9105472818593,422.));
#36051=CARTESIAN_POINT('',(-2.77524548545753,19.2835472465181,0.));
#36052=CARTESIAN_POINT('Origin',(-2.57224549068278,19.2835933057566,0.));
#36053=CARTESIAN_POINT('',(-2.50285868490141,19.4743666560534,422.));
#36054=CARTESIAN_POINT('Origin',(-2.57224549068278,19.2835933057566,422.));
#36055=CARTESIAN_POINT('',(-2.50285868490141,19.4743666560534,0.));
#36056=CARTESIAN_POINT('Origin',(-1.1157578719061,18.9698596347071,0.));
#36057=CARTESIAN_POINT('',(-1.1157578719061,18.9698596347071,422.));
#36058=CARTESIAN_POINT('',(-2.50285868490141,19.4743666560534,422.));
#36059=CARTESIAN_POINT('',(-1.1157578719061,18.9698596347071,0.));
#36060=CARTESIAN_POINT('Origin',(-1.15916735138508,18.8505088194968,0.));
#36061=CARTESIAN_POINT('',(-1.06752374914854,18.9384317981151,422.));
#36062=CARTESIAN_POINT('Origin',(-1.15916735138508,18.8505088194968,422.));
#36063=CARTESIAN_POINT('',(-1.06752374914854,18.9384317981151,0.));
#36064=CARTESIAN_POINT('Origin',(-0.749754873669872,18.6072159443625,0.));
#36065=CARTESIAN_POINT('',(-0.749754873669872,18.6072159443625,422.));
#36066=CARTESIAN_POINT('',(-1.06752374914854,18.9384317981151,422.));
#36067=CARTESIAN_POINT('',(-0.749754873669872,18.6072159443625,0.));
#36068=CARTESIAN_POINT('Origin',(-0.635019970082392,18.7172927443649,0.));
#36069=CARTESIAN_POINT('',(-0.476019974175079,18.7173288203203,422.));
#36070=CARTESIAN_POINT('Origin',(-0.635019970082392,18.7172927443649,422.));
#36071=CARTESIAN_POINT('',(-0.476019974175079,18.7173288203203,0.));
#36072=CARTESIAN_POINT('Origin',(-0.47640410368686,20.4103287767422,0.));
#36073=CARTESIAN_POINT('',(-0.476404103686861,20.4103287767422,422.));
#36074=CARTESIAN_POINT('',(-0.476019974175079,18.7173288203203,422.));
#36075=CARTESIAN_POINT('',(-0.476404103686861,20.4103287767422,0.));
#36076=CARTESIAN_POINT('Origin',(-0.273404108912115,20.4103748359807,0.));
#36077=CARTESIAN_POINT('',(-0.27345016815068,20.6133748307555,422.));
#36078=CARTESIAN_POINT('Origin',(-0.273404108912115,20.4103748359807,422.));
#36079=CARTESIAN_POINT('',(-0.27345016815068,20.6133748307555,0.));
#36080=CARTESIAN_POINT('Origin',(0.,20.6145,0.));
#36081=CARTESIAN_POINT('',(0.,20.6145,422.));
#36082=CARTESIAN_POINT('',(-0.27345016815068,20.6133748307555,422.));
#36083=CARTESIAN_POINT('',(0.,20.6145,0.));
#36084=CARTESIAN_POINT('Origin',(0.27345016815068,20.6133748307555,0.));
#36085=CARTESIAN_POINT('',(0.27345016815068,20.6133748307555,422.));
#36086=CARTESIAN_POINT('',(0.27345016815068,20.6133748307555,422.));
#36087=CARTESIAN_POINT('',(0.27345016815068,20.6133748307555,0.));
#36088=CARTESIAN_POINT('Origin',(0.273404108912115,20.4103748359807,0.));
#36089=CARTESIAN_POINT('',(0.47640410368686,20.4103287767422,422.));
#36090=CARTESIAN_POINT('Origin',(0.273404108912115,20.4103748359807,422.));
#36091=CARTESIAN_POINT('',(0.47640410368686,20.4103287767422,0.));
#36092=CARTESIAN_POINT('Origin',(0.476019974175079,18.7173288203203,0.));
#36093=CARTESIAN_POINT('',(0.476019974175079,18.7173288203203,422.));
#36094=CARTESIAN_POINT('',(0.476019974175079,18.7173288203203,422.));
#36095=CARTESIAN_POINT('',(0.476019974175079,18.7173288203203,0.));
#36096=CARTESIAN_POINT('Origin',(0.635019970082392,18.7172927443649,0.));
#36097=CARTESIAN_POINT('',(0.749754873669872,18.6072159443625,422.));
#36098=CARTESIAN_POINT('Origin',(0.635019970082392,18.7172927443649,422.));
#36099=CARTESIAN_POINT('',(0.749754873669872,18.6072159443625,0.));
#36100=CARTESIAN_POINT('Origin',(1.06752374914854,18.9384317981151,0.));
#36101=CARTESIAN_POINT('',(1.06752374914854,18.9384317981151,422.));
#36102=CARTESIAN_POINT('',(1.06752374914854,18.9384317981151,422.));
#36103=CARTESIAN_POINT('',(1.06752374914854,18.9384317981151,0.));
#36104=CARTESIAN_POINT('Origin',(1.15916735138508,18.8505088194968,0.));
#36105=CARTESIAN_POINT('',(1.1157578719061,18.9698596347071,422.));
#36106=CARTESIAN_POINT('Origin',(1.15916735138508,18.8505088194968,422.));
#36107=CARTESIAN_POINT('',(1.1157578719061,18.9698596347071,0.));
#36108=CARTESIAN_POINT('Origin',(2.50285868490141,19.4743666560534,0.));
#36109=CARTESIAN_POINT('',(2.50285868490141,19.4743666560534,422.));
#36110=CARTESIAN_POINT('',(2.50285868490141,19.4743666560534,422.));
#36111=CARTESIAN_POINT('',(2.50285868490141,19.4743666560534,0.));
#36112=CARTESIAN_POINT('Origin',(2.57224549068278,19.2835933057566,0.));
#36113=CARTESIAN_POINT('',(2.77524548545753,19.2835472465181,422.));
#36114=CARTESIAN_POINT('Origin',(2.57224549068278,19.2835933057566,422.));
#36115=CARTESIAN_POINT('',(2.77524548545753,19.2835472465181,0.));
#36116=CARTESIAN_POINT('Origin',(2.77493396164202,17.9105472818593,0.));
#36117=CARTESIAN_POINT('',(2.77493396164202,17.9105472818593,422.));
#36118=CARTESIAN_POINT('',(2.77493396164202,17.9105472818593,422.));
#36119=CARTESIAN_POINT('',(2.77493396164202,17.9105472818593,0.));
#36120=CARTESIAN_POINT('Origin',(2.90193395837302,17.9105184664736,0.));
#36121=CARTESIAN_POINT('',(2.86121610856864,17.7902227611999,422.));
#36122=CARTESIAN_POINT('Origin',(2.90193395837302,17.9105184664736,422.));
#36123=CARTESIAN_POINT('',(2.86121610856864,17.7902227611999,0.));
#36124=CARTESIAN_POINT('Origin',(4.76226713600492,17.1467524890944,0.));
#36125=CARTESIAN_POINT('',(4.76226713600492,17.1467524890944,422.));
#36126=CARTESIAN_POINT('',(4.76226713600492,17.1467524890944,422.));
#36127=CARTESIAN_POINT('',(4.76226713600492,17.1467524890944,0.));
#36128=CARTESIAN_POINT('Origin',(2.0145,16.8045,0.));
#36129=CARTESIAN_POINT('',(2.0145,16.8045,422.));
#36130=CARTESIAN_POINT('',(2.0145,16.8045,422.));
#36131=CARTESIAN_POINT('',(2.0145,16.8045,0.));
#36132=CARTESIAN_POINT('Origin',(-2.0145,16.8045,0.));
#36133=CARTESIAN_POINT('',(-2.0145,16.8045,422.));
#36134=CARTESIAN_POINT('Origin',(0.,18.7095,422.));
#36135=CARTESIAN_POINT('',(0.,0.,0.));
#36136=CARTESIAN_POINT('Origin',(5.55111512312578E-16,19.8980255661466,
-22.));
#36137=CARTESIAN_POINT('',(0.476000000000002,18.7185,-22.));
#36138=CARTESIAN_POINT('',(0.476000000000002,20.4115,-22.));
#36139=CARTESIAN_POINT('',(0.476000000000002,20.4115,-22.));
#36140=CARTESIAN_POINT('',(0.273,20.6145,-22.));
#36141=CARTESIAN_POINT('Origin',(0.273,20.4115,-22.));
#36142=CARTESIAN_POINT('',(-0.273,20.6145,-22.));
#36143=CARTESIAN_POINT('',(0.273,20.6145,-22.));
#36144=CARTESIAN_POINT('',(-0.476000000000002,20.4115,-22.));
#36145=CARTESIAN_POINT('Origin',(-0.273,20.4115,-22.));
#36146=CARTESIAN_POINT('',(-0.475999999999999,18.7185,-22.));
#36147=CARTESIAN_POINT('',(-0.476000000000002,20.4115,-22.));
#36148=CARTESIAN_POINT('',(-0.749759876267637,18.6084492353546,-22.));
#36149=CARTESIAN_POINT('Origin',(-0.634999999999998,18.7185,-22.));
#36150=CARTESIAN_POINT('',(-1.55887524652215,19.4521869420016,-22.));
#36151=CARTESIAN_POINT('',(-0.749759876267637,18.6084492353546,-22.));
#36152=CARTESIAN_POINT('',(-1.55887524652215,19.9211869420016,-22.));
#36153=CARTESIAN_POINT('',(-1.55887524652215,19.4521869420016,-22.));
#36154=CARTESIAN_POINT('',(-3.19087524652215,19.9211869420016,-22.));
#36155=CARTESIAN_POINT('',(-1.55887524652215,19.9211869420016,-22.));
#36156=CARTESIAN_POINT('',(-3.19087524652215,18.3251869420016,-22.));
#36157=CARTESIAN_POINT('',(-3.19087524652215,19.9211869420016,-22.));
#36158=CARTESIAN_POINT('',(-4.34687524652215,18.3251869420016,-22.));
#36159=CARTESIAN_POINT('',(-3.19087524652215,18.3251869420016,-22.));
#36160=CARTESIAN_POINT('',(-4.34687524652215,20.1981869420016,-22.));
#36161=CARTESIAN_POINT('',(-4.34687524652215,18.3251869420016,-22.));
#36162=CARTESIAN_POINT('',(-4.06833369817656,20.5651518799515,-22.));
#36163=CARTESIAN_POINT('Origin',(-3.96587524652215,20.1981869420016,-22.));
#36164=CARTESIAN_POINT('',(-1.15958274644764,21.3772897382096,-22.));
#36165=CARTESIAN_POINT('',(-4.06833369817656,20.5651518799515,-22.));
#36166=CARTESIAN_POINT('',(-0.476500000000001,21.4708641902917,-22.));
#36167=CARTESIAN_POINT('Origin',(-0.476499999999996,18.9308641902917,-22.));
#36168=CARTESIAN_POINT('',(0.476499999999998,21.4708641902917,-22.));
#36169=CARTESIAN_POINT('',(0.476499999999999,21.4708641902917,-22.));
#36170=CARTESIAN_POINT('',(1.15958274644764,21.3772897382096,-22.));
#36171=CARTESIAN_POINT('Origin',(0.476499999999999,18.9308641902917,-22.));
#36172=CARTESIAN_POINT('',(4.06833369817657,20.5651518799515,-22.));
#36173=CARTESIAN_POINT('',(4.06833369817657,20.5651518799515,-22.));
#36174=CARTESIAN_POINT('',(4.34687524652215,20.1981869420016,-22.));
#36175=CARTESIAN_POINT('Origin',(3.96587524652215,20.1981869420016,-22.));
#36176=CARTESIAN_POINT('',(4.34687524652215,18.3251869420016,-22.));
#36177=CARTESIAN_POINT('',(4.34687524652215,18.3251869420016,-22.));
#36178=CARTESIAN_POINT('',(3.19087524652215,18.3251869420016,-22.));
#36179=CARTESIAN_POINT('',(3.19087524652215,18.3251869420016,-22.));
#36180=CARTESIAN_POINT('',(3.19087524652215,19.9211869420016,-22.));
#36181=CARTESIAN_POINT('',(3.19087524652215,19.9211869420016,-22.));
#36182=CARTESIAN_POINT('',(1.55887524652215,19.9211869420016,-22.));
#36183=CARTESIAN_POINT('',(1.55887524652215,19.9211869420016,-22.));
#36184=CARTESIAN_POINT('',(1.55887524652215,19.4521869420016,-22.));
#36185=CARTESIAN_POINT('',(1.55887524652215,19.4521869420016,-22.));
#36186=CARTESIAN_POINT('',(0.749759876267641,18.6084492353546,-22.));
#36187=CARTESIAN_POINT('',(0.749759876267641,18.6084492353546,-22.));
#36188=CARTESIAN_POINT('Origin',(0.635000000000002,18.7185,-22.));
#36189=CARTESIAN_POINT('Origin',(0.273,20.4115,0.));
#36190=CARTESIAN_POINT('',(0.476000000000002,20.4115,422.));
#36191=CARTESIAN_POINT('',(0.476000000000002,20.4115,0.));
#36192=CARTESIAN_POINT('',(0.273,20.6145,422.));
#36193=CARTESIAN_POINT('Origin',(0.273,20.4115,422.));
#36194=CARTESIAN_POINT('',(0.273,20.6145,0.));
#36195=CARTESIAN_POINT('Origin',(-0.273,20.6145,0.));
#36196=CARTESIAN_POINT('',(-0.273,20.6145,422.));
#36197=CARTESIAN_POINT('',(0.273,20.6145,422.));
#36198=CARTESIAN_POINT('',(-0.273,20.6145,0.));
#36199=CARTESIAN_POINT('Origin',(-0.273,20.4115,0.));
#36200=CARTESIAN_POINT('',(-0.476000000000002,20.4115,422.));
#36201=CARTESIAN_POINT('Origin',(-0.273,20.4115,422.));
#36202=CARTESIAN_POINT('',(-0.476000000000002,20.4115,0.));
#36203=CARTESIAN_POINT('Origin',(-0.475999999999999,18.7185,0.));
#36204=CARTESIAN_POINT('',(-0.475999999999999,18.7185,422.));
#36205=CARTESIAN_POINT('',(-0.476000000000002,20.4115,422.));
#36206=CARTESIAN_POINT('',(-0.475999999999999,18.7185,0.));
#36207=CARTESIAN_POINT('Origin',(-0.634999999999998,18.7185,0.));
#36208=CARTESIAN_POINT('',(-0.749759876267637,18.6084492353546,422.));
#36209=CARTESIAN_POINT('Origin',(-0.634999999999998,18.7185,422.));
#36210=CARTESIAN_POINT('',(-0.749759876267637,18.6084492353546,0.));
#36211=CARTESIAN_POINT('Origin',(-1.55887524652215,19.4521869420016,0.));
#36212=CARTESIAN_POINT('',(-1.55887524652215,19.4521869420016,422.));
#36213=CARTESIAN_POINT('',(-0.749759876267637,18.6084492353546,422.));
#36214=CARTESIAN_POINT('',(-1.55887524652215,19.4521869420016,0.));
#36215=CARTESIAN_POINT('Origin',(-1.55887524652215,19.9211869420016,0.));
#36216=CARTESIAN_POINT('',(-1.55887524652215,19.9211869420016,422.));
#36217=CARTESIAN_POINT('',(-1.55887524652215,19.4521869420016,422.));
#36218=CARTESIAN_POINT('',(-1.55887524652215,19.9211869420016,0.));
#36219=CARTESIAN_POINT('Origin',(-3.19087524652215,19.9211869420016,0.));
#36220=CARTESIAN_POINT('',(-3.19087524652215,19.9211869420016,422.));
#36221=CARTESIAN_POINT('',(-1.55887524652215,19.9211869420016,422.));
#36222=CARTESIAN_POINT('',(-3.19087524652215,19.9211869420016,0.));
#36223=CARTESIAN_POINT('Origin',(-3.19087524652215,18.3251869420016,0.));
#36224=CARTESIAN_POINT('',(-3.19087524652215,18.3251869420016,422.));
#36225=CARTESIAN_POINT('',(-3.19087524652215,19.9211869420016,422.));
#36226=CARTESIAN_POINT('',(-3.19087524652215,18.3251869420016,0.));
#36227=CARTESIAN_POINT('Origin',(-4.34687524652215,18.3251869420016,0.));
#36228=CARTESIAN_POINT('',(-4.34687524652215,18.3251869420016,422.));
#36229=CARTESIAN_POINT('',(-3.19087524652215,18.3251869420016,422.));
#36230=CARTESIAN_POINT('',(-4.34687524652215,18.3251869420016,0.));
#36231=CARTESIAN_POINT('Origin',(-4.34687524652215,20.1981869420016,0.));
#36232=CARTESIAN_POINT('',(-4.34687524652215,20.1981869420016,422.));
#36233=CARTESIAN_POINT('',(-4.34687524652215,18.3251869420016,422.));
#36234=CARTESIAN_POINT('',(-4.34687524652215,20.1981869420016,0.));
#36235=CARTESIAN_POINT('Origin',(-3.96587524652215,20.1981869420016,0.));
#36236=CARTESIAN_POINT('',(-4.06833369817656,20.5651518799515,422.));
#36237=CARTESIAN_POINT('Origin',(-3.96587524652215,20.1981869420016,422.));
#36238=CARTESIAN_POINT('',(-4.06833369817656,20.5651518799515,0.));
#36239=CARTESIAN_POINT('Origin',(-1.15958274644764,21.3772897382096,0.));
#36240=CARTESIAN_POINT('',(-1.15958274644764,21.3772897382096,422.));
#36241=CARTESIAN_POINT('',(-4.06833369817656,20.5651518799515,422.));
#36242=CARTESIAN_POINT('',(-1.15958274644764,21.3772897382096,0.));
#36243=CARTESIAN_POINT('Origin',(-0.476499999999996,18.9308641902917,0.));
#36244=CARTESIAN_POINT('',(-0.476500000000001,21.4708641902917,422.));
#36245=CARTESIAN_POINT('Origin',(-0.476499999999996,18.9308641902917,422.));
#36246=CARTESIAN_POINT('',(-0.476500000000001,21.4708641902917,0.));
#36247=CARTESIAN_POINT('Origin',(0.476499999999998,21.4708641902917,0.));
#36248=CARTESIAN_POINT('',(0.476499999999998,21.4708641902917,422.));
#36249=CARTESIAN_POINT('',(0.476499999999999,21.4708641902917,422.));
#36250=CARTESIAN_POINT('',(0.476499999999998,21.4708641902917,0.));
#36251=CARTESIAN_POINT('Origin',(0.476499999999999,18.9308641902917,0.));
#36252=CARTESIAN_POINT('',(1.15958274644764,21.3772897382096,422.));
#36253=CARTESIAN_POINT('Origin',(0.476499999999999,18.9308641902917,422.));
#36254=CARTESIAN_POINT('',(1.15958274644764,21.3772897382096,0.));
#36255=CARTESIAN_POINT('Origin',(4.06833369817657,20.5651518799515,0.));
#36256=CARTESIAN_POINT('',(4.06833369817657,20.5651518799515,422.));
#36257=CARTESIAN_POINT('',(4.06833369817657,20.5651518799515,422.));
#36258=CARTESIAN_POINT('',(4.06833369817657,20.5651518799515,0.));
#36259=CARTESIAN_POINT('Origin',(3.96587524652215,20.1981869420016,0.));
#36260=CARTESIAN_POINT('',(4.34687524652215,20.1981869420016,422.));
#36261=CARTESIAN_POINT('Origin',(3.96587524652215,20.1981869420016,422.));
#36262=CARTESIAN_POINT('',(4.34687524652215,20.1981869420016,0.));
#36263=CARTESIAN_POINT('Origin',(4.34687524652215,18.3251869420016,0.));
#36264=CARTESIAN_POINT('',(4.34687524652215,18.3251869420016,422.));
#36265=CARTESIAN_POINT('',(4.34687524652215,18.3251869420016,422.));
#36266=CARTESIAN_POINT('',(4.34687524652215,18.3251869420016,0.));
#36267=CARTESIAN_POINT('Origin',(3.19087524652215,18.3251869420016,0.));
#36268=CARTESIAN_POINT('',(3.19087524652215,18.3251869420016,422.));
#36269=CARTESIAN_POINT('',(3.19087524652215,18.3251869420016,422.));
#36270=CARTESIAN_POINT('',(3.19087524652215,18.3251869420016,0.));
#36271=CARTESIAN_POINT('Origin',(3.19087524652215,19.9211869420016,0.));
#36272=CARTESIAN_POINT('',(3.19087524652215,19.9211869420016,422.));
#36273=CARTESIAN_POINT('',(3.19087524652215,19.9211869420016,422.));
#36274=CARTESIAN_POINT('',(3.19087524652215,19.9211869420016,0.));
#36275=CARTESIAN_POINT('Origin',(1.55887524652215,19.9211869420016,0.));
#36276=CARTESIAN_POINT('',(1.55887524652215,19.9211869420016,422.));
#36277=CARTESIAN_POINT('',(1.55887524652215,19.9211869420016,422.));
#36278=CARTESIAN_POINT('',(1.55887524652215,19.9211869420016,0.));
#36279=CARTESIAN_POINT('Origin',(1.55887524652215,19.4521869420016,0.));
#36280=CARTESIAN_POINT('',(1.55887524652215,19.4521869420016,422.));
#36281=CARTESIAN_POINT('',(1.55887524652215,19.4521869420016,422.));
#36282=CARTESIAN_POINT('',(1.55887524652215,19.4521869420016,0.));
#36283=CARTESIAN_POINT('Origin',(0.749759876267641,18.6084492353546,0.));
#36284=CARTESIAN_POINT('',(0.749759876267641,18.6084492353546,422.));
#36285=CARTESIAN_POINT('',(0.749759876267641,18.6084492353546,422.));
#36286=CARTESIAN_POINT('',(0.749759876267641,18.6084492353546,0.));
#36287=CARTESIAN_POINT('Origin',(0.635000000000002,18.7185,0.));
#36288=CARTESIAN_POINT('',(0.476000000000002,18.7185,422.));
#36289=CARTESIAN_POINT('Origin',(0.635000000000002,18.7185,422.));
#36290=CARTESIAN_POINT('',(0.476000000000002,18.7185,0.));
#36291=CARTESIAN_POINT('Origin',(0.476000000000002,20.4115,0.));
#36292=CARTESIAN_POINT('',(0.476000000000002,20.4115,422.));
#36293=CARTESIAN_POINT('Origin',(5.55111512312578E-16,19.8980255661466,
422.));
#36294=CARTESIAN_POINT('',(0.,0.,0.));
#36295=CARTESIAN_POINT('Origin',(-26.8463464956315,10.1295,-7.));
#36296=CARTESIAN_POINT('',(-18.1904820161982,14.1758012177496,-3.89721939943572));
#36297=CARTESIAN_POINT('',(-18.0651682165609,14.1759493590362,-3.89710566674782));
#36298=CARTESIAN_POINT('',(-26.8463464956315,14.1758012177496,-3.89721939943572));
#36299=CARTESIAN_POINT('',(-17.734,7.81752421401937,-2.45527019889639));
#36300=CARTESIAN_POINT('Ctrl Pts',(-18.0651682165609,14.1759493590362,-3.89710566674782));
#36301=CARTESIAN_POINT('Ctrl Pts',(-18.0323425743127,13.7488769914328,-3.34120500142468));
#36302=CARTESIAN_POINT('Ctrl Pts',(-17.9607350504285,12.5654944078269,-2.3209180299781));
#36303=CARTESIAN_POINT('Ctrl Pts',(-17.8503456449082,10.2181819306684,-1.69542365644608));
#36304=CARTESIAN_POINT('Ctrl Pts',(-17.772781881636,8.55581177954194,-2.07969166083582));
#36305=CARTESIAN_POINT('Ctrl Pts',(-17.734,7.81752421401937,-2.45527019889639));
#36306=CARTESIAN_POINT('',(-17.734,5.85128156875001,-4.22571665929507));
#36307=CARTESIAN_POINT('Origin',(-17.734,10.1295,-7.));
#36308=CARTESIAN_POINT('Ctrl Pts',(-18.1904820161982,14.1758012177496,-3.89721939943572));
#36309=CARTESIAN_POINT('Ctrl Pts',(-18.1876881222065,14.1394962858778,-3.84987454688103));
#36310=CARTESIAN_POINT('Ctrl Pts',(-18.1848942282147,14.1023624762433,-3.80316978768467));
#36311=CARTESIAN_POINT('Ctrl Pts',(-18.182100334223,14.0644233505464,-3.75713410309268));
#36312=CARTESIAN_POINT('Ctrl Pts',(-18.1751666150798,13.9702682956653,-3.64288549220289));
#36313=CARTESIAN_POINT('Ctrl Pts',(-18.1682328959365,13.8711179308502,-3.53272057308594));
#36314=CARTESIAN_POINT('Ctrl Pts',(-18.1612991767932,13.7673500985625,-3.42706735854301));
#36315=CARTESIAN_POINT('Ctrl Pts',(-18.154366774106,13.6636019679364,-3.32143420362577));
#36316=CARTESIAN_POINT('Ctrl Pts',(-18.1474343714188,13.5552383504529,-3.22031127992504));
#36317=CARTESIAN_POINT('Ctrl Pts',(-18.1405019687316,13.4426745623103,-3.12409038809468));
#36318=CARTESIAN_POINT('Ctrl Pts',(-18.1335693228231,13.3301068249018,-3.02786612038393));
#36319=CARTESIAN_POINT('Ctrl Pts',(-18.1266366769147,13.2133388710388,-2.93654444601234));
#36320=CARTESIAN_POINT('Ctrl Pts',(-18.1197040310062,13.0928201831576,-2.85047779954234));
#36321=CARTESIAN_POINT('Ctrl Pts',(-18.1127717611685,12.9723080329749,-2.76441582187356));
#36322=CARTESIAN_POINT('Ctrl Pts',(-18.1058394913308,12.8480458254471,-2.68360849304181));
#36323=CARTESIAN_POINT('Ctrl Pts',(-18.0989072214931,12.7205131946587,-2.60836572275146));
#36324=CARTESIAN_POINT('Ctrl Pts',(-18.0919734128154,12.5929522539071,-2.53310624991173));
#36325=CARTESIAN_POINT('Ctrl Pts',(-18.0850396041378,12.462119724094,-2.46341397180043));
#36326=CARTESIAN_POINT('Ctrl Pts',(-18.0781057954601,12.3285216260018,-2.39955383811784));
#36327=CARTESIAN_POINT('Ctrl Pts',(-18.0739887600783,12.2491960890059,-2.36163608727149));
#36328=CARTESIAN_POINT('Ctrl Pts',(-18.0698717246966,12.168896016092,-2.32577360896847));
#36329=CARTESIAN_POINT('Ctrl Pts',(-18.0657546893148,12.0877310379076,-2.29201399724091));
#36330=CARTESIAN_POINT('Ctrl Pts',(-18.0588213575568,11.9510444008739,-2.23516080886065));
#36331=CARTESIAN_POINT('Ctrl Pts',(-18.0518880257988,11.8118565702988,-2.18425443407282));
#36332=CARTESIAN_POINT('Ctrl Pts',(-18.0449546940409,11.6707017706744,-2.13949610615628));
#36333=CARTESIAN_POINT('Ctrl Pts',(-18.0380226791153,11.52957378027,-2.09474627909029));
#36334=CARTESIAN_POINT('Ctrl Pts',(-18.0310906641897,11.3864798811559,-2.05614226907002));
#36335=CARTESIAN_POINT('Ctrl Pts',(-18.0241586492642,11.2419704520384,-2.02383576503533));
#36336=CARTESIAN_POINT('Ctrl Pts',(-18.0172263879248,11.0974558860127,-1.99152811259429));
#36337=CARTESIAN_POINT('Ctrl Pts',(-18.0102941265854,10.9515260112177,-1.96551848947931));
#36338=CARTESIAN_POINT('Ctrl Pts',(-18.0033618652459,10.8047429609757,-1.94590780222078));
#36339=CARTESIAN_POINT('Ctrl Pts',(-17.9964299772503,10.6579678158787,-1.92629817111502));
#36340=CARTESIAN_POINT('Ctrl Pts',(-17.9894980892546,10.5103399151234,-1.9130868291269));
#36341=CARTESIAN_POINT('Ctrl Pts',(-17.9825662012589,10.3624281190368,-1.9063229891009));
#36342=CARTESIAN_POINT('Ctrl Pts',(-17.9756327668903,10.2144833266306,-1.89955764019033));
#36343=CARTESIAN_POINT('Ctrl Pts',(-17.9686993325218,10.0662548427467,-1.89924268229057));
#36344=CARTESIAN_POINT('Ctrl Pts',(-17.9617658981532,9.91831378778123,-1.90537524602953));
#36345=CARTESIAN_POINT('Ctrl Pts',(-17.9576469469043,9.8304263195057,-1.90901842338271));
#36346=CARTESIAN_POINT('Ctrl Pts',(-17.9535279956555,9.74264030258537,-1.91493606689122));
#36347=CARTESIAN_POINT('Ctrl Pts',(-17.9494090444066,9.65507506418636,-1.92311887274498));
#36348=CARTESIAN_POINT('Ctrl Pts',(-17.9424753846608,9.50767162774376,-1.93689344499123));
#36349=CARTESIAN_POINT('Ctrl Pts',(-17.9355417249149,9.36084306546452,-1.95709434074805));
#36350=CARTESIAN_POINT('Ctrl Pts',(-17.9286080651691,9.21515569028204,-1.98364918658131));
#36351=CARTESIAN_POINT('Ctrl Pts',(-17.921675723217,9.06949600407137,-2.01019898546813));
#36352=CARTESIAN_POINT('Ctrl Pts',(-17.9147433812648,8.9249773972537,-2.04310026581364));
#36353=CARTESIAN_POINT('Ctrl Pts',(-17.9078110393127,8.78215725526951,-2.08222931317227));
#36354=CARTESIAN_POINT('Ctrl Pts',(-17.9008784555401,8.63933213129698,-2.12135972546763));
#36355=CARTESIAN_POINT('Ctrl Pts',(-17.8939458717674,8.49820591040426,-2.16671825537547));
#36356=CARTESIAN_POINT('Ctrl Pts',(-17.8870132879947,8.35932258344625,-2.21813081380062));
#36357=CARTESIAN_POINT('Ctrl Pts',(-17.8800810809331,8.22044680329677,-2.26954057850861));
#36358=CARTESIAN_POINT('Ctrl Pts',(-17.8731488738714,8.08381398289625,-2.32700359783838));
#36359=CARTESIAN_POINT('Ctrl Pts',(-17.8662166668098,7.94994985065518,-2.39029695679961));
#36360=CARTESIAN_POINT('Ctrl Pts',(-17.8592829213363,7.81605601096829,-2.45360436197322));
#36361=CARTESIAN_POINT('Ctrl Pts',(-17.8523491758629,7.68493238611156,-2.52274455078309));
#36362=CARTESIAN_POINT('Ctrl Pts',(-17.8454154303894,7.55708231303193,-2.59744753083239));
#36363=CARTESIAN_POINT('Ctrl Pts',(-17.8412980867591,7.48116336186096,-2.64180708228259));
#36364=CARTESIAN_POINT('Ctrl Pts',(-17.8371807431287,7.40639825299786,-2.68812726300884));
#36365=CARTESIAN_POINT('Ctrl Pts',(-17.8330633994984,7.33288794460905,-2.73634405566748));
#36366=CARTESIAN_POINT('Ctrl Pts',(-17.8261558247304,7.20956135421445,-2.81723628382821));
#36367=CARTESIAN_POINT('Ctrl Pts',(-17.8192482499625,7.08972242521831,-2.90349902317069));
#36368=CARTESIAN_POINT('Ctrl Pts',(-17.8123406751945,6.9738347131051,-2.9948061723449));
#36369=CARTESIAN_POINT('Ctrl Pts',(-17.805433730195,6.85795756655736,-3.08610499698111));
#36370=CARTESIAN_POINT('Ctrl Pts',(-17.7985267851956,6.74603118445736,-3.18244710971482));
#36371=CARTESIAN_POINT('Ctrl Pts',(-17.7916198401962,6.63848738561534,-3.28346506457867));
#36372=CARTESIAN_POINT('Ctrl Pts',(-17.7847137708704,6.53095722135077,-3.38447021222218));
#36373=CARTESIAN_POINT('Ctrl Pts',(-17.7778077015447,6.4278087750554,-3.49014978807379));
#36374=CARTESIAN_POINT('Ctrl Pts',(-17.7709016322189,6.32943824184797,-3.60009829050449));
#36375=CARTESIAN_POINT('Ctrl Pts',(-17.763994324437,6.23105006798389,-3.71006650985363));
#36376=CARTESIAN_POINT('Ctrl Pts',(-17.757087016655,6.13744174453664,-3.82430493647222));
#36377=CARTESIAN_POINT('Ctrl Pts',(-17.7501797088731,6.04897067901331,-3.94237323066272));
#36378=CARTESIAN_POINT('Ctrl Pts',(-17.7447864725821,5.97989233816772,-4.03456113210717));
#36379=CARTESIAN_POINT('Ctrl Pts',(-17.739393236291,5.91394518475807,-4.12908318533048));
#36380=CARTESIAN_POINT('Ctrl Pts',(-17.734,5.85128156875001,-4.22571665929507));
#36381=CARTESIAN_POINT('Origin',(-26.8463464956315,10.1295,-7.));
#36382=CARTESIAN_POINT('',(-19.6904980116781,14.1761130084764,-3.89698020567858));
#36383=CARTESIAN_POINT('',(-19.5651698472381,14.1758012177496,-3.89721939943572));
#36384=CARTESIAN_POINT('',(-26.8463464956315,14.1758012177496,-3.89721939943572));
#36385=CARTESIAN_POINT('',(-18.5963464953293,10.1295585775261,-12.0989827703721));
#36386=CARTESIAN_POINT('Ctrl Pts',(-19.5651698472381,14.1758012177496,-3.89721939943573));
#36387=CARTESIAN_POINT('Ctrl Pts',(-19.5580044161035,14.0826682834138,-3.77576578922978));
#36388=CARTESIAN_POINT('Ctrl Pts',(-19.5508389849689,13.9840555505791,-3.65849855785608));
#36389=CARTESIAN_POINT('Ctrl Pts',(-19.5436735538343,13.880367165973,-3.54590149196268));
#36390=CARTESIAN_POINT('Ctrl Pts',(-19.5367389751113,13.7800193638371,-3.43693202414545));
#36391=CARTESIAN_POINT('Ctrl Pts',(-19.5298043963883,13.6749181421213,-3.33233670473415));
#36392=CARTESIAN_POINT('Ctrl Pts',(-19.5228698176653,13.5654689251814,-3.23251827540095));
#36393=CARTESIAN_POINT('Ctrl Pts',(-19.5155889603249,13.4505543548251,-3.1277154066261));
#36394=CARTESIAN_POINT('Ctrl Pts',(-19.5083081029845,13.3308466771977,-3.02817903320695));
#36395=CARTESIAN_POINT('Ctrl Pts',(-19.5010272456441,13.2068564753748,-2.93432931443421));
#36396=CARTESIAN_POINT('Ctrl Pts',(-19.4937463883037,13.0828662735518,-2.84047959566147));
#36397=CARTESIAN_POINT('Ctrl Pts',(-19.4864655309633,12.9545938885293,-2.75231677826634));
#36398=CARTESIAN_POINT('Ctrl Pts',(-19.4791846736229,12.8225874034969,-2.67021002390112));
#36399=CARTESIAN_POINT('Ctrl Pts',(-19.4722525221646,12.6969031736126,-2.59203565096662));
#36400=CARTESIAN_POINT('Ctrl Pts',(-19.4653203707063,12.5677907388499,-2.51932374374965));
#36401=CARTESIAN_POINT('Ctrl Pts',(-19.4583882192479,12.4357445771248,-2.45235918849316));
#36402=CARTESIAN_POINT('Ctrl Pts',(-19.4514574046156,12.3037238797517,-2.38540754697069));
#36403=CARTESIAN_POINT('Ctrl Pts',(-19.4445265899834,12.168770879082,-2.32420119569286));
#36404=CARTESIAN_POINT('Ctrl Pts',(-19.4375957753511,12.0314040081222,-2.26897874197455));
#36405=CARTESIAN_POINT('Ctrl Pts',(-19.4306647326403,11.8940326167085,-2.2137544710018));
#36406=CARTESIAN_POINT('Ctrl Pts',(-19.4237336899295,11.7542475017452,-2.16451461821824));
#36407=CARTESIAN_POINT('Ctrl Pts',(-19.4168026472187,11.6125869069859,-2.12144957735118));
#36408=CARTESIAN_POINT('Ctrl Pts',(-19.4098719853274,11.4709340956326,-2.07838690265165));
#36409=CARTESIAN_POINT('Ctrl Pts',(-19.4029413234362,11.3274063275017,-2.04149845637549));
#36410=CARTESIAN_POINT('Ctrl Pts',(-19.3960106615449,11.1825568421866,-2.01092470620817));
#36411=CARTESIAN_POINT('Ctrl Pts',(-19.3890784541281,11.0376750556868,-1.98034413814746));
#36412=CARTESIAN_POINT('Ctrl Pts',(-19.3821462467112,10.8914712869161,-1.95608114825948));
#36413=CARTESIAN_POINT('Ctrl Pts',(-19.3752140392943,10.7445094240284,-1.93822517210057));
#36414=CARTESIAN_POINT('Ctrl Pts',(-19.3710890357678,10.6570599052498,-1.92759999022186));
#36415=CARTESIAN_POINT('Ctrl Pts',(-19.3669640322412,10.5693421308198,-1.91924244470383));
#36416=CARTESIAN_POINT('Ctrl Pts',(-19.3628390287147,10.481475913415,-1.91316267643876));
#36417=CARTESIAN_POINT('Ctrl Pts',(-19.3559048049855,10.3337708252122,-1.90294244920731));
#36418=CARTESIAN_POINT('Ctrl Pts',(-19.3489705812563,10.1855950223114,-1.89915811409712));
#36419=CARTESIAN_POINT('Ctrl Pts',(-19.3420363575271,10.0375191660747,-1.90182968838914));
#36420=CARTESIAN_POINT('Ctrl Pts',(-19.3351034415158,9.8894712353064,-1.9045007588518));
#36421=CARTESIAN_POINT('Ctrl Pts',(-19.3281705255045,9.74152354381111,-1.9136253036207));
#36422=CARTESIAN_POINT('Ctrl Pts',(-19.3212376094931,9.59424623169765,-1.9291712310986));
#36423=CARTESIAN_POINT('Ctrl Pts',(-19.3143044421616,9.44696358073864,-1.9447177221209));
#36424=CARTESIAN_POINT('Ctrl Pts',(-19.30737127483,9.30035168675085,-1.96668603024645));
#36425=CARTESIAN_POINT('Ctrl Pts',(-19.3004381074985,9.15497560566773,-1.99499218733364));
#36426=CARTESIAN_POINT('Ctrl Pts',(-19.2935053129045,9.00960734022225,-2.02329682263908));
#36427=CARTESIAN_POINT('Ctrl Pts',(-19.2865725183105,8.86547507891971,-2.05793856101137));
#36428=CARTESIAN_POINT('Ctrl Pts',(-19.2796397237165,8.72313373977314,-2.09878230007118));
#36429=CARTESIAN_POINT('Ctrl Pts',(-19.2727053897295,8.58076079443217,-2.13963510828241));
#36430=CARTESIAN_POINT('Ctrl Pts',(-19.2657710557426,8.44017988357931,-2.18669257768057));
#36431=CARTESIAN_POINT('Ctrl Pts',(-19.2588367217556,8.30193143109621,-2.23976953016401));
#36432=CARTESIAN_POINT('Ctrl Pts',(-19.2547222757726,8.21990253098119,-2.27126242542232));
#36433=CARTESIAN_POINT('Ctrl Pts',(-19.2506078297895,8.13869448353687,-2.30487357806509));
#36434=CARTESIAN_POINT('Ctrl Pts',(-19.2464933838065,8.05841702068354,-2.34055622495714));
#36435=CARTESIAN_POINT('Ctrl Pts',(-19.2395600669797,7.92314022125396,-2.40068560741598));
#36436=CARTESIAN_POINT('Ctrl Pts',(-19.232626750153,7.79046037418254,-2.4667205608979));
#36437=CARTESIAN_POINT('Ctrl Pts',(-19.2256934333262,7.66089097296183,-2.53841166493079));
#36438=CARTESIAN_POINT('Ctrl Pts',(-19.218761436208,7.53134623437504,-2.61008912306088));
#36439=CARTESIAN_POINT('Ctrl Pts',(-19.2118294390899,7.40491104954959,-2.68742042376904));
#36440=CARTESIAN_POINT('Ctrl Pts',(-19.2048974419717,7.28207405548853,-2.77011034534907));
#36441=CARTESIAN_POINT('Ctrl Pts',(-19.1979652025665,7.1592327680301,-2.8528031571064));
#36442=CARTESIAN_POINT('Ctrl Pts',(-19.1910329631612,7.03999019913484,-2.94085478267516));
#36443=CARTESIAN_POINT('Ctrl Pts',(-19.184100723756,6.92480620440643,-3.03392654171861));
#36444=CARTESIAN_POINT('Ctrl Pts',(-19.177168859976,6.8096284509534,-3.12699325764406));
#36445=CARTESIAN_POINT('Ctrl Pts',(-19.170236996196,6.69850908820766,-3.22507935421226));
#36446=CARTESIAN_POINT('Ctrl Pts',(-19.163305132416,6.5918750714188,-3.32780571528673));
#36447=CARTESIAN_POINT('Ctrl Pts',(-19.1563717255625,6.48521731727435,-3.43055494384976));
#36448=CARTESIAN_POINT('Ctrl Pts',(-19.1494383187091,6.38304714234844,-3.53794627142115));
#36449=CARTESIAN_POINT('Ctrl Pts',(-19.1425049118557,6.28575524711227,-3.64956312182307));
#36450=CARTESIAN_POINT('Ctrl Pts',(-19.1383858542032,6.22795524574662,-3.71587341509055));
#36451=CARTESIAN_POINT('Ctrl Pts',(-19.1342667965508,6.17187627667052,-3.7836743770029));
#36452=CARTESIAN_POINT('Ctrl Pts',(-19.1301477388983,6.11759365881622,-3.8528729753044));
#36453=CARTESIAN_POINT('Ctrl Pts',(-19.1232141282746,6.02621971662068,-3.96935499056361));
#36454=CARTESIAN_POINT('Ctrl Pts',(-19.1162805176509,5.93990636053414,-4.08983920703717));
#36455=CARTESIAN_POINT('Ctrl Pts',(-19.1093469070272,5.85899051470744,-4.21386473120448));
#36456=CARTESIAN_POINT('Ctrl Pts',(-19.1024146126326,5.77809002939035,-4.3378667112163));
#36457=CARTESIAN_POINT('Ctrl Pts',(-19.095482318238,5.70258519057678,-4.46540838095846));
#36458=CARTESIAN_POINT('Ctrl Pts',(-19.0885500238434,5.63276951068097,-4.5960000194616));
#36459=CARTESIAN_POINT('Ctrl Pts',(-19.0816174848406,5.56295136731649,-4.72659626593262));
#36460=CARTESIAN_POINT('Ctrl Pts',(-19.0746849458378,5.49882294336051,-4.86024240657262));
#36461=CARTESIAN_POINT('Ctrl Pts',(-19.067752406835,5.44063196898206,-4.99642380037644));
#36462=CARTESIAN_POINT('Ctrl Pts',(-19.0608202428625,5.38244414256678,-5.13259782716129));
#36463=CARTESIAN_POINT('Ctrl Pts',(-19.0538880788899,5.33019325204807,-5.27130652831807));
#36464=CARTESIAN_POINT('Ctrl Pts',(-19.0469559149174,5.28407902177485,-5.41201494220643));
#36465=CARTESIAN_POINT('Ctrl Pts',(-19.0400222095796,5.2379545380122,-5.55275464258111));
#36466=CARTESIAN_POINT('Ctrl Pts',(-19.0330885042419,5.19796954390401,-5.69549462988479));
#36467=CARTESIAN_POINT('Ctrl Pts',(-19.0261547989042,5.1642741877754,-5.83968382170268));
#36468=CARTESIAN_POINT('Ctrl Pts',(-19.0220372305995,5.1442642618192,-5.92531031103094));
#36469=CARTESIAN_POINT('Ctrl Pts',(-19.0179196622948,5.12647145780716,-6.01144759299916));
#36470=CARTESIAN_POINT('Ctrl Pts',(-19.0138020939901,5.11091873588374,-6.09797832871864));
#36471=CARTESIAN_POINT('Ctrl Pts',(-19.0068685366575,5.08472956762835,-6.24368709970922));
#36472=CARTESIAN_POINT('Ctrl Pts',(-18.9999349793249,5.06488588872228,-6.39056232944993));
#36473=CARTESIAN_POINT('Ctrl Pts',(-18.9930014219922,5.05146956995229,-6.53803901516524));
#36474=CARTESIAN_POINT('Ctrl Pts',(-18.9860691811566,5.03805579858218,-6.68548769900486));
#36475=CARTESIAN_POINT('Ctrl Pts',(-18.9791369403209,5.03106698243318,-6.83353728193027));
#36476=CARTESIAN_POINT('Ctrl Pts',(-18.9722046994853,5.03053313522663,-6.981617618673));
#36477=CARTESIAN_POINT('Ctrl Pts',(-18.9652722139179,5.02999926917346,-7.12970318315557));
#36478=CARTESIAN_POINT('Ctrl Pts',(-18.9583397283506,5.03592083259744,-7.27781917307014));
#36479=CARTESIAN_POINT('Ctrl Pts',(-18.9514072427832,5.04827571738031,-7.42539486329296));
#36480=CARTESIAN_POINT('Ctrl Pts',(-18.9444751320469,5.06062993414973,-7.57296257427935));
#36481=CARTESIAN_POINT('Ctrl Pts',(-18.9375430213105,5.07941674773549,-7.71998971467166));
#36482=CARTESIAN_POINT('Ctrl Pts',(-18.9306109105741,5.10456211729912,-7.86591008482266));
#36483=CARTESIAN_POINT('Ctrl Pts',(-18.9236772576965,5.12971308078845,-8.01186291692284));
#36484=CARTESIAN_POINT('Ctrl Pts',(-18.9167436048189,5.16122537054672,-8.1567081609133));
#36485=CARTESIAN_POINT('Ctrl Pts',(-18.9098099519412,5.19897359234514,-8.29988858884832));
#36486=CARTESIAN_POINT('Ctrl Pts',(-18.9056921176548,5.22139192287262,-8.38492216144028));
#36487=CARTESIAN_POINT('Ctrl Pts',(-18.9015742833683,5.24600873413897,-8.46936874424748));
#36488=CARTESIAN_POINT('Ctrl Pts',(-18.8974564490819,5.27278935781425,-8.55311388445269));
#36489=CARTESIAN_POINT('Ctrl Pts',(-18.8905228748665,5.31788234331871,-8.69412323655478));
#36490=CARTESIAN_POINT('Ctrl Pts',(-18.883589300651,5.36912832626771,-8.83319175144094));
#36491=CARTESIAN_POINT('Ctrl Pts',(-18.8766557264356,5.42633506454241,-8.96978186352757));
#36492=CARTESIAN_POINT('Ctrl Pts',(-18.8697234691356,5.48353093736216,-9.1063460326265));
#36493=CARTESIAN_POINT('Ctrl Pts',(-18.8627912118356,5.54668517907365,-9.2404324333557));
#36494=CARTESIAN_POINT('Ctrl Pts',(-18.8558589545357,5.61555731959328,-9.37152324003005));
#36495=CARTESIAN_POINT('Ctrl Pts',(-18.8489264532936,5.68443188368328,-9.50261865971326));
#36496=CARTESIAN_POINT('Ctrl Pts',(-18.8419939520516,5.75902459842385,-9.63071798021076));
#36497=CARTESIAN_POINT('Ctrl Pts',(-18.8350614508095,5.83904866843853,-9.75532727121524));
#36498=CARTESIAN_POINT('Ctrl Pts',(-18.8281293248839,5.91906840605573,-9.87992981603726));
#36499=CARTESIAN_POINT('Ctrl Pts',(-18.8211971989583,6.00451873113978,-10.0010424317848));
#36500=CARTESIAN_POINT('Ctrl Pts',(-18.8142650730327,6.09506908079314,-10.1181995058283));
#36501=CARTESIAN_POINT('Ctrl Pts',(-18.8073314058495,6.18563956300298,-10.2353826280473));
#36502=CARTESIAN_POINT('Ctrl Pts',(-18.8003977386663,6.28131213326655,-10.3486081896358));
#36503=CARTESIAN_POINT('Ctrl Pts',(-18.7934640714831,6.3817150551582,-10.4574425529887));
#36504=CARTESIAN_POINT('Ctrl Pts',(-18.7893463157133,6.44134219040977,-10.5220769399308));
#36505=CARTESIAN_POINT('Ctrl Pts',(-18.7852285599435,6.50263691562057,-10.5851632219833));
#36506=CARTESIAN_POINT('Ctrl Pts',(-18.7811108041737,6.56551500754935,-10.646616510354));
#36507=CARTESIAN_POINT('Ctrl Pts',(-18.7741773223733,6.6713892095192,-10.7500916264889));
#36508=CARTESIAN_POINT('Ctrl Pts',(-18.7672438405729,6.78179109135341,-10.8489706372656));
#36509=CARTESIAN_POINT('Ctrl Pts',(-18.7603103587725,6.8962990704977,-10.9428685939891));
#36510=CARTESIAN_POINT('Ctrl Pts',(-18.7533781937436,7.01078530286897,-11.0367487180902));
#36511=CARTESIAN_POINT('Ctrl Pts',(-18.7464460287148,7.12937582121678,-11.1256494659908));
#36512=CARTESIAN_POINT('Ctrl Pts',(-18.739513863686,7.25161567360849,-11.2092259150478));
#36513=CARTESIAN_POINT('Ctrl Pts',(-18.7325814536027,7.37385984722272,-11.2928053185622));
#36514=CARTESIAN_POINT('Ctrl Pts',(-18.7256490435193,7.49975334201189,-11.3710598572636));
#36515=CARTESIAN_POINT('Ctrl Pts',(-18.718716633436,7.62881146378363,-11.4436874152933));
#36516=CARTESIAN_POINT('Ctrl Pts',(-18.7117845978205,7.75786261422604,-11.516311050202));
#36517=CARTESIAN_POINT('Ctrl Pts',(-18.704852562205,7.8900777610185,-11.5833081513277));
#36518=CARTESIAN_POINT('Ctrl Pts',(-18.6979205265895,8.02494679887543,-11.64442211945));
#36519=CARTESIAN_POINT('Ctrl Pts',(-18.6909869476181,8.15984586411981,-11.7055496940518));
#36520=CARTESIAN_POINT('Ctrl Pts',(-18.6840533686468,8.29739969982354,-11.7607913819451));
#36521=CARTESIAN_POINT('Ctrl Pts',(-18.6771197896754,8.43707679425735,-11.8099381173424));
#36522=CARTESIAN_POINT('Ctrl Pts',(-18.6730015795388,8.52003822420948,-11.8391288981399));
#36523=CARTESIAN_POINT('Ctrl Pts',(-18.6688833694022,8.60374831456233,-11.8661704298008));
#36524=CARTESIAN_POINT('Ctrl Pts',(-18.6647651592655,8.68809285583543,-11.8910271359655));
#36525=CARTESIAN_POINT('Ctrl Pts',(-18.6577998241514,8.83074900390097,-11.9330685283489));
#36526=CARTESIAN_POINT('Ctrl Pts',(-18.6508344890373,8.97526829574175,-11.9688711530495));
#36527=CARTESIAN_POINT('Ctrl Pts',(-18.6438691539232,9.12109290423389,-11.9982913209625));
#36528=CARTESIAN_POINT('Ctrl Pts',(-18.6369053501428,9.26688545308524,-12.0277050208312));
#36529=CARTESIAN_POINT('Ctrl Pts',(-18.6299415463624,9.41398242822589,-12.0507390002111));
#36530=CARTESIAN_POINT('Ctrl Pts',(-18.622977742582,9.56181530050721,-12.0673005715037));
#36531=CARTESIAN_POINT('Ctrl Pts',(-18.6160146854246,9.70963232291145,-12.0838603671502));
#36532=CARTESIAN_POINT('Ctrl Pts',(-18.6090516282673,9.85818476303232,-12.0939491026305));
#36533=CARTESIAN_POINT('Ctrl Pts',(-18.60208857111,10.0068979934788,-12.097525845741));
#36534=CARTESIAN_POINT('Ctrl Pts',(-18.6001745459505,10.0477767135858,-12.0985090311648));
#36535=CARTESIAN_POINT('Ctrl Pts',(-18.598260520791,10.0886675622518,-12.099000469371));
#36536=CARTESIAN_POINT('Ctrl Pts',(-18.5963464956315,10.1295585712674,-12.0989999996636));
#36537=CARTESIAN_POINT('Ctrl Pts',(-18.5963464895958,10.1295586962519,-12.098655931404));
#36538=CARTESIAN_POINT('Ctrl Pts',(-18.580370831183,10.4708377603055,-12.0988021573896));
#36539=CARTESIAN_POINT('Ctrl Pts',(-18.5256132911341,11.6404949371434,-11.9829820272798));
#36540=CARTESIAN_POINT('Ctrl Pts',(-18.4320738694491,13.4987506203882,-11.0980785037433));
#36541=CARTESIAN_POINT('Ctrl Pts',(-18.3157282245409,15.0255448975692,-9.04320498956965));
#36542=CARTESIAN_POINT('Ctrl Pts',(-18.1993825796327,15.4123695196911,-6.51259611415262));
#36543=CARTESIAN_POINT('Ctrl Pts',(-18.1158625769727,14.8069605767375,-4.77742165783899));
#36544=CARTESIAN_POINT('Ctrl Pts',(-18.0711244559488,14.2534419862377,-3.99797429297315));
#36545=CARTESIAN_POINT('Ctrl Pts',(-18.0651682165609,14.1759493590362,-3.89710566674782));
#36546=CARTESIAN_POINT('',(-18.7216535051799,10.1294128054764,-12.0989687534116));
#36547=CARTESIAN_POINT('Ctrl Pts',(-18.7216535043684,10.1294128222767,-12.0989999992548));
#36548=CARTESIAN_POINT('Ctrl Pts',(-18.7147113419131,10.2777169024359,-12.0990025348131));
#36549=CARTESIAN_POINT('Ctrl Pts',(-18.7077691794578,10.4260250034406,-12.0925306047745));
#36550=CARTESIAN_POINT('Ctrl Pts',(-18.7008270170026,10.5737648955722,-12.0796092076618));
#36551=CARTESIAN_POINT('Ctrl Pts',(-18.6938850825327,10.7214999358232,-12.0666882348967));
#36552=CARTESIAN_POINT('Ctrl Pts',(-18.6869431480629,10.8686664773571,-12.0473182494839));
#36553=CARTESIAN_POINT('Ctrl Pts',(-18.680001213593,11.0146970824474,-12.021576159457));
#36554=CARTESIAN_POINT('Ctrl Pts',(-18.6730576379768,11.1607622107104,-11.9958279837289));
#36555=CARTESIAN_POINT('Ctrl Pts',(-18.6661140623605,11.3056905422907,-11.9637047507785));
#36556=CARTESIAN_POINT('Ctrl Pts',(-18.6591704867443,11.4489238560583,-11.9253346777721));
#36557=CARTESIAN_POINT('Ctrl Pts',(-18.6552746291148,11.5292883007021,-11.9038062391219));
#36558=CARTESIAN_POINT('Ctrl Pts',(-18.6513787714853,11.6091193479438,-11.8803121893208));
#36559=CARTESIAN_POINT('Ctrl Pts',(-18.6474829138558,11.6883203008384,-11.854882106673));
#36560=CARTESIAN_POINT('Ctrl Pts',(-18.6405493032985,11.8292773417162,-11.8096231916184));
#36561=CARTESIAN_POINT('Ctrl Pts',(-18.6336156927412,11.9682862806913,-11.7582135007032));
#36562=CARTESIAN_POINT('Ctrl Pts',(-18.626682082184,12.1048097739243,-11.7008459129224));
#36563=CARTESIAN_POINT('Ctrl Pts',(-18.6197497878564,12.2413073504607,-11.6434892154165));
#36564=CARTESIAN_POINT('Ctrl Pts',(-18.6128174935289,12.3753201180157,-11.5801770055648));
#36565=CARTESIAN_POINT('Ctrl Pts',(-18.6058851992013,12.5063305296346,-11.5111503669682));
#36566=CARTESIAN_POINT('Ctrl Pts',(-18.5989526602658,12.6373455639937,-11.4421212927467));
#36567=CARTESIAN_POINT('Ctrl Pts',(-18.5920201213302,12.7653577364192,-11.3673775374312));
#36568=CARTESIAN_POINT('Ctrl Pts',(-18.5850875823947,12.8898734499727,-11.2872064816948));
#36569=CARTESIAN_POINT('Ctrl Pts',(-18.5781554184894,13.0143824275872,-11.20703976298));
#36570=CARTESIAN_POINT('Ctrl Pts',(-18.5712232545841,13.1353950473725,-11.121446511085));
#36571=CARTESIAN_POINT('Ctrl Pts',(-18.5642910906788,13.2524460816721,-11.0307578407749));
#36572=CARTESIAN_POINT('Ctrl Pts',(-18.5573573854077,13.3695231422555,-10.9400490058497));
#36573=CARTESIAN_POINT('Ctrl Pts',(-18.5504236801366,13.4826365958723,-10.8442426912284));
#36574=CARTESIAN_POINT('Ctrl Pts',(-18.5434899748654,13.5913532383767,-10.7437111475033));
#36575=CARTESIAN_POINT('Ctrl Pts',(-18.5393724062262,13.6559144246746,-10.6840106676712));
#36576=CARTESIAN_POINT('Ctrl Pts',(-18.5352548375869,13.7189256853204,-10.6226445735402));
#36577=CARTESIAN_POINT('Ctrl Pts',(-18.5311372689476,13.7803022426319,-10.5596971760522));
#36578=CARTESIAN_POINT('Ctrl Pts',(-18.5242037116084,13.8836539816517,-10.453700305551));
#36579=CARTESIAN_POINT('Ctrl Pts',(-18.5172701542692,13.9824041897261,-10.3431810712656));
#36580=CARTESIAN_POINT('Ctrl Pts',(-18.51033659693,14.0761684078321,-10.2285615184816));
#36581=CARTESIAN_POINT('Ctrl Pts',(-18.5034043560879,14.1699148226197,-10.1139637288865));
#36582=CARTESIAN_POINT('Ctrl Pts',(-18.4964721152459,14.2586769270584,-9.99526742983162));
#36583=CARTESIAN_POINT('Ctrl Pts',(-18.4895398744039,14.3421103275237,-9.87292798873217));
#36584=CARTESIAN_POINT('Ctrl Pts',(-18.4826073888305,14.4255466734673,-9.75058422864091));
#36585=CARTESIAN_POINT('Ctrl Pts',(-18.4756749032572,14.5036537499851,-9.62459734036535));
#36586=CARTESIAN_POINT('Ctrl Pts',(-18.4687424176839,14.5761300052532,-9.49545238311256));
#36587=CARTESIAN_POINT('Ctrl Pts',(-18.4618103069418,14.6486023418167,-9.36631440857343));
#36588=CARTESIAN_POINT('Ctrl Pts',(-18.4548781961996,14.7154443053631,-9.23401899548399));
#36589=CARTESIAN_POINT('Ctrl Pts',(-18.4479460854575,14.7763998905137,-9.09907656066754));
#36590=CARTESIAN_POINT('Ctrl Pts',(-18.4410124325745,14.8373690360505,-8.96410410609937));
#36591=CARTESIAN_POINT('Ctrl Pts',(-18.4340787796916,14.8924490504929,-8.82648375455177));
#36592=CARTESIAN_POINT('Ctrl Pts',(-18.4271451268086,14.9414314869883,-8.6867472734616));
#36593=CARTESIAN_POINT('Ctrl Pts',(-18.4230272925522,14.9705217166792,-8.60375903069658));
#36594=CARTESIAN_POINT('Ctrl Pts',(-18.4189094582958,14.9974622098978,-8.52002479361661));
#36595=CARTESIAN_POINT('Ctrl Pts',(-18.4147916240394,15.0222175337942,-8.43565878066583));
#36596=CARTESIAN_POINT('Ctrl Pts',(-18.4078580498408,15.0639003370249,-8.29360400764394));
#36597=CARTESIAN_POINT('Ctrl Pts',(-18.4009244756422,15.099399552533,-8.14970818352137));
#36598=CARTESIAN_POINT('Ctrl Pts',(-18.3939909014436,15.1285731159382,-8.00452425630458));
#36599=CARTESIAN_POINT('Ctrl Pts',(-18.3870586441602,15.1577411383182,-7.85936790432008));
#36600=CARTESIAN_POINT('Ctrl Pts',(-18.3801263868768,15.1805858405798,-7.71292426128418));
#36601=CARTESIAN_POINT('Ctrl Pts',(-18.3731941295934,15.1970161634336,-7.56575695606785));
#36602=CARTESIAN_POINT('Ctrl Pts',(-18.3662616283674,15.2134470644621,-7.41858447210894));
#36603=CARTESIAN_POINT('Ctrl Pts',(-18.3593291271414,15.2234630944089,-7.27068860316924));
#36604=CARTESIAN_POINT('Ctrl Pts',(-18.3523966259154,15.2270249522307,-7.12263915111047));
#36605=CARTESIAN_POINT('Ctrl Pts',(-18.3454645000055,15.2305866172184,-6.9745977142461));
#36606=CARTESIAN_POINT('Ctrl Pts',(-18.3385323740955,15.2276948022499,-6.82640304141275));
#36607=CARTESIAN_POINT('Ctrl Pts',(-18.3316002481857,15.2183623246744,-6.67862601146168));
#36608=CARTESIAN_POINT('Ctrl Pts',(-18.3246665810175,15.2090277721571,-6.53081612541791));
#36609=CARTESIAN_POINT('Ctrl Pts',(-18.3177329138493,15.1932497165721,-6.38342439783593));
#36610=CARTESIAN_POINT('Ctrl Pts',(-18.3107992466811,15.1710929950943,-6.23701830178175));
#36611=CARTESIAN_POINT('Ctrl Pts',(-18.3066814908311,15.1579345946017,-6.15007086922192));
#36612=CARTESIAN_POINT('Ctrl Pts',(-18.3025637349812,15.1425274812019,-6.06347096462069));
#36613=CARTESIAN_POINT('Ctrl Pts',(-18.2984459791312,15.1248938320092,-5.97733609473846));
#36614=CARTESIAN_POINT('Ctrl Pts',(-18.2915125309928,15.0952024183793,-5.83230281083452));
#36615=CARTESIAN_POINT('Ctrl Pts',(-18.2845790828544,15.059185411284,-5.68853843504666));
#36616=CARTESIAN_POINT('Ctrl Pts',(-18.277645634716,15.0169762154728,-5.54659804486579));
#36617=CARTESIAN_POINT('Ctrl Pts',(-18.2703819998395,14.9727569207318,-5.39789812702961));
#36618=CARTESIAN_POINT('Ctrl Pts',(-18.2631183649631,14.9217412775336,-5.25120055839765));
#36619=CARTESIAN_POINT('Ctrl Pts',(-18.2558547300866,14.8641417140795,-5.10712682957934));
#36620=CARTESIAN_POINT('Ctrl Pts',(-18.2489226347855,14.8091712110254,-4.96962916683512));
#36621=CARTESIAN_POINT('Ctrl Pts',(-18.2419905394845,14.7482046250438,-4.83452146236116));
#36622=CARTESIAN_POINT('Ctrl Pts',(-18.2350584441835,14.6814762990125,-4.70232448478292));
#36623=CARTESIAN_POINT('Ctrl Pts',(-18.2281266662119,14.6147510275939,-4.57013355876596));
#36624=CARTESIAN_POINT('Ctrl Pts',(-18.2211948882404,14.5422646938408,-4.44085338759471));
#36625=CARTESIAN_POINT('Ctrl Pts',(-18.2142631102688,14.4642980869847,-4.31498109036941));
#36626=CARTESIAN_POINT('Ctrl Pts',(-18.2073302843237,14.3863196928292,-4.18908976327339));
#36627=CARTESIAN_POINT('Ctrl Pts',(-18.2003974583786,14.3028595456927,-4.06660761962958));
#36628=CARTESIAN_POINT('Ctrl Pts',(-18.1934646324335,14.2142425998208,-3.94800411317289));
#36629=CARTESIAN_POINT('Ctrl Pts',(-18.1924704270217,14.2015344418692,-3.93099571733137));
#36630=CARTESIAN_POINT('Ctrl Pts',(-18.19147622161,14.1887203048187,-3.91406703530483));
#36631=CARTESIAN_POINT('Ctrl Pts',(-18.1904820161982,14.1758012177496,-3.89721939943572));
#36632=CARTESIAN_POINT('Ctrl Pts',(-19.6904980116781,14.1761130084766,-3.89698020567888));
#36633=CARTESIAN_POINT('Ctrl Pts',(-19.6530813654925,13.6895815995602,-3.2628026380609));
#36634=CARTESIAN_POINT('Ctrl Pts',(-19.5768828376708,12.391409734591,-2.20936993870382));
#36635=CARTESIAN_POINT('Ctrl Pts',(-19.4619024282132,9.91265035575874,-1.69885130841003));
#36636=CARTESIAN_POINT('Ctrl Pts',(-19.3455567833049,7.45588094355372,-2.41786028132917));
#36637=CARTESIAN_POINT('Ctrl Pts',(-19.2292111383967,5.62120273326431,-4.20319480177778));
#36638=CARTESIAN_POINT('Ctrl Pts',(-19.1128654934885,4.83646615949574,-6.64003369704514));
#36639=CARTESIAN_POINT('Ctrl Pts',(-18.9965198485804,5.28407824547955,-9.16055201698359));
#36640=CARTESIAN_POINT('Ctrl Pts',(-18.8801742036722,6.85996538611778,-11.1780643879153));
#36641=CARTESIAN_POINT('Ctrl Pts',(-18.7885520913348,8.70047320199483,-12.0007213768745));
#36642=CARTESIAN_POINT('Ctrl Pts',(-18.7357118606335,9.829103193625,-12.0989141769127));
#36643=CARTESIAN_POINT('Ctrl Pts',(-18.7216535115683,10.1294126732152,-12.0987227687564));
#36644=CARTESIAN_POINT('Origin',(-26.8463464956315,10.1295,-7.));
#36645=CARTESIAN_POINT('',(-21.1904791369099,14.1758012177496,-3.89721939943572));
#36646=CARTESIAN_POINT('',(-21.0652864992102,14.1758012177496,-3.89721939943571));
#36647=CARTESIAN_POINT('',(-26.8463464956315,14.1758012177496,-3.89721939943572));
#36648=CARTESIAN_POINT('',(-20.0963464956032,10.1297172757599,-12.0989999953708));
#36649=CARTESIAN_POINT('Ctrl Pts',(-21.0652864992102,14.1758012177496,-3.89721939943571));
#36650=CARTESIAN_POINT('Ctrl Pts',(-21.0585700937333,14.0885055180282,-3.78337806111393));
#36651=CARTESIAN_POINT('Ctrl Pts',(-21.0518536882564,13.996453500271,-3.67329050358813));
#36652=CARTESIAN_POINT('Ctrl Pts',(-21.0451372827796,13.9000084618648,-3.56735277970396));
#36653=CARTESIAN_POINT('Ctrl Pts',(-21.0384166004951,13.8035020101215,-3.46134759782241));
#36654=CARTESIAN_POINT('Ctrl Pts',(-21.0316959182107,13.7025972199478,-3.35949778112184));
#36655=CARTESIAN_POINT('Ctrl Pts',(-21.0249752359262,13.5976933622283,-3.26216161368693));
#36656=CARTESIAN_POINT('Ctrl Pts',(-21.0182444490511,13.4926317808584,-3.16467910067446));
#36657=CARTESIAN_POINT('Ctrl Pts',(-21.0115136621759,13.3835593986938,-3.07172403740939));
#36658=CARTESIAN_POINT('Ctrl Pts',(-21.0047828753008,13.2709083136366,-2.9836142108838));
#36659=CARTESIAN_POINT('Ctrl Pts',(-21.000414602677,13.1977978943015,-2.92643103895467));
#36660=CARTESIAN_POINT('Ctrl Pts',(-20.9960463300532,13.1231807485872,-2.87128781070681));
#36661=CARTESIAN_POINT('Ctrl Pts',(-20.9916780574294,13.0471810287064,-2.81826131678142));
#36662=CARTESIAN_POINT('Ctrl Pts',(-20.9851848243432,12.9342109972609,-2.73943991197112));
#36663=CARTESIAN_POINT('Ctrl Pts',(-20.978691591257,12.8178257484995,-2.66504726072125));
#36664=CARTESIAN_POINT('Ctrl Pts',(-20.9721983581708,12.6984140612851,-2.59540222656693));
#36665=CARTESIAN_POINT('Ctrl Pts',(-20.9657135848688,12.5791579509767,-2.52584793025562));
#36666=CARTESIAN_POINT('Ctrl Pts',(-20.9592288115669,12.4568835846726,-2.46102915145838));
#36667=CARTESIAN_POINT('Ctrl Pts',(-20.9527440382649,12.3320115771828,-2.40122366793344));
#36668=CARTESIAN_POINT('Ctrl Pts',(-20.9462660723299,12.2072706536243,-2.34148096499519));
#36669=CARTESIAN_POINT('Ctrl Pts',(-20.9397881063949,12.0799378707507,-2.28674126299211));
#36670=CARTESIAN_POINT('Ctrl Pts',(-20.93331014046,11.9504610849406,-2.23723801485609));
#36671=CARTESIAN_POINT('Ctrl Pts',(-20.9268373376135,11.8210874951198,-2.18777422195239));
#36672=CARTESIAN_POINT('Ctrl Pts',(-20.920364534767,11.689573674354,-2.14353872349991));
#36673=CARTESIAN_POINT('Ctrl Pts',(-20.9138917319205,11.5563897947138,-2.10471793317875));
#36674=CARTESIAN_POINT('Ctrl Pts',(-20.9074218424767,11.4232658610167,-2.06591461606002));
#36675=CARTESIAN_POINT('Ctrl Pts',(-20.9009519530328,11.2884737466344,-2.03252127528968));
#36676=CARTESIAN_POINT('Ctrl Pts',(-20.894482063589,11.1525008815489,-2.00467516608278));
#36677=CARTESIAN_POINT('Ctrl Pts',(-20.8880136068028,11.0165581255649,-1.97683522296886));
#36678=CARTESIAN_POINT('Ctrl Pts',(-20.8815451500166,10.8794355313577,-1.9545401504312));
#36679=CARTESIAN_POINT('Ctrl Pts',(-20.8750766932304,10.7416323549945,-1.93787643572691));
#36680=CARTESIAN_POINT('Ctrl Pts',(-20.8686081907121,10.603828204361,-1.92121260320993));
#36681=CARTESIAN_POINT('Ctrl Pts',(-20.8621396881938,10.4653438603438,-1.91018025615939));
#36682=CARTESIAN_POINT('Ctrl Pts',(-20.8556711856755,10.3266848256198,-1.90481412070715));
#36683=CARTESIAN_POINT('Ctrl Pts',(-20.8492011591069,10.1879931213035,-1.89944672093442));
#36684=CARTESIAN_POINT('Ctrl Pts',(-20.8427311325383,10.0491270452882,-1.89974820296179));
#36685=CARTESIAN_POINT('Ctrl Pts',(-20.8362611059698,9.91059269125152,-1.90570116795486));
#36686=CARTESIAN_POINT('Ctrl Pts',(-20.8297838192035,9.77190288394293,-1.91166081293638));
#36687=CARTESIAN_POINT('Ctrl Pts',(-20.8233065324372,9.63354594344199,-1.92328458861938));
#36688=CARTESIAN_POINT('Ctrl Pts',(-20.8168292456709,9.49602388099765,-1.94050308759322));
#36689=CARTESIAN_POINT('Ctrl Pts',(-20.8103483111701,9.35842437193014,-1.9577312832992));
#36690=CARTESIAN_POINT('Ctrl Pts',(-20.8038673766692,9.2216610719723,-1.98056040833024));
#36691=CARTESIAN_POINT('Ctrl Pts',(-20.7973864421683,9.08622511032832,-2.00887001726257));
#36692=CARTESIAN_POINT('Ctrl Pts',(-20.7908944963578,8.95055903876625,-2.03722772510241));
#36693=CARTESIAN_POINT('Ctrl Pts',(-20.7844025505473,8.81622519910036,-2.07108441947365));
#36694=CARTESIAN_POINT('Ctrl Pts',(-20.7779106047368,8.68369966808348,-2.11026970066548));
#36695=CARTESIAN_POINT('Ctrl Pts',(-20.7716026590288,8.55493028537938,-2.1483443601778));
#36696=CARTESIAN_POINT('Ctrl Pts',(-20.7652947133209,8.42786837598066,-2.19144945063066));
#36697=CARTESIAN_POINT('Ctrl Pts',(-20.758986767613,8.30292988577589,-2.23938631919967));
#36698=CARTESIAN_POINT('Ctrl Pts',(-20.7522553481606,8.16960385187237,-2.29054135199688));
#36699=CARTESIAN_POINT('Ctrl Pts',(-20.7455239287083,8.0382566326181,-2.34736719785055));
#36700=CARTESIAN_POINT('Ctrl Pts',(-20.7387925092559,7.90939433831116,-2.4096915298711));
#36701=CARTESIAN_POINT('Ctrl Pts',(-20.7320693374223,7.7806899315173,-2.47193949949378));
#36702=CARTESIAN_POINT('Ctrl Pts',(-20.7253461655886,7.65446471705759,-2.53967237964706));
#36703=CARTESIAN_POINT('Ctrl Pts',(-20.718622993755,7.53120645650351,-2.6126691870997));
#36704=CARTESIAN_POINT('Ctrl Pts',(-20.7119066869372,7.40807405468524,-2.68559145767453));
#36705=CARTESIAN_POINT('Ctrl Pts',(-20.7051903801194,7.28790288938902,-2.76376676295887));
#36706=CARTESIAN_POINT('Ctrl Pts',(-20.6984740733016,7.17115757741741,-2.8469275095722));
#36707=CARTESIAN_POINT('Ctrl Pts',(-20.691763254633,7.05450766246991,-2.93002030238408));
#36708=CARTESIAN_POINT('Ctrl Pts',(-20.6850524359643,6.94127832456694,-3.0180902078119));
#36709=CARTESIAN_POINT('Ctrl Pts',(-20.6783416172957,6.83190647329252,-3.11082554613232));
#36710=CARTESIAN_POINT('Ctrl Pts',(-20.6716350376826,6.72260370946926,-3.20350230586892));
#36711=CARTESIAN_POINT('Ctrl Pts',(-20.6649284580695,6.6171538582951,-3.30083838763056));
#36712=CARTESIAN_POINT('Ctrl Pts',(-20.6582218784564,6.51596181868043,-3.40248101990474));
#36713=CARTESIAN_POINT('Ctrl Pts',(-20.651517616954,6.41480475581314,-3.50408851968543));
#36714=CARTESIAN_POINT('Ctrl Pts',(-20.6448133554515,6.31790283410827,-3.60999934380801));
#36715=CARTESIAN_POINT('Ctrl Pts',(-20.638109093949,6.22562508005278,-3.7198229301748));
#36716=CARTESIAN_POINT('Ctrl Pts',(-20.6314059106226,6.13336216605965,-3.82962885476722));
#36717=CARTESIAN_POINT('Ctrl Pts',(-20.6247027272961,6.04572217583957,-3.94334600500746));
#36718=CARTESIAN_POINT('Ctrl Pts',(-20.6179995439696,5.96303463779049,-4.06054981578045));
#36719=CARTESIAN_POINT('Ctrl Pts',(-20.6112961998865,5.88034511671715,-4.17775643735183));
#36720=CARTESIAN_POINT('Ctrl Pts',(-20.6045928558033,5.80260849649827,-4.29844958329638));
#36721=CARTESIAN_POINT('Ctrl Pts',(-20.5978895117201,5.73011159094298,-4.4221748262819));
#36722=CARTESIAN_POINT('Ctrl Pts',(-20.5911822561601,5.65757238262621,-4.54597226434116));
#36723=CARTESIAN_POINT('Ctrl Pts',(-20.5844750006002,5.5902791850645,-4.67280501527352));
#36724=CARTESIAN_POINT('Ctrl Pts',(-20.5777677450402,5.52847358717437,-4.80219269532544));
#36725=CARTESIAN_POINT('Ctrl Pts',(-20.5710584023763,5.46664875716989,-4.93162063708084));
#36726=CARTESIAN_POINT('Ctrl Pts',(-20.5643490597123,5.41031508149065,-5.06360475507181));
#36727=CARTESIAN_POINT('Ctrl Pts',(-20.5576397170484,5.35966624389706,-5.19764405869958));
#36728=CARTESIAN_POINT('Ctrl Pts',(-20.550923952482,5.3089689273521,-5.33181165914898));
#36729=CARTESIAN_POINT('Ctrl Pts',(-20.5442081879156,5.26396744082792,-5.4680380257195));
#36730=CARTESIAN_POINT('Ctrl Pts',(-20.5374924233492,5.22480597472622,-5.60580578166324));
#36731=CARTESIAN_POINT('Ctrl Pts',(-20.533760108165,5.20304182067926,-5.68237080747907));
#36732=CARTESIAN_POINT('Ctrl Pts',(-20.5300277929808,5.18308053177186,-5.75941167581817));
#36733=CARTESIAN_POINT('Ctrl Pts',(-20.5262954777966,5.16494003467883,-5.83683820956401));
#36734=CARTESIAN_POINT('Ctrl Pts',(-20.5195533162237,5.13217051860649,-5.97670372862882));
#36735=CARTESIAN_POINT('Ctrl Pts',(-20.5128111546507,5.10528904643073,-6.11806934857135));
#36736=CARTESIAN_POINT('Ctrl Pts',(-20.5060689930777,5.08442238336995,-6.26041035554948));
#36737=CARTESIAN_POINT('Ctrl Pts',(-20.4993317332857,5.06357089108348,-6.40264787577052));
#36738=CARTESIAN_POINT('Ctrl Pts',(-20.4925944734937,5.04872555025018,-6.54585900974967));
#36739=CARTESIAN_POINT('Ctrl Pts',(-20.4858572137016,5.03996208500966,-6.6895087571673));
#36740=CARTESIAN_POINT('Ctrl Pts',(-20.4791236997966,5.03120349221753,-6.83307863595294));
#36741=CARTESIAN_POINT('Ctrl Pts',(-20.4723901858916,5.02852005962299,-6.97708627789357));
#36742=CARTESIAN_POINT('Ctrl Pts',(-20.4656566719866,5.03193567501759,-7.1209915396491));
#36743=CARTESIAN_POINT('Ctrl Pts',(-20.4589254983211,5.03535010331164,-7.26484678698641));
#36744=CARTESIAN_POINT('Ctrl Pts',(-20.4521943246556,5.04485934699365,-7.40859935977456));
#36745=CARTESIAN_POINT('Ctrl Pts',(-20.4454631509901,5.0604351888477,-7.55170910844169));
#36746=CARTESIAN_POINT('Ctrl Pts',(-20.4387320860167,5.07601077918974,-7.69481654623394));
#36747=CARTESIAN_POINT('Ctrl Pts',(-20.4320010210433,5.09765273928879,-7.83728081633711));
#36748=CARTESIAN_POINT('Ctrl Pts',(-20.4252699560699,5.1252809594022,-7.97856670376547));
#36749=CARTESIAN_POINT('Ctrl Pts',(-20.4201632483428,5.14624186910953,-8.0857571314206));
#36750=CARTESIAN_POINT('Ctrl Pts',(-20.4150565406156,5.17064735025744,-8.19226935385371));
#36751=CARTESIAN_POINT('Ctrl Pts',(-20.4099498328884,5.19844276440152,-8.29787346812079));
#36752=CARTESIAN_POINT('Ctrl Pts',(-20.4026900647831,5.23795711921841,-8.44800177416587));
#36753=CARTESIAN_POINT('Ctrl Pts',(-20.3954302966777,5.28430937275062,-8.59623943939993));
#36754=CARTESIAN_POINT('Ctrl Pts',(-20.3881705285724,5.33729197690511,-8.74199404803374));
#36755=CARTESIAN_POINT('Ctrl Pts',(-20.3809033209466,5.39032887551694,-8.88789802017107));
#36756=CARTESIAN_POINT('Ctrl Pts',(-20.3736361133207,5.45000961080975,-9.03131361418626));
#36757=CARTESIAN_POINT('Ctrl Pts',(-20.3663689056949,5.51607819102709,-9.1716676109601));
#36758=CARTESIAN_POINT('Ctrl Pts',(-20.3590936962913,5.58221951804341,-9.31217614872688));
#36759=CARTESIAN_POINT('Ctrl Pts',(-20.3518184868878,5.65476264327944,-9.44961612005003));
#36760=CARTESIAN_POINT('Ctrl Pts',(-20.3445432774843,5.73340458011022,-9.583436869603));
#36761=CARTESIAN_POINT('Ctrl Pts',(-20.3372657453866,5.81207162428195,-9.7173003429662));
#36762=CARTESIAN_POINT('Ctrl Pts',(-20.329988213289,5.89684123596267,-9.84754207082839));
#36763=CARTESIAN_POINT('Ctrl Pts',(-20.3227106811913,5.98736594979328,-9.97363859776505));
#36764=CARTESIAN_POINT('Ctrl Pts',(-20.3154318373513,6.07790698029596,-10.0997578530329));
#36765=CARTESIAN_POINT('Ctrl Pts',(-20.3081529935112,6.17420503683368,-10.2217302093752));
#36766=CARTESIAN_POINT('Ctrl Pts',(-20.3008741496712,6.2758704453382,-10.3390627809967));
#36767=CARTESIAN_POINT('Ctrl Pts',(-20.2984508291075,6.30971756178363,-10.3781259124288));
#36768=CARTESIAN_POINT('Ctrl Pts',(-20.2960275085439,6.34415926105529,-10.4166750362839));
#36769=CARTESIAN_POINT('Ctrl Pts',(-20.2936041879802,6.3791801760683,-10.4546927820321));
#36770=CARTESIAN_POINT('Ctrl Pts',(-20.2868779809018,6.47638478448219,-10.5602154414733));
#36771=CARTESIAN_POINT('Ctrl Pts',(-20.2801517738235,6.57810999823997,-10.6617018342539));
#36772=CARTESIAN_POINT('Ctrl Pts',(-20.2734255667451,6.68398946099055,-10.7587575241793));
#36773=CARTESIAN_POINT('Ctrl Pts',(-20.2667029434128,6.7898125108012,-10.8557615025012));
#36774=CARTESIAN_POINT('Ctrl Pts',(-20.2599803200806,6.89978512979311,-10.9483392324725));
#36775=CARTESIAN_POINT('Ctrl Pts',(-20.2532576967484,7.01350428426586,-11.0361332608731));
#36776=CARTESIAN_POINT('Ctrl Pts',(-20.2465367266287,7.12719547317678,-11.1239056991614));
#36777=CARTESIAN_POINT('Ctrl Pts',(-20.2398157565091,7.24463107375143,-11.2068965514905));
#36778=CARTESIAN_POINT('Ctrl Pts',(-20.2330947863894,7.36537511122738,-11.2847887461656));
#36779=CARTESIAN_POINT('Ctrl Pts',(-20.2263749847876,7.48609815596555,-11.3626673983881));
#36780=CARTESIAN_POINT('Ctrl Pts',(-20.2196551831858,7.61012818104768,-11.435448961937));
#36781=CARTESIAN_POINT('Ctrl Pts',(-20.212935381584,7.73700061751279,-11.5028599472778));
#36782=CARTESIAN_POINT('Ctrl Pts',(-20.2062137509067,7.86390758762793,-11.570289281343));
#36783=CARTESIAN_POINT('Ctrl Pts',(-20.1994921202293,7.99365819072875,-11.6323449420533));
#36784=CARTESIAN_POINT('Ctrl Pts',(-20.1927704895519,8.12576338186563,-11.6887994801599));
#36785=CARTESIAN_POINT('Ctrl Pts',(-20.1875998407253,8.2273859767871,-11.732227422757));
#36786=CARTESIAN_POINT('Ctrl Pts',(-20.1824291918987,8.33040137579851,-11.7723418012303));
#36787=CARTESIAN_POINT('Ctrl Pts',(-20.1772585430721,8.43457914043762,-11.809058564815));
#36788=CARTESIAN_POINT('Ctrl Pts',(-20.1702026804407,8.57674002221321,-11.8591622266207));
#36789=CARTESIAN_POINT('Ctrl Pts',(-20.1631468178092,8.72111220267323,-11.9029539856882));
#36790=CARTESIAN_POINT('Ctrl Pts',(-20.1560909551778,8.86712880719496,-11.9402651721923));
#36791=CARTESIAN_POINT('Ctrl Pts',(-20.1490348696706,9.01315002398955,-11.9775775372567));
#36792=CARTESIAN_POINT('Ctrl Pts',(-20.1419787841634,9.16081547203784,-12.0084088496475));
#36793=CARTESIAN_POINT('Ctrl Pts',(-20.1349226986562,9.30954582988,-12.0326410719326));
#36794=CARTESIAN_POINT('Ctrl Pts',(-20.1278650246748,9.45830967007435,-12.0568787494039));
#36795=CARTESIAN_POINT('Ctrl Pts',(-20.1208073506934,9.60813859809027,-12.0745143189556));
#36796=CARTESIAN_POINT('Ctrl Pts',(-20.1137496767119,9.75844499148024,-12.085481214266));
#36797=CARTESIAN_POINT('Ctrl Pts',(-20.1079486163518,9.8819894429335,-12.094495461995));
#36798=CARTESIAN_POINT('Ctrl Pts',(-20.1021475559916,10.0058562501456,-12.0990052732534));
#36799=CARTESIAN_POINT('Ctrl Pts',(-20.0963464956315,10.1297172751558,-12.0989999953708));
#36800=CARTESIAN_POINT('Ctrl Pts',(-20.0963464956032,10.1297172757598,-12.0989999953708));
#36801=CARTESIAN_POINT('Ctrl Pts',(-20.089015871315,10.2862367018524,-12.0989933258518));
#36802=CARTESIAN_POINT('Ctrl Pts',(-20.0816852470269,10.4427270477282,-12.0917755131971));
#36803=CARTESIAN_POINT('Ctrl Pts',(-20.0743546227387,10.5985501666255,-12.0773805196369));
#36804=CARTESIAN_POINT('Ctrl Pts',(-20.0698740478804,10.6937913250079,-12.06858210852));
#36805=CARTESIAN_POINT('Ctrl Pts',(-20.0653934730221,10.7887832630484,-12.0571034512937));
#36806=CARTESIAN_POINT('Ctrl Pts',(-20.0609128981638,10.883381113265,-12.0429618546111));
#36807=CARTESIAN_POINT('Ctrl Pts',(-20.0540299000486,11.0287010432615,-12.0212377262588));
#36808=CARTESIAN_POINT('Ctrl Pts',(-20.0471469019333,11.1731216585732,-11.9932218786075));
#36809=CARTESIAN_POINT('Ctrl Pts',(-20.040263903818,11.3160889030018,-11.959012782326));
#36810=CARTESIAN_POINT('Ctrl Pts',(-20.0333828335523,11.4590161039285,-11.924813267624));
#36811=CARTESIAN_POINT('Ctrl Pts',(-20.0265017632867,11.6004904149984,-11.8844240428383));
#36812=CARTESIAN_POINT('Ctrl Pts',(-20.019620693021,11.7399691658932,-11.837994425969));
#36813=CARTESIAN_POINT('Ctrl Pts',(-20.0127398324751,11.8794436657853,-11.7915662241714));
#36814=CARTESIAN_POINT('Ctrl Pts',(-20.0058589719292,12.0169224023365,-11.7390981002918));
#36815=CARTESIAN_POINT('Ctrl Pts',(-19.9989781113832,12.1518786132926,-11.6807890087566));
#36816=CARTESIAN_POINT('Ctrl Pts',(-19.9920977747547,12.2868245485124,-11.6224843569492));
#36817=CARTESIAN_POINT('Ctrl Pts',(-19.9852174381262,12.419248029891,-11.5583397622004));
#36818=CARTESIAN_POINT('Ctrl Pts',(-19.9783371014977,12.5486430535138,-11.4886019969068));
#36819=CARTESIAN_POINT('Ctrl Pts',(-19.9714550222469,12.6780708497566,-11.4188465687294));
#36820=CARTESIAN_POINT('Ctrl Pts',(-19.964572942996,12.8044683557619,-11.3434953008952));
#36821=CARTESIAN_POINT('Ctrl Pts',(-19.9576908637452,12.9273544175526,-11.2628407967201));
#36822=CARTESIAN_POINT('Ctrl Pts',(-19.9533163269153,13.0054659276911,-11.2115734273474));
#36823=CARTESIAN_POINT('Ctrl Pts',(-19.9489417900855,13.0821591944104,-11.1581642466885));
#36824=CARTESIAN_POINT('Ctrl Pts',(-19.9445672532557,13.1573167585015,-11.1026974878654));
#36825=CARTESIAN_POINT('Ctrl Pts',(-19.9376178346047,13.2767125706703,-11.014582621476));
#36826=CARTESIAN_POINT('Ctrl Pts',(-19.9306684159537,13.392276360347,-10.9212397631479));
#36827=CARTESIAN_POINT('Ctrl Pts',(-19.9237189973027,13.5035591632226,-10.8230257340323));
#36828=CARTESIAN_POINT('Ctrl Pts',(-19.9167707096019,13.6148238559054,-10.724827688294));
#36829=CARTESIAN_POINT('Ctrl Pts',(-19.9098224219011,13.7218087066573,-10.6217602701984));
#36830=CARTESIAN_POINT('Ctrl Pts',(-19.9028741342004,13.8240989854157,-10.5142195914549));
#36831=CARTESIAN_POINT('Ctrl Pts',(-19.8959254836163,13.9263946064161,-10.4066732962605));
#36832=CARTESIAN_POINT('Ctrl Pts',(-19.8889768330322,14.0239949372702,-10.2946535083665));
#36833=CARTESIAN_POINT('Ctrl Pts',(-19.8820281824482,14.116522779692,-10.1785925115084));
#36834=CARTESIAN_POINT('Ctrl Pts',(-19.8750798802786,14.209045982645,-10.0625373341027));
#36835=CARTESIAN_POINT('Ctrl Pts',(-19.8681315781091,14.2964970028861,-9.9424416099158));
#36836=CARTESIAN_POINT('Ctrl Pts',(-19.8611832759396,14.3785395224088,-9.81876996879985));
#36837=CARTESIAN_POINT('Ctrl Pts',(-19.8542335347365,14.4605990334123,-9.69507271457101));
#36838=CARTESIAN_POINT('Ctrl Pts',(-19.8472837935334,14.5372476244609,-9.56779833651679));
#36839=CARTESIAN_POINT('Ctrl Pts',(-19.8403340523302,14.6081924776181,-9.43744019227688));
#36840=CARTESIAN_POINT('Ctrl Pts',(-19.8362965710027,14.6494081878925,-9.36170808112577));
#36841=CARTESIAN_POINT('Ctrl Pts',(-19.8322590896751,14.6886996717564,-9.28493568412992));
#36842=CARTESIAN_POINT('Ctrl Pts',(-19.8282216083475,14.7260166271649,-9.20722357186493));
#36843=CARTESIAN_POINT('Ctrl Pts',(-19.8212896270348,14.7900863816857,-9.07379907617413));
#36844=CARTESIAN_POINT('Ctrl Pts',(-19.8143576457221,14.8483539160099,-8.93755987242083));
#36845=CARTESIAN_POINT('Ctrl Pts',(-19.8074256644093,14.9005897744139,-8.79902845015939));
#36846=CARTESIAN_POINT('Ctrl Pts',(-19.800494999141,14.9528157157817,-8.66052332824371));
#36847=CARTESIAN_POINT('Ctrl Pts',(-19.7935643338727,14.9990121492195,-8.51972716550497));
#36848=CARTESIAN_POINT('Ctrl Pts',(-19.7866336686044,15.0389982277045,-8.37718123432116));
#36849=CARTESIAN_POINT('Ctrl Pts',(-19.7797027424108,15.0789858115835,-8.23462993657493));
#36850=CARTESIAN_POINT('Ctrl Pts',(-19.7727718162171,15.1127624801018,-8.09032905625727));
#36851=CARTESIAN_POINT('Ctrl Pts',(-19.7658408900234,15.1401974670158,-7.94483432094795));
#36852=CARTESIAN_POINT('Ctrl Pts',(-19.7589103257021,15.1676310215149,-7.79934718210023));
#36853=CARTESIAN_POINT('Ctrl Pts',(-19.7519797613807,15.1887234966507,-7.65266663834769));
#36854=CARTESIAN_POINT('Ctrl Pts',(-19.7450491970594,15.2033953868547,-7.50535789620315));
#36855=CARTESIAN_POINT('Ctrl Pts',(-19.7381170569175,15.2180706130446,-7.35801566008556));
#36856=CARTESIAN_POINT('Ctrl Pts',(-19.7311849167757,15.2263223045308,-7.21004526955849));
#36857=CARTESIAN_POINT('Ctrl Pts',(-19.7242527766338,15.228122843019,-7.06201697061806));
#36858=CARTESIAN_POINT('Ctrl Pts',(-19.7201271722356,15.2291944182259,-6.97391918426839));
#36859=CARTESIAN_POINT('Ctrl Pts',(-19.7160015678375,15.2279820313568,-6.88580095229293));
#36860=CARTESIAN_POINT('Ctrl Pts',(-19.7118759634393,15.2244886255794,-6.79778252989406));
#36861=CARTESIAN_POINT('Ctrl Pts',(-19.7049446779354,15.2186194751504,-6.64990581745022));
#36862=CARTESIAN_POINT('Ctrl Pts',(-19.6980133924316,15.2063069875029,-6.50225841772228));
#36863=CARTESIAN_POINT('Ctrl Pts',(-19.6910821069277,15.1875929083198,-6.35540933081153));
#36864=CARTESIAN_POINT('Ctrl Pts',(-19.6841521797915,15.1688824966527,-6.20858902284129));
#36865=CARTESIAN_POINT('Ctrl Pts',(-19.6772222526554,15.1437730382402,-6.06256704375094));
#36866=CARTESIAN_POINT('Ctrl Pts',(-19.6702923255192,15.1123580259662,-5.91790624571443));
#36867=CARTESIAN_POINT('Ctrl Pts',(-19.6633621941248,15.080942087741,-5.77324118382958));
#36868=CARTESIAN_POINT('Ctrl Pts',(-19.6564320627304,15.0432202905388,-5.62993770751543));
#36869=CARTESIAN_POINT('Ctrl Pts',(-19.649501931336,14.9993371489926,-5.48854800198896));
#36870=CARTESIAN_POINT('Ctrl Pts',(-19.6425721921158,14.9554564907815,-5.34716629766766));
#36871=CARTESIAN_POINT('Ctrl Pts',(-19.6356424528957,14.9054152848105,-5.20769846335097));
#36872=CARTESIAN_POINT('Ctrl Pts',(-19.6287127136755,14.8494077822419,-5.07068107169067));
#36873=CARTESIAN_POINT('Ctrl Pts',(-19.6217814385138,14.793387865894,-4.93363331081956));
#36874=CARTESIAN_POINT('Ctrl Pts',(-19.614850163352,14.7313991358925,-4.79903738439233));
#36875=CARTESIAN_POINT('Ctrl Pts',(-19.6079188881903,14.6636840544645,-4.66741003169438));
#36876=CARTESIAN_POINT('Ctrl Pts',(-19.6037893649706,14.6233406840806,-4.58898893360879));
#36877=CARTESIAN_POINT('Ctrl Pts',(-19.5996598417508,14.5809656252748,-4.5116211384534));
#36878=CARTESIAN_POINT('Ctrl Pts',(-19.5955303185311,14.5366179506424,-4.43541185194857));
#36879=CARTESIAN_POINT('Ctrl Pts',(-19.5885944518774,14.4621324613293,-4.30741222079398));
#36880=CARTESIAN_POINT('Ctrl Pts',(-19.5816585852237,14.3820543577257,-4.18263838139734));
#36881=CARTESIAN_POINT('Ctrl Pts',(-19.5747227185701,14.296687716155,-4.06157396922663));
#36882=CARTESIAN_POINT('Ctrl Pts',(-19.5715384281261,14.2574954717591,-4.00599270303001));
#36883=CARTESIAN_POINT('Ctrl Pts',(-19.5683541376821,14.2171891408564,-3.95119292358269));
#36884=CARTESIAN_POINT('Ctrl Pts',(-19.5651698472381,14.1758012177496,-3.89721939943573));
#36885=CARTESIAN_POINT('',(-20.2216535043684,10.1252586289357,-12.098998236004));
#36886=CARTESIAN_POINT('Ctrl Pts',(-20.2216531624029,10.1252652855325,-12.0997546424994));
#36887=CARTESIAN_POINT('Ctrl Pts',(-20.1623123258533,11.389567257658,-12.087821313962));
#36888=CARTESIAN_POINT('Ctrl Pts',(-20.0641896076676,13.4904584433699,-11.2892797426427));
#36889=CARTESIAN_POINT('Ctrl Pts',(-19.9272850078459,15.1309521650029,-8.75245213992368));
#36890=CARTESIAN_POINT('Ctrl Pts',(-19.8109393629377,15.377488382025,-6.21192549167328));
#36891=CARTESIAN_POINT('Ctrl Pts',(-19.7320103642151,14.7099924706043,-4.60515278330599));
#36892=CARTESIAN_POINT('Ctrl Pts',(-19.6918632471286,14.1938652656919,-3.92011968463998));
#36893=CARTESIAN_POINT('Ctrl Pts',(-19.6904980116781,14.1761130084766,-3.89698020567888));
#36894=CARTESIAN_POINT('Ctrl Pts',(-21.1904791369099,14.1758012177496,-3.89721939943572));
#36895=CARTESIAN_POINT('Ctrl Pts',(-21.1834164152794,14.084049569575,-3.7775671089476));
#36896=CARTESIAN_POINT('Ctrl Pts',(-21.1763536936489,13.9869830080975,-3.66198180115258));
#36897=CARTESIAN_POINT('Ctrl Pts',(-21.1692909720185,13.8849805995519,-3.55091802556254));
#36898=CARTESIAN_POINT('Ctrl Pts',(-21.1622286881234,13.7829845129405,-3.43986113351475));
#36899=CARTESIAN_POINT('Ctrl Pts',(-21.1551664042283,13.6760533941024,-3.33332543922702));
#36900=CARTESIAN_POINT('Ctrl Pts',(-21.1481041203332,13.5646048872596,-3.23173044839874));
#36901=CARTESIAN_POINT('Ctrl Pts',(-21.1410431083921,13.453176452872,-3.13015375535622));
#36902=CARTESIAN_POINT('Ctrl Pts',(-21.133982096451,13.3372324800264,-3.03351619308533));
#36903=CARTESIAN_POINT('Ctrl Pts',(-21.12692108451,13.217225829596,-2.94219884651238));
#36904=CARTESIAN_POINT('Ctrl Pts',(-21.1198610202629,13.0972352858636,-2.85089375610116));
#36905=CARTESIAN_POINT('Ctrl Pts',(-21.1128009560159,12.9731833943003,-2.76490764052895));
#36906=CARTESIAN_POINT('Ctrl Pts',(-21.1057408917689,12.8455548055735,-2.68458028772159));
#36907=CARTESIAN_POINT('Ctrl Pts',(-21.1007410801552,12.7551705147481,-2.62769388875879));
#36908=CARTESIAN_POINT('Ctrl Pts',(-21.0957412685416,12.6629931066556,-2.57364462842989));
#36909=CARTESIAN_POINT('Ctrl Pts',(-21.0907414569279,12.5692033929549,-2.52253996618568));
#36910=CARTESIAN_POINT('Ctrl Pts',(-21.0840199577374,12.4431171454252,-2.45383738847869));
#36911=CARTESIAN_POINT('Ctrl Pts',(-21.0772984585468,12.314077704637,-2.39043779766261));
#36912=CARTESIAN_POINT('Ctrl Pts',(-21.0705769593563,12.1825638082227,-2.33258851188732));
#36913=CARTESIAN_POINT('Ctrl Pts',(-21.0638571099993,12.0510821927081,-2.27475342557725));
#36914=CARTESIAN_POINT('Ctrl Pts',(-21.0571372606424,11.917127668362,-2.22246607754469));
#36915=CARTESIAN_POINT('Ctrl Pts',(-21.0504174112854,11.7812007609424,-2.17592645202187));
#36916=CARTESIAN_POINT('Ctrl Pts',(-21.0436962436786,11.6452471883978,-2.12937769670307));
#36917=CARTESIAN_POINT('Ctrl Pts',(-21.0369750760718,11.5073208059466,-2.08857904163402));
#36918=CARTESIAN_POINT('Ctrl Pts',(-21.030253908465,11.3679394888552,-2.05368130500631));
#36919=CARTESIAN_POINT('Ctrl Pts',(-21.0235322550113,11.2285480964326,-2.01878104575747));
#36920=CARTESIAN_POINT('Ctrl Pts',(-21.0168106015575,11.0877019181292,-1.98978263908411));
#36921=CARTESIAN_POINT('Ctrl Pts',(-21.0100889481037,10.9459306945814,-1.96678612406095));
#36922=CARTESIAN_POINT('Ctrl Pts',(-21.00336283355,10.8040653787671,-1.94377434646078));
#36923=CARTESIAN_POINT('Ctrl Pts',(-20.9966367189962,10.6612741552293,-1.92677247459321));
#36924=CARTESIAN_POINT('Ctrl Pts',(-20.9899106044424,10.5180941451527,-1.91582891806805));
#36925=CARTESIAN_POINT('Ctrl Pts',(-20.9847390069682,10.4080054197,-1.90741459969268));
#36926=CARTESIAN_POINT('Ctrl Pts',(-20.9795674094939,10.297687025457,-1.90258079609333));
#36927=CARTESIAN_POINT('Ctrl Pts',(-20.9743958120197,10.1873835904047,-1.90132855638237));
#36928=CARTESIAN_POINT('Ctrl Pts',(-20.9671170684873,10.0321374757399,-1.89956609676666));
#36929=CARTESIAN_POINT('Ctrl Pts',(-20.959838324955,9.87682543926592,-1.90489862489669));
#36930=CARTESIAN_POINT('Ctrl Pts',(-20.9525595814226,9.7220753784726,-1.91730325734721));
#36931=CARTESIAN_POINT('Ctrl Pts',(-20.9452817167969,9.56734400371569,-1.92970639194104));
#36932=CARTESIAN_POINT('Ctrl Pts',(-20.9380038521713,9.41317472155407,-1.94917990409636));
#36933=CARTESIAN_POINT('Ctrl Pts',(-20.9307259875456,9.26019127590926,-1.97564896307795));
#36934=CARTESIAN_POINT('Ctrl Pts',(-20.9234524716548,9.10729924230271,-2.00210220603041));
#36935=CARTESIAN_POINT('Ctrl Pts',(-20.9161789557639,8.95559187901386,-2.03554260156708));
#36936=CARTESIAN_POINT('Ctrl Pts',(-20.9089054398731,8.80568411965762,-2.07584397942619));
#36937=CARTESIAN_POINT('Ctrl Pts',(-20.9016367742746,8.65587632522299,-2.11611848259851));
#36938=CARTESIAN_POINT('Ctrl Pts',(-20.894368108676,8.50786598368629,-2.16324476993341));
#36939=CARTESIAN_POINT('Ctrl Pts',(-20.8870994430774,8.36225537649466,-2.21704615946469));
#36940=CARTESIAN_POINT('Ctrl Pts',(-20.8798397779555,8.21682507266881,-2.27078092904428));
#36941=CARTESIAN_POINT('Ctrl Pts',(-20.8725801128336,8.07378880792323,-2.33117421095855));
#36942=CARTESIAN_POINT('Ctrl Pts',(-20.8653204477117,7.93373154482647,-2.39800022911074));
#36943=CARTESIAN_POINT('Ctrl Pts',(-20.862897020845,7.88697752400415,-2.42030814071116));
#36944=CARTESIAN_POINT('Ctrl Pts',(-20.8604735939782,7.84055533141693,-2.44333248635513));
#36945=CARTESIAN_POINT('Ctrl Pts',(-20.8580501671115,7.79448628016983,-2.46706365275169));
#36946=CARTESIAN_POINT('Ctrl Pts',(-20.8513195102469,7.6665373082926,-2.53297294021673));
#36947=CARTESIAN_POINT('Ctrl Pts',(-20.8445888533824,7.54135727855362,-2.6043155917558));
#36948=CARTESIAN_POINT('Ctrl Pts',(-20.8378581965178,7.41941799831926,-2.68082686800284));
#36949=CARTESIAN_POINT('Ctrl Pts',(-20.8311277589209,7.29748269055658,-2.75733565170707));
#36950=CARTESIAN_POINT('Ctrl Pts',(-20.824397321324,7.17878823114962,-2.83901252941112));
#36951=CARTESIAN_POINT('Ctrl Pts',(-20.8176668837272,7.06377874695439,-2.92554860151401));
#36952=CARTESIAN_POINT('Ctrl Pts',(-20.8109330039709,6.94871044325873,-3.01212893091069));
#36953=CARTESIAN_POINT('Ctrl Pts',(-20.8041991242146,6.83733117429048,-3.10357320184736));
#36954=CARTESIAN_POINT('Ctrl Pts',(-20.7974652444583,6.73005358099377,-3.19953094417206));
#36955=CARTESIAN_POINT('Ctrl Pts',(-20.7907296988947,6.62274944968287,-3.29551242423964));
#36956=CARTESIAN_POINT('Ctrl Pts',(-20.7839941533312,6.51954928410615,-3.3960093515451));
#36957=CARTESIAN_POINT('Ctrl Pts',(-20.7772586077676,6.42082972916417,-3.50063351130258));
#36958=CARTESIAN_POINT('Ctrl Pts',(-20.7705168109826,6.32201855316575,-3.60535477214659));
#36959=CARTESIAN_POINT('Ctrl Pts',(-20.7637750141976,6.22769654299804,-3.7142106479578));
#36960=CARTESIAN_POINT('Ctrl Pts',(-20.7570332174125,6.13820130284807,-3.82677833895687));
#36961=CARTESIAN_POINT('Ctrl Pts',(-20.7519236523428,6.07037342734832,-3.91209267877634));
#36962=CARTESIAN_POINT('Ctrl Pts',(-20.746814087273,6.00531726134624,-3.99953837678175));
#36963=CARTESIAN_POINT('Ctrl Pts',(-20.7417045222033,5.9431632940884,-4.08892013425649));
#36964=CARTESIAN_POINT('Ctrl Pts',(-20.7349885840485,5.86146902178138,-4.20640221877302));
#36965=CARTESIAN_POINT('Ctrl Pts',(-20.7282726458937,5.78464992982721,-4.32743176090145));
#36966=CARTESIAN_POINT('Ctrl Pts',(-20.7215567077389,5.7130174542218,-4.45157246074436));
#36967=CARTESIAN_POINT('Ctrl Pts',(-20.7148461284493,5.64144213649508,-4.57561410469117));
#36968=CARTESIAN_POINT('Ctrl Pts',(-20.7081355491596,5.57504537611949,-4.7027616427771));
#36969=CARTESIAN_POINT('Ctrl Pts',(-20.70142496987,5.51409512437858,-4.83255015419271));
#36970=CARTESIAN_POINT('Ctrl Pts',(-20.6947183775871,5.45318108546705,-4.96226155338837));
#36971=CARTESIAN_POINT('Ctrl Pts',(-20.6880117853042,5.39770726562999,-5.09461046626493));
#36972=CARTESIAN_POINT('Ctrl Pts',(-20.6813051930213,5.34789546567046,-5.22910783013783));
#36973=CARTESIAN_POINT('Ctrl Pts',(-20.6746012193564,5.29810311494418,-5.36355267893188));
#36974=CARTESIAN_POINT('Ctrl Pts',(-20.6678972456915,5.25396850735601,-5.50014396102834));
#36975=CARTESIAN_POINT('Ctrl Pts',(-20.6611932720266,5.21566509698604,-5.63837319873549));
#36976=CARTESIAN_POINT('Ctrl Pts',(-20.6544892305015,5.17736129889407,-5.77660383565271));
#36977=CARTESIAN_POINT('Ctrl Pts',(-20.6477851889764,5.14488892341433,-5.91647210752719));
#36978=CARTESIAN_POINT('Ctrl Pts',(-20.6410811474513,5.11837144179936,-6.05745473679721));
#36979=CARTESIAN_POINT('Ctrl Pts',(-20.6343767553807,5.09185257362039,-6.19844473786225));
#36980=CARTESIAN_POINT('Ctrl Pts',(-20.6276723633102,5.07128928850261,-6.34054884896783));
#36981=CARTESIAN_POINT('Ctrl Pts',(-20.6209679712396,5.05675377886097,-6.48323431236225));
#36982=CARTESIAN_POINT('Ctrl Pts',(-20.6142619894755,5.0422148226719,-6.62595360822839));
#36983=CARTESIAN_POINT('Ctrl Pts',(-20.6075560077115,5.03370652666764,-6.76925416302939));
#36984=CARTESIAN_POINT('Ctrl Pts',(-20.6008500259474,5.03124911809655,-6.91259894067772));
#36985=CARTESIAN_POINT('Ctrl Pts',(-20.5941412144946,5.02879067258535,-7.05600420478707));
#36986=CARTESIAN_POINT('Ctrl Pts',(-20.5874324030418,5.03238820704158,-7.19945335934861));
#36987=CARTESIAN_POINT('Ctrl Pts',(-20.5807235915889,5.04200983658002,-7.34241033440146));
#36988=CARTESIAN_POINT('Ctrl Pts',(-20.5740068318481,5.051642865378,-7.48553667823489));
#36989=CARTESIAN_POINT('Ctrl Pts',(-20.5672900721072,5.06731422089053,-7.62816930839583));
#36990=CARTESIAN_POINT('Ctrl Pts',(-20.5605733123664,5.0889401403371,-7.76977743611718));
#36991=CARTESIAN_POINT('Ctrl Pts',(-20.5538521696222,5.11058017171852,-7.91147796983666));
#36992=CARTESIAN_POINT('Ctrl Pts',(-20.5471310268781,5.13818244351978,-8.05215230563819));
#36993=CARTESIAN_POINT('Ctrl Pts',(-20.540409884134,5.1716123485166,-8.1912812578348));
#36994=CARTESIAN_POINT('Ctrl Pts',(-20.5336788198585,5.2050916016471,-8.3306155876456));
#36995=CARTESIAN_POINT('Ctrl Pts',(-20.526947755583,5.24441557450129,-8.46839962056696));
#36996=CARTESIAN_POINT('Ctrl Pts',(-20.5202166913075,5.28939995726636,-8.60412985020847));
#36997=CARTESIAN_POINT('Ctrl Pts',(-20.5164822050006,5.31435790664599,-8.6794348336817));
#36998=CARTESIAN_POINT('Ctrl Pts',(-20.5127477186938,5.34105737182245,-8.75410796890097));
#36999=CARTESIAN_POINT('Ctrl Pts',(-20.5090132323869,5.36946062600318,-8.82806623457683));
#37000=CARTESIAN_POINT('Ctrl Pts',(-20.502520006881,5.41884592811497,-8.95665893986427));
#37001=CARTESIAN_POINT('Ctrl Pts',(-20.4960267813751,5.47354175068292,-9.08349785559962));
#37002=CARTESIAN_POINT('Ctrl Pts',(-20.4895335558692,5.53340481851077,-9.20810101279165));
#37003=CARTESIAN_POINT('Ctrl Pts',(-20.4830487901846,5.59318989261193,-9.33254182841081));
#37004=CARTESIAN_POINT('Ctrl Pts',(-20.4765640245,5.65812865411813,-9.45475232040486));
#37005=CARTESIAN_POINT('Ctrl Pts',(-20.4700792588154,5.72802843516658,-9.57426670412428));
#37006=CARTESIAN_POINT('Ctrl Pts',(-20.4636013005293,5.79785483875086,-9.6936556273304));
#37007=CARTESIAN_POINT('Ctrl Pts',(-20.4571233422431,5.87263170391494,-9.81035372750212));
#37008=CARTESIAN_POINT('Ctrl Pts',(-20.450645383957,5.95211895982359,-9.92391666180394));
#37009=CARTESIAN_POINT('Ctrl Pts',(-20.4441725887856,6.03154286215628,-10.0373890832568));
#37010=CARTESIAN_POINT('Ctrl Pts',(-20.4376997936142,6.11566945835049,-10.1477309823946));
#37011=CARTESIAN_POINT('Ctrl Pts',(-20.4312269984427,6.20421383286382,-10.2545244669674));
#37012=CARTESIAN_POINT('Ctrl Pts',(-20.4247571166935,6.29271835332039,-10.3612698835108));
#37013=CARTESIAN_POINT('Ctrl Pts',(-20.4182872349443,6.38563644465789,-10.4644697516912));
#37014=CARTESIAN_POINT('Ctrl Pts',(-20.4118173531951,6.48264134772176,-10.5637372195917));
#37015=CARTESIAN_POINT('Ctrl Pts',(-20.4053489041175,6.57962477030434,-10.6629827059953));
#37016=CARTESIAN_POINT('Ctrl Pts',(-20.39888045504,6.68069292567982,-10.7582972360804));
#37017=CARTESIAN_POINT('Ctrl Pts',(-20.3924120059624,6.78548080763127,-10.8493293754977));
#37018=CARTESIAN_POINT('Ctrl Pts',(-20.3859435111625,6.89026943027771,-10.9403621583773));
#37019=CARTESIAN_POINT('Ctrl Pts',(-20.3794750163626,6.99877752904281,-11.0271122270101));
#37020=CARTESIAN_POINT('Ctrl Pts',(-20.3730065215627,7.11060591490089,-11.1092675141628));
#37021=CARTESIAN_POINT('Ctrl Pts',(-20.3665365027179,7.22246064869354,-11.1914421579583));
#37022=CARTESIAN_POINT('Ctrl Pts',(-20.3600664838731,7.33763690188177,-11.2690196300627));
#37023=CARTESIAN_POINT('Ctrl Pts',(-20.3535964650283,7.45570578264319,-11.3417307013712));
#37024=CARTESIAN_POINT('Ctrl Pts',(-20.347119185956,7.57390715249828,-11.4145233642377));
#37025=CARTESIAN_POINT('Ctrl Pts',(-20.3406419068838,7.69500729020921,-11.4824385099356));
#37026=CARTESIAN_POINT('Ctrl Pts',(-20.3341646278115,7.81855153687926,-11.5452522703146));
#37027=CARTESIAN_POINT('Ctrl Pts',(-20.3276837010034,7.9421653585622,-11.6081014048069));
#37028=CARTESIAN_POINT('Ctrl Pts',(-20.3212027741953,8.06822566499679,-11.6658432682261));
#37029=CARTESIAN_POINT('Ctrl Pts',(-20.3147218473872,8.19625820555243,-11.7183023604048));
#37030=CARTESIAN_POINT('Ctrl Pts',(-20.3082299091909,8.3245082791934,-11.7708505829571));
#37031=CARTESIAN_POINT('Ctrl Pts',(-20.3017379709947,8.45473690394363,-11.818097967878));
#37032=CARTESIAN_POINT('Ctrl Pts',(-20.2952460327984,8.58645429869657,-11.8599188227468));
#37033=CARTESIAN_POINT('Ctrl Pts',(-20.2889380027224,8.71444031188824,-11.9005549474817));
#37034=CARTESIAN_POINT('Ctrl Pts',(-20.2826299726465,8.84383154608124,-11.9360678348261));
#37035=CARTESIAN_POINT('Ctrl Pts',(-20.2763219425705,8.97417216558045,-11.9663888888221));
#37036=CARTESIAN_POINT('Ctrl Pts',(-20.2664274954747,9.17861766576668,-12.0139489132734));
#37037=CARTESIAN_POINT('Ctrl Pts',(-20.2565330483789,9.38595698020578,-12.0488706803317));
#37038=CARTESIAN_POINT('Ctrl Pts',(-20.2466386012831,9.59491891455191,-12.0708997291488));
#37039=CARTESIAN_POINT('Ctrl Pts',(-20.2383102356448,9.77080659951878,-12.0894420460094));
#37040=CARTESIAN_POINT('Ctrl Pts',(-20.2299818700066,9.94784426009558,-12.0988506618854));
#37041=CARTESIAN_POINT('Ctrl Pts',(-20.2216535043684,10.1252586289357,-12.098998236004));
#37042=CARTESIAN_POINT('Origin',(-26.8463464956315,10.1295,-7.));
#37043=CARTESIAN_POINT('',(-22.6904763727661,14.1758012177496,-3.89721939943571));
#37044=CARTESIAN_POINT('',(-22.5651720736883,14.1754919335057,-3.89745664672315));
#37045=CARTESIAN_POINT('',(-26.8463464956315,14.1758012177496,-3.89721939943572));
#37046=CARTESIAN_POINT('',(-23.2216535038438,10.1296134641623,-12.0989489123299));
#37047=CARTESIAN_POINT('Ctrl Pts',(-23.2216535036443,10.1296134695606,-12.0989999987375));
#37048=CARTESIAN_POINT('Ctrl Pts',(-23.2144616176573,10.2832380933687,-12.0989965800831));
#37049=CARTESIAN_POINT('Ctrl Pts',(-23.2072697316703,10.4368320308009,-12.092046129591));
#37050=CARTESIAN_POINT('Ctrl Pts',(-23.2000778456833,10.589781612833,-12.0781829266863));
#37051=CARTESIAN_POINT('Ctrl Pts',(-23.1950395855473,10.6969301109268,-12.0684710899472));
#37052=CARTESIAN_POINT('Ctrl Pts',(-23.1900013254114,10.80376240697,-12.0553677903385));
#37053=CARTESIAN_POINT('Ctrl Pts',(-23.1849630652754,10.9100690396704,-12.0388999766128));
#37054=CARTESIAN_POINT('Ctrl Pts',(-23.1780322210911,11.0563089493057,-12.016246154081));
#37055=CARTESIAN_POINT('Ctrl Pts',(-23.1711013769068,11.2015880256627,-11.9872177039362));
#37056=CARTESIAN_POINT('Ctrl Pts',(-23.1641705327225,11.3453457830432,-11.9519208426484));
#37057=CARTESIAN_POINT('Ctrl Pts',(-23.1572410393046,11.4890755231802,-11.9166308604382));
#37058=CARTESIAN_POINT('Ctrl Pts',(-23.1503115458867,11.6312842144825,-11.875074983332));
#37059=CARTESIAN_POINT('Ctrl Pts',(-23.1433820524688,11.7714233688928,-11.8274101390584));
#37060=CARTESIAN_POINT('Ctrl Pts',(-23.1364523390414,11.9115669726828,-11.779743781439));
#37061=CARTESIAN_POINT('Ctrl Pts',(-23.129522625614,12.0496405935019,-11.725968171853));
#37062=CARTESIAN_POINT('Ctrl Pts',(-23.1225929121865,12.1851121473728,-11.666289714492));
#37063=CARTESIAN_POINT('Ctrl Pts',(-23.1156635809782,12.3205762291,-11.6066145487888));
#37064=CARTESIAN_POINT('Ctrl Pts',(-23.1087342497699,12.453438228391,-11.5410373210932));
#37065=CARTESIAN_POINT('Ctrl Pts',(-23.1018049185616,12.5831872350453,-11.4698120712817));
#37066=CARTESIAN_POINT('Ctrl Pts',(-23.0948740323597,12.7129653583441,-11.3985708379931));
#37067=CARTESIAN_POINT('Ctrl Pts',(-23.0879431461578,12.8396288027836,-11.3216792094331));
#37068=CARTESIAN_POINT('Ctrl Pts',(-23.0810122599559,12.9626918508012,-11.2394368654992));
#37069=CARTESIAN_POINT('Ctrl Pts',(-23.0768806467596,13.0360517211474,-11.1904108760966));
#37070=CARTESIAN_POINT('Ctrl Pts',(-23.0727490335634,13.1081326835169,-11.1394843440002));
#37071=CARTESIAN_POINT('Ctrl Pts',(-23.0686174203672,13.1788367906057,-11.0867280478958));
#37072=CARTESIAN_POINT('Ctrl Pts',(-23.0616832477982,13.2975009676742,-10.9981860562044));
#37073=CARTESIAN_POINT('Ctrl Pts',(-23.0547490752291,13.4123264715572,-10.9044570184215));
#37074=CARTESIAN_POINT('Ctrl Pts',(-23.0478149026601,13.5228675281008,-10.8058977678376));
#37075=CARTESIAN_POINT('Ctrl Pts',(-23.0408820410097,13.6333876866445,-10.7073571500701));
#37076=CARTESIAN_POINT('Ctrl Pts',(-23.0339491793593,13.7396247673742,-10.6039883612046));
#37077=CARTESIAN_POINT('Ctrl Pts',(-23.027016317709,13.8411673613832,-10.4961874089417));
#37078=CARTESIAN_POINT('Ctrl Pts',(-23.0200832090312,13.9427135734955,-10.3883826155816));
#37079=CARTESIAN_POINT('Ctrl Pts',(-23.0131501003533,14.0395647351762,-10.2761455810761));
#37080=CARTESIAN_POINT('Ctrl Pts',(-23.0062169916755,14.131347111674,-10.1599083364532));
#37081=CARTESIAN_POINT('Ctrl Pts',(-22.9992842580324,14.2231245233599,-10.0436773794868));
#37082=CARTESIAN_POINT('Ctrl Pts',(-22.9923515243894,14.3098334944501,-9.9234469053268));
#37083=CARTESIAN_POINT('Ctrl Pts',(-22.9854187907463,14.3911413124602,-9.79968111111478));
#37084=CARTESIAN_POINT('Ctrl Pts',(-22.9784845207415,14.4724671490789,-9.67588788919075));
#37085=CARTESIAN_POINT('Ctrl Pts',(-22.9715502507368,14.5483892594452,-9.54855805804282));
#37086=CARTESIAN_POINT('Ctrl Pts',(-22.9646159807321,14.6186185668019,-9.41818433813362));
#37087=CARTESIAN_POINT('Ctrl Pts',(-22.960501245641,14.6602920227245,-9.34082171454237));
#37088=CARTESIAN_POINT('Ctrl Pts',(-22.95638651055,14.6999618159018,-9.26238781469777));
#37089=CARTESIAN_POINT('Ctrl Pts',(-22.952271775459,14.7375752110852,-9.18298965846895));
#37090=CARTESIAN_POINT('Ctrl Pts',(-22.9453381247487,14.800956726167,-9.04919755031274));
#37091=CARTESIAN_POINT('Ctrl Pts',(-22.9384044740384,14.8585183931822,-8.91262019456305));
#37092=CARTESIAN_POINT('Ctrl Pts',(-22.9314708233281,14.9100334467114,-8.77378154372893));
#37093=CARTESIAN_POINT('Ctrl Pts',(-22.92453848664,14.9615387374293,-8.63496920472942));
#37094=CARTESIAN_POINT('Ctrl Pts',(-22.917606149952,15.0069995860105,-8.49389673540899));
#37095=CARTESIAN_POINT('Ctrl Pts',(-22.9106738132639,15.0462379353463,-8.35110661131037));
#37096=CARTESIAN_POINT('Ctrl Pts',(-22.9037412290525,15.085477685711,-8.20831138880432));
#37097=CARTESIAN_POINT('Ctrl Pts',(-22.8968086448412,15.1184944014449,-8.06379870665251));
#37098=CARTESIAN_POINT('Ctrl Pts',(-22.8898760606299,15.1451601822359,-7.91812522911281));
#37099=CARTESIAN_POINT('Ctrl Pts',(-22.8829438499011,15.1718245264478,-7.77245959951431));
#37100=CARTESIAN_POINT('Ctrl Pts',(-22.8760116391724,15.1921385617596,-7.62563362499968));
#37101=CARTESIAN_POINT('Ctrl Pts',(-22.8690794284437,15.2060256970908,-7.47821318130803));
#37102=CARTESIAN_POINT('Ctrl Pts',(-22.8621456743553,15.2199159241982,-7.33075991651844));
#37103=CARTESIAN_POINT('Ctrl Pts',(-22.855211920267,15.2273763612686,-7.18271224732234));
#37104=CARTESIAN_POINT('Ctrl Pts',(-22.8482781661786,15.2283823298558,-7.03464081817565));
#37105=CARTESIAN_POINT('Ctrl Pts',(-22.8441608209693,15.2289796859043,-6.9467142517509));
#37106=CARTESIAN_POINT('Ctrl Pts',(-22.8400434757601,15.2273021079282,-6.85877936703632));
#37107=CARTESIAN_POINT('Ctrl Pts',(-22.8359261305508,15.223353127859,-6.77095565538246));
#37108=CARTESIAN_POINT('Ctrl Pts',(-22.8289927904143,15.2167033036104,-6.62306626695431));
#37109=CARTESIAN_POINT('Ctrl Pts',(-22.8220594502778,15.2036075003542,-6.47544108085083));
#37110=CARTESIAN_POINT('Ctrl Pts',(-22.8151261101414,15.1841106766401,-6.32864919185574));
#37111=CARTESIAN_POINT('Ctrl Pts',(-22.8081940903344,15.1646175657443,-6.18188525672731));
#37112=CARTESIAN_POINT('Ctrl Pts',(-22.8012620705275,15.1387259098974,-6.03595462967193));
#37113=CARTESIAN_POINT('Ctrl Pts',(-22.7943300507205,15.1065323796292,-5.8914199658471));
#37114=CARTESIAN_POINT('Ctrl Pts',(-22.7873977897876,15.0743377295293,-5.74688027447465));
#37115=CARTESIAN_POINT('Ctrl Pts',(-22.7804655288547,15.0358408349672,-5.60373696693589));
#37116=CARTESIAN_POINT('Ctrl Pts',(-22.7735332679218,14.9911893286948,-5.46254174975221));
#37117=CARTESIAN_POINT('Ctrl Pts',(-22.7666013833261,14.9465402464547,-5.32135419774698));
#37118=CARTESIAN_POINT('Ctrl Pts',(-22.7596694987304,14.8957373216521,-5.18211483944176));
#37119=CARTESIAN_POINT('Ctrl Pts',(-22.7527376141347,14.8389778369684,-5.04535949517476));
#37120=CARTESIAN_POINT('Ctrl Pts',(-22.7458041877542,14.7822057278808,-4.9085737338822));
#37121=CARTESIAN_POINT('Ctrl Pts',(-22.7388707613737,14.7194745384637,-4.77427339605927));
#37122=CARTESIAN_POINT('Ctrl Pts',(-22.7319373349933,14.6510296539597,-4.64297420710704));
#37123=CARTESIAN_POINT('Ctrl Pts',(-22.7278183852097,14.6103685108622,-4.56497312420261));
#37124=CARTESIAN_POINT('Ctrl Pts',(-22.7236994354262,14.5676917913382,-4.48803079706271));
#37125=CARTESIAN_POINT('Ctrl Pts',(-22.7195804856426,14.5230586438665,-4.4122512790253));
#37126=CARTESIAN_POINT('Ctrl Pts',(-22.7126467713343,14.4479245661251,-4.28468635201598));
#37127=CARTESIAN_POINT('Ctrl Pts',(-22.7057130570259,14.3672181299662,-4.16037389465996));
#37128=CARTESIAN_POINT('Ctrl Pts',(-22.6987793427176,14.2812456171528,-4.03979572825579));
#37129=CARTESIAN_POINT('Ctrl Pts',(-22.6960116860671,14.2469288878693,-3.99166583000592));
#37130=CARTESIAN_POINT('Ctrl Pts',(-22.6932440294166,14.2117736184024,-3.94413060177475));
#37131=CARTESIAN_POINT('Ctrl Pts',(-22.6904763727661,14.1758012177496,-3.89721939943571));
#37132=CARTESIAN_POINT('',(-23.534,5.20509380555675,-8.32288496556916));
#37133=CARTESIAN_POINT('Ctrl Pts',(-23.534,5.20509380555674,-8.3228849655691));
#37134=CARTESIAN_POINT('Ctrl Pts',(-23.4952181183639,5.41999536482199,-9.12285064450934));
#37135=CARTESIAN_POINT('Ctrl Pts',(-23.4176543550918,6.24677152044682,-10.6153578631701));
#37136=CARTESIAN_POINT('Ctrl Pts',(-23.3135388565479,8.1665770620453,-11.8658594947153));
#37137=CARTESIAN_POINT('Ctrl Pts',(-23.2482052396401,9.56246707210738,-12.0983697268913));
#37138=CARTESIAN_POINT('Ctrl Pts',(-23.2216535043684,10.1296134499674,-12.0988145792455));
#37139=CARTESIAN_POINT('',(-23.534,5.20511879703991,-5.67702200776683));
#37140=CARTESIAN_POINT('Origin',(-23.534,10.1295,-7.));
#37141=CARTESIAN_POINT('',(-23.0963464956316,10.1295667753203,-12.099051464939));
#37142=CARTESIAN_POINT('Ctrl Pts',(-23.534,5.20511879703991,-5.67702200776683));
#37143=CARTESIAN_POINT('Ctrl Pts',(-23.5270930683901,5.16684928138222,-5.81946858258322));
#37144=CARTESIAN_POINT('Ctrl Pts',(-23.5201861367802,5.13475838719278,-5.96360047114363));
#37145=CARTESIAN_POINT('Ctrl Pts',(-23.5132792051702,5.10897409853572,-6.10886551367019));
#37146=CARTESIAN_POINT('Ctrl Pts',(-23.5063724191029,5.08319035320424,-6.25412749517716));
#37147=CARTESIAN_POINT('Ctrl Pts',(-23.4994656330356,5.06371301191541,-6.40052225348957));
#37148=CARTESIAN_POINT('Ctrl Pts',(-23.4925588469683,5.05061883811789,-6.54748796316664));
#37149=CARTESIAN_POINT('Ctrl Pts',(-23.4856526672931,5.03752581394379,-6.69444076975995));
#37150=CARTESIAN_POINT('Ctrl Pts',(-23.4787464876178,5.03081486640317,-6.84196409317219));
#37151=CARTESIAN_POINT('Ctrl Pts',(-23.4718403079426,5.03051082838708,-6.98949153797166));
#37152=CARTESIAN_POINT('Ctrl Pts',(-23.4649324605092,5.03020671694952,-7.13705460884828));
#37153=CARTESIAN_POINT('Ctrl Pts',(-23.4580246130759,5.03631260848016,-7.28462146729374));
#37154=CARTESIAN_POINT('Ctrl Pts',(-23.4511167656425,5.04880119697882,-7.4316256166855));
#37155=CARTESIAN_POINT('Ctrl Pts',(-23.4457233772622,5.05855181882528,-7.54640094703876));
#37156=CARTESIAN_POINT('Ctrl Pts',(-23.4403299888818,5.07219222530019,-7.6608332110995));
#37157=CARTESIAN_POINT('Ctrl Pts',(-23.4349366005015,5.08968742686135,-7.77465490873909));
#37158=CARTESIAN_POINT('Ctrl Pts',(-23.4280029500233,5.11217896726539,-7.92098219181541));
#37159=CARTESIAN_POINT('Ctrl Pts',(-23.4210692995451,5.14105143184807,-8.06635446880544));
#37160=CARTESIAN_POINT('Ctrl Pts',(-23.4141356490668,5.17619897751155,-8.21021071744341));
#37161=CARTESIAN_POINT('Ctrl Pts',(-23.4072033126132,5.21133986221929,-8.35403970329283));
#37162=CARTESIAN_POINT('Ctrl Pts',(-23.4002709761595,5.25275337692516,-8.49635291307339));
#37163=CARTESIAN_POINT('Ctrl Pts',(-23.3933386397059,5.30028295761182,-8.63660128238601));
#37164=CARTESIAN_POINT('Ctrl Pts',(-23.3864060557303,5.34781423536222,-8.77685465932585));
#37165=CARTESIAN_POINT('Ctrl Pts',(-23.3794734717546,5.40146191313028,-8.9150427341364));
#37166=CARTESIAN_POINT('Ctrl Pts',(-23.372540887779,5.46101993551568,-9.05063280172548));
#37167=CARTESIAN_POINT('Ctrl Pts',(-23.3656086772861,5.5205747493001,-9.18621556459883));
#37168=CARTESIAN_POINT('Ctrl Pts',(-23.3586764667932,5.58603913675344,-9.31920029803885));
#37169=CARTESIAN_POINT('Ctrl Pts',(-23.3517442563004,5.65715938613674,-9.44907542423447));
#37170=CARTESIAN_POINT('Ctrl Pts',(-23.344810502446,5.72829546946732,-9.57897946534417));
#37171=CARTESIAN_POINT('Ctrl Pts',(-23.3378767485916,5.80508977194574,-9.70577222584034));
#37172=CARTESIAN_POINT('Ctrl Pts',(-23.3309429947373,5.8872429156988,-9.82896727282171));
#37173=CARTESIAN_POINT('Ctrl Pts',(-23.3268256483559,5.93602643992676,-9.90212197250362));
#37174=CARTESIAN_POINT('Ctrl Pts',(-23.3227083019746,5.98669870451527,-9.9740085792241));
#37175=CARTESIAN_POINT('Ctrl Pts',(-23.3185909555933,6.03918981564711,-10.0445301108347));
#37176=CARTESIAN_POINT('Ctrl Pts',(-23.3116576154912,6.12758138927418,-10.1632837249084));
#37177=CARTESIAN_POINT('Ctrl Pts',(-23.3047242753892,6.2211633857878,-10.2782058956995));
#37178=CARTESIAN_POINT('Ctrl Pts',(-23.2977909352871,6.31957962315759,-10.3888505015891));
#37179=CARTESIAN_POINT('Ctrl Pts',(-23.2908589155155,6.41797711891773,-10.4994740371954));
#37180=CARTESIAN_POINT('Ctrl Pts',(-23.2839268957439,6.52120679919802,-10.6058213862124));
#37181=CARTESIAN_POINT('Ctrl Pts',(-23.2769948759722,6.62887326370307,-10.7074807421109));
#37182=CARTESIAN_POINT('Ctrl Pts',(-23.2700626150757,6.73654347330243,-10.8091436341511));
#37183=CARTESIAN_POINT('Ctrl Pts',(-23.2631303541791,6.84865053786333,-10.9061179773462));
#37184=CARTESIAN_POINT('Ctrl Pts',(-23.2561980932826,6.96476298683145,-10.9980295943728));
#37185=CARTESIAN_POINT('Ctrl Pts',(-23.2492662087238,7.08086913230112,-11.0899362217128));
#37186=CARTESIAN_POINT('Ctrl Pts',(-23.242334324165,7.20097996725761,-11.1767804683628));
#37187=CARTESIAN_POINT('Ctrl Pts',(-23.2354024396061,7.32463180495147,-11.2582291399601));
#37188=CARTESIAN_POINT('Ctrl Pts',(-23.228469013263,7.44831114519037,-11.3396959273073));
#37189=CARTESIAN_POINT('Ctrl Pts',(-23.2215355869198,7.57553278566364,-11.4157645597463));
#37190=CARTESIAN_POINT('Ctrl Pts',(-23.2146021605767,7.70580446372751,-11.4861454443044));
#37191=CARTESIAN_POINT('Ctrl Pts',(-23.2104832106128,7.78319513568321,-11.5279567115709));
#37192=CARTESIAN_POINT('Ctrl Pts',(-23.206364260649,7.86166171055427,-11.5677615028387));
#37193=CARTESIAN_POINT('Ctrl Pts',(-23.2022453106851,7.94109688570871,-11.6055067918048));
#37194=CARTESIAN_POINT('Ctrl Pts',(-23.1953326013538,8.0744105412136,-11.6688535703621));
#37195=CARTESIAN_POINT('Ctrl Pts',(-23.1884198920225,8.21050236448007,-11.7264202219746));
#37196=CARTESIAN_POINT('Ctrl Pts',(-23.1815071826912,8.34885199561309,-11.7779800841436));
#37197=CARTESIAN_POINT('Ctrl Pts',(-23.1744104587696,8.49088445926188,-11.8309124569247));
#37198=CARTESIAN_POINT('Ctrl Pts',(-23.1673137348479,8.63529628394864,-11.8775136191942));
#37199=CARTESIAN_POINT('Ctrl Pts',(-23.1602170109263,8.78150369622116,-11.9175915817602));
#37200=CARTESIAN_POINT('Ctrl Pts',(-23.1533056463726,8.92389231635461,-11.9566227478196));
#37201=CARTESIAN_POINT('Ctrl Pts',(-23.1463942818189,9.06798355227891,-11.9894671549689));
#37202=CARTESIAN_POINT('Ctrl Pts',(-23.1394829172652,9.21322389390579,-12.0159983151314));
#37203=CARTESIAN_POINT('Ctrl Pts',(-23.1322935136596,9.36430714637444,-12.0435968041202));
#37204=CARTESIAN_POINT('Ctrl Pts',(-23.125104110054,9.51663350849815,-12.0643634281151));
#37205=CARTESIAN_POINT('Ctrl Pts',(-23.1179147064484,9.66956947446774,-12.0782147366652));
#37206=CARTESIAN_POINT('Ctrl Pts',(-23.1107253028428,9.82250544043734,-12.0920660452153));
#37207=CARTESIAN_POINT('Ctrl Pts',(-23.1035358992372,9.97605060390634,-12.0990020099546));
#37208=CARTESIAN_POINT('Ctrl Pts',(-23.0963464956316,10.1295667746463,-12.0989999995628));
#37209=CARTESIAN_POINT('Ctrl Pts',(-23.0963464956316,10.129566778808,-12.099317792417));
#37210=CARTESIAN_POINT('Ctrl Pts',(-23.0928642190133,10.2039288711016,-12.0993673408814));
#37211=CARTESIAN_POINT('Ctrl Pts',(-23.0506000607591,11.1064308613037,-12.0800148219986));
#37212=CARTESIAN_POINT('Ctrl Pts',(-22.9695540208687,12.8165649252773,-11.5744658007328));
#37213=CARTESIAN_POINT('Ctrl Pts',(-22.8532083759605,14.6458800384554,-9.78358876962574));
#37214=CARTESIAN_POINT('Ctrl Pts',(-22.7368627310523,15.4235830862095,-7.34457044966851));
#37215=CARTESIAN_POINT('Ctrl Pts',(-22.640850630295,15.0481127832734,-5.26560594787934));
#37216=CARTESIAN_POINT('Ctrl Pts',(-22.5836204111736,14.4153514965049,-4.21017316538278));
#37217=CARTESIAN_POINT('Ctrl Pts',(-22.5651720736884,14.1754919335065,-3.89745664672419));
#37218=CARTESIAN_POINT('Origin',(26.8463464956315,10.1295,-7.));
#37219=CARTESIAN_POINT('',(18.1904820160362,6.08319878352125,-3.8972193977784));
#37220=CARTESIAN_POINT('',(18.0651682149652,6.08305061783963,-3.89710564634619));
#37221=CARTESIAN_POINT('',(26.8463464956315,6.08319878352126,-3.89721939777839));
#37222=CARTESIAN_POINT('',(17.734,12.4414757859806,-2.45527019889635));
#37223=CARTESIAN_POINT('Ctrl Pts',(18.0651682149652,6.08305061783963,-3.89710564634619));
#37224=CARTESIAN_POINT('Ctrl Pts',(18.0323425732489,6.51012300040625,-3.34120496454716));
#37225=CARTESIAN_POINT('Ctrl Pts',(17.9607350498965,7.69350565290941,-2.32091790294544));
#37226=CARTESIAN_POINT('Ctrl Pts',(17.8503456449082,10.0408176861101,-1.69542432103654));
#37227=CARTESIAN_POINT('Ctrl Pts',(17.772781881636,11.703188220458,-2.0796916608358));
#37228=CARTESIAN_POINT('Ctrl Pts',(17.734,12.4414757859806,-2.45527019889635));
#37229=CARTESIAN_POINT('',(17.734,14.4077184404108,-4.2257166734219));
#37230=CARTESIAN_POINT('Origin',(17.734,10.1295,-7.));
#37231=CARTESIAN_POINT('Ctrl Pts',(18.1904820160362,6.08319878352125,-3.89721939777841));
#37232=CARTESIAN_POINT('Ctrl Pts',(18.1876881220985,6.11950371475326,-3.84987454609825));
#37233=CARTESIAN_POINT('Ctrl Pts',(18.1848942281607,6.15663752372707,-3.80316978774102));
#37234=CARTESIAN_POINT('Ctrl Pts',(18.182100334223,6.19457664874617,-3.75713410395105));
#37235=CARTESIAN_POINT('Ctrl Pts',(18.1751666155273,6.28873169768777,-3.6428855002175));
#37236=CARTESIAN_POINT('Ctrl Pts',(18.1682328968315,6.38788205597123,-3.53272058770171));
#37237=CARTESIAN_POINT('Ctrl Pts',(18.1612991781358,6.49164988118888,-3.42706737915953));
#37238=CARTESIAN_POINT('Ctrl Pts',(18.1543667758962,6.59539800474323,-3.32143423024506));
#37239=CARTESIAN_POINT('Ctrl Pts',(18.1474343736566,6.70376161461654,-3.22031131194671));
#37240=CARTESIAN_POINT('Ctrl Pts',(18.140501971417,6.81632539466393,-3.12409042487364));
#37241=CARTESIAN_POINT('Ctrl Pts',(18.133569325952,6.92889312404448,-3.0278661618626));
#37242=CARTESIAN_POINT('Ctrl Pts',(18.1266366804871,7.0456610693994,-2.93654449155152));
#37243=CARTESIAN_POINT('Ctrl Pts',(18.1197040350221,7.16617974834539,-2.85047784845849));
#37244=CARTESIAN_POINT('Ctrl Pts',(18.1127717656245,7.28669188965202,-2.76441587412453));
#37245=CARTESIAN_POINT('Ctrl Pts',(18.1058394962268,7.41095408788024,-2.6836085479493));
#37246=CARTESIAN_POINT('Ctrl Pts',(18.0989072268292,7.538486708999,-2.60836577959227));
#37247=CARTESIAN_POINT('Ctrl Pts',(18.0919734185825,7.66604764024758,-2.53310630858678));
#37248=CARTESIAN_POINT('Ctrl Pts',(18.0850396103359,7.796880160196,-2.46341403160095));
#37249=CARTESIAN_POINT('Ctrl Pts',(18.0781058020892,7.93047824811605,-2.39955389828973));
#37250=CARTESIAN_POINT('Ctrl Pts',(18.0739887644978,8.00980382657902,-2.36163612495553));
#37251=CARTESIAN_POINT('Ctrl Pts',(18.0698717269063,8.09010394201909,-2.3257736263611));
#37252=CARTESIAN_POINT('Ctrl Pts',(18.0657546893148,8.17126896360323,-2.29201399661252));
#37253=CARTESIAN_POINT('Ctrl Pts',(18.0588213573683,8.30795560407876,-2.2351608068521));
#37254=CARTESIAN_POINT('Ctrl Pts',(18.0518880254217,8.44714343822144,-2.18425443098161));
#37255=CARTESIAN_POINT('Ctrl Pts',(18.0449546934752,8.58829824151367,-2.13949610229159));
#37256=CARTESIAN_POINT('Ctrl Pts',(18.0380226783627,8.72942623555296,-2.09474627446251));
#37257=CARTESIAN_POINT('Ctrl Pts',(18.0310906632502,8.87252013840123,-2.0561422639854));
#37258=CARTESIAN_POINT('Ctrl Pts',(18.0241586481377,9.01702957132649,-2.02383575981188));
#37259=CARTESIAN_POINT('Ctrl Pts',(18.0172263866156,9.16154414107234,-1.99152810725164));
#37260=CARTESIAN_POINT('Ctrl Pts',(18.0102941250934,9.30747401965934,-1.96551848432784));
#37261=CARTESIAN_POINT('Ctrl Pts',(18.0033618635713,9.45425707373931,-1.94590779758275));
#37262=CARTESIAN_POINT('Ctrl Pts',(17.9964299753957,9.60103222261469,-1.92629816699833));
#37263=CARTESIAN_POINT('Ctrl Pts',(17.9894980872201,9.74866012719367,-1.9130868258486));
#37264=CARTESIAN_POINT('Ctrl Pts',(17.9825661990445,9.89657192712221,-1.9063229869901));
#37265=CARTESIAN_POINT('Ctrl Pts',(17.9756327645019,10.0445167232454,-1.89955763925304));
#37266=CARTESIAN_POINT('Ctrl Pts',(17.9686993299592,10.1927452108641,-1.89924268284508));
#37267=CARTESIAN_POINT('Ctrl Pts',(17.9617658954166,10.3406862695542,-1.90537524840624));
#37268=CARTESIAN_POINT('Ctrl Pts',(17.9576469450799,10.4285737183722,-1.90901842594365));
#37269=CARTESIAN_POINT('Ctrl Pts',(17.9535279947433,10.5163597158814,-1.9149360686311));
#37270=CARTESIAN_POINT('Ctrl Pts',(17.9494090444066,10.6039249349976,-1.92311887266872));
#37271=CARTESIAN_POINT('Ctrl Pts',(17.9424753834828,10.7513283966681,-1.93689344724857));
#37272=CARTESIAN_POINT('Ctrl Pts',(17.9355417225589,10.8981569837258,-1.9570943475134));
#37273=CARTESIAN_POINT('Ctrl Pts',(17.9286080616351,11.043844383057,-1.98364919994901));
#37274=CARTESIAN_POINT('Ctrl Pts',(17.921675718497,11.1895040935834,-2.01019900546824));
#37275=CARTESIAN_POINT('Ctrl Pts',(17.914743375359,11.3340227240848,-2.04310029455465));
#37276=CARTESIAN_POINT('Ctrl Pts',(17.9078110322209,11.4768428889456,-2.08222935268351));
#37277=CARTESIAN_POINT('Ctrl Pts',(17.9008784472619,11.6196680358023,-2.12135977575131));
#37278=CARTESIAN_POINT('Ctrl Pts',(17.893945862303,11.760794278772,-2.16671831846166));
#37279=CARTESIAN_POINT('Ctrl Pts',(17.887013277344,11.8996776268284,-2.2181308916412));
#37280=CARTESIAN_POINT('Ctrl Pts',(17.8800810690987,12.0385534280233,-2.26954067108361));
#37281=CARTESIAN_POINT('Ctrl Pts',(17.8731488608534,12.1751862684927,-2.32700370709501));
#37282=CARTESIAN_POINT('Ctrl Pts',(17.8662166526081,12.3090504196554,-2.3902970846073));
#37283=CARTESIAN_POINT('Ctrl Pts',(17.8592829059654,12.4429442779832,-2.45360450820139));
#37284=CARTESIAN_POINT('Ctrl Pts',(17.8523491593228,12.5740679203451,-2.52274471727729));
#37285=CARTESIAN_POINT('Ctrl Pts',(17.8454154126802,12.7019180096239,-2.59744771936065));
#37286=CARTESIAN_POINT('Ctrl Pts',(17.8412980749529,12.7778368487668,-2.64180721281625));
#37287=CARTESIAN_POINT('Ctrl Pts',(17.8371807372257,12.8526018488398,-2.68812732988671));
#37288=CARTESIAN_POINT('Ctrl Pts',(17.8330633994984,12.9261120521225,-2.73634405352367));
#37289=CARTESIAN_POINT('Ctrl Pts',(17.8261558289376,13.0494385678835,-2.8172362325956));
#37290=CARTESIAN_POINT('Ctrl Pts',(17.8192482583768,13.1692774271192,-2.90349891677528));
#37291=CARTESIAN_POINT('Ctrl Pts',(17.812340687816,13.2851650747901,-2.99480600522892));
#37292=CARTESIAN_POINT('Ctrl Pts',(17.805433747039,13.4010421566397,-3.08610476894398));
#37293=CARTESIAN_POINT('Ctrl Pts',(17.7985268062619,13.512968479376,-3.18244681517665));
#37294=CARTESIAN_POINT('Ctrl Pts',(17.7916198654848,13.6205122246208,-3.28346469846606));
#37295=CARTESIAN_POINT('Ctrl Pts',(17.7847138003811,13.728042335292,-3.38446977454133));
#37296=CARTESIAN_POINT('Ctrl Pts',(17.7778077352774,13.8311907337587,-3.49014927375184));
#37297=CARTESIAN_POINT('Ctrl Pts',(17.7709016701737,13.929561225329,-3.60009769496956));
#37298=CARTESIAN_POINT('Ctrl Pts',(17.7639943665765,14.0279493580916,-3.71006583369829));
#37299=CARTESIAN_POINT('Ctrl Pts',(17.7570870629792,14.1215576465777,-3.82430417516951));
#37300=CARTESIAN_POINT('Ctrl Pts',(17.7501797593819,14.2100286837041,-3.94237238018294));
#37301=CARTESIAN_POINT('Ctrl Pts',(17.7447865062546,14.2791072598717,-4.03456055563452));
#37302=CARTESIAN_POINT('Ctrl Pts',(17.7393932531273,14.3450546292517,-4.12908289781627));
#37303=CARTESIAN_POINT('Ctrl Pts',(17.734,14.4077184404108,-4.2257166734219));
#37304=CARTESIAN_POINT('Origin',(26.8463464956315,10.1295,-7.));
#37305=CARTESIAN_POINT('',(19.690497962139,6.0828868892326,-3.89698012451499));
#37306=CARTESIAN_POINT('',(19.5651698457322,6.08319878352126,-3.8972193977784));
#37307=CARTESIAN_POINT('',(26.8463464956315,6.08319878352126,-3.89721939777839));
#37308=CARTESIAN_POINT('',(18.5963464953293,10.1294414208446,-12.0989827726088));
#37309=CARTESIAN_POINT('Ctrl Pts',(19.5651698457322,6.08319878352126,-3.8972193977784));
#37310=CARTESIAN_POINT('Ctrl Pts',(19.5580044147231,6.17633171704041,-3.77576578874045));
#37311=CARTESIAN_POINT('Ctrl Pts',(19.550838983714,6.2749444499284,-3.65849855722346));
#37312=CARTESIAN_POINT('Ctrl Pts',(19.5436735527049,6.37863283527319,-3.54590149060942));
#37313=CARTESIAN_POINT('Ctrl Pts',(19.5367389813393,6.47898053341559,-3.43693213579948));
#37314=CARTESIAN_POINT('Ctrl Pts',(19.5298044099736,6.58408164185059,-3.3323369197218));
#37315=CARTESIAN_POINT('Ctrl Pts',(19.522869838608,6.69353073715527,-3.23251858335224));
#37316=CARTESIAN_POINT('Ctrl Pts',(19.5155889777771,6.80844535681325,-3.12771565074809));
#37317=CARTESIAN_POINT('Ctrl Pts',(19.5083081169463,6.92815308930806,-3.02817921830671));
#37318=CARTESIAN_POINT('Ctrl Pts',(19.5010272561154,7.05214335024002,-2.93432944642854));
#37319=CARTESIAN_POINT('Ctrl Pts',(19.4937463952846,7.17613361117198,-2.84047967455038));
#37320=CARTESIAN_POINT('Ctrl Pts',(19.4864655344537,7.3044060595409,-2.75231680996947));
#37321=CARTESIAN_POINT('Ctrl Pts',(19.4791846736229,7.43641261061583,-2.67021001512314));
#37322=CARTESIAN_POINT('Ctrl Pts',(19.4722525172567,7.56209693210968,-2.59203558577654));
#37323=CARTESIAN_POINT('Ctrl Pts',(19.4653203608905,7.69120946211311,-2.51932363092219));
#37324=CARTESIAN_POINT('Ctrl Pts',(19.4583882045243,7.82325572183359,-2.45235903688245));
#37325=CARTESIAN_POINT('Ctrl Pts',(19.4514573849167,7.95527651848407,-2.38540735592446));
#37326=CARTESIAN_POINT('Ctrl Pts',(19.4445265653092,8.09022962124302,-2.32420097417425));
#37327=CARTESIAN_POINT('Ctrl Pts',(19.4375957457017,8.22759659625989,-2.26897849900872));
#37328=CARTESIAN_POINT('Ctrl Pts',(19.4306646979627,8.36496809278,-2.21375420616758));
#37329=CARTESIAN_POINT('Ctrl Pts',(19.4237336502237,8.50475331485513,-2.1645143406319));
#37330=CARTESIAN_POINT('Ctrl Pts',(19.4168026024848,8.64641401791106,-2.12144929618116));
#37331=CARTESIAN_POINT('Ctrl Pts',(19.4098719355473,8.78806693792943,-2.07838661778433));
#37332=CARTESIAN_POINT('Ctrl Pts',(19.4029412686098,8.93159481592084,-2.04149817701049));
#37333=CARTESIAN_POINT('Ctrl Pts',(19.3960106016723,9.07644441149005,-2.01092444159161));
#37334=CARTESIAN_POINT('Ctrl Pts',(19.3890783892253,9.22132630791031,-1.98034388835823));
#37335=CARTESIAN_POINT('Ctrl Pts',(19.3821461767782,9.36753018698962,-1.95608092251631));
#37336=CARTESIAN_POINT('Ctrl Pts',(19.3752139643311,9.51449215978502,-1.93822497966631));
#37337=CARTESIAN_POINT('Ctrl Pts',(19.3710889857923,9.60194115077149,-1.92759988968118));
#37338=CARTESIAN_POINT('Ctrl Pts',(19.3669640072535,9.68965839362785,-1.91924240856535));
#37339=CARTESIAN_POINT('Ctrl Pts',(19.3628390287147,9.77752407795016,-1.91316267703624));
#37340=CARTESIAN_POINT('Ctrl Pts',(19.3559048075467,9.9252291102158,-1.90294245342334));
#37341=CARTESIAN_POINT('Ctrl Pts',(19.3489705863787,10.0734048576221,-1.89915811700655));
#37342=CARTESIAN_POINT('Ctrl Pts',(19.3420363652107,10.2214806592299,-1.9018296852373));
#37343=CARTESIAN_POINT('Ctrl Pts',(19.335103451794,10.3695285346548,-1.90450074962676));
#37344=CARTESIAN_POINT('Ctrl Pts',(19.3281705383774,10.5174761716726,-1.91362528350658));
#37345=CARTESIAN_POINT('Ctrl Pts',(19.3212376249607,10.6647534305791,-1.92917119545007));
#37346=CARTESIAN_POINT('Ctrl Pts',(19.3143044602487,10.8120360278019,-1.94471767088173));
#37347=CARTESIAN_POINT('Ctrl Pts',(19.3073712955368,10.9586478693285,-1.96668595872507));
#37348=CARTESIAN_POINT('Ctrl Pts',(19.3004381308248,11.1040238996176,-1.99499209100783));
#37349=CARTESIAN_POINT('Ctrl Pts',(19.2935053388582,11.2493921141048,-2.02329670147767));
#37350=CARTESIAN_POINT('Ctrl Pts',(19.2865725468916,11.3935243261183,-2.05793841047807));
#37351=CARTESIAN_POINT('Ctrl Pts',(19.279639754925,11.535865618028,-2.09878211579726));
#37352=CARTESIAN_POINT('Ctrl Pts',(19.2727054235545,11.678238516357,-2.13963489032792));
#37353=CARTESIAN_POINT('Ctrl Pts',(19.2657710921841,11.8188193822447,-2.18669232169525));
#37354=CARTESIAN_POINT('Ctrl Pts',(19.2588367608137,11.9570677921862,-2.23976923196325));
#37355=CARTESIAN_POINT('Ctrl Pts',(19.2547223018113,12.0390969575754,-2.27126221370942));
#37356=CARTESIAN_POINT('Ctrl Pts',(19.2506078428089,12.1203052653314,-2.30487346637448));
#37357=CARTESIAN_POINT('Ctrl Pts',(19.2464933838065,12.2005829824517,-2.34055622635073));
#37358=CARTESIAN_POINT('Ctrl Pts',(19.2395600659607,12.3358598021767,-2.40068561793972));
#37359=CARTESIAN_POINT('Ctrl Pts',(19.2326267481149,12.4685396684855,-2.4667205822027));
#37360=CARTESIAN_POINT('Ctrl Pts',(19.225693430269,12.5981090877672,-2.53841169853235));
#37361=CARTESIAN_POINT('Ctrl Pts',(19.2187614321196,12.7276538446444,-2.6100891690857));
#37362=CARTESIAN_POINT('Ctrl Pts',(19.2118294339701,12.8540890465733,-2.68742048375259));
#37363=CARTESIAN_POINT('Ctrl Pts',(19.2048974358206,12.9769260564387,-2.77011042069487));
#37364=CARTESIAN_POINT('Ctrl Pts',(19.1979651953757,13.0997673598497,-2.85280324791448));
#37365=CARTESIAN_POINT('Ctrl Pts',(19.1910329549307,13.2190099433899,-2.9408548903621));
#37366=CARTESIAN_POINT('Ctrl Pts',(19.1841007144858,13.3341939513471,-3.03392666757164));
#37367=CARTESIAN_POINT('Ctrl Pts',(19.1771688496638,13.4493717180665,-3.12699340169313));
#37368=CARTESIAN_POINT('Ctrl Pts',(19.1702369848419,13.5604910926603,-3.22507951774791));
#37369=CARTESIAN_POINT('Ctrl Pts',(19.1633051200199,13.667125119773,-3.3278058994722));
#37370=CARTESIAN_POINT('Ctrl Pts',(19.1563717121302,13.7737828841536,-3.430555148603));
#37371=CARTESIAN_POINT('Ctrl Pts',(19.1494383042404,13.8759530677986,-3.53794649789823));
#37372=CARTESIAN_POINT('Ctrl Pts',(19.1425048963507,13.9732449701325,-3.64956337105432));
#37373=CARTESIAN_POINT('Ctrl Pts',(19.1383858438666,14.0310448945516,-3.71587358472634));
#37374=CARTESIAN_POINT('Ctrl Pts',(19.1342667913824,14.0871237909435,-3.78367446321953));
#37375=CARTESIAN_POINT('Ctrl Pts',(19.1301477388983,14.1414063406675,-3.85287297464629));
#37376=CARTESIAN_POINT('Ctrl Pts',(19.1232141285398,14.2327802793352,-3.96935498536888));
#37377=CARTESIAN_POINT('Ctrl Pts',(19.1162805181812,14.3190936323279,-4.08983919704816));
#37378=CARTESIAN_POINT('Ctrl Pts',(19.1093469078227,14.400009475508,-4.213864716207));
#37379=CARTESIAN_POINT('Ctrl Pts',(19.1024146136957,14.4809099581506,-4.3378666911678));
#37380=CARTESIAN_POINT('Ctrl Pts',(19.0954823195687,14.5564147947404,-4.46540835564231));
#37381=CARTESIAN_POINT('Ctrl Pts',(19.0885500254416,14.6262304728754,-4.59599998870346));
#37382=CARTESIAN_POINT('Ctrl Pts',(19.0816174867073,14.6960486144694,-4.72659622971433));
#37383=CARTESIAN_POINT('Ctrl Pts',(19.0746849479731,14.7601770371195,-4.86024236471895));
#37384=CARTESIAN_POINT('Ctrl Pts',(19.0677524092388,14.8183680106684,-4.99642375275354));
#37385=CARTESIAN_POINT('Ctrl Pts',(19.0608202455346,14.8765558362549,-5.13259777377116));
#37386=CARTESIAN_POINT('Ctrl Pts',(19.0538880818305,14.928806726421,-5.2713064690269));
#37387=CARTESIAN_POINT('Ctrl Pts',(19.0469559181264,14.9749209568293,-5.41201487692134));
#37388=CARTESIAN_POINT('Ctrl Pts',(19.0400222130546,15.0210454407442,-5.55275457135289));
#37389=CARTESIAN_POINT('Ctrl Pts',(19.0330885079828,15.061030435488,-5.69549455262194));
#37390=CARTESIAN_POINT('Ctrl Pts',(19.0261548029109,15.0947257927471,-5.83968373835435));
#37391=CARTESIAN_POINT('Ctrl Pts',(19.0220372332707,15.1147357266325,-5.92531025512671));
#37392=CARTESIAN_POINT('Ctrl Pts',(19.0179196636304,15.1325285371395,-6.01144756489171));
#37393=CARTESIAN_POINT('Ctrl Pts',(19.0138020939901,15.1480812641024,-6.09797832864145));
#37394=CARTESIAN_POINT('Ctrl Pts',(19.0068685366312,15.1742704324482,-6.243687100122));
#37395=CARTESIAN_POINT('Ctrl Pts',(18.9999349792723,15.1941141114036,-6.39056233036988));
#37396=CARTESIAN_POINT('Ctrl Pts',(18.9930014219134,15.2075304301788,-6.53803901660621));
#37397=CARTESIAN_POINT('Ctrl Pts',(18.9860691810523,15.2209442015525,-6.68548770094879));
#37398=CARTESIAN_POINT('Ctrl Pts',(18.9791369401912,15.2279330176624,-6.83353728439083));
#37399=CARTESIAN_POINT('Ctrl Pts',(18.9722046993301,15.2284668647841,-6.98161762166019));
#37400=CARTESIAN_POINT('Ctrl Pts',(18.9652722137388,15.2290007307523,-7.12970318663658));
#37401=CARTESIAN_POINT('Ctrl Pts',(18.9583397281476,15.2230791672004,-7.27781917705496));
#37402=CARTESIAN_POINT('Ctrl Pts',(18.9514072425563,15.2107242822434,-7.42539486778765));
#37403=CARTESIAN_POINT('Ctrl Pts',(18.944475131797,15.1983700653015,-7.57296257926424));
#37404=CARTESIAN_POINT('Ctrl Pts',(18.9375430210376,15.1795832514988,-7.71998972015298));
#37405=CARTESIAN_POINT('Ctrl Pts',(18.9306109102783,15.1544378816705,-7.86591009080227));
#37406=CARTESIAN_POINT('Ctrl Pts',(18.9236772573793,15.1292869179224,-8.01186292336624));
#37407=CARTESIAN_POINT('Ctrl Pts',(18.9167436044803,15.0977746278606,-8.1567081678229));
#37408=CARTESIAN_POINT('Ctrl Pts',(18.9098099515813,15.0600264057109,-8.29988859622186));
#37409=CARTESIAN_POINT('Ctrl Pts',(18.9056921174149,15.0376080756969,-8.38492216635026));
#37410=CARTESIAN_POINT('Ctrl Pts',(18.9015742832484,15.0129912650688,-8.46936874673093));
#37411=CARTESIAN_POINT('Ctrl Pts',(18.8974564490819,14.9862106421525,-8.55311388455654));
#37412=CARTESIAN_POINT('Ctrl Pts',(18.8905228749338,14.94111765705,-8.69412323539135));
#37413=CARTESIAN_POINT('Ctrl Pts',(18.8835893007856,14.8898716746156,-8.83319174903818));
#37414=CARTESIAN_POINT('Ctrl Pts',(18.8766557266375,14.832664936967,-8.96978185992368));
#37415=CARTESIAN_POINT('Ctrl Pts',(18.8697234694038,14.7754690647647,-9.10634602784188));
#37416=CARTESIAN_POINT('Ctrl Pts',(18.8627912121701,14.7123148237805,-9.2404324274278));
#37417=CARTESIAN_POINT('Ctrl Pts',(18.8558589549363,14.6434426840965,-9.37152323300689));
#37418=CARTESIAN_POINT('Ctrl Pts',(18.8489264537584,14.5745681208209,-9.50261865163537));
#37419=CARTESIAN_POINT('Ctrl Pts',(18.8419939525805,14.4999754069997,-9.6307179711243));
#37420=CARTESIAN_POINT('Ctrl Pts',(18.8350614514025,14.419951338008,-9.75532726117709));
#37421=CARTESIAN_POINT('Ctrl Pts',(18.8281293255397,14.3399316013977,-9.87992980507238));
#37422=CARTESIAN_POINT('Ctrl Pts',(18.8211971996768,14.254481277422,-10.0010424199487));
#37423=CARTESIAN_POINT('Ctrl Pts',(18.8142650738139,14.1639309289768,-10.1181994931876));
#37424=CARTESIAN_POINT('Ctrl Pts',(18.8073314066908,14.0733604479404,-10.2353826146473));
#37425=CARTESIAN_POINT('Ctrl Pts',(18.8003977395676,13.9776878789461,-10.3486081755401));
#37426=CARTESIAN_POINT('Ctrl Pts',(18.7934640724445,13.8772849584178,-10.4574425382726));
#37427=CARTESIAN_POINT('Ctrl Pts',(18.7893463163542,13.8176578188189,-10.5220769304364));
#37428=CARTESIAN_POINT('Ctrl Pts',(18.785228560264,13.7563630890054,-10.5851632174693));
#37429=CARTESIAN_POINT('Ctrl Pts',(18.7811108041737,13.6934849922401,-10.6466165105598));
#37430=CARTESIAN_POINT('Ctrl Pts',(18.7741773221436,13.5876107868588,-10.7500916300169));
#37431=CARTESIAN_POINT('Ctrl Pts',(18.7672438401135,13.4772089013387,-10.8489706438041));
#37432=CARTESIAN_POINT('Ctrl Pts',(18.7603103580834,13.3627009182633,-10.9428686032052));
#37433=CARTESIAN_POINT('Ctrl Pts',(18.7533781928252,13.2482146819653,-11.0367487299805));
#37434=CARTESIAN_POINT('Ctrl Pts',(18.7464460275669,13.1296241594458,-11.125649480223));
#37435=CARTESIAN_POINT('Ctrl Pts',(18.7395138623087,13.0073843026664,-11.2092259312689));
#37436=CARTESIAN_POINT('Ctrl Pts',(18.7325814519985,12.8851401247102,-11.2928053367408));
#37437=CARTESIAN_POINT('Ctrl Pts',(18.7256490416884,12.7592466253657,-11.3710598770506));
#37438=CARTESIAN_POINT('Ctrl Pts',(18.7187166313782,12.6301884988541,-11.443687436319));
#37439=CARTESIAN_POINT('Ctrl Pts',(18.7117845955379,12.5011373437089,-11.5163110724455));
#37440=CARTESIAN_POINT('Ctrl Pts',(18.7048525596975,12.3689221920308,-11.5833081744225));
#37441=CARTESIAN_POINT('Ctrl Pts',(18.6979205238572,12.2340531491347,-11.6444221430084));
#37442=CARTESIAN_POINT('Ctrl Pts',(18.6909869446661,12.0991540789498,-11.7055497180288));
#37443=CARTESIAN_POINT('Ctrl Pts',(18.684053365475,11.9616002381559,-11.7607914059617));
#37444=CARTESIAN_POINT('Ctrl Pts',(18.6771197862838,11.8219231385118,-11.8099381409983));
#37445=CARTESIAN_POINT('Ctrl Pts',(18.6730015772777,11.7389617308688,-11.8391289126429));
#37446=CARTESIAN_POINT('Ctrl Pts',(18.6688833682717,11.6552516632413,-11.8661704363263));
#37447=CARTESIAN_POINT('Ctrl Pts',(18.6647651592656,11.5709071450112,-11.891027135716));
#37448=CARTESIAN_POINT('Ctrl Pts',(18.6577998246933,11.4282510078553,-11.9330685249111));
#37449=CARTESIAN_POINT('Ctrl Pts',(18.650834490121,11.2837317271447,-11.9688711473952));
#37450=CARTESIAN_POINT('Ctrl Pts',(18.6438691555487,11.1379071299167,-11.9982913140726));
#37451=CARTESIAN_POINT('Ctrl Pts',(18.6369053523104,10.9921145923347,-12.0277050127044));
#37452=CARTESIAN_POINT('Ctrl Pts',(18.6299415490721,10.8450176285976,-12.0507389918283));
#37453=CARTESIAN_POINT('Ctrl Pts',(18.6229777458338,10.6971847677683,-12.0673005638549));
#37454=CARTESIAN_POINT('Ctrl Pts',(18.6160146892149,10.5493677567394,-12.0838603602436));
#37455=CARTESIAN_POINT('Ctrl Pts',(18.609051632596,10.4008153280418,-12.0939490974492));
#37456=CARTESIAN_POINT('Ctrl Pts',(18.6020885759772,10.2521021089812,-12.0975258432767));
#37457=CARTESIAN_POINT('Ctrl Pts',(18.6001745491953,10.2112233541923,-12.0985090303568));
#37458=CARTESIAN_POINT('Ctrl Pts',(18.5982605224134,10.1703324708191,-12.0990004693845));
#37459=CARTESIAN_POINT('Ctrl Pts',(18.5963464956315,10.1294414271024,-12.0989999996636));
#37460=CARTESIAN_POINT('Ctrl Pts',(18.5963464895963,10.1294413021288,-12.0986559623714));
#37461=CARTESIAN_POINT('Ctrl Pts',(18.5803708311834,9.78816223566316,-12.0988021887428));
#37462=CARTESIAN_POINT('Ctrl Pts',(18.5256132911343,8.61850505157706,-11.9829820583334));
#37463=CARTESIAN_POINT('Ctrl Pts',(18.4320738694491,6.76024937160752,-11.0980785162391));
#37464=CARTESIAN_POINT('Ctrl Pts',(18.3157282245409,5.23345505271711,-9.04320502425034));
#37465=CARTESIAN_POINT('Ctrl Pts',(18.1993825796327,4.8466304876897,-6.51259606632921));
#37466=CARTESIAN_POINT('Ctrl Pts',(18.1158625764408,5.45203935924674,-4.777421692593));
#37467=CARTESIAN_POINT('Ctrl Pts',(18.071124454885,6.00555797974676,-3.99797428620377));
#37468=CARTESIAN_POINT('Ctrl Pts',(18.0651682149652,6.08305061783963,-3.89710564634619));
#37469=CARTESIAN_POINT('',(18.721653505176,10.1295871904926,-12.0989689030608));
#37470=CARTESIAN_POINT('Ctrl Pts',(18.7216535043684,10.1295871737727,-12.0989999992548));
#37471=CARTESIAN_POINT('Ctrl Pts',(18.7147113410273,9.98128307520553,-12.0990025346986));
#37472=CARTESIAN_POINT('Ctrl Pts',(18.7077691776862,9.8329749558716,-12.0925306029392));
#37473=CARTESIAN_POINT('Ctrl Pts',(18.7008270143451,9.68523504562768,-12.0796092025191));
#37474=CARTESIAN_POINT('Ctrl Pts',(18.6938850789891,9.53749998725783,-12.0666882264461));
#37475=CARTESIAN_POINT('Ctrl Pts',(18.6869431436331,9.3903334278217,-12.0473182361383));
#37476=CARTESIAN_POINT('Ctrl Pts',(18.6800012082771,9.244302805183,-12.0215761396486));
#37477=CARTESIAN_POINT('Ctrl Pts',(18.6730576317816,9.0982376595178,-11.9958279574827));
#37478=CARTESIAN_POINT('Ctrl Pts',(18.6661140552862,8.95330931088689,-11.9637047165393));
#37479=CARTESIAN_POINT('Ctrl Pts',(18.6591704787908,8.81007598055744,-11.9253346340039));
#37480=CARTESIAN_POINT('Ctrl Pts',(18.6552746238124,8.72971159148627,-11.9038062073836));
#37481=CARTESIAN_POINT('Ctrl Pts',(18.6513787688341,8.64988059910993,-11.8803121723026));
#37482=CARTESIAN_POINT('Ctrl Pts',(18.6474829138558,8.57067970016459,-11.8548821069951));
#37483=CARTESIAN_POINT('Ctrl Pts',(18.6405493036326,8.4297226661706,-11.8096231941828));
#37484=CARTESIAN_POINT('Ctrl Pts',(18.6336156934094,8.29071373380833,-11.7582135060853));
#37485=CARTESIAN_POINT('Ctrl Pts',(18.6266820831862,8.15419024687287,-11.7008459216614));
#37486=CARTESIAN_POINT('Ctrl Pts',(18.6197497891957,8.01769267669309,-11.6434892275371));
#37487=CARTESIAN_POINT('Ctrl Pts',(18.6128174952052,7.88367991517738,-11.5801770216112));
#37488=CARTESIAN_POINT('Ctrl Pts',(18.6058852012147,7.75266950923779,-11.5111503874492));
#37489=CARTESIAN_POINT('Ctrl Pts',(18.5989526626174,7.62165448058108,-11.4421213176745));
#37490=CARTESIAN_POINT('Ctrl Pts',(18.5920201240202,7.49364231349697,-11.3673775673167));
#37491=CARTESIAN_POINT('Ctrl Pts',(18.5850875854229,7.36912660488231,-11.2872065170139));
#37492=CARTESIAN_POINT('Ctrl Pts',(18.5781554218558,7.24461763220445,-11.2070398037311));
#37493=CARTESIAN_POINT('Ctrl Pts',(18.5712232582886,7.12360501695346,-11.121446557744));
#37494=CARTESIAN_POINT('Ctrl Pts',(18.5642910947215,7.00655398674484,-11.030757893783));
#37495=CARTESIAN_POINT('Ctrl Pts',(18.5573573897854,6.8894769301988,-10.9400490651659));
#37496=CARTESIAN_POINT('Ctrl Pts',(18.5504236848492,6.77636348017962,-10.8442427572896));
#37497=CARTESIAN_POINT('Ctrl Pts',(18.5434899799131,6.6676468407924,-10.7437112207119));
#37498=CARTESIAN_POINT('Ctrl Pts',(18.5393724095913,6.60308562684493,-10.6840107178447));
#37499=CARTESIAN_POINT('Ctrl Pts',(18.5352548392694,6.54007433979697,-10.622644599298));
#37500=CARTESIAN_POINT('Ctrl Pts',(18.5311372689476,6.47869775743707,-10.5596971761229));
#37501=CARTESIAN_POINT('Ctrl Pts',(18.5242037115753,6.37534601797689,-10.4537003051742));
#37502=CARTESIAN_POINT('Ctrl Pts',(18.5172701542029,6.27659580949282,-10.3431810703944));
#37503=CARTESIAN_POINT('Ctrl Pts',(18.5103365968306,6.18283159101337,-10.2285615170703));
#37504=CARTESIAN_POINT('Ctrl Pts',(18.5034043559565,6.089085175867,-10.113963726953));
#37505=CARTESIAN_POINT('Ctrl Pts',(18.4964721150824,6.0003230711042,-9.99526742733144));
#37506=CARTESIAN_POINT('Ctrl Pts',(18.4895398742083,5.91688967035563,-9.87292798562261));
#37507=CARTESIAN_POINT('Ctrl Pts',(18.4826073886049,5.83345332415193,-9.75058422495596));
#37508=CARTESIAN_POINT('Ctrl Pts',(18.4756749030014,5.75534624741186,-9.62459733606426));
#37509=CARTESIAN_POINT('Ctrl Pts',(18.4687424173979,5.68286999196541,-9.49545237815638));
#37510=CARTESIAN_POINT('Ctrl Pts',(18.4618103066269,5.61039765523575,-9.36631440298387));
#37511=CARTESIAN_POINT('Ctrl Pts',(18.4548781958558,5.5435556915652,-9.23401898922316));
#37512=CARTESIAN_POINT('Ctrl Pts',(18.4479460850847,5.48260010633888,-9.09907655369981));
#37513=CARTESIAN_POINT('Ctrl Pts',(18.4410124321748,5.42163096074452,-8.96410409846483));
#37514=CARTESIAN_POINT('Ctrl Pts',(18.434078779265,5.36655094628959,-8.82648374621635));
#37515=CARTESIAN_POINT('Ctrl Pts',(18.4271451263551,5.3175685098331,-8.68674726439385));
#37516=CARTESIAN_POINT('Ctrl Pts',(18.4230272922499,5.28847828134614,-8.6037590245624));
#37517=CARTESIAN_POINT('Ctrl Pts',(18.4189094581446,5.26153778917509,-8.52002479046549));
#37518=CARTESIAN_POINT('Ctrl Pts',(18.4147916240394,5.23678246616714,-8.43565878053404));
#37519=CARTESIAN_POINT('Ctrl Pts',(18.4078580499257,5.19509966341243,-8.29360400912006));
#37520=CARTESIAN_POINT('Ctrl Pts',(18.400924475812,5.15960044824281,-8.1497081866558));
#37521=CARTESIAN_POINT('Ctrl Pts',(18.3939909016982,5.13042688503271,-8.00452426113619));
#37522=CARTESIAN_POINT('Ctrl Pts',(18.3870586444984,5.10125886284241,-7.85936791082228));
#37523=CARTESIAN_POINT('Ctrl Pts',(18.3801263872986,5.07841416062936,-7.71292426949538));
#37524=CARTESIAN_POINT('Ctrl Pts',(18.3731941300988,5.06198383767688,-7.56575696601455));
#37525=CARTESIAN_POINT('Ctrl Pts',(18.3662616289537,5.04555293654322,-7.41858448373312));
#37526=CARTESIAN_POINT('Ctrl Pts',(18.3593291278085,5.03553690634891,-7.27068861649685));
#37527=CARTESIAN_POINT('Ctrl Pts',(18.3523966266634,5.03197504813123,-7.12263916615529));
#37528=CARTESIAN_POINT('Ctrl Pts',(18.3454645008326,5.02841338274678,-6.97459773097103));
#37529=CARTESIAN_POINT('Ctrl Pts',(18.3385323750019,5.0313051971733,-6.82640305983149));
#37530=CARTESIAN_POINT('Ctrl Pts',(18.3316002491711,5.04063767405535,-6.67862603157506));
#37531=CARTESIAN_POINT('Ctrl Pts',(18.3246665820787,5.0499722258837,-6.53081614715388));
#37532=CARTESIAN_POINT('Ctrl Pts',(18.3177329149862,5.06575028063441,-6.38342442119573));
#37533=CARTESIAN_POINT('Ctrl Pts',(18.3107992478938,5.08790700112659,-6.23701832675314));
#37534=CARTESIAN_POINT('Ctrl Pts',(18.3066814916396,5.10106540246934,-6.15007088566497));
#37535=CARTESIAN_POINT('Ctrl Pts',(18.3025637353854,5.11647251715666,-6.06347097260691));
#37536=CARTESIAN_POINT('Ctrl Pts',(18.2984459791312,5.13410616806531,-5.97733609437465));
#37537=CARTESIAN_POINT('Ctrl Pts',(18.2915125307032,5.16379758291008,-5.83230280458991));
#37538=CARTESIAN_POINT('Ctrl Pts',(18.2845790822751,5.19981459172732,-5.68853842305289));
#37539=CARTESIAN_POINT('Ctrl Pts',(18.2776456338471,5.2420237897517,-5.54659802729703));
#37540=CARTESIAN_POINT('Ctrl Pts',(18.2703819990295,5.28624308460534,-5.39789811103834));
#37541=CARTESIAN_POINT('Ctrl Pts',(18.263118364212,5.33725872777692,-5.25120054397503));
#37542=CARTESIAN_POINT('Ctrl Pts',(18.2558547293944,5.3948582910805,-5.10712681667265));
#37543=CARTESIAN_POINT('Ctrl Pts',(18.2489226338069,5.44982879670795,-4.9696291485792));
#37544=CARTESIAN_POINT('Ctrl Pts',(18.2419905382195,5.51079538574318,-4.83452143894434));
#37545=CARTESIAN_POINT('Ctrl Pts',(18.2350584426321,5.57752371529563,-4.70232445643669));
#37546=CARTESIAN_POINT('Ctrl Pts',(18.2281266643766,5.64424899021099,-4.57013352553874));
#37547=CARTESIAN_POINT('Ctrl Pts',(18.2211948861212,5.71673532792395,-4.44085334971581));
#37548=CARTESIAN_POINT('Ctrl Pts',(18.2142631078658,5.79470193918982,-4.31498104811227));
#37549=CARTESIAN_POINT('Ctrl Pts',(18.2073302816422,5.87268033769472,-4.18908971673583));
#37550=CARTESIAN_POINT('Ctrl Pts',(18.2003974554187,5.95614048962211,-4.06660756907976));
#37551=CARTESIAN_POINT('Ctrl Pts',(18.1934646291951,6.04475744071231,-3.94800405892409));
#37552=CARTESIAN_POINT('Ctrl Pts',(18.1924704248088,6.0574655857937,-3.93099568077885));
#37553=CARTESIAN_POINT('Ctrl Pts',(18.1914762204225,6.07027970975569,-3.91406701628419));
#37554=CARTESIAN_POINT('Ctrl Pts',(18.1904820160362,6.08319878352125,-3.89721939777841));
#37555=CARTESIAN_POINT('Ctrl Pts',(19.690497962139,6.08288688923237,-3.89698012451529));
#37556=CARTESIAN_POINT('Ctrl Pts',(19.6530813324665,6.56941784810607,-3.2628032921712));
#37557=CARTESIAN_POINT('Ctrl Pts',(19.5768828211578,7.86759191038278,-2.20936840056837));
#37558=CARTESIAN_POINT('Ctrl Pts',(19.4619024282131,10.3463489318624,-1.69885207129888));
#37559=CARTESIAN_POINT('Ctrl Pts',(19.3455567833049,12.803119455071,-2.41785981379941));
#37560=CARTESIAN_POINT('Ctrl Pts',(19.2292111383967,14.6377971005625,-4.2031950129451));
#37561=CARTESIAN_POINT('Ctrl Pts',(19.1128654934886,15.4225339830853,-6.640033572117));
#37562=CARTESIAN_POINT('Ctrl Pts',(18.9965198485803,14.9749217362807,-9.16055209676269));
#37563=CARTESIAN_POINT('Ctrl Pts',(18.8801742036722,13.399034665446,-11.1780643853626));
#37564=CARTESIAN_POINT('Ctrl Pts',(18.7885520913344,11.5585268032384,-12.0007214198279));
#37565=CARTESIAN_POINT('Ctrl Pts',(18.7357118606328,10.4298968038467,-12.0989142199688));
#37566=CARTESIAN_POINT('Ctrl Pts',(18.7216535115672,10.1295873228123,-12.0987228108905));
#37567=CARTESIAN_POINT('Origin',(26.8463464956315,10.1295,-7.));
#37568=CARTESIAN_POINT('',(21.1904791240421,6.08319878352126,-3.89721939777839));
#37569=CARTESIAN_POINT('',(21.065286535997,6.08319878352127,-3.89721939777838));
#37570=CARTESIAN_POINT('',(26.8463464956315,6.08319878352126,-3.89721939777839));
#37571=CARTESIAN_POINT('',(20.0963464956032,10.1292828156512,-12.0989999953747));
#37572=CARTESIAN_POINT('Ctrl Pts',(21.065286535997,6.08319878352127,-3.89721939777838));
#37573=CARTESIAN_POINT('Ctrl Pts',(21.0585701332919,6.17049443209072,-3.78337812625988));
#37574=CARTESIAN_POINT('Ctrl Pts',(21.0518537305868,6.26254638853162,-3.67329063711811));
#37575=CARTESIAN_POINT('Ctrl Pts',(21.0451373278817,6.35899135444725,-3.5673529814716));
#37576=CARTESIAN_POINT('Ctrl Pts',(21.0384166480659,6.45549773803189,-3.46134786306215));
#37577=CARTESIAN_POINT('Ctrl Pts',(21.0316959682501,6.55640244925519,-3.35949811006252));
#37578=CARTESIAN_POINT('Ctrl Pts',(21.0249752884342,6.6613062164028,-3.26216200465862));
#37579=CARTESIAN_POINT('Ctrl Pts',(21.0182445035305,6.76636771488332,-3.16467954651578));
#37580=CARTESIAN_POINT('Ctrl Pts',(21.0115137186268,6.87544000309704,-3.07172453711754));
#37581=CARTESIAN_POINT('Ctrl Pts',(21.0047829337231,6.98809098247977,-2.98361476142508));
#37582=CARTESIAN_POINT('Ctrl Pts',(21.0004146416252,7.0612016805781,-2.92643135081061));
#37583=CARTESIAN_POINT('Ctrl Pts',(20.9960463495273,7.13581911444332,-2.87128790198545));
#37584=CARTESIAN_POINT('Ctrl Pts',(20.9916780574294,7.21181912996737,-2.81826120607161));
#37585=CARTESIAN_POINT('Ctrl Pts',(20.9851848545906,7.32478857099484,-2.73944021958085));
#37586=CARTESIAN_POINT('Ctrl Pts',(20.9786916517519,7.4411732082542,-2.66504792986056));
#37587=CARTESIAN_POINT('Ctrl Pts',(20.9721984489131,7.5605842685465,-2.59540320066743));
#37588=CARTESIAN_POINT('Ctrl Pts',(20.9657137060064,7.679839749308,-2.52584921092728));
#37589=CARTESIAN_POINT('Ctrl Pts',(20.9592289630997,7.80211347051069,-2.46103068201192));
#37590=CARTESIAN_POINT('Ctrl Pts',(20.9527442201929,7.92698482267712,-2.40122539216561));
#37591=CARTESIAN_POINT('Ctrl Pts',(20.9462662847788,8.05172508856592,-2.3414828841559));
#37592=CARTESIAN_POINT('Ctrl Pts',(20.9397883493647,8.17905720344193,-2.28674332075737));
#37593=CARTESIAN_POINT('Ctrl Pts',(20.9333104139506,8.30853331594396,-2.23724015558648));
#37594=CARTESIAN_POINT('Ctrl Pts',(20.9268376417297,8.43790623041245,-2.18777644656854));
#37595=CARTESIAN_POINT('Ctrl Pts',(20.9203648695089,8.56941937043644,-2.14354097624662));
#37596=CARTESIAN_POINT('Ctrl Pts',(20.9138920972881,8.70260256867513,-2.10472015912487));
#37597=CARTESIAN_POINT('Ctrl Pts',(20.9074222385478,8.83572581939206,-2.06591681576715));
#37598=CARTESIAN_POINT('Ctrl Pts',(20.9009523798075,8.97051725008503,-2.03252339372634));
#37599=CARTESIAN_POINT('Ctrl Pts',(20.8944825210672,9.10648943524987,-2.00467714913144));
#37600=CARTESIAN_POINT('Ctrl Pts',(20.8880140950405,9.24243151014331,-1.97683707092991));
#37601=CARTESIAN_POINT('Ctrl Pts',(20.8815456690139,9.37955342700083,-1.95454180910603));
#37602=CARTESIAN_POINT('Ctrl Pts',(20.8750772429872,9.51735593402374,-1.9378778518797));
#37603=CARTESIAN_POINT('Ctrl Pts',(20.8686087712673,9.65515941448958,-1.92121377693845));
#37604=CARTESIAN_POINT('Ctrl Pts',(20.8621402995473,9.79364309633691,-1.91018113416165));
#37605=CARTESIAN_POINT('Ctrl Pts',(20.8556718278274,9.93230148099877,-1.90481465066248));
#37606=CARTESIAN_POINT('Ctrl Pts',(20.8492018320788,10.0709925347921,-1.89944690277274));
#37607=CARTESIAN_POINT('Ctrl Pts',(20.8427318363303,10.2098579723932,-1.89974798431355));
#37608=CARTESIAN_POINT('Ctrl Pts',(20.8362618405817,10.3483917041282,-1.90570049743207));
#37609=CARTESIAN_POINT('Ctrl Pts',(20.8297845845165,10.487080891723,-1.91165969017319));
#37610=CARTESIAN_POINT('Ctrl Pts',(20.8233073284513,10.6254372286393,-1.92328296238101));
#37611=CARTESIAN_POINT('Ctrl Pts',(20.8168300723862,10.7629587075552,-1.94050090761719));
#37612=CARTESIAN_POINT('Ctrl Pts',(20.8103491685815,10.9005576332364,-1.95772854933259));
#37613=CARTESIAN_POINT('Ctrl Pts',(20.8038682647768,11.0373203698773,-1.98055707009135));
#37614=CARTESIAN_POINT('Ctrl Pts',(20.7973873609722,11.1727557922057,-2.00886602543778));
#37615=CARTESIAN_POINT('Ctrl Pts',(20.7908954455443,11.3084213311775,-2.03722308017853));
#37616=CARTESIAN_POINT('Ctrl Pts',(20.7844035301165,11.4427546621825,-2.07107907258745));
#37617=CARTESIAN_POINT('Ctrl Pts',(20.7779116146887,11.5752797123965,-2.11026360391251));
#37618=CARTESIAN_POINT('Ctrl Pts',(20.7716033323302,11.7040561029136,-2.14833974498919));
#37619=CARTESIAN_POINT('Ctrl Pts',(20.7652950499716,11.8311248479606,-2.19144685620594));
#37620=CARTESIAN_POINT('Ctrl Pts',(20.758986767613,11.956069933585,-2.23938624989138));
#37621=CARTESIAN_POINT('Ctrl Pts',(20.752255350081,12.089395852133,-2.29054123262481));
#37622=CARTESIAN_POINT('Ctrl Pts',(20.7455239325489,12.2207429681633,-2.34736702175228));
#37623=CARTESIAN_POINT('Ctrl Pts',(20.7387925150168,12.3496051713782,-2.40969129273208));
#37624=CARTESIAN_POINT('Ctrl Pts',(20.7320693455013,12.4783094795322,-2.47193919768429));
#37625=CARTESIAN_POINT('Ctrl Pts',(20.7253461759858,12.604534607748,-2.53967200821282));
#37626=CARTESIAN_POINT('Ctrl Pts',(20.7186230064702,12.7277927942082,-2.61266874335141));
#37627=CARTESIAN_POINT('Ctrl Pts',(20.7119067023597,12.8509251148298,-2.68559093743474));
#37628=CARTESIAN_POINT('Ctrl Pts',(20.7051903982492,12.9710962113983,-2.7637661629336));
#37629=CARTESIAN_POINT('Ctrl Pts',(20.6984740941386,13.0878414666366,-2.84692682862695));
#37630=CARTESIAN_POINT('Ctrl Pts',(20.691763278558,13.2044913182398,-2.93001953584278));
#37631=CARTESIAN_POINT('Ctrl Pts',(20.6850524629774,13.3177206051619,-3.01808935397584));
#37632=CARTESIAN_POINT('Ctrl Pts',(20.6783416473968,13.427092417135,-3.11082460533681));
#37633=CARTESIAN_POINT('Ctrl Pts',(20.6716350714244,13.5363951326426,-3.20350127050457));
#37634=CARTESIAN_POINT('Ctrl Pts',(20.6649284954521,13.6418449478012,-3.30083725726319));
#37635=CARTESIAN_POINT('Ctrl Pts',(20.6582219194797,13.7430369628603,-3.40247979602026));
#37636=CARTESIAN_POINT('Ctrl Pts',(20.6515176619563,13.8441939960568,-3.50408719716967));
#37637=CARTESIAN_POINT('Ctrl Pts',(20.6448134044329,13.9410958999718,-3.60999792371146));
#37638=CARTESIAN_POINT('Ctrl Pts',(20.6381091469095,14.0333736471028,-3.71982141531038));
#37639=CARTESIAN_POINT('Ctrl Pts',(20.6314059678938,14.1256365495977,-3.82962723970549));
#37640=CARTESIAN_POINT('Ctrl Pts',(20.6247027888781,14.2132765396375,-3.94334429217381));
#37641=CARTESIAN_POINT('Ctrl Pts',(20.6179996098624,14.2959640876569,-4.060548009192));
#37642=CARTESIAN_POINT('Ctrl Pts',(20.6112962704155,14.378653614687,-4.17775453131697));
#37643=CARTESIAN_POINT('Ctrl Pts',(20.6045929309686,14.456390251492,-4.29844758149486));
#37644=CARTESIAN_POINT('Ctrl Pts',(20.5978895915217,14.5288871829675,-4.42217273380445));
#37645=CARTESIAN_POINT('Ctrl Pts',(20.5911823410669,14.6014264121778,-4.54597007253031));
#37646=CARTESIAN_POINT('Ctrl Pts',(20.5844750906121,14.668719640705,-4.67280272880459));
#37647=CARTESIAN_POINT('Ctrl Pts',(20.5777678401573,14.7305252782473,-4.80219032013015));
#37648=CARTESIAN_POINT('Ctrl Pts',(20.5710585028671,14.7923501454557,-4.93161816798048));
#37649=CARTESIAN_POINT('Ctrl Pts',(20.564349165577,14.8486838674656,-5.06360219779874));
#37650=CARTESIAN_POINT('Ctrl Pts',(20.5576398282869,14.8993327590442,-5.19764142004176));
#37651=CARTESIAN_POINT('Ctrl Pts',(20.5509240694714,14.9500301268172,-5.33180893159575));
#37652=CARTESIAN_POINT('Ctrl Pts',(20.544208310656,14.9950316728671,-5.4680352158438));
#37653=CARTESIAN_POINT('Ctrl Pts',(20.5374925518406,15.0341932052633,-5.60580289691735));
#37654=CARTESIAN_POINT('Ctrl Pts',(20.5337601938259,15.055957664548,-5.68236882531709));
#37655=CARTESIAN_POINT('Ctrl Pts',(20.5300278358113,15.0759192163065,-5.75941061027489));
#37656=CARTESIAN_POINT('Ctrl Pts',(20.5262954777967,15.0940599329618,-5.83683807144917));
#37657=CARTESIAN_POINT('Ctrl Pts',(20.5195531565522,15.1268302456745,-5.97670697318204));
#37658=CARTESIAN_POINT('Ctrl Pts',(20.5128108353077,15.1537122172889,-6.11807599491532));
#37659=CARTESIAN_POINT('Ctrl Pts',(20.5060685140632,15.174579088646,-6.26042039691011));
#37660=CARTESIAN_POINT('Ctrl Pts',(20.4993310938359,15.1954307918007,-6.40266132825656));
#37661=CARTESIAN_POINT('Ctrl Pts',(20.4925936736085,15.210276051231,-6.54587586687352));
#37662=CARTESIAN_POINT('Ctrl Pts',(20.4858562533812,15.2190391491384,-6.68952898784726));
#37663=CARTESIAN_POINT('Ctrl Pts',(20.4791225787158,15.2277973753404,-6.83310224714431));
#37664=CARTESIAN_POINT('Ctrl Pts',(20.4723889040505,15.2304801549966,-6.97711323862747));
#37665=CARTESIAN_POINT('Ctrl Pts',(20.4656552293852,15.2270636067672,-7.12102179540484));
#37666=CARTESIAN_POINT('Ctrl Pts',(20.4589238948687,15.2236482458881,-7.26488033975003));
#37667=CARTESIAN_POINT('Ctrl Pts',(20.4521925603523,15.2141377896593,-7.40863615508435));
#37668=CARTESIAN_POINT('Ctrl Pts',(20.4454612258358,15.1985604617483,-7.55174906899793));
#37669=CARTESIAN_POINT('Ctrl Pts',(20.4387300007792,15.182983387144,-7.69485965571773));
#37670=CARTESIAN_POINT('Ctrl Pts',(20.4319987757227,15.161339670661,-7.83732699762328));
#37671=CARTESIAN_POINT('Ctrl Pts',(20.4252675506661,15.1337094284332,-7.97861585741328));
#37672=CARTESIAN_POINT('Ctrl Pts',(20.4201616447402,15.1127507743489,-8.08578916099401));
#37673=CARTESIAN_POINT('Ctrl Pts',(20.4150557388143,15.0883486417902,-8.19228444747344));
#37674=CARTESIAN_POINT('Ctrl Pts',(20.4099498328885,15.0605576408463,-8.2978719284471));
#37675=CARTESIAN_POINT('Ctrl Pts',(20.4026904401681,15.0210453989695,-8.44799239714914));
#37676=CARTESIAN_POINT('Ctrl Pts',(20.3954310474478,14.9746959459559,-8.59622252503325));
#37677=CARTESIAN_POINT('Ctrl Pts',(20.3881716547275,14.9217167822243,-8.74196995156864));
#37678=CARTESIAN_POINT('Ctrl Pts',(20.3809048355569,14.8686834201407,-8.88786647955733));
#37679=CARTESIAN_POINT('Ctrl Pts',(20.3736380163864,14.8090068857943,-9.03127499398435));
#37680=CARTESIAN_POINT('Ctrl Pts',(20.3663711972158,14.7429431237293,-9.17162232999089));
#37681=CARTESIAN_POINT('Ctrl Pts',(20.3590963867037,14.6768067111584,-9.31212400635949));
#37682=CARTESIAN_POINT('Ctrl Pts',(20.3518215761916,14.6042691365757,-9.44955754437085));
#37683=CARTESIAN_POINT('Ctrl Pts',(20.3445467656795,14.5256333395251,-9.58337234271712));
#37684=CARTESIAN_POINT('Ctrl Pts',(20.337269635131,14.4469724644459,-9.71722981642851));
#37685=CARTESIAN_POINT('Ctrl Pts',(20.3299925045826,14.3622096156487,-9.84746602947761));
#37686=CARTESIAN_POINT('Ctrl Pts',(20.3227153740341,14.2716922118622,-9.97355757973308));
#37687=CARTESIAN_POINT('Ctrl Pts',(20.3154369289258,14.1811584567754,-10.0996719074956));
#37688=CARTESIAN_POINT('Ctrl Pts',(20.3081584838175,14.0848682185007,-10.2216398712836));
#37689=CARTESIAN_POINT('Ctrl Pts',(20.3008800387091,13.983211124939,-10.3389686379961));
#37690=CARTESIAN_POINT('Ctrl Pts',(20.2984547551328,13.9493375055381,-10.3780642864073));
#37691=CARTESIAN_POINT('Ctrl Pts',(20.2960294715565,13.9148683294575,-10.4166451029411));
#37692=CARTESIAN_POINT('Ctrl Pts',(20.2936041879802,13.8798190021703,-10.4546936741136));
#37693=CARTESIAN_POINT('Ctrl Pts',(20.2868777084082,13.7826103349796,-10.5602206892792));
#37694=CARTESIAN_POINT('Ctrl Pts',(20.2801512288361,13.6808807511221,-10.6617110339456));
#37695=CARTESIAN_POINT('Ctrl Pts',(20.2734247492641,13.5749966495666,-10.7587702560579));
#37696=CARTESIAN_POINT('Ctrl Pts',(20.2667018516651,13.469168933226,-10.8557777923645));
#37697=CARTESIAN_POINT('Ctrl Pts',(20.2599789540661,13.3591913769016,-10.9483586585881));
#37698=CARTESIAN_POINT('Ctrl Pts',(20.2532560564671,13.2454670553348,-11.0361553872551));
#37699=CARTESIAN_POINT('Ctrl Pts',(20.2465348108106,13.1317706779763,-11.1239305426118));
#37700=CARTESIAN_POINT('Ctrl Pts',(20.2398135651542,13.0143296577915,-11.2069236743742));
#37701=CARTESIAN_POINT('Ctrl Pts',(20.2330923194978,12.8935800092736,-11.2848176976779));
#37702=CARTESIAN_POINT('Ctrl Pts',(20.2263722417576,12.7728513428002,-11.3626981857384));
#37703=CARTESIAN_POINT('Ctrl Pts',(20.2196521640174,12.6488155039475,-11.4354811335248));
#37704=CARTESIAN_POINT('Ctrl Pts',(20.2129320862773,12.5219371004029,-11.5028930389935));
#37705=CARTESIAN_POINT('Ctrl Pts',(20.2062101801347,12.3950241757137,-11.5703232859298));
#37706=CARTESIAN_POINT('Ctrl Pts',(20.1994882739921,12.2652674652435,-11.6323793963712));
#37707=CARTESIAN_POINT('Ctrl Pts',(20.1927663678496,12.1331560519276,-11.6888339089345));
#37708=CARTESIAN_POINT('Ctrl Pts',(20.1875970929237,12.0315598377311,-11.7322485133716));
#37709=CARTESIAN_POINT('Ctrl Pts',(20.1824278179979,11.9285716059888,-11.7723513056034));
#37710=CARTESIAN_POINT('Ctrl Pts',(20.1772585430721,11.8244215995656,-11.8090583040057));
#37711=CARTESIAN_POINT('Ctrl Pts',(20.1702029153173,11.6822655551441,-11.8591602855097));
#37712=CARTESIAN_POINT('Ctrl Pts',(20.1631472875625,11.5378982969924,-11.9029508158294));
#37713=CARTESIAN_POINT('Ctrl Pts',(20.1560916598077,11.3918866567047,-11.9402612207224));
#37714=CARTESIAN_POINT('Ctrl Pts',(20.1490358127607,11.245870478308,-11.9775727852401));
#37715=CARTESIAN_POINT('Ctrl Pts',(20.1419799657137,11.0982101122984,-12.0084037507865));
#37716=CARTESIAN_POINT('Ctrl Pts',(20.1349241186668,10.9494848386558,-12.0326360750977));
#37717=CARTESIAN_POINT('Ctrl Pts',(20.1278666858757,10.8007261402202,-12.0568738454262));
#37718=CARTESIAN_POINT('Ctrl Pts',(20.1208092530846,10.6509023569821,-12.0745099618943));
#37719=CARTESIAN_POINT('Ctrl Pts',(20.1137518202935,10.5006010709216,-12.0854778531777));
#37720=CARTESIAN_POINT('Ctrl Pts',(20.1079500454062,10.3770413782099,-12.0944943380808));
#37721=CARTESIAN_POINT('Ctrl Pts',(20.1021482705188,10.2531592030081,-12.0990052716912));
#37722=CARTESIAN_POINT('Ctrl Pts',(20.0963464956315,10.1292828162553,-12.0989999953747));
#37723=CARTESIAN_POINT('Ctrl Pts',(20.0963464956032,10.1292828156512,-12.0989999953747));
#37724=CARTESIAN_POINT('Ctrl Pts',(20.0890161304489,9.9727687890773,-12.0989933288916));
#37725=CARTESIAN_POINT('Ctrl Pts',(20.0816857652947,9.81628384987453,-12.0917760164965));
#37726=CARTESIAN_POINT('Ctrl Pts',(20.0743554001404,9.66046609801297,-12.0773820221436));
#37727=CARTESIAN_POINT('Ctrl Pts',(20.0698745661482,9.56521934502955,-12.0685834019081));
#37728=CARTESIAN_POINT('Ctrl Pts',(20.065393732156,9.4702218440322,-12.0571042223294));
#37729=CARTESIAN_POINT('Ctrl Pts',(20.0609128981638,9.37561849205956,-12.0429617956103));
#37730=CARTESIAN_POINT('Ctrl Pts',(20.0540297945509,9.23029628755551,-12.0212373156105));
#37731=CARTESIAN_POINT('Ctrl Pts',(20.0471466909379,9.0858734579511,-11.9932209241342));
#37732=CARTESIAN_POINT('Ctrl Pts',(20.040263587325,8.94290407468458,-11.9590111020268));
#37733=CARTESIAN_POINT('Ctrl Pts',(20.0333824104595,8.79997471201355,-11.9248108560777));
#37734=CARTESIAN_POINT('Ctrl Pts',(20.0265012335941,8.65849831506874,-11.8844207161138));
#37735=CARTESIAN_POINT('Ctrl Pts',(20.0196200567286,8.51901756866879,-11.8379900101564));
#37736=CARTESIAN_POINT('Ctrl Pts',(20.0127390888202,8.37954105780559,-11.7915607141354));
#37737=CARTESIAN_POINT('Ctrl Pts',(20.0058581209118,8.24206040107134,-11.7390913207874));
#37738=CARTESIAN_POINT('Ctrl Pts',(19.9989771530033,8.10710237471126,-11.6807807944003));
#37739=CARTESIAN_POINT('Ctrl Pts',(19.9920967087737,7.97215461938547,-11.6224747057589));
#37740=CARTESIAN_POINT('Ctrl Pts',(19.985216264544,7.83972942282541,-11.5583285083938));
#37741=CARTESIAN_POINT('Ctrl Pts',(19.9783358203144,7.71033280260142,-11.4885889844171));
#37742=CARTESIAN_POINT('Ctrl Pts',(19.9714536339439,7.58090341892158,-11.4188318022682));
#37743=CARTESIAN_POINT('Ctrl Pts',(19.9645714475735,7.45450444365356,-11.3434786251353));
#37744=CARTESIAN_POINT('Ctrl Pts',(19.957689261203,7.33161704422618,-11.2628220659312));
#37745=CARTESIAN_POINT('Ctrl Pts',(19.9533152585539,7.25351543788963,-11.2115604486721));
#37746=CARTESIAN_POINT('Ctrl Pts',(19.9489412559048,7.17683173753798,-11.1581575511211));
#37747=CARTESIAN_POINT('Ctrl Pts',(19.9445672532557,7.10168335770222,-11.1026975736245));
#37748=CARTESIAN_POINT('Ctrl Pts',(19.9376178748488,6.9822882475402,-11.0145832305441));
#37749=CARTESIAN_POINT('Ctrl Pts',(19.930668496442,6.8667251055417,-10.921240950437));
#37750=CARTESIAN_POINT('Ctrl Pts',(19.9237191180351,6.75544289250122,-10.8230275483361));
#37751=CARTESIAN_POINT('Ctrl Pts',(19.9167708710451,6.64417879713505,-10.7248301361979));
#37752=CARTESIAN_POINT('Ctrl Pts',(19.9098226240551,6.53719448530056,-10.6217634011466));
#37753=CARTESIAN_POINT('Ctrl Pts',(19.9028743770652,6.43490468373816,-10.5142234489366));
#37754=CARTESIAN_POINT('Ctrl Pts',(19.8959257674772,6.33260954412695,-10.4066778846959));
#37755=CARTESIAN_POINT('Ctrl Pts',(19.8889771578891,6.23500963255852,-10.2946588716185));
#37756=CARTESIAN_POINT('Ctrl Pts',(19.8820285483011,6.14248214411779,-10.1785986876101));
#37757=CARTESIAN_POINT('Ctrl Pts',(19.8750802871826,6.04995929588631,-10.0625443239643));
#37758=CARTESIAN_POINT('Ctrl Pts',(19.868132026064,5.96250856499122,-9.94244945163858));
#37759=CARTESIAN_POINT('Ctrl Pts',(19.8611837649454,5.88046626630638,-9.8187786947424));
#37760=CARTESIAN_POINT('Ctrl Pts',(19.8542340645085,5.79840697272408,-9.6950823196972));
#37761=CARTESIAN_POINT('Ctrl Pts',(19.8472843640716,5.72175853102108,-9.56780885290348));
#37762=CARTESIAN_POINT('Ctrl Pts',(19.8403346636347,5.65081375603784,-9.43745164631919));
#37763=CARTESIAN_POINT('Ctrl Pts',(19.8362969785389,5.60959576928118,-9.36171581354087));
#37764=CARTESIAN_POINT('Ctrl Pts',(19.8322592934432,5.57030220177107,-9.28493958658977));
#37765=CARTESIAN_POINT('Ctrl Pts',(19.8282216083474,5.53298336328829,-9.20722355198392));
#37766=CARTESIAN_POINT('Ctrl Pts',(19.821289621329,5.46891355651218,-9.07379894599301));
#37767=CARTESIAN_POINT('Ctrl Pts',(19.8143576343105,5.41064597993131,-8.93755962820844));
#37768=CARTESIAN_POINT('Ctrl Pts',(19.807425647292,5.35841008944348,-8.79902808910417));
#37769=CARTESIAN_POINT('Ctrl Pts',(19.800494976297,5.30618411583254,-8.66052284992904));
#37770=CARTESIAN_POINT('Ctrl Pts',(19.7935643053021,5.25998766035838,-8.51972656710486));
#37771=CARTESIAN_POINT('Ctrl Pts',(19.7866336343072,5.22000157021081,-8.37718051391147));
#37772=CARTESIAN_POINT('Ctrl Pts',(19.7797027024116,5.18001397481245,-8.23462909466308));
#37773=CARTESIAN_POINT('Ctrl Pts',(19.772771770516,5.14623730510447,-8.09032809093049));
#37774=CARTESIAN_POINT('Ctrl Pts',(19.7658408386203,5.11880232749438,-7.94483323118251));
#37775=CARTESIAN_POINT('Ctrl Pts',(19.7589102686247,5.09136878240709,-7.7993459684775));
#37776=CARTESIAN_POINT('Ctrl Pts',(19.7519796986291,5.07027632712535,-7.65266529985237));
#37777=CARTESIAN_POINT('Ctrl Pts',(19.7450491286335,5.05560446738238,-7.50535643271154));
#37778=CARTESIAN_POINT('Ctrl Pts',(19.73811698291,5.04092927185914,-7.35801407356488));
#37779=CARTESIAN_POINT('Ctrl Pts',(19.7311848371864,5.03267762147763,-7.21004355990087));
#37780=CARTESIAN_POINT('Ctrl Pts',(19.7242526914629,5.03087713469774,-7.06201513861103));
#37781=CARTESIAN_POINT('Ctrl Pts',(19.720127115455,5.02980559850131,-6.97391795662521));
#37782=CARTESIAN_POINT('Ctrl Pts',(19.7160015394472,5.03101799301621,-6.88580032960711));
#37783=CARTESIAN_POINT('Ctrl Pts',(19.7118759634393,5.03451137520289,-6.7977825101827));
#37784=CARTESIAN_POINT('Ctrl Pts',(19.7049446719573,5.04038053144858,-6.64990566562309));
#37785=CARTESIAN_POINT('Ctrl Pts',(19.6980133804754,5.05269303632925,-6.50225813648039));
#37786=CARTESIAN_POINT('Ctrl Pts',(19.6910820889935,5.07140714354957,-6.35540892379343));
#37787=CARTESIAN_POINT('Ctrl Pts',(19.684152155773,5.09011758353832,-6.20858848779685));
#37788=CARTESIAN_POINT('Ctrl Pts',(19.6772222225525,5.11522708127018,-6.06256638434076));
#37789=CARTESIAN_POINT('Ctrl Pts',(19.6702922893321,5.1466421432545,-5.91790546648196));
#37790=CARTESIAN_POINT('Ctrl Pts',(19.6633621517524,5.17805813164832,-5.77324028266789));
#37791=CARTESIAN_POINT('Ctrl Pts',(19.6564320141728,5.21577998959384,-5.62993668900659));
#37792=CARTESIAN_POINT('Ctrl Pts',(19.6495018765932,5.25966320185877,-5.48854687156048));
#37793=CARTESIAN_POINT('Ctrl Pts',(19.6425721311451,5.30354393105683,-5.34716505444877));
#37794=CARTESIAN_POINT('Ctrl Pts',(19.6356423856971,5.3535852180655,-5.20769711279107));
#37795=CARTESIAN_POINT('Ctrl Pts',(19.6287126402491,5.40959281113337,-5.07067962005138));
#37796=CARTESIAN_POINT('Ctrl Pts',(19.6217813588474,5.46561281808687,-4.93363175786727));
#37797=CARTESIAN_POINT('Ctrl Pts',(19.6148500774458,5.52760164817825,-4.79903573639779));
#37798=CARTESIAN_POINT('Ctrl Pts',(19.6079187960441,5.59531683860077,-4.66740829571833));
#37799=CARTESIAN_POINT('Ctrl Pts',(19.6037893035398,5.63565993752784,-4.58898779911019));
#37800=CARTESIAN_POINT('Ctrl Pts',(19.5996598110354,5.6780346941485,-4.51162059036813));
#37801=CARTESIAN_POINT('Ctrl Pts',(19.5955303185311,5.72238203724709,-4.43541187275996));
#37802=CARTESIAN_POINT('Ctrl Pts',(19.5885944590229,5.79686744700874,-4.30741237692011));
#37803=CARTESIAN_POINT('Ctrl Pts',(19.5816585995147,5.87694546042748,-4.18263866391877));
#37804=CARTESIAN_POINT('Ctrl Pts',(19.5747227400066,5.96231200227857,-4.06157436853568));
#37805=CARTESIAN_POINT('Ctrl Pts',(19.5715384419151,6.00150433539447,-4.00599296521056));
#37806=CARTESIAN_POINT('Ctrl Pts',(19.5683541438237,6.04181076065445,-3.95119305197544));
#37807=CARTESIAN_POINT('Ctrl Pts',(19.5651698457322,6.08319878352126,-3.8972193977784));
#37808=CARTESIAN_POINT('',(20.2216535043684,10.1337426824875,-12.0989982349129));
#37809=CARTESIAN_POINT('Ctrl Pts',(20.2216531628861,10.1337360354165,-12.0997534730252));
#37810=CARTESIAN_POINT('Ctrl Pts',(20.1623123261755,8.86943546207591,-12.0878187862941));
#37811=CARTESIAN_POINT('Ctrl Pts',(20.0641896078287,6.76854703791684,-11.2892745934799));
#37812=CARTESIAN_POINT('Ctrl Pts',(19.9272850078459,5.12804044036981,-8.75245917967931));
#37813=CARTESIAN_POINT('Ctrl Pts',(19.8109393629377,4.88151594588123,-6.21192105474875));
#37814=CARTESIAN_POINT('Ctrl Pts',(19.7320103477021,5.54900739211662,-4.60515275155534));
#37815=CARTESIAN_POINT('Ctrl Pts',(19.6918632141025,6.06513442588355,-3.92011986674037));
#37816=CARTESIAN_POINT('Ctrl Pts',(19.690497962139,6.08288688923237,-3.89698012451529));
#37817=CARTESIAN_POINT('Ctrl Pts',(21.1904791240421,6.08319878352127,-3.89721939777839));
#37818=CARTESIAN_POINT('Ctrl Pts',(21.1834167056448,6.17494656980835,-3.77757214363582));
#37819=CARTESIAN_POINT('Ctrl Pts',(21.1763542872475,6.27200884096288,-3.66199150568125));
#37820=CARTESIAN_POINT('Ctrl Pts',(21.1692918688503,6.37400656717798,-3.55093199892628));
#37821=CARTESIAN_POINT('Ctrl Pts',(21.1622298870913,6.47599798732141,-3.43987935849309));
#37822=CARTESIAN_POINT('Ctrl Pts',(21.1551679053324,6.58292404919854,-3.33334751629621));
#37823=CARTESIAN_POINT('Ctrl Pts',(21.1481059235734,6.69436714454001,-3.23175594403185));
#37824=CARTESIAN_POINT('Ctrl Pts',(21.1410452118414,6.80579019795256,-3.13018264199826));
#37825=CARTESIAN_POINT('Ctrl Pts',(21.1339845001094,6.92172843775375,-3.03354804002583));
#37826=CARTESIAN_POINT('Ctrl Pts',(21.1269237883774,7.04172903905915,-2.9422331889609));
#37827=CARTESIAN_POINT('Ctrl Pts',(21.1198640177282,7.16171364615532,-2.85093050874193));
#37828=CARTESIAN_POINT('Ctrl Pts',(21.112804247079,7.28575929258829,-2.76494634862895));
#37829=CARTESIAN_POINT('Ctrl Pts',(21.1057444764298,7.41338136355489,-2.68462046249052));
#37830=CARTESIAN_POINT('Ctrl Pts',(21.1007434699292,7.50378639769025,-2.62771914108665));
#37831=CARTESIAN_POINT('Ctrl Pts',(21.0957424634285,7.5959854190011,-2.57365630587753));
#37832=CARTESIAN_POINT('Ctrl Pts',(21.0907414569279,7.68979747601854,-2.52253949269471));
#37833=CARTESIAN_POINT('Ctrl Pts',(21.0840196099996,7.81589015100785,-2.45383344449506));
#37834=CARTESIAN_POINT('Ctrl Pts',(21.0772977630712,7.9449362626361,-2.39043095335399));
#37835=CARTESIAN_POINT('Ctrl Pts',(21.0705759161429,8.07645702253597,-2.33257934907452));
#37836=CARTESIAN_POINT('Ctrl Pts',(21.0638557183066,8.20794551603063,-2.27474193771263));
#37837=CARTESIAN_POINT('Ctrl Pts',(21.0571355204702,8.34190711156151,-2.22245284749552));
#37838=CARTESIAN_POINT('Ctrl Pts',(21.0504153226339,8.47784123377184,-2.17591207377585));
#37839=CARTESIAN_POINT('Ctrl Pts',(21.0436938073277,8.61380200536455,-2.12936217590945));
#37840=CARTESIAN_POINT('Ctrl Pts',(21.0369722920214,8.75173573007874,-2.08856297103887));
#37841=CARTESIAN_POINT('Ctrl Pts',(21.0302507767151,8.89112448377531,-2.05366528823461));
#37842=CARTESIAN_POINT('Ctrl Pts',(21.0235287760831,9.03052330201039,-2.01876508564978));
#37843=CARTESIAN_POINT('Ctrl Pts',(21.0168067754511,9.17137700030015,-1.98976733838324));
#37844=CARTESIAN_POINT('Ctrl Pts',(21.0100847748191,9.31315578902763,-1.96677209643634));
#37845=CARTESIAN_POINT('Ctrl Pts',(21.0033583161372,9.45502860584993,-1.94376160397975));
#37846=CARTESIAN_POINT('Ctrl Pts',(20.9966318574553,9.59782737480171,-1.92676162587731));
#37847=CARTESIAN_POINT('Ctrl Pts',(20.9899053987734,9.74101492534841,-1.91582058275154));
#37848=CARTESIAN_POINT('Ctrl Pts',(20.9847355365222,9.85106687800675,-1.90741144972626));
#37849=CARTESIAN_POINT('Ctrl Pts',(20.9795656742709,9.96134831898086,-1.90258042790854));
#37850=CARTESIAN_POINT('Ctrl Pts',(20.9743958120197,10.071614880693,-1.90132857373974));
#37851=CARTESIAN_POINT('Ctrl Pts',(20.9671175717702,10.2268504534471,-1.89956618724759));
#37852=CARTESIAN_POINT('Ctrl Pts',(20.9598393315207,10.38215201505,-1.90489782475772));
#37853=CARTESIAN_POINT('Ctrl Pts',(20.9525610912711,10.5368917561104,-1.91730062299045));
#37854=CARTESIAN_POINT('Ctrl Pts',(20.9452837330259,10.6916127452311,-1.92970191820577));
#37855=CARTESIAN_POINT('Ctrl Pts',(20.9380063747807,10.8457717972154,-1.94917264147978));
#37856=CARTESIAN_POINT('Ctrl Pts',(20.9307290165355,10.998745255065,-1.97563798213674));
#37857=CARTESIAN_POINT('Ctrl Pts',(20.9234560005045,11.1516274375505,-2.00208753159934));
#37858=CARTESIAN_POINT('Ctrl Pts',(20.9161829844736,11.3033251896582,-2.03552331724142));
#37859=CARTESIAN_POINT('Ctrl Pts',(20.9089099684426,11.4532236629269,-2.07581918851396));
#37860=CARTESIAN_POINT('Ctrl Pts',(20.9016417943633,11.6030223424974,-2.11608823313558));
#37861=CARTESIAN_POINT('Ctrl Pts',(20.894373620284,11.7510238897501,-2.16320818147162));
#37862=CARTESIAN_POINT('Ctrl Pts',(20.8871054462047,11.8966261080614,-2.21700237108486));
#37863=CARTESIAN_POINT('Ctrl Pts',(20.8798462532636,12.0420484086068,-2.27073008828768));
#37864=CARTESIAN_POINT('Ctrl Pts',(20.8725870603225,12.1850770620086,-2.33111549332836));
#37865=CARTESIAN_POINT('Ctrl Pts',(20.8653278673814,12.3251271892484,-2.39793282906112));
#37866=CARTESIAN_POINT('Ctrl Pts',(20.8629019672915,12.3719295843671,-2.42026205795495));
#37867=CARTESIAN_POINT('Ctrl Pts',(20.8604760672015,12.4183994834494,-2.44330918750438));
#37868=CARTESIAN_POINT('Ctrl Pts',(20.8580501671115,12.4645155072712,-2.46706457350171));
#37869=CARTESIAN_POINT('Ctrl Pts',(20.851319308004,12.5924682041796,-2.53297584365391));
#37870=CARTESIAN_POINT('Ctrl Pts',(20.8445884488965,12.7176517637429,-2.60432077926021));
#37871=CARTESIAN_POINT('Ctrl Pts',(20.8378575897889,12.8395943566171,-2.68083462018041));
#37872=CARTESIAN_POINT('Ctrl Pts',(20.8311269491109,12.9615329922165,-2.75734597807738));
#37873=CARTESIAN_POINT('Ctrl Pts',(20.8243963084329,13.0802305615075,-2.8390257118703));
#37874=CARTESIAN_POINT('Ctrl Pts',(20.8176656677548,13.1952429162414,-2.92556490154576));
#37875=CARTESIAN_POINT('Ctrl Pts',(20.8109315848184,13.3103140918602,-3.01214835004661));
#37876=CARTESIAN_POINT('Ctrl Pts',(20.804197501882,13.4216959931946,-3.10359600184866));
#37877=CARTESIAN_POINT('Ctrl Pts',(20.7974634189456,13.52897595819,-3.19955736661001));
#37878=CARTESIAN_POINT('Ctrl Pts',(20.790727670196,13.6362824610811,-3.29554246937953));
#37879=CARTESIAN_POINT('Ctrl Pts',(20.7839919214463,13.7394847375183,-3.3960432610415));
#37880=CARTESIAN_POINT('Ctrl Pts',(20.7772561726966,13.8382061214154,-3.5006715065636));
#37881=CARTESIAN_POINT('Ctrl Pts',(20.7705141740967,13.9370191052046,-3.60539683273453));
#37882=CARTESIAN_POINT('Ctrl Pts',(20.7637721754969,14.0313426428299,-3.71425699380575));
#37883=CARTESIAN_POINT('Ctrl Pts',(20.757030176897,14.1208391087228,-3.82682916955609));
#37884=CARTESIAN_POINT('Ctrl Pts',(20.7519216253324,14.1886524290741,-3.91212743179073));
#37885=CARTESIAN_POINT('Ctrl Pts',(20.7468130737678,14.2536951325735,-3.99955619341295));
#37886=CARTESIAN_POINT('Ctrl Pts',(20.7417045222033,14.3158368081123,-4.08892028122819));
#37887=CARTESIAN_POINT('Ctrl Pts',(20.7349885913884,14.3975310395132,-4.20640231571828));
#37888=CARTESIAN_POINT('Ctrl Pts',(20.7282726605735,14.4743500912044,-4.3274317992558));
#37889=CARTESIAN_POINT('Ctrl Pts',(20.7215567297586,14.5459825288401,-4.45157243139028));
#37890=CARTESIAN_POINT('Ctrl Pts',(20.7148461574089,14.6175578128304,-4.57561401496664));
#37891=CARTESIAN_POINT('Ctrl Pts',(20.7081355850593,14.6839545411525,-4.70276148394193));
#37892=CARTESIAN_POINT('Ctrl Pts',(20.7014250127097,14.7449047642867,-4.83254991711475));
#37893=CARTESIAN_POINT('Ctrl Pts',(20.6947184269592,14.8058187782729,-4.962261245917));
#37894=CARTESIAN_POINT('Ctrl Pts',(20.6880118412087,14.8612925759747,-5.09461007959434));
#37895=CARTESIAN_POINT('Ctrl Pts',(20.6813052554582,14.9111043584523,-5.22910735524996));
#37896=CARTESIAN_POINT('Ctrl Pts',(20.6746012879102,14.9608966947709,-5.36355212414347));
#37897=CARTESIAN_POINT('Ctrl Pts',(20.6678973203622,15.0050312919063,-5.50014331759118));
#37898=CARTESIAN_POINT('Ctrl Pts',(20.6611933528142,15.0433346977241,-5.63837245788636));
#37899=CARTESIAN_POINT('Ctrl Pts',(20.6544893167563,15.0816384949762,-5.77660301078764));
#37900=CARTESIAN_POINT('Ctrl Pts',(20.6477852806984,15.1141108743886,-5.91647119019885));
#37901=CARTESIAN_POINT('Ctrl Pts',(20.6410812446405,15.1406283667068,-6.05745371870328));
#37902=CARTESIAN_POINT('Ctrl Pts',(20.6343768576303,15.1671472471998,-6.19844362755812));
#37903=CARTESIAN_POINT('Ctrl Pts',(20.6276724706202,15.1877105506822,-6.34054763828436));
#37904=CARTESIAN_POINT('Ctrl Pts',(20.62096808361,15.2022460867859,-6.48323299350801));
#37905=CARTESIAN_POINT('Ctrl Pts',(20.6142621064915,15.2167850703453,-6.62595219003299));
#37906=CARTESIAN_POINT('Ctrl Pts',(20.6075561293729,15.2252934010757,-6.76925263776888));
#37907=CARTESIAN_POINT('Ctrl Pts',(20.6008501522544,15.227750853798,-6.91259730125182));
#37908=CARTESIAN_POINT('Ctrl Pts',(20.5941413450238,15.2302093436348,-7.05600246023726));
#37909=CARTESIAN_POINT('Ctrl Pts',(20.5874325377932,15.2266118621726,-7.19945150257357));
#37910=CARTESIAN_POINT('Ctrl Pts',(20.5807237305627,15.2169902963606,-7.34240835917999));
#37911=CARTESIAN_POINT('Ctrl Pts',(20.5740069743706,15.2073573303917,-7.48553459888302));
#37912=CARTESIAN_POINT('Ctrl Pts',(20.5672902181786,15.1916860472491,-7.62816711857751));
#37913=CARTESIAN_POINT('Ctrl Pts',(20.5605734619866,15.1700602117555,-7.76977513058491));
#37914=CARTESIAN_POINT('Ctrl Pts',(20.5538523224127,15.1484202631557,-7.9114755565444));
#37915=CARTESIAN_POINT('Ctrl Pts',(20.5471311828389,15.1208180850618,-8.05214977921533));
#37916=CARTESIAN_POINT('Ctrl Pts',(20.5404100432651,15.0873882866751,-8.19127861428367));
#37917=CARTESIAN_POINT('Ctrl Pts',(20.5336789815349,15.0539091371805,-8.33061283982664));
#37918=CARTESIAN_POINT('Ctrl Pts',(20.5269479198048,15.0145852798129,-8.46839676418098));
#37919=CARTESIAN_POINT('Ctrl Pts',(20.5202168580746,14.9696010262843,-8.60412688256326));
#37920=CARTESIAN_POINT('Ctrl Pts',(20.5164823161787,14.9446427676626,-8.67943295372376));
#37921=CARTESIAN_POINT('Ctrl Pts',(20.5127477742828,14.9179429442996,-8.75410715651371));
#37922=CARTESIAN_POINT('Ctrl Pts',(20.5090132323869,14.8895392850499,-8.82806646618269));
#37923=CARTESIAN_POINT('Ctrl Pts',(20.5025200449742,14.8401543034763,-8.95665831813692));
#37924=CARTESIAN_POINT('Ctrl Pts',(20.4960268575615,14.7854588635406,-9.08349642489812));
#37925=CARTESIAN_POINT('Ctrl Pts',(20.4895336701487,14.7255962343738,-9.20809882124304));
#37926=CARTESIAN_POINT('Ctrl Pts',(20.4830489427434,14.6658116005356,-9.33253887248255));
#37927=CARTESIAN_POINT('Ctrl Pts',(20.4765642153381,14.6008733355466,-9.45474864825517));
#37928=CARTESIAN_POINT('Ctrl Pts',(20.4700794879328,14.5309741013637,-9.57426236716936));
#37929=CARTESIAN_POINT('Ctrl Pts',(20.4636015680842,14.46114824621,-9.69365062261074));
#37930=CARTESIAN_POINT('Ctrl Pts',(20.4571236482356,14.3863719800204,-9.81034810648507));
#37931=CARTESIAN_POINT('Ctrl Pts',(20.450645728387,14.3068853679125,-9.92391047878529));
#37932=CARTESIAN_POINT('Ctrl Pts',(20.4441729717852,14.227462110864,-10.0373823358321));
#37933=CARTESIAN_POINT('Ctrl Pts',(20.4377002151834,14.1433362049446,-10.1477237249245));
#37934=CARTESIAN_POINT('Ctrl Pts',(20.4312274585816,14.0547925601806,-10.2545167562928));
#37935=CARTESIAN_POINT('Ctrl Pts',(20.4247576155,13.9662887707232,-10.3612617179322));
#37936=CARTESIAN_POINT('Ctrl Pts',(20.4182877724184,13.8733714499816,-10.464461188119));
#37937=CARTESIAN_POINT('Ctrl Pts',(20.4118179293369,13.7763673517941,-10.5637283171446));
#37938=CARTESIAN_POINT('Ctrl Pts',(20.4053495189975,13.679384735096,-10.6629734635342));
#37939=CARTESIAN_POINT('Ctrl Pts',(20.3988811086581,13.5783174199717,-10.758287712789));
#37940=CARTESIAN_POINT('Ctrl Pts',(20.3924126983188,13.4735304075049,-10.8493196325692));
#37941=CARTESIAN_POINT('Ctrl Pts',(20.385944242306,13.3687426551373,-10.9403521951256));
#37942=CARTESIAN_POINT('Ctrl Pts',(20.3794757862932,13.2602354559434,-11.0271021046895));
#37943=CARTESIAN_POINT('Ctrl Pts',(20.3730073302804,13.1484079939686,-11.1092572959055));
#37944=CARTESIAN_POINT('Ctrl Pts',(20.3665373502499,13.0365541845895,-11.1914318435122));
#37945=CARTESIAN_POINT('Ctrl Pts',(20.3600673702195,12.9213788801603,-11.2690092826117));
#37946=CARTESIAN_POINT('Ctrl Pts',(20.353597390189,12.8033109676334,-11.3417203859027));
#37947=CARTESIAN_POINT('Ctrl Pts',(20.3471201497813,12.6851105635712,-11.4145130829604));
#37948=CARTESIAN_POINT('Ctrl Pts',(20.3406429093736,12.5640114110033,-11.4824283276885));
#37949=CARTESIAN_POINT('Ctrl Pts',(20.3341656689659,12.4404681640428,-11.5452422536957));
#37950=CARTESIAN_POINT('Ctrl Pts',(20.3276847808162,12.3168553420999,-11.6080915541802));
#37951=CARTESIAN_POINT('Ctrl Pts',(20.3212038926665,12.1907960499717,-11.6658336502188));
#37952=CARTESIAN_POINT('Ctrl Pts',(20.3147230045168,12.0627645335034,-11.7182930434107));
#37953=CARTESIAN_POINT('Ctrl Pts',(20.3082311045841,11.9345154765905,-11.770841571216));
#37954=CARTESIAN_POINT('Ctrl Pts',(20.3017392046513,11.8042878781064,-11.8180893292629));
#37955=CARTESIAN_POINT('Ctrl Pts',(20.2952473047185,11.6725715143819,-11.8599106269049));
#37956=CARTESIAN_POINT('Ctrl Pts',(20.2889388506692,11.5445771465229,-11.9005501526507));
#37957=CARTESIAN_POINT('Ctrl Pts',(20.2826303966198,11.4151773566558,-11.9360657571026));
#37958=CARTESIAN_POINT('Ctrl Pts',(20.2763219425705,11.2848280760658,-11.9663888326081));
#37959=CARTESIAN_POINT('Ctrl Pts',(20.2664266823321,11.0803659299939,-12.0139527398677));
#37960=CARTESIAN_POINT('Ctrl Pts',(20.2565314220938,10.8730095382161,-12.0488763230015));
#37961=CARTESIAN_POINT('Ctrl Pts',(20.2466361618554,10.6640303707002,-12.0709050753094));
#37962=CARTESIAN_POINT('Ctrl Pts',(20.2383086093597,10.4881598078176,-12.0894438086868));
#37963=CARTESIAN_POINT('Ctrl Pts',(20.2299810568641,10.3111395726563,-12.098850629708));
#37964=CARTESIAN_POINT('Ctrl Pts',(20.2216535043684,10.1337426824875,-12.0989982349129));
#37965=CARTESIAN_POINT('Origin',(26.8463464956315,10.1295,-7.));
#37966=CARTESIAN_POINT('',(22.6904763725673,6.08319878352126,-3.8972193977784));
#37967=CARTESIAN_POINT('',(22.5651720735025,6.0835080422226,-3.89745662547144));
#37968=CARTESIAN_POINT('',(26.8463464956315,6.08319878352126,-3.89721939777839));
#37969=CARTESIAN_POINT('',(23.2216535038443,10.1293865183057,-12.0989488216269));
#37970=CARTESIAN_POINT('Ctrl Pts',(23.2216535036445,10.1293865128977,-12.0989999987371));
#37971=CARTESIAN_POINT('Ctrl Pts',(23.2144616473686,9.97576251488196,-12.0989965795681));
#37972=CARTESIAN_POINT('Ctrl Pts',(23.2072697910928,9.82216920243597,-12.0920461851236));
#37973=CARTESIAN_POINT('Ctrl Pts',(23.2000779348169,9.66922023943467,-12.0781830945737));
#37974=CARTESIAN_POINT('Ctrl Pts',(23.1950396449697,9.56207110048146,-12.0684712391514));
#37975=CARTESIAN_POINT('Ctrl Pts',(23.1900013551225,9.45523816700231,-12.0553678804514));
#37976=CARTESIAN_POINT('Ctrl Pts',(23.1849630652753,9.34893090479854,-12.0388999680105));
#37977=CARTESIAN_POINT('Ctrl Pts',(23.1780322106042,9.20269077031505,-12.0162461089975));
#37978=CARTESIAN_POINT('Ctrl Pts',(23.1711013559331,9.05741147522505,-11.9872176032497));
#37979=CARTESIAN_POINT('Ctrl Pts',(23.1641705012619,8.91365350675345,-11.9519206682721));
#37980=CARTESIAN_POINT('Ctrl Pts',(23.1572409972287,8.76992355285804,-11.9166306117213));
#37981=CARTESIAN_POINT('Ctrl Pts',(23.1503114931954,8.6277146554914,-11.8750746419589));
#37982=CARTESIAN_POINT('Ctrl Pts',(23.1433819891621,8.48757530416641,-11.8274096877323));
#37983=CARTESIAN_POINT('Ctrl Pts',(23.1364522650283,8.34743150162177,-11.7797432195329));
#37984=CARTESIAN_POINT('Ctrl Pts',(23.1295225408946,8.20935769125029,-11.7259674819089));
#37985=CARTESIAN_POINT('Ctrl Pts',(23.1225928167608,8.07388595843718,-11.6662888800555));
#37986=CARTESIAN_POINT('Ctrl Pts',(23.1156634748197,7.93842169724982,-11.6066135696355));
#37987=CARTESIAN_POINT('Ctrl Pts',(23.1087341328786,7.80555952912581,-11.5410361807239));
#37988=CARTESIAN_POINT('Ctrl Pts',(23.1018047909375,7.67581036564082,-11.4698107541862));
#37989=CARTESIAN_POINT('Ctrl Pts',(23.0948738940547,7.54603208649339,-11.3985693446901));
#37990=CARTESIAN_POINT('Ctrl Pts',(23.0879429971719,7.4193684981623,-11.321677524493));
#37991=CARTESIAN_POINT('Ctrl Pts',(23.0810121002891,7.29630531956496,-11.2394349744694));
#37992=CARTESIAN_POINT('Ctrl Pts',(23.0768805403151,7.22294642942954,-11.1904095693044));
#37993=CARTESIAN_POINT('Ctrl Pts',(23.0727489803412,7.15086641510118,-11.139483671144));
#37994=CARTESIAN_POINT('Ctrl Pts',(23.0686174203672,7.08016321996373,-11.0867280557823));
#37995=CARTESIAN_POINT('Ctrl Pts',(23.0616832524995,6.96149912529913,-10.9981861260548));
#37996=CARTESIAN_POINT('Ctrl Pts',(23.0547490846318,6.84667369731443,-10.9044571565873));
#37997=CARTESIAN_POINT('Ctrl Pts',(23.0478149167641,6.73613270977454,-10.805897979929));
#37998=CARTESIAN_POINT('Ctrl Pts',(23.0408820598754,6.62561262119616,-10.7073574369422));
#37999=CARTESIAN_POINT('Ctrl Pts',(23.0339492029866,6.51937560346518,-10.603988728551));
#38000=CARTESIAN_POINT('Ctrl Pts',(23.0270163460979,6.4178330651246,-10.4961878617364));
#38001=CARTESIAN_POINT('Ctrl Pts',(23.0200832422255,6.3162869093225,-10.3883831545067));
#38002=CARTESIAN_POINT('Ctrl Pts',(23.0131501383532,6.21943579656273,-10.2761462111623));
#38003=CARTESIAN_POINT('Ctrl Pts',(23.0062170344808,6.127653461249,-10.159909062028));
#38004=CARTESIAN_POINT('Ctrl Pts',(22.9992843056565,6.0358760909238,-10.0436782007715));
#38005=CARTESIAN_POINT('Ctrl Pts',(22.9923515768321,5.94916715343914,-9.92344782666485));
#38006=CARTESIAN_POINT('Ctrl Pts',(22.9854188480078,5.86785936094203,-9.79968213615932));
#38007=CARTESIAN_POINT('Ctrl Pts',(22.9784845828,5.78653354957469,-9.67588901755805));
#38008=CARTESIAN_POINT('Ctrl Pts',(22.9715503175923,5.71061145639965,-9.54855929336527));
#38009=CARTESIAN_POINT('Ctrl Pts',(22.9646160523846,5.64038215784226,-9.41818568336285));
#38010=CARTESIAN_POINT('Ctrl Pts',(22.9605012934094,5.59870843641641,-9.34082262241638));
#38011=CARTESIAN_POINT('Ctrl Pts',(22.9563865344342,5.55903840082034,-9.26238827233416));
#38012=CARTESIAN_POINT('Ctrl Pts',(22.952271775459,5.52142478724157,-9.18298965493686));
#38013=CARTESIAN_POINT('Ctrl Pts',(22.9453381235802,5.45804326136591,-9.04919752373096));
#38014=CARTESIAN_POINT('Ctrl Pts',(22.9384044717014,5.40048158569252,-8.91262014426123));
#38015=CARTESIAN_POINT('Ctrl Pts',(22.9314708198227,5.34896652564976,-8.77378146923933));
#38016=CARTESIAN_POINT('Ctrl Pts',(22.9245384819542,5.29746122832944,-8.63496910581344));
#38017=CARTESIAN_POINT('Ctrl Pts',(22.9176061440857,5.25200037531062,-8.49389661159093));
#38018=CARTESIAN_POINT('Ctrl Pts',(22.9106738062172,5.21276202370896,-8.3511064623106));
#38019=CARTESIAN_POINT('Ctrl Pts',(22.9037412208191,5.17352227104248,-8.20831121449157));
#38020=CARTESIAN_POINT('Ctrl Pts',(22.896808635421,5.14050555518979,-8.06379850674376));
#38021=CARTESIAN_POINT('Ctrl Pts',(22.8898760500228,5.1138397764683,-7.9181250035164));
#38022=CARTESIAN_POINT('Ctrl Pts',(22.8829438381066,5.08717543432276,-7.77245934821475));
#38023=CARTESIAN_POINT('Ctrl Pts',(22.8760116261904,5.06686140326674,-7.62563334790481));
#38024=CARTESIAN_POINT('Ctrl Pts',(22.8690794142742,5.05297427438577,-7.4782128785143));
#38025=CARTESIAN_POINT('Ctrl Pts',(22.8621456590075,5.03908405374907,-7.33075958822291));
#38026=CARTESIAN_POINT('Ctrl Pts',(22.8552119037409,5.03162362532709,-7.18271189362287));
#38027=CARTESIAN_POINT('Ctrl Pts',(22.8482781484743,5.03061766757055,-7.03464043935698));
#38028=CARTESIAN_POINT('Ctrl Pts',(22.8441608091664,5.03002031891117,-6.94671399898356));
#38029=CARTESIAN_POINT('Ctrl Pts',(22.8400434698586,5.03169789774968,-6.85877924044733));
#38030=CARTESIAN_POINT('Ctrl Pts',(22.8359261305508,5.03564687217782,-6.77095565456406));
#38031=CARTESIAN_POINT('Ctrl Pts',(22.8289927902407,5.04229669662495,-6.62306626225001));
#38032=CARTESIAN_POINT('Ctrl Pts',(22.8220594499305,5.05539250041431,-6.47544107236297));
#38033=CARTESIAN_POINT('Ctrl Pts',(22.8151261096204,5.07488932497261,-6.32864917971362));
#38034=CARTESIAN_POINT('Ctrl Pts',(22.8081940896352,5.09438243672549,-6.18188524083354));
#38035=CARTESIAN_POINT('Ctrl Pts',(22.80126206965,5.12027409374892,-6.03595461015682));
#38036=CARTESIAN_POINT('Ctrl Pts',(22.7943300496648,5.15246762548965,-5.8914199428657));
#38037=CARTESIAN_POINT('Ctrl Pts',(22.7873977885485,5.18466227708635,-5.74688024791841));
#38038=CARTESIAN_POINT('Ctrl Pts',(22.7804655274321,5.22315917345076,-5.60373693696194));
#38039=CARTESIAN_POINT('Ctrl Pts',(22.7735332663157,5.26781068180791,-5.46254171654092));
#38040=CARTESIAN_POINT('Ctrl Pts',(22.7666013815341,5.312459766149,-5.3213541612469));
#38041=CARTESIAN_POINT('Ctrl Pts',(22.7596694967524,5.36326269333952,-5.18211479983463));
#38042=CARTESIAN_POINT('Ctrl Pts',(22.7527376119708,5.42002218067546,-5.04535945266396));
#38043=CARTESIAN_POINT('Ctrl Pts',(22.745804185402,5.47679429243441,-4.90857368842235));
#38044=CARTESIAN_POINT('Ctrl Pts',(22.7388707588332,5.53952548479134,-4.77427334785542));
#38045=CARTESIAN_POINT('Ctrl Pts',(22.7319373322645,5.60797037248123,-4.6429741563848));
#38046=CARTESIAN_POINT('Ctrl Pts',(22.7278183833905,5.6486315073879,-4.56497309132771));
#38047=CARTESIAN_POINT('Ctrl Pts',(22.7236994345166,5.69130821780808,-4.48803078158948));
#38048=CARTESIAN_POINT('Ctrl Pts',(22.7195804856426,5.73594135530312,-4.41225128043519));
#38049=CARTESIAN_POINT('Ctrl Pts',(22.7126467717647,5.811075428178,-4.28468636159476));
#38050=CARTESIAN_POINT('Ctrl Pts',(22.7057130578868,5.89178185883559,-4.16037391185343));
#38051=CARTESIAN_POINT('Ctrl Pts',(22.6987793440089,5.97775436558227,-4.03979575247022));
#38052=CARTESIAN_POINT('Ctrl Pts',(22.6960116868617,6.01207110073318,-3.99166584539737));
#38053=CARTESIAN_POINT('Ctrl Pts',(22.6932440297145,6.04722637638245,-3.944130608536));
#38054=CARTESIAN_POINT('Ctrl Pts',(22.6904763725673,6.08319878352126,-3.8972193977784));
#38055=CARTESIAN_POINT('',(23.534,15.0539061944433,-8.32288496556904));
#38056=CARTESIAN_POINT('Ctrl Pts',(23.534,15.0539061944433,-8.32288496556903));
#38057=CARTESIAN_POINT('Ctrl Pts',(23.4952181183639,14.8390046351781,-9.12285064450927));
#38058=CARTESIAN_POINT('Ctrl Pts',(23.4176543550918,14.012227531697,-10.6153576611852));
#38059=CARTESIAN_POINT('Ctrl Pts',(23.3135388565479,12.092423032665,-11.8658595382605));
#38060=CARTESIAN_POINT('Ctrl Pts',(23.2482052396401,10.6965329474454,-12.0983697707759));
#38061=CARTESIAN_POINT('Ctrl Pts',(23.2216535043684,10.1293865324873,-12.0988146186003));
#38062=CARTESIAN_POINT('',(23.5339999999999,15.0538811994916,-5.6770219948566));
#38063=CARTESIAN_POINT('Origin',(23.534,10.1295,-7.));
#38064=CARTESIAN_POINT('',(23.0963464956316,10.1294332241516,-12.0990513781753));
#38065=CARTESIAN_POINT('Ctrl Pts',(23.5339999999999,15.0538811994916,-5.6770219948566));
#38066=CARTESIAN_POINT('Ctrl Pts',(23.5270930717027,15.0921506970965,-5.8194685009863));
#38067=CARTESIAN_POINT('Ctrl Pts',(23.5201861434054,15.1242415793792,-5.96360031998381));
#38068=CARTESIAN_POINT('Ctrl Pts',(23.5132792151082,15.1500258622284,-6.10886529262073));
#38069=CARTESIAN_POINT('Ctrl Pts',(23.5063724323829,15.1758096016423,-6.25412720362094));
#38070=CARTESIAN_POINT('Ctrl Pts',(23.4994656496576,15.1952869431655,-6.40052189108961));
#38071=CARTESIAN_POINT('Ctrl Pts',(23.4925588669324,15.2083811232991,-6.54748753012045));
#38072=CARTESIAN_POINT('Ctrl Pts',(23.4856526906085,15.2214741537902,-6.69444026586755));
#38073=CARTESIAN_POINT('Ctrl Pts',(23.4787465142847,15.2281851137662,-6.84196351862882));
#38074=CARTESIAN_POINT('Ctrl Pts',(23.4718403379609,15.2284891702847,-6.98949089349636));
#38075=CARTESIAN_POINT('Ctrl Pts',(23.4649324938645,15.2287933002297,-7.13705389474971));
#38076=CARTESIAN_POINT('Ctrl Pts',(23.4580246497681,15.2226874332482,-7.28462068429066));
#38077=CARTESIAN_POINT('Ctrl Pts',(23.4511168056718,15.2101988752891,-7.43162476601365));
#38078=CARTESIAN_POINT('Ctrl Pts',(23.4457234039484,15.2004482484538,-7.54640038292906));
#38079=CARTESIAN_POINT('Ctrl Pts',(23.4403300022249,15.186807817628,-7.66083293227476));
#38080=CARTESIAN_POINT('Ctrl Pts',(23.4349366005015,15.1693125726679,-7.77465491180164));
#38081=CARTESIAN_POINT('Ctrl Pts',(23.4280029490964,15.1468210291077,-7.92098221481945));
#38082=CARTESIAN_POINT('Ctrl Pts',(23.4210692976913,15.1179485596679,-8.06635451124193));
#38083=CARTESIAN_POINT('Ctrl Pts',(23.4141356462862,15.0828010075303,-8.21021077866611));
#38084=CARTESIAN_POINT('Ctrl Pts',(23.4072033088961,15.0476601163007,-8.35403978349831));
#38085=CARTESIAN_POINT('Ctrl Pts',(23.4002709715061,15.0062465934393,-8.49635301161162));
#38086=CARTESIAN_POINT('Ctrl Pts',(23.3933386341161,14.958717003046,-8.63660139847525));
#38087=CARTESIAN_POINT('Ctrl Pts',(23.3864060491991,14.9111857155543,-8.77685479306806));
#38088=CARTESIAN_POINT('Ctrl Pts',(23.379473464282,14.857538026485,-8.91504288474696));
#38089=CARTESIAN_POINT('Ctrl Pts',(23.372540879365,14.79797999132,-9.05063296829173));
#38090=CARTESIAN_POINT('Ctrl Pts',(23.3656086679301,14.7384251647511,-9.18621574713243));
#38091=CARTESIAN_POINT('Ctrl Pts',(23.3586764564952,14.6729607630339,-9.31920049562694));
#38092=CARTESIAN_POINT('Ctrl Pts',(23.3517442450604,14.6018404979881,-9.44907563583814));
#38093=CARTESIAN_POINT('Ctrl Pts',(23.3448104902714,14.530704399069,-9.57897969082492));
#38094=CARTESIAN_POINT('Ctrl Pts',(23.3378767354823,14.453910079615,-9.70577246416573));
#38095=CARTESIAN_POINT('Ctrl Pts',(23.3309429806933,14.3717569175791,-9.82896752283444));
#38096=CARTESIAN_POINT('Ctrl Pts',(23.3268256389933,14.3229734445361,-9.90212213642044));
#38097=CARTESIAN_POINT('Ctrl Pts',(23.3227082972933,14.2723012354768,-9.97400865986319));
#38098=CARTESIAN_POINT('Ctrl Pts',(23.3185909555933,14.2198101839654,-10.0445301113552));
#38099=CARTESIAN_POINT('Ctrl Pts',(23.3116576153536,14.1314186084821,-10.1632837278912));
#38100=CARTESIAN_POINT('Ctrl Pts',(23.304724275114,14.0378366099381,-10.2782059009288));
#38101=CARTESIAN_POINT('Ctrl Pts',(23.2977909348743,13.9394203703912,-10.3888505088419));
#38102=CARTESIAN_POINT('Ctrl Pts',(23.2908589149614,13.8410228724023,-10.4994740465298));
#38103=CARTESIAN_POINT('Ctrl Pts',(23.2839268950485,13.7377931897414,-10.6058213974011));
#38104=CARTESIAN_POINT('Ctrl Pts',(23.2769948751356,13.6301267227303,-10.7074807549205));
#38105=CARTESIAN_POINT('Ctrl Pts',(23.2700626140937,13.5224565105608,-10.8091436486423));
#38106=CARTESIAN_POINT('Ctrl Pts',(23.2631303530518,13.410349443299,-10.9061179932801));
#38107=CARTESIAN_POINT('Ctrl Pts',(23.2561980920098,13.2942369915247,-10.9980296115056));
#38108=CARTESIAN_POINT('Ctrl Pts',(23.2492662073036,13.1781308432153,-11.089936240071));
#38109=CARTESIAN_POINT('Ctrl Pts',(23.2423343225974,13.0580200053115,-11.1767804876996));
#38110=CARTESIAN_POINT('Ctrl Pts',(23.2354024378912,12.9343681645872,-11.2582291600248));
#38111=CARTESIAN_POINT('Ctrl Pts',(23.2284690113988,12.8106888212852,-11.339695948121));
#38112=CARTESIAN_POINT('Ctrl Pts',(23.2215355849065,12.6834671776638,-11.4157645810553));
#38113=CARTESIAN_POINT('Ctrl Pts',(23.2146021584141,12.5531954963905,-11.4861454658511));
#38114=CARTESIAN_POINT('Ctrl Pts',(23.2104832091711,12.4758048377378,-11.5279567250417));
#38115=CARTESIAN_POINT('Ctrl Pts',(23.2063642599281,12.3973382765711,-11.5677615089315));
#38116=CARTESIAN_POINT('Ctrl Pts',(23.2022453106851,12.3179031154636,-11.6055067912478));
#38117=CARTESIAN_POINT('Ctrl Pts',(23.1953326016546,12.1845894660025,-11.6688535669748));
#38118=CARTESIAN_POINT('Ctrl Pts',(23.1884198926241,12.0484976489229,-11.7264202163307));
#38119=CARTESIAN_POINT('Ctrl Pts',(23.1815071835936,11.9101480240635,-11.7779800768106));
#38120=CARTESIAN_POINT('Ctrl Pts',(23.1744104595967,11.7681155591704,-11.8309124507215));
#38121=CARTESIAN_POINT('Ctrl Pts',(23.1673137355999,11.6237037330732,-11.8775136140333));
#38122=CARTESIAN_POINT('Ctrl Pts',(23.1602170116031,11.4774963192628,-11.9175915775158));
#38123=CARTESIAN_POINT('Ctrl Pts',(23.1533056473611,11.3351077055635,-11.9566227422935));
#38124=CARTESIAN_POINT('Ctrl Pts',(23.1463942831192,11.1910164761425,-11.9894671487316));
#38125=CARTESIAN_POINT('Ctrl Pts',(23.1394829188772,11.045776141037,-12.0159983087484));
#38126=CARTESIAN_POINT('Ctrl Pts',(23.132293515003,10.8946928828906,-12.0435967998619));
#38127=CARTESIAN_POINT('Ctrl Pts',(23.1251041111287,10.7423665149036,-12.0643634254656));
#38128=CARTESIAN_POINT('Ctrl Pts',(23.1179147072544,10.5894305429874,-12.0782147350843));
#38129=CARTESIAN_POINT('Ctrl Pts',(23.1107253033801,10.4364945710712,-12.092066044703));
#38130=CARTESIAN_POINT('Ctrl Pts',(23.1035358995059,10.2829494015725,-12.0990020099706));
#38131=CARTESIAN_POINT('Ctrl Pts',(23.0963464956316,10.1294332248244,-12.0989999995628));
#38132=CARTESIAN_POINT('Ctrl Pts',(23.0963464956316,10.1294332206623,-12.0993178216526));
#38133=CARTESIAN_POINT('Ctrl Pts',(23.0928642190134,10.0550711278111,-12.0993673700521));
#38134=CARTESIAN_POINT('Ctrl Pts',(23.0506000607591,9.15256913101046,-12.0800148503643));
#38135=CARTESIAN_POINT('Ctrl Pts',(22.9695540208687,7.44243506000627,-11.5744658280441));
#38136=CARTESIAN_POINT('Ctrl Pts',(22.8532083759605,5.61311993670382,-9.783588785421));
#38137=CARTESIAN_POINT('Ctrl Pts',(22.7368627310523,4.83541687908909,-7.34457045164505));
#38138=CARTESIAN_POINT('Ctrl Pts',(22.640850630233,5.21088719501814,-5.26560593676018));
#38139=CARTESIAN_POINT('Ctrl Pts',(22.5836204110498,5.84364847870133,-4.21017314688403));
#38140=CARTESIAN_POINT('Ctrl Pts',(22.5651720735026,6.08350804222181,-3.89745662547247));
#38141=CARTESIAN_POINT('Origin',(-18.734,19.211,1.76670989022852));
#38142=CARTESIAN_POINT('',(-17.1724222554293,21.243756036567,-21.2501821897702));
#38143=CARTESIAN_POINT('',(-17.176309351333,21.2386979557192,-21.3166133841489));
#38144=CARTESIAN_POINT('',(-17.1744642439897,21.2411350264762,1.76670989022852));
#38145=CARTESIAN_POINT('',(-21.2914665292272,19.2141433713253,-21.8332901097715));
#38146=CARTESIAN_POINT('Ctrl Pts',(-17.1763093513331,21.2386979557192,-21.3166133841489));
#38147=CARTESIAN_POINT('Ctrl Pts',(-16.9218454614608,21.0458242180231,-21.3324492449635));
#38148=CARTESIAN_POINT('Ctrl Pts',(-16.1161223190266,20.1710072681535,-21.3906770413387));
#38149=CARTESIAN_POINT('Ctrl Pts',(-16.015951705204,17.8786575813002,-21.4912967732743));
#38150=CARTESIAN_POINT('Ctrl Pts',(-18.3819424961549,16.2052786378474,-21.6184725799557));
#38151=CARTESIAN_POINT('Ctrl Pts',(-20.7940989859098,17.1742606647151,-21.7324703587881));
#38152=CARTESIAN_POINT('Ctrl Pts',(-21.2869488363774,18.6256784793645,-21.80407620206));
#38153=CARTESIAN_POINT('Ctrl Pts',(-21.2914665292272,19.2141433713253,-21.8332901097715));
#38154=CARTESIAN_POINT('',(-19.3957372685686,21.6839949024184,-22.));
#38155=CARTESIAN_POINT('Ctrl Pts',(-21.2914665292272,19.2141433713253,-21.8332901097715));
#38156=CARTESIAN_POINT('Ctrl Pts',(-21.2935044038853,19.4795925132556,-21.8464681376205));
#38157=CARTESIAN_POINT('Ctrl Pts',(-21.1334432779756,20.5957914633395,-21.90203810103));
#38158=CARTESIAN_POINT('Ctrl Pts',(-20.2191097516038,21.4636724677035,-21.9576080644395));
#38159=CARTESIAN_POINT('Ctrl Pts',(-19.3957372685686,21.6839949024184,-22.));
#38160=CARTESIAN_POINT('',(-18.0722321029123,21.6839867064714,-21.999999999982));
#38161=CARTESIAN_POINT('Origin',(-18.734,19.211,-22.));
#38162=CARTESIAN_POINT('',(-21.2939992552807,19.2090473192565,-21.7667098902285));
#38163=CARTESIAN_POINT('Ctrl Pts',(-21.2939992552807,19.2090473192565,-21.7667098902285));
#38164=CARTESIAN_POINT('Ctrl Pts',(-21.2940622859128,19.291681601191,-21.7708336286224));
#38165=CARTESIAN_POINT('Ctrl Pts',(-21.2901200772654,19.3744638362772,-21.7749573670163));
#38166=CARTESIAN_POINT('Ctrl Pts',(-21.2821561956048,19.456967483218,-21.7790811054102));
#38167=CARTESIAN_POINT('Ctrl Pts',(-21.2742021181198,19.5393695615683,-21.7831997671522));
#38168=CARTESIAN_POINT('Ctrl Pts',(-21.2622362475653,19.621493264571,-21.7873184288942));
#38169=CARTESIAN_POINT('Ctrl Pts',(-21.2462941860021,19.7029125155758,-21.7914370906363));
#38170=CARTESIAN_POINT('Ctrl Pts',(-21.2303628161442,19.7842771619339,-21.795552990156));
#38171=CARTESIAN_POINT('Ctrl Pts',(-21.2104606359213,19.8649378301924,-21.7996688896757));
#38172=CARTESIAN_POINT('Ctrl Pts',(-21.1866748718834,19.9444752707705,-21.8037847891954));
#38173=CARTESIAN_POINT('Ctrl Pts',(-21.1628974693084,20.0239847513738,-21.8078992418438));
#38174=CARTESIAN_POINT('Ctrl Pts',(-21.1352393281534,20.102371334612,-21.8120136944921));
#38175=CARTESIAN_POINT('Ctrl Pts',(-21.1038380300699,20.1792291625614,-21.8161281471405));
#38176=CARTESIAN_POINT('Ctrl Pts',(-21.0724377503042,20.2560844980759,-21.8202424663606));
#38177=CARTESIAN_POINT('Ctrl Pts',(-21.0372947356062,20.3314107390252,-21.8243567855807));
#38178=CARTESIAN_POINT('Ctrl Pts',(-20.9985947990105,20.404821760689,-21.8284711048008));
#38179=CARTESIAN_POINT('Ctrl Pts',(-20.959859212032,20.4783004085882,-21.8325892141319));
#38180=CARTESIAN_POINT('Ctrl Pts',(-20.9175603821396,20.5498598946646,-21.836707323463));
#38181=CARTESIAN_POINT('Ctrl Pts',(-20.8719298670911,20.6191391562625,-21.8408254327941));
#38182=CARTESIAN_POINT('Ctrl Pts',(-20.8262774610213,20.6884516542547,-21.8449455177684));
#38183=CARTESIAN_POINT('Ctrl Pts',(-20.7772904689067,20.7554813685366,-21.8490656027427));
#38184=CARTESIAN_POINT('Ctrl Pts',(-20.7252420320998,20.8198987443587,-21.8531856877171));
#38185=CARTESIAN_POINT('Ctrl Pts',(-20.6731075655348,20.884422594296,-21.8573125826926));
#38186=CARTESIAN_POINT('Ctrl Pts',(-20.617901867132,20.9463251318754,-21.861439477668));
#38187=CARTESIAN_POINT('Ctrl Pts',(-20.5599360229587,21.0053125814812,-21.8655663726435));
#38188=CARTESIAN_POINT('Ctrl Pts',(-20.5193323219955,21.0466318928538,-21.8684571648312));
#38189=CARTESIAN_POINT('Ctrl Pts',(-20.477375083183,21.0865216493047,-21.871347957019));
#38190=CARTESIAN_POINT('Ctrl Pts',(-20.4341804477789,21.1248930077176,-21.8742387492067));
#38191=CARTESIAN_POINT('Ctrl Pts',(-20.3717054008517,21.1803918536987,-21.8784198790135));
#38192=CARTESIAN_POINT('Ctrl Pts',(-20.3063945881463,21.2329309746761,-21.8826010088204));
#38193=CARTESIAN_POINT('Ctrl Pts',(-20.2385603336045,21.2822069434375,-21.8867821386272));
#38194=CARTESIAN_POINT('Ctrl Pts',(-20.1708211017769,21.3314138860656,-21.8909574114772));
#38195=CARTESIAN_POINT('Ctrl Pts',(-20.1005658190123,21.3773664872955,-21.8951326843272));
#38196=CARTESIAN_POINT('Ctrl Pts',(-20.0281414820515,21.4198000870231,-21.8993079571772));
#38197=CARTESIAN_POINT('Ctrl Pts',(-19.9553662537474,21.4624392748643,-21.9035034589607));
#38198=CARTESIAN_POINT('Ctrl Pts',(-19.8804012470982,21.5015249551222,-21.9076989607443));
#38199=CARTESIAN_POINT('Ctrl Pts',(-19.8036298896135,21.5368314425696,-21.9118944625278));
#38200=CARTESIAN_POINT('Ctrl Pts',(-19.7273621652182,21.571906313488,-21.9160624411101));
#38201=CARTESIAN_POINT('Ctrl Pts',(-19.6493121425953,21.6032512322234,-21.9202304196923));
#38202=CARTESIAN_POINT('Ctrl Pts',(-19.5698807349969,21.6306907647179,-21.9243983982746));
#38203=CARTESIAN_POINT('Ctrl Pts',(-19.4904743833841,21.6581216416371,-21.9285650621022));
#38204=CARTESIAN_POINT('Ctrl Pts',(-19.4096879474075,21.6816494286122,-21.9327317259298));
#38205=CARTESIAN_POINT('Ctrl Pts',(-19.3279406124946,21.7011474953965,-21.9368983897574));
#38206=CARTESIAN_POINT('Ctrl Pts',(-19.2461944456416,21.7206452835795,-21.941064994049));
#38207=CARTESIAN_POINT('Ctrl Pts',(-19.1634878556314,21.7361133602598,-21.9452315983405));
#38208=CARTESIAN_POINT('Ctrl Pts',(-19.0802520749481,21.7474758032739,-21.9493982026321));
#38209=CARTESIAN_POINT('Ctrl Pts',(-18.9960132117624,21.7589751761959,-21.9536150190779));
#38210=CARTESIAN_POINT('Ctrl Pts',(-18.9112327938041,21.7662692144946,-21.9578318355238));
#38211=CARTESIAN_POINT('Ctrl Pts',(-18.8263632855961,21.7693332510589,-21.9620486519696));
#38212=CARTESIAN_POINT('Ctrl Pts',(-18.742382112111,21.7723652161511,-21.9662213307204));
#38213=CARTESIAN_POINT('Ctrl Pts',(-18.6583141699189,21.7712553860981,-21.9703940094712));
#38214=CARTESIAN_POINT('Ctrl Pts',(-18.5745961490186,21.7660323701065,-21.9745666882221));
#38215=CARTESIAN_POINT('Ctrl Pts',(-18.489549801391,21.7607264822116,-21.9788055735154));
#38216=CARTESIAN_POINT('Ctrl Pts',(-18.404865068191,21.7511758035055,-21.9830444588087));
#38217=CARTESIAN_POINT('Ctrl Pts',(-18.3209906477349,21.7374645801874,-21.987283344102));
#38218=CARTESIAN_POINT('Ctrl Pts',(-18.2371162272788,21.7237533568693,-21.9915222293954));
#38219=CARTESIAN_POINT('Ctrl Pts',(-18.15405258588,21.7058817570232,-21.9957611146887));
#38220=CARTESIAN_POINT('Ctrl Pts',(-18.0722321029123,21.6839867064714,-21.999999999982));
#38221=CARTESIAN_POINT('Ctrl Pts',(-17.1724222554293,21.243756036567,-21.2501821897702));
#38222=CARTESIAN_POINT('Ctrl Pts',(-16.5648620804737,20.7701940639652,-21.2886333006738));
#38223=CARTESIAN_POINT('Ctrl Pts',(-15.7493319248272,19.1595847174514,-21.3694763471378));
#38224=CARTESIAN_POINT('Ctrl Pts',(-17.0720918435031,16.6810623606466,-21.4927113291624));
#38225=CARTESIAN_POINT('Ctrl Pts',(-19.9618263432431,16.4438210470481,-21.6198871358438));
#38226=CARTESIAN_POINT('Ctrl Pts',(-21.2281784392051,18.0973738826004,-21.7112199895325));
#38227=CARTESIAN_POINT('Ctrl Pts',(-21.2971424588611,19.0777088858588,-21.7601609076608));
#38228=CARTESIAN_POINT('Ctrl Pts',(-21.2960081347233,19.2090457869513,-21.7667098902285));
#38229=CARTESIAN_POINT('Origin',(-18.734,19.211,1.76670989022852));
#38230=CARTESIAN_POINT('',(-17.173927552048,21.2418454004354,-20.4499991710565));
#38231=CARTESIAN_POINT('',(-17.1744642439897,21.2411350264762,-20.5167504934799));
#38232=CARTESIAN_POINT('',(-17.1744642439897,21.2411350264762,1.76670989022852));
#38233=CARTESIAN_POINT('',(-21.2939288326654,19.209658289924,-21.0332900817688));
#38234=CARTESIAN_POINT('Ctrl Pts',(-17.1744642439897,21.2411350264762,-20.5167504934799));
#38235=CARTESIAN_POINT('Ctrl Pts',(-17.1078271467209,21.1899448669488,-20.5209209326673));
#38236=CARTESIAN_POINT('Ctrl Pts',(-17.0436732700516,21.1354397282691,-20.5250913718547));
#38237=CARTESIAN_POINT('Ctrl Pts',(-16.9823432210665,21.0778954252491,-20.5292618110421));
#38238=CARTESIAN_POINT('Ctrl Pts',(-16.9210263875684,21.0203635219582,-20.5334313515773));
#38239=CARTESIAN_POINT('Ctrl Pts',(-16.8625325082685,20.9597940700024,-20.5376008921125));
#38240=CARTESIAN_POINT('Ctrl Pts',(-16.8071671720215,20.8965014841359,-20.5417704326477));
#38241=CARTESIAN_POINT('Ctrl Pts',(-16.7517971586262,20.8332035514436,-20.545940325417));
#38242=CARTESIAN_POINT('Ctrl Pts',(-16.6995565149628,20.7671823751704,-20.5501102181863));
#38243=CARTESIAN_POINT('Ctrl Pts',(-16.6507112795958,20.6987863110799,-20.5542801109556));
#38244=CARTESIAN_POINT('Ctrl Pts',(-16.601814675656,20.630318317595,-20.5584543890337));
#38245=CARTESIAN_POINT('Ctrl Pts',(-16.5563208778988,20.559470824403,-20.5626286671118));
#38246=CARTESIAN_POINT('Ctrl Pts',(-16.5144529067884,20.4866216919667,-20.5668029451899));
#38247=CARTESIAN_POINT('Ctrl Pts',(-16.4725619714146,20.4137326023358,-20.5709795128277));
#38248=CARTESIAN_POINT('Ctrl Pts',(-16.434301032018,20.3388400971842,-20.5751560804656));
#38249=CARTESIAN_POINT('Ctrl Pts',(-16.3998462658687,20.2623450173186,-20.5793326481034));
#38250=CARTESIAN_POINT('Ctrl Pts',(-16.3653318783308,20.1857175684548,-20.5835164429783));
#38251=CARTESIAN_POINT('Ctrl Pts',(-16.3346369867409,20.1074824347686,-20.5877002378532));
#38252=CARTESIAN_POINT('Ctrl Pts',(-16.3078888304113,20.0280585002293,-20.5918840327281));
#38253=CARTESIAN_POINT('Ctrl Pts',(-16.2883209431143,19.9699551087057,-20.5949447306535));
#38254=CARTESIAN_POINT('Ctrl Pts',(-16.2708642318565,19.9112158548677,-20.5980054285788));
#38255=CARTESIAN_POINT('Ctrl Pts',(-16.255551151987,19.8520080403421,-20.6010661265042));
#38256=CARTESIAN_POINT('Ctrl Pts',(-16.2346154332719,19.7710603693827,-20.6052506479319));
#38257=CARTESIAN_POINT('Ctrl Pts',(-16.217610614143,19.6889352736661,-20.6094351693596));
#38258=CARTESIAN_POINT('Ctrl Pts',(-16.2046649078707,19.6060493535286,-20.6136196907873));
#38259=CARTESIAN_POINT('Ctrl Pts',(-16.1917376291181,19.5232814170601,-20.6177982557728));
#38260=CARTESIAN_POINT('Ctrl Pts',(-16.18285805684,19.4397552579917,-20.6219768207584));
#38261=CARTESIAN_POINT('Ctrl Pts',(-16.1781041141918,19.355900727772,-20.6261553857439));
#38262=CARTESIAN_POINT('Ctrl Pts',(-16.1732647974111,19.2705402879724,-20.6304089918873));
#38263=CARTESIAN_POINT('Ctrl Pts',(-16.1727008781513,19.1848400329948,-20.6346625980307));
#38264=CARTESIAN_POINT('Ctrl Pts',(-16.1764397024494,19.0992622517103,-20.6389162041741));
#38265=CARTESIAN_POINT('Ctrl Pts',(-16.180105918999,19.0153463859165,-20.6430872055358));
#38266=CARTESIAN_POINT('Ctrl Pts',(-16.1879092340601,18.9315487603075,-20.6472582068975));
#38267=CARTESIAN_POINT('Ctrl Pts',(-16.1998229072908,18.8483066546134,-20.6514292082593));
#38268=CARTESIAN_POINT('Ctrl Pts',(-16.2117325838689,18.7650924739571,-20.6555988103847));
#38269=CARTESIAN_POINT('Ctrl Pts',(-16.2277498149938,18.6824338981451,-20.6597684125102));
#38270=CARTESIAN_POINT('Ctrl Pts',(-16.2477960925062,18.6007622345654,-20.6639380146357));
#38271=CARTESIAN_POINT('Ctrl Pts',(-16.2678416593871,18.5190934662098,-20.6681074689506));
#38272=CARTESIAN_POINT('Ctrl Pts',(-16.2919158781826,18.4384119871213,-20.6722769232655));
#38273=CARTESIAN_POINT('Ctrl Pts',(-16.3198896103171,18.3591367325533,-20.6764463775805));
#38274=CARTESIAN_POINT('Ctrl Pts',(-16.3488485357306,18.2770695213161,-20.6807626738809));
#38275=CARTESIAN_POINT('Ctrl Pts',(-16.3819865976511,18.1965099318424,-20.6850789701814));
#38276=CARTESIAN_POINT('Ctrl Pts',(-16.4191057647636,18.1179013403771,-20.6893952664818));
#38277=CARTESIAN_POINT('Ctrl Pts',(-16.4550137295479,18.0418577555218,-20.6935707215798));
#38278=CARTESIAN_POINT('Ctrl Pts',(-16.4946467243009,17.9676401977747,-20.6977461766779));
#38279=CARTESIAN_POINT('Ctrl Pts',(-16.5377790112352,17.8956242481674,-20.7019216317759));
#38280=CARTESIAN_POINT('Ctrl Pts',(-16.5830936242915,17.8199645713388,-20.7063083486775));
#38281=CARTESIAN_POINT('Ctrl Pts',(-16.6322706438836,17.7467356488663,-20.7106950655792));
#38282=CARTESIAN_POINT('Ctrl Pts',(-16.68499874854,17.6763359092247,-20.7150817824808));
#38283=CARTESIAN_POINT('Ctrl Pts',(-16.7377268531964,17.605936169583,-20.7194684993824));
#38284=CARTESIAN_POINT('Ctrl Pts',(-16.7940056129075,17.538366010084,-20.7238552162841));
#38285=CARTESIAN_POINT('Ctrl Pts',(-16.8534788424305,17.473979511942,-20.7282419331857));
#38286=CARTESIAN_POINT('Ctrl Pts',(-16.9102137543729,17.4125575523197,-20.7324266730952));
#38287=CARTESIAN_POINT('Ctrl Pts',(-16.970066659675,17.3538038607528,-20.7366114130047));
#38288=CARTESIAN_POINT('Ctrl Pts',(-17.0327566248197,17.2980517575206,-20.7407961529141));
#38289=CARTESIAN_POINT('Ctrl Pts',(-17.0953573508923,17.2423790173243,-20.7449749358526));
#38290=CARTESIAN_POINT('Ctrl Pts',(-17.1607867741654,17.189699681497,-20.749153718791));
#38291=CARTESIAN_POINT('Ctrl Pts',(-17.2287255995826,17.1403119550623,-20.7533325017295));
#38292=CARTESIAN_POINT('Ctrl Pts',(-17.2978800168063,17.0900405613692,-20.7575860533186));
#38293=CARTESIAN_POINT('Ctrl Pts',(-17.369634193181,17.0431800825081,-20.7618396049076));
#38294=CARTESIAN_POINT('Ctrl Pts',(-17.4436142556255,17.0000037017862,-20.7660931564967));
#38295=CARTESIAN_POINT('Ctrl Pts',(-17.516162301524,16.9576630772066,-20.7702643729802));
#38296=CARTESIAN_POINT('Ctrl Pts',(-17.5908504136365,16.9188654393416,-20.7744355894636));
#38297=CARTESIAN_POINT('Ctrl Pts',(-17.6672964027753,16.8838250096592,-20.7786068059471));
#38298=CARTESIAN_POINT('Ctrl Pts',(-17.7437167203783,16.8487963469989,-20.782776621683));
#38299=CARTESIAN_POINT('Ctrl Pts',(-17.8218933248018,16.8175225782417,-20.7869464374188));
#38300=CARTESIAN_POINT('Ctrl Pts',(-17.9014210276993,16.7901711636543,-20.7911162531547));
#38301=CARTESIAN_POINT('Ctrl Pts',(-17.980945877539,16.7628207302995,-20.7952859192984));
#38302=CARTESIAN_POINT('Ctrl Pts',(-18.0618212942028,16.7393925201402,-20.7994555854421));
#38303=CARTESIAN_POINT('Ctrl Pts',(-18.1436250863857,16.7200047247385,-20.8036252515858));
#38304=CARTESIAN_POINT('Ctrl Pts',(-18.2283005696263,16.6999363281423,-20.8079412922759));
#38305=CARTESIAN_POINT('Ctrl Pts',(-18.3139703091589,16.6841974227859,-20.812257332966));
#38306=CARTESIAN_POINT('Ctrl Pts',(-18.4001544252699,16.6728614828514,-20.8165733736561));
#38307=CARTESIAN_POINT('Ctrl Pts',(-18.4835353811664,16.6618942472358,-20.8207490340291));
#38308=CARTESIAN_POINT('Ctrl Pts',(-18.5673972928076,16.6550479436589,-20.8249246944022));
#38309=CARTESIAN_POINT('Ctrl Pts',(-18.6513021326319,16.6523360785885,-20.8291003547752));
#38310=CARTESIAN_POINT('Ctrl Pts',(-18.7394381312311,16.6494874594082,-20.8334865856239));
#38311=CARTESIAN_POINT('Ctrl Pts',(-18.8276209178941,16.651201212818,-20.8378728164725));
#38312=CARTESIAN_POINT('Ctrl Pts',(-18.915347159059,16.6574312799728,-20.8422590473212));
#38313=CARTESIAN_POINT('Ctrl Pts',(-19.0030734002238,16.6636613471276,-20.8466452781698));
#38314=CARTESIAN_POINT('Ctrl Pts',(-19.0903425295494,16.6744075817306,-20.8510315090185));
#38315=CARTESIAN_POINT('Ctrl Pts',(-19.1766642028218,16.6895622348469,-20.8554177398671));
#38316=CARTESIAN_POINT('Ctrl Pts',(-19.2590223527151,16.7040210508733,-20.859602573687));
#38317=CARTESIAN_POINT('Ctrl Pts',(-19.3408244952178,16.7225461130517,-20.8637874075069));
#38318=CARTESIAN_POINT('Ctrl Pts',(-19.4216382791443,16.7450815915656,-20.8679722413268));
#38319=CARTESIAN_POINT('Ctrl Pts',(-19.5023370763703,16.7675850052486,-20.8721511207141));
#38320=CARTESIAN_POINT('Ctrl Pts',(-19.5820498690826,16.7940873783027,-20.8763300001013));
#38321=CARTESIAN_POINT('Ctrl Pts',(-19.6603530717564,16.8244816182465,-20.8805088794886));
#38322=CARTESIAN_POINT('Ctrl Pts',(-19.7400550248591,16.8554187983856,-20.8847624072828));
#38323=CARTESIAN_POINT('Ctrl Pts',(-19.8182960576179,16.8903881737627,-20.8890159350769));
#38324=CARTESIAN_POINT('Ctrl Pts',(-19.8946441220389,16.9292232313444,-20.8932694628711));
#38325=CARTESIAN_POINT('Ctrl Pts',(-19.9695165810175,16.9673077103389,-20.8974407812627));
#38326=CARTESIAN_POINT('Ctrl Pts',(-20.0425681641198,17.0091095557736,-20.9016120996543));
#38327=CARTESIAN_POINT('Ctrl Pts',(-20.1134118643462,17.0544233358165,-20.9057834180459));
#38328=CARTESIAN_POINT('Ctrl Pts',(-20.1842318054818,17.0997219188241,-20.9099533374884));
#38329=CARTESIAN_POINT('Ctrl Pts',(-20.2528449471495,17.1485298496365,-20.9141232569308));
#38330=CARTESIAN_POINT('Ctrl Pts',(-20.3188911542421,17.2005970480511,-20.9182931763733));
#38331=CARTESIAN_POINT('Ctrl Pts',(-20.3849350181168,17.2526623992014,-20.9224629478734));
#38332=CARTESIAN_POINT('Ctrl Pts',(-20.4484117677876,17.3079865025997,-20.9266327193736));
#38333=CARTESIAN_POINT('Ctrl Pts',(-20.5089934936092,17.3662783143127,-20.9308024908737));
#38334=CARTESIAN_POINT('Ctrl Pts',(-20.5716985989688,17.4266132444504,-20.9351184121799));
#38335=CARTESIAN_POINT('Ctrl Pts',(-20.6313015884267,17.4901274194612,-20.9394343334862));
#38336=CARTESIAN_POINT('Ctrl Pts',(-20.6874809779159,17.5564571420115,-20.9437502547924));
#38337=CARTESIAN_POINT('Ctrl Pts',(-20.7418360321656,17.6206329135956,-20.9479260235017));
#38338=CARTESIAN_POINT('Ctrl Pts',(-20.7929861867181,17.6874437676866,-20.9521017922111));
#38339=CARTESIAN_POINT('Ctrl Pts',(-20.84068298328,17.756528684381,-20.9562775609204));
#38340=CARTESIAN_POINT('Ctrl Pts',(-20.8907810730051,17.8290916782231,-20.9606635585251));
#38341=CARTESIAN_POINT('Ctrl Pts',(-20.937068653801,17.9041632231128,-20.9650495561297));
#38342=CARTESIAN_POINT('Ctrl Pts',(-20.9793120563336,17.9812952510122,-20.9694355537344));
#38343=CARTESIAN_POINT('Ctrl Pts',(-21.0215554588661,18.0584272789116,-20.9738215513391));
#38344=CARTESIAN_POINT('Ctrl Pts',(-21.0597544996862,18.1376192346801,-20.9782075489438));
#38345=CARTESIAN_POINT('Ctrl Pts',(-21.0937343932684,18.2184005877363,-20.9825935465485));
#38346=CARTESIAN_POINT('Ctrl Pts',(-21.1297845102027,18.3041035407708,-20.9872467608424));
#38347=CARTESIAN_POINT('Ctrl Pts',(-21.1612011557346,18.3918658581185,-20.9918999751363));
#38348=CARTESIAN_POINT('Ctrl Pts',(-21.1877704304992,18.4811981951189,-20.9965531894303));
#38349=CARTESIAN_POINT('Ctrl Pts',(-21.2142564917145,18.5702507480116,-21.0011918301056));
#38350=CARTESIAN_POINT('Ctrl Pts',(-21.2359253488098,18.6608632602714,-21.0058304707809));
#38351=CARTESIAN_POINT('Ctrl Pts',(-21.2526114411354,18.7525281812567,-21.0104691114562));
#38352=CARTESIAN_POINT('Ctrl Pts',(-21.2692072331732,18.8436970382994,-21.0150826491548));
#38353=CARTESIAN_POINT('Ctrl Pts',(-21.2808739262263,18.9359066855585,-21.0196961868533));
#38354=CARTESIAN_POINT('Ctrl Pts',(-21.2874965126302,19.0286389296337,-21.0243097245519));
#38355=CARTESIAN_POINT('Ctrl Pts',(-21.2917935179279,19.0888074075896,-21.0273031767656));
#38356=CARTESIAN_POINT('Ctrl Pts',(-21.2939679583765,19.1491955214723,-21.0302966289794));
#38357=CARTESIAN_POINT('Ctrl Pts',(-21.2939996483756,19.2096582411964,-21.0332900811932));
#38358=CARTESIAN_POINT('Ctrl Pts',(-21.2904840295148,19.2096606602608,-21.0332901097715));
#38359=CARTESIAN_POINT('Ctrl Pts',(-21.288030249326,19.7238724906044,-21.0587831909243));
#38360=CARTESIAN_POINT('Ctrl Pts',(-20.8878309688531,21.0966582904734,-21.1266682076376));
#38361=CARTESIAN_POINT('Ctrl Pts',(-18.9689508715201,22.0730071282985,-21.2211092990968));
#38362=CARTESIAN_POINT('Ctrl Pts',(-17.6030346275064,21.5621391285562,-21.2900573094031));
#38363=CARTESIAN_POINT('Ctrl Pts',(-17.1763093513331,21.2386979557192,-21.3166133841489));
#38364=CARTESIAN_POINT('',(-21.2964371679699,19.2128544327287,-20.9667098902285));
#38365=CARTESIAN_POINT('Ctrl Pts',(-21.2964371679699,19.2128544327287,-20.9667098902285));
#38366=CARTESIAN_POINT('Ctrl Pts',(-21.2973789664463,19.3284704701528,-20.9724759609646));
#38367=CARTESIAN_POINT('Ctrl Pts',(-21.2376963737069,20.2931122040567,-21.0206339672611));
#38368=CARTESIAN_POINT('Ctrl Pts',(-20.0126665865687,21.9547543377114,-21.1111839091181));
#38369=CARTESIAN_POINT('Ctrl Pts',(-17.9939164834006,21.8268016750118,-21.1999086048959));
#38370=CARTESIAN_POINT('Ctrl Pts',(-17.2346906284817,21.2922910373603,-21.2462413651133));
#38371=CARTESIAN_POINT('Ctrl Pts',(-17.1724222554293,21.243756036567,-21.2501821897702));
#38372=CARTESIAN_POINT('Ctrl Pts',(-17.1739275520481,21.2418454004355,-20.4499991710565));
#38373=CARTESIAN_POINT('Ctrl Pts',(-17.0385457538407,21.1400081684298,-20.4584344059413));
#38374=CARTESIAN_POINT('Ctrl Pts',(-16.2862201916857,20.4464549384029,-20.5092615763866));
#38375=CARTESIAN_POINT('Ctrl Pts',(-15.8255860927207,18.3717008434114,-20.6024806823924));
#38376=CARTESIAN_POINT('Ctrl Pts',(-17.8654473830542,16.3111912047089,-20.7296564890738));
#38377=CARTESIAN_POINT('Ctrl Pts',(-20.5735369877998,16.8838680312786,-20.8510662250192));
#38378=CARTESIAN_POINT('Ctrl Pts',(-21.2904548994085,18.4784657038926,-20.9300840254041));
#38379=CARTESIAN_POINT('Ctrl Pts',(-21.2964371679699,19.2128544327287,-20.9667098902285));
#38380=CARTESIAN_POINT('Origin',(-18.734,19.211,1.76670989022852));
#38381=CARTESIAN_POINT('',(-17.1744642439897,21.2411350264762,-19.6501081077316));
#38382=CARTESIAN_POINT('',(-17.1744642439897,21.2411350264762,-19.7167245443048));
#38383=CARTESIAN_POINT('',(-17.1744642439897,21.2411350264762,1.76670989022852));
#38384=CARTESIAN_POINT('',(-21.2939995273706,19.2094444092821,-20.2332901098006));
#38385=CARTESIAN_POINT('Ctrl Pts',(-17.1744642439897,21.2411350264762,-19.7167245443048));
#38386=CARTESIAN_POINT('Ctrl Pts',(-17.1080940647866,21.1901499115699,-19.7209062128092));
#38387=CARTESIAN_POINT('Ctrl Pts',(-17.0441149697057,21.1358207858829,-19.7250878813135));
#38388=CARTESIAN_POINT('Ctrl Pts',(-16.982882251611,21.0784010365417,-19.7292695498179));
#38389=CARTESIAN_POINT('Ctrl Pts',(-16.9217271760624,21.0210540949359,-19.7334459160035));
#38390=CARTESIAN_POINT('Ctrl Pts',(-16.8633118927493,20.9606246273613,-19.7376222821892));
#38391=CARTESIAN_POINT('Ctrl Pts',(-16.8079596809234,20.8974070354725,-19.7417986483748));
#38392=CARTESIAN_POINT('Ctrl Pts',(-16.7526597829306,20.8342491910526,-19.7459710674422));
#38393=CARTESIAN_POINT('Ctrl Pts',(-16.7004175050121,20.7683088038869,-19.7501434865096));
#38394=CARTESIAN_POINT('Ctrl Pts',(-16.6515192476679,20.6999170279657,-19.754315905577));
#38395=CARTESIAN_POINT('Ctrl Pts',(-16.60264546862,20.6315594887279,-19.758486235946));
#38396=CARTESIAN_POINT('Ctrl Pts',(-16.5571126534136,20.5607533708702,-19.7626565663151));
#38397=CARTESIAN_POINT('Ctrl Pts',(-16.5151661257008,20.487861871254,-19.7668268966841));
#38398=CARTESIAN_POINT('Ctrl Pts',(-16.4732280132432,20.4149849950311,-19.7709963904071));
#38399=CARTESIAN_POINT('Ctrl Pts',(-16.4348749882279,20.3400239668443,-19.7751658841302));
#38400=CARTESIAN_POINT('Ctrl Pts',(-16.4003076097238,20.2633686747366,-19.7793353778532));
#38401=CARTESIAN_POINT('Ctrl Pts',(-16.365736796812,20.1867057666183,-19.7835052858322));
#38402=CARTESIAN_POINT('Ctrl Pts',(-16.3349525651543,20.1083486802376,-19.7876751938112));
#38403=CARTESIAN_POINT('Ctrl Pts',(-16.3081077362453,20.0287082148634,-19.7918451017901));
#38404=CARTESIAN_POINT('Ctrl Pts',(-16.2812344363892,19.948983284824,-19.7960194322681));
#38405=CARTESIAN_POINT('Ctrl Pts',(-16.2583090282375,19.8679726950072,-19.8001937627461));
#38406=CARTESIAN_POINT('Ctrl Pts',(-16.2394345742077,19.7861028920479,-19.8043680932241));
#38407=CARTESIAN_POINT('Ctrl Pts',(-16.2205495154889,19.7041870902052,-19.8085447690667));
#38408=CARTESIAN_POINT('Ctrl Pts',(-16.2057200237114,19.6214115669634,-19.8127214449094));
#38409=CARTESIAN_POINT('Ctrl Pts',(-16.194997652802,19.5382110647933,-19.816898120752));
#38410=CARTESIAN_POINT('Ctrl Pts',(-16.1842568910067,19.4548678580888,-19.8210819603805));
#38411=CARTESIAN_POINT('Ctrl Pts',(-16.1776373544537,19.3710986755521,-19.825265800009));
#38412=CARTESIAN_POINT('Ctrl Pts',(-16.1751385298197,19.2873411843422,-19.8294496396375));
#38413=CARTESIAN_POINT('Ctrl Pts',(-16.1734340306215,19.230208492968,-19.8323035218969));
#38414=CARTESIAN_POINT('Ctrl Pts',(-16.1736457558925,19.1730812523769,-19.8351574041563));
#38415=CARTESIAN_POINT('Ctrl Pts',(-16.1757597065464,19.1160968865085,-19.8380112864156));
#38416=CARTESIAN_POINT('Ctrl Pts',(-16.1788593811049,19.0325410150462,-19.8421959187372));
#38417=CARTESIAN_POINT('Ctrl Pts',(-16.1860627143394,18.9489816683593,-19.8463805510587));
#38418=CARTESIAN_POINT('Ctrl Pts',(-16.1973733531866,18.8658547339507,-19.8505651833802));
#38419=CARTESIAN_POINT('Ctrl Pts',(-16.2086678927321,18.7828461204975,-19.8547438593928));
#38420=CARTESIAN_POINT('Ctrl Pts',(-16.2240580639186,18.700269148709,-19.8589225354055));
#38421=CARTESIAN_POINT('Ctrl Pts',(-16.2434955346196,18.6185580130341,-19.8631012114182));
#38422=CARTESIAN_POINT('Ctrl Pts',(-16.2632814202296,18.5353822126226,-19.8673547898215));
#38423=CARTESIAN_POINT('Ctrl Pts',(-16.287261115507,18.4531040767777,-19.8716083682248));
#38424=CARTESIAN_POINT('Ctrl Pts',(-16.315328555729,18.3721743657541,-19.875861946628));
#38425=CARTESIAN_POINT('Ctrl Pts',(-16.3428518369366,18.2928136838773,-19.8800330585501));
#38426=CARTESIAN_POINT('Ctrl Pts',(-16.3743056171544,18.2147500627578,-19.8842041704722));
#38427=CARTESIAN_POINT('Ctrl Pts',(-16.4095391529049,18.1383948674737,-19.8883752823943));
#38428=CARTESIAN_POINT('Ctrl Pts',(-16.4447608657818,18.0620652937402,-19.8925449946689));
#38429=CARTESIAN_POINT('Ctrl Pts',(-16.4837596226908,17.9874434246684,-19.8967147069435));
#38430=CARTESIAN_POINT('Ctrl Pts',(-16.5263367853317,17.9149200909664,-19.9008844192181));
#38431=CARTESIAN_POINT('Ctrl Pts',(-16.5689124330239,17.8423993377355,-19.9050539831292));
#38432=CARTESIAN_POINT('Ctrl Pts',(-16.6150659996536,17.7719773677011,-19.9092235470402));
#38433=CARTESIAN_POINT('Ctrl Pts',(-16.6645538728597,17.7040186706983,-19.9133931109512));
#38434=CARTESIAN_POINT('Ctrl Pts',(-16.7157817325743,17.6336705556774,-19.9177092761301));
#38435=CARTESIAN_POINT('Ctrl Pts',(-16.7705824268663,17.5659625858456,-19.9220254413089));
#38436=CARTESIAN_POINT('Ctrl Pts',(-16.828639391307,17.5012629000805,-19.9263416064877));
#38437=CARTESIAN_POINT('Ctrl Pts',(-16.8848050978436,17.4386708648494,-19.9305171686985));
#38438=CARTESIAN_POINT('Ctrl Pts',(-16.9440178150289,17.3788944293155,-19.9346927309094));
#38439=CARTESIAN_POINT('Ctrl Pts',(-17.0059537750657,17.3222289062752,-19.9388682931203));
#38440=CARTESIAN_POINT('Ctrl Pts',(-17.0710180730474,17.2627012510296,-19.9432547597831));
#38441=CARTESIAN_POINT('Ctrl Pts',(-17.1390875043195,17.2066074135524,-19.9476412264458));
#38442=CARTESIAN_POINT('Ctrl Pts',(-17.2097498587669,17.154240046347,-19.9520276931086));
#38443=CARTESIAN_POINT('Ctrl Pts',(-17.2804122132143,17.1018726791415,-19.9564141597714));
#38444=CARTESIAN_POINT('Ctrl Pts',(-17.3536669653909,17.0532320397927,-19.9608006264342));
#38445=CARTESIAN_POINT('Ctrl Pts',(-17.4290716121177,17.0085554711869,-19.965187093097));
#38446=CARTESIAN_POINT('Ctrl Pts',(-17.501006718607,16.9659345736727,-19.9693717283973));
#38447=CARTESIAN_POINT('Ctrl Pts',(-17.5751659817943,16.9267623274508,-19.9735563636976));
#38448=CARTESIAN_POINT('Ctrl Pts',(-17.6511848627828,16.8912777367509,-19.9777409989979));
#38449=CARTESIAN_POINT('Ctrl Pts',(-17.7270955400278,16.8558436541026,-19.9819196779726));
#38450=CARTESIAN_POINT('Ctrl Pts',(-17.8048601641239,16.8240869938583,-19.9860983569473));
#38451=CARTESIAN_POINT('Ctrl Pts',(-17.8840874845046,16.7962021376512,-19.990277035922));
#38452=CARTESIAN_POINT('Ctrl Pts',(-17.9647348762106,16.7678174729877,-19.9945306135827));
#38453=CARTESIAN_POINT('Ctrl Pts',(-18.0468975020319,16.7434450254351,-19.9987841912434));
#38454=CARTESIAN_POINT('Ctrl Pts',(-18.1301389337681,16.723239599019,-20.0030377689041));
#38455=CARTESIAN_POINT('Ctrl Pts',(-18.2117665887585,16.7034258891629,-20.0072088837266));
#38456=CARTESIAN_POINT('Ctrl Pts',(-18.2944311263188,16.6876191861686,-20.0113799985491));
#38457=CARTESIAN_POINT('Ctrl Pts',(-18.3777050584842,16.6759154028612,-20.0155511133716));
#38458=CARTESIAN_POINT('Ctrl Pts',(-18.4609510469055,16.6642155469237,-20.0197208285176));
#38459=CARTESIAN_POINT('Ctrl Pts',(-18.5448055686334,16.6566159403141,-20.0238905436636));
#38460=CARTESIAN_POINT('Ctrl Pts',(-18.6288324772911,16.6531611090283,-20.0280602588096));
#38461=CARTESIAN_POINT('Ctrl Pts',(-18.7128563955109,16.6497064006967,-20.0322298255595));
#38462=CARTESIAN_POINT('Ctrl Pts',(-18.7970522287831,16.6503961924512,-20.0363993923093));
#38463=CARTESIAN_POINT('Ctrl Pts',(-18.880981635612,16.6552229364061,-20.0405689590591));
#38464=CARTESIAN_POINT('Ctrl Pts',(-18.9678618596805,16.6602193805865,-20.0448851207857));
#38465=CARTESIAN_POINT('Ctrl Pts',(-19.0544560473056,16.6696490660325,-20.0492012825123));
#38466=CARTESIAN_POINT('Ctrl Pts',(-19.1402833031872,16.6834450792216,-20.0535174442389));
#38467=CARTESIAN_POINT('Ctrl Pts',(-19.2233147795964,16.6967916942552,-20.0576930091793));
#38468=CARTESIAN_POINT('Ctrl Pts',(-19.3056280709207,16.7142243988718,-20.0618685741196));
#38469=CARTESIAN_POINT('Ctrl Pts',(-19.3867996159112,16.735630802998,-20.0660441390599));
#38470=CARTESIAN_POINT('Ctrl Pts',(-19.4720708905892,16.7581183799726,-20.0704305991796));
#38471=CARTESIAN_POINT('Ctrl Pts',(-19.5560814939681,16.7849914459207,-20.0748170592994));
#38472=CARTESIAN_POINT('Ctrl Pts',(-19.6383622323597,16.8160618060832,-20.0792035194192));
#38473=CARTESIAN_POINT('Ctrl Pts',(-19.7206429707512,16.8471321662457,-20.0835899795389));
#38474=CARTESIAN_POINT('Ctrl Pts',(-19.8011933431587,16.8823995182362,-20.0879764396587));
#38475=CARTESIAN_POINT('Ctrl Pts',(-19.8795742651096,16.9216202579916,-20.0923628997785));
#38476=CARTESIAN_POINT('Ctrl Pts',(-19.9543489005549,16.9590364613751,-20.0965475399714));
#38477=CARTESIAN_POINT('Ctrl Pts',(-20.0274276526341,17.0001895262269,-20.1007321801642));
#38478=CARTESIAN_POINT('Ctrl Pts',(-20.0984122381085,17.0449023003337,-20.1049168203571));
#38479=CARTESIAN_POINT('Ctrl Pts',(-20.1692957865176,17.0895514317855,-20.1090955042742));
#38480=CARTESIAN_POINT('Ctrl Pts',(-20.2380907031438,17.137749965204,-20.1132741881914));
#38481=CARTESIAN_POINT('Ctrl Pts',(-20.3044217668728,17.189274134772,-20.1174528721085));
#38482=CARTESIAN_POINT('Ctrl Pts',(-20.3719416499117,17.2417217469061,-20.1217064485398));
#38483=CARTESIAN_POINT('Ctrl Pts',(-20.4369080598406,17.2976151641855,-20.1259600249711));
#38484=CARTESIAN_POINT('Ctrl Pts',(-20.4989546019222,17.3566712122297,-20.1302136014024));
#38485=CARTESIAN_POINT('Ctrl Pts',(-20.5597983571728,17.4145824448741,-20.1343847212528));
#38486=CARTESIAN_POINT('Ctrl Pts',(-20.6178340905372,17.4755344539392,-20.1385558411033));
#38487=CARTESIAN_POINT('Ctrl Pts',(-20.6727497630573,17.5392197045529,-20.1427269609537));
#38488=CARTESIAN_POINT('Ctrl Pts',(-20.7276470081433,17.6028835850239,-20.1468966811484));
#38489=CARTESIAN_POINT('Ctrl Pts',(-20.7794259715033,17.6692785374397,-20.151066401343));
#38490=CARTESIAN_POINT('Ctrl Pts',(-20.8278131357729,17.7380619318977,-20.1552361215377));
#38491=CARTESIAN_POINT('Ctrl Pts',(-20.8761985781537,17.8068428786539,-20.1594056933502));
#38492=CARTESIAN_POINT('Ctrl Pts',(-20.9211921974361,17.8780117217137,-20.1635752651627));
#38493=CARTESIAN_POINT('Ctrl Pts',(-20.9625630739946,17.9511957988531,-20.1677448369751));
#38494=CARTESIAN_POINT('Ctrl Pts',(-21.0053883703184,18.0269527092786,-20.1720609927655));
#38495=CARTESIAN_POINT('Ctrl Pts',(-21.0443311966684,18.104868729537,-20.1763771485559));
#38496=CARTESIAN_POINT('Ctrl Pts',(-21.0791875184544,18.1845032862763,-20.1806933043463));
#38497=CARTESIAN_POINT('Ctrl Pts',(-21.112908500301,18.2615439866305,-20.1848688743318));
#38498=CARTESIAN_POINT('Ctrl Pts',(-21.1428049786358,18.3401925327768,-20.1890444443173));
#38499=CARTESIAN_POINT('Ctrl Pts',(-21.1687421896672,18.4200319413184,-20.1932200143028));
#38500=CARTESIAN_POINT('Ctrl Pts',(-21.1959893070235,18.5039034775277,-20.1976064629957));
#38501=CARTESIAN_POINT('Ctrl Pts',(-21.2188665678873,18.5890887630882,-20.2019929116885));
#38502=CARTESIAN_POINT('Ctrl Pts',(-21.2372782491424,18.6750914188312,-20.2063793603814));
#38503=CARTESIAN_POINT('Ctrl Pts',(-21.2556899303975,18.7610940745742,-20.2107658090742));
#38504=CARTESIAN_POINT('Ctrl Pts',(-21.2696360151223,18.8479135155775,-20.215152257767));
#38505=CARTESIAN_POINT('Ctrl Pts',(-21.2790836672405,18.935048687726,-20.2195387064599));
#38506=CARTESIAN_POINT('Ctrl Pts',(-21.288956382332,19.0261041921328,-20.2241225075637));
#38507=CARTESIAN_POINT('Ctrl Pts',(-21.2939437779116,19.1176988534549,-20.2287063086676));
#38508=CARTESIAN_POINT('Ctrl Pts',(-21.2939995273702,19.2094444086991,-20.2332901097715));
#38509=CARTESIAN_POINT('Ctrl Pts',(-21.2939995273706,19.209444409282,-20.2332901098006));
#38510=CARTESIAN_POINT('Ctrl Pts',(-21.2940497238898,19.292051655634,-20.2374173417521));
#38511=CARTESIAN_POINT('Ctrl Pts',(-21.2900972916445,19.3748187808655,-20.2415445737036));
#38512=CARTESIAN_POINT('Ctrl Pts',(-21.2821221995875,19.4573194185792,-20.2456718056551));
#38513=CARTESIAN_POINT('Ctrl Pts',(-21.2739869560054,19.5414767898907,-20.249881918467));
#38514=CARTESIAN_POINT('Ctrl Pts',(-21.2616656478282,19.6253563615795,-20.254092031279));
#38515=CARTESIAN_POINT('Ctrl Pts',(-21.2451929662144,19.7085036546953,-20.2583021440909));
#38516=CARTESIAN_POINT('Ctrl Pts',(-21.2290800677258,19.7898349111956,-20.262420302989));
#38517=CARTESIAN_POINT('Ctrl Pts',(-21.2089953889688,19.8704650608503,-20.2665384618872));
#38518=CARTESIAN_POINT('Ctrl Pts',(-21.1850236968841,19.9499741790566,-20.2706566207853));
#38519=CARTESIAN_POINT('Ctrl Pts',(-21.1610629739661,20.0294469148178,-20.274772895262));
#38520=CARTESIAN_POINT('Ctrl Pts',(-21.1332189034159,20.1077991846501,-20.2788891697386));
#38521=CARTESIAN_POINT('Ctrl Pts',(-21.1016267106028,20.1846240338243,-20.2830054442153));
#38522=CARTESIAN_POINT('Ctrl Pts',(-21.0700389112288,20.2614381991786,-20.287121146253));
#38523=CARTESIAN_POINT('Ctrl Pts',(-21.0347042052762,20.3367249283834,-20.2912368482907));
#38524=CARTESIAN_POINT('Ctrl Pts',(-20.9958062168364,20.4100965922228,-20.2953525503285));
#38525=CARTESIAN_POINT('Ctrl Pts',(-20.9553538829569,20.4864001534601,-20.2996327138962));
#38526=CARTESIAN_POINT('Ctrl Pts',(-20.9110477401698,20.5606318825454,-20.3039128774639));
#38527=CARTESIAN_POINT('Ctrl Pts',(-20.8631463404351,20.6323851909359,-20.3081930410317));
#38528=CARTESIAN_POINT('Ctrl Pts',(-20.8170263796525,20.7014700149142,-20.3123140265766));
#38529=CARTESIAN_POINT('Ctrl Pts',(-20.7675741880587,20.7682571483522,-20.3164350121215));
#38530=CARTESIAN_POINT('Ctrl Pts',(-20.7150628498031,20.832416043195,-20.3205559976664));
#38531=CARTESIAN_POINT('Ctrl Pts',(-20.6625158670912,20.8966184888021,-20.3246797805174));
#38532=CARTESIAN_POINT('Ctrl Pts',(-20.6069059263909,20.958188799342,-20.3288035633684));
#38533=CARTESIAN_POINT('Ctrl Pts',(-20.5485433933874,21.0168328476119,-20.3329273462195));
#38534=CARTESIAN_POINT('Ctrl Pts',(-20.4900913059675,21.0755668822695,-20.3370574568111));
#38535=CARTESIAN_POINT('Ctrl Pts',(-20.4288785557237,21.1313653881747,-20.3411875674027));
#38536=CARTESIAN_POINT('Ctrl Pts',(-20.3652483070037,21.1839746478091,-20.3453176779943));
#38537=CARTESIAN_POINT('Ctrl Pts',(-20.358074893939,21.1899055998009,-20.3457832897099));
#38538=CARTESIAN_POINT('Ctrl Pts',(-20.3508707850611,21.1957960645337,-20.3462489014256));
#38539=CARTESIAN_POINT('Ctrl Pts',(-20.3436364935458,21.2016457139947,-20.3467145131413));
#38540=CARTESIAN_POINT('Ctrl Pts',(-20.278618922688,21.2542189338493,-20.3508991582656));
#38541=CARTESIAN_POINT('Ctrl Pts',(-20.2109019654201,21.3037012778441,-20.3550838033898));
#38542=CARTESIAN_POINT('Ctrl Pts',(-20.1408117781385,21.3498035489242,-20.3592684485141));
#38543=CARTESIAN_POINT('Ctrl Pts',(-20.0708213570877,21.3958401981249,-20.363447137223));
#38544=CARTESIAN_POINT('Ctrl Pts',(-19.9984647969503,21.4385060803064,-20.3676258259318));
#38545=CARTESIAN_POINT('Ctrl Pts',(-19.9241011364255,21.4775522903915,-20.3718045146407));
#38546=CARTESIAN_POINT('Ctrl Pts',(-19.8484048007058,21.5172982497259,-20.3760580898566));
#38547=CARTESIAN_POINT('Ctrl Pts',(-19.770629090414,21.553293216013,-20.3803116650725));
#38548=CARTESIAN_POINT('Ctrl Pts',(-19.6911834656509,21.5853209161957,-20.3845652402884));
#38549=CARTESIAN_POINT('Ctrl Pts',(-19.6132778082299,21.6167277941183,-20.3887363645583));
#38550=CARTESIAN_POINT('Ctrl Pts',(-19.5337668439882,21.6443196560401,-20.3929074888282));
#38551=CARTESIAN_POINT('Ctrl Pts',(-19.4530597043387,21.6679397920169,-20.3970786130981));
#38552=CARTESIAN_POINT('Ctrl Pts',(-19.3723796494948,21.6915520012256,-20.4012483375651));
#38553=CARTESIAN_POINT('Ctrl Pts',(-19.2905046576304,21.7111950025156,-20.4054180620321));
#38554=CARTESIAN_POINT('Ctrl Pts',(-19.2078598569048,21.7267616810847,-20.409587786499));
#38555=CARTESIAN_POINT('Ctrl Pts',(-19.1252180001541,21.7423278051372,-20.413757362432));
#38556=CARTESIAN_POINT('Ctrl Pts',(-19.041806841303,21.7538178108621,-20.4179269383649));
#38557=CARTESIAN_POINT('Ctrl Pts',(-18.9580612092296,21.7611757928658,-20.4220965142979));
#38558=CARTESIAN_POINT('Ctrl Pts',(-18.8713716383372,21.7687924325249,-20.4264126647583));
#38559=CARTESIAN_POINT('Ctrl Pts',(-18.7843241655966,21.7719810786356,-20.4307288152187));
#38560=CARTESIAN_POINT('Ctrl Pts',(-18.6974043027305,21.7707384153349,-20.4350449656791));
#38561=CARTESIAN_POINT('Ctrl Pts',(-18.6133154147563,21.7695362255058,-20.4392205393694));
#38562=CARTESIAN_POINT('Ctrl Pts',(-18.5293464188554,21.7641870271194,-20.4433961130596));
#38563=CARTESIAN_POINT('Ctrl Pts',(-18.4459326767642,21.7547407920784,-20.4475716867499));
#38564=CARTESIAN_POINT('Ctrl Pts',(-18.3583065669894,21.7448175251453,-20.4519581255954));
#38565=CARTESIAN_POINT('Ctrl Pts',(-18.271293843584,21.7303726259075,-20.4563445644409));
#38566=CARTESIAN_POINT('Ctrl Pts',(-18.1853859711597,21.7115244744572,-20.4607310032864));
#38567=CARTESIAN_POINT('Ctrl Pts',(-18.0994780987354,21.6926763230069,-20.4651174421318));
#38568=CARTESIAN_POINT('Ctrl Pts',(-18.0146756167236,21.6694251461087,-20.4695038809773));
#38569=CARTESIAN_POINT('Ctrl Pts',(-17.9314482086413,21.6419485025781,-20.4738903198228));
#38570=CARTESIAN_POINT('Ctrl Pts',(-17.8520649990632,21.6157409802949,-20.4780741530359));
#38571=CARTESIAN_POINT('Ctrl Pts',(-17.7738191779357,21.5855921988556,-20.4822579862489));
#38572=CARTESIAN_POINT('Ctrl Pts',(-17.6971302094549,21.5516197977149,-20.486441819462));
#38573=CARTESIAN_POINT('Ctrl Pts',(-17.6205369358846,21.5176897884064,-20.4906204319562));
#38574=CARTESIAN_POINT('Ctrl Pts',(-17.545497076438,21.4799458123768,-20.4947990444504));
#38575=CARTESIAN_POINT('Ctrl Pts',(-17.4724142389696,21.4385550200984,-20.4989776569446));
#38576=CARTESIAN_POINT('Ctrl Pts',(-17.3994143840766,21.397211225373,-20.503151524795));
#38577=CARTESIAN_POINT('Ctrl Pts',(-17.3283675330366,21.3522290693436,-20.5073253926455));
#38578=CARTESIAN_POINT('Ctrl Pts',(-17.2596551457062,21.3038227948437,-20.511499260496));
#38579=CARTESIAN_POINT('Ctrl Pts',(-17.2308389678685,21.2835224695509,-20.5132496714906));
#38580=CARTESIAN_POINT('Ctrl Pts',(-17.2024330747213,21.2626204897635,-20.5150000824852));
#38581=CARTESIAN_POINT('Ctrl Pts',(-17.1744642439897,21.2411350264762,-20.5167504934799));
#38582=CARTESIAN_POINT('',(-21.2937660450662,19.2120076676442,-20.1667099326));
#38583=CARTESIAN_POINT('Ctrl Pts',(-21.2901594272135,19.212019439545,-20.166710586346));
#38584=CARTESIAN_POINT('Ctrl Pts',(-21.2914431884923,19.5768333887026,-20.1847914783466));
#38585=CARTESIAN_POINT('Ctrl Pts',(-21.0477248310816,20.7953392166858,-20.2452643059079));
#38586=CARTESIAN_POINT('Ctrl Pts',(-19.3278236771125,22.0902445830675,-20.3396938341447));
#38587=CARTESIAN_POINT('Ctrl Pts',(-17.7189176159228,21.6517991779038,-20.4160424703808));
#38588=CARTESIAN_POINT('Ctrl Pts',(-17.1739275520481,21.2418454004355,-20.4499991710565));
#38589=CARTESIAN_POINT('Ctrl Pts',(-17.1744642439897,21.2411350264762,-19.6501081077317));
#38590=CARTESIAN_POINT('Ctrl Pts',(-17.1077738078371,21.1899038923853,-19.6542777748744));
#38591=CARTESIAN_POINT('Ctrl Pts',(-17.0436134208209,21.135385404573,-19.6584474420171));
#38592=CARTESIAN_POINT('Ctrl Pts',(-16.9823135556347,21.0778675905449,-19.6626171091599));
#38593=CARTESIAN_POINT('Ctrl Pts',(-16.9209517695699,21.0202916760043,-19.6667909882116));
#38594=CARTESIAN_POINT('Ctrl Pts',(-16.8624566135658,20.9597106987123,-19.6709648672633));
#38595=CARTESIAN_POINT('Ctrl Pts',(-16.8071223925888,20.8964502917788,-19.675138746315));
#38596=CARTESIAN_POINT('Ctrl Pts',(-16.7517612063089,20.8331590569777,-19.6793146593687));
#38597=CARTESIAN_POINT('Ctrl Pts',(-16.6995643093342,20.7671861526635,-19.6834905724224));
#38598=CARTESIAN_POINT('Ctrl Pts',(-16.6507847507581,20.6988891844912,-19.687666485476));
#38599=CARTESIAN_POINT('Ctrl Pts',(-16.6019172419757,20.6304690759582,-19.6918499277576));
#38600=CARTESIAN_POINT('Ctrl Pts',(-16.5564796329369,20.5597169183466,-19.6960333700392));
#38601=CARTESIAN_POINT('Ctrl Pts',(-16.5146807414217,20.4870180361199,-19.7002168123208));
#38602=CARTESIAN_POINT('Ctrl Pts',(-16.4746040644093,20.4173145220662,-19.7042278867546));
#38603=CARTESIAN_POINT('Ctrl Pts',(-16.4378722674183,20.3458218948274,-19.7082389611885));
#38604=CARTESIAN_POINT('Ctrl Pts',(-16.4046276535517,20.2728966388503,-19.7122500356223));
#38605=CARTESIAN_POINT('Ctrl Pts',(-16.3699445411192,20.1968158980013,-19.7164346697445));
#38606=CARTESIAN_POINT('Ctrl Pts',(-16.3389281684758,20.1188925846309,-19.7206193038666));
#38607=CARTESIAN_POINT('Ctrl Pts',(-16.3117771822155,20.0395147077776,-19.7248039379887));
#38608=CARTESIAN_POINT('Ctrl Pts',(-16.2846648420244,19.9602498155099,-19.728982615802));
#38609=CARTESIAN_POINT('Ctrl Pts',(-16.2614071073244,19.879534903759,-19.7331612936152));
#38610=CARTESIAN_POINT('Ctrl Pts',(-16.2421554012761,19.797779767724,-19.7373399714285));
#38611=CARTESIAN_POINT('Ctrl Pts',(-16.2225586206514,19.7145592229166,-19.7415935493816));
#38612=CARTESIAN_POINT('Ctrl Pts',(-16.2071130980707,19.6302612335116,-19.7458471273348));
#38613=CARTESIAN_POINT('Ctrl Pts',(-16.1959260745095,19.5453362809288,-19.7501007052879));
#38614=CARTESIAN_POINT('Ctrl Pts',(-16.1849559341096,19.4620577709489,-19.7542718189977));
#38615=CARTESIAN_POINT('Ctrl Pts',(-16.1780807097821,19.3781768678582,-19.7584429327075));
#38616=CARTESIAN_POINT('Ctrl Pts',(-16.175350045093,19.294128865351,-19.7626140464172));
#38617=CARTESIAN_POINT('Ctrl Pts',(-16.172620296704,19.2101090659343,-19.766783760471));
#38618=CARTESIAN_POINT('Ctrl Pts',(-16.1740323608365,19.1259227378681,-19.7709534745247));
#38619=CARTESIAN_POINT('Ctrl Pts',(-16.1795838629489,19.0420082878574,-19.7751231885784));
#38620=CARTESIAN_POINT('Ctrl Pts',(-16.1851351675175,18.9580968238458,-19.7792927542576));
#38621=CARTESIAN_POINT('Ctrl Pts',(-16.1948255859832,18.8744576776277,-19.7834623199368));
#38622=CARTESIAN_POINT('Ctrl Pts',(-16.2086007338245,18.7915258692122,-19.787631885616));
#38623=CARTESIAN_POINT('Ctrl Pts',(-16.2228602008279,18.7056782689351,-19.7919480486733));
#38624=CARTESIAN_POINT('Ctrl Pts',(-16.2414968944959,18.6205891924187,-19.7962642117307));
#38625=CARTESIAN_POINT('Ctrl Pts',(-16.2643928538834,18.536729621109,-19.800580374788));
#38626=CARTESIAN_POINT('Ctrl Pts',(-16.2865429768018,18.4556017775032,-19.8047559387221));
#38627=CARTESIAN_POINT('Ctrl Pts',(-16.312678943375,18.3756249997159,-19.8089315026562));
#38628=CARTESIAN_POINT('Ctrl Pts',(-16.3426437089087,18.2972083995474,-19.8131070665903));
#38629=CARTESIAN_POINT('Ctrl Pts',(-16.3741219298082,18.2148311468531,-19.8174935292092));
#38630=CARTESIAN_POINT('Ctrl Pts',(-16.4098256651864,18.1341763575637,-19.8218799918281));
#38631=CARTESIAN_POINT('Ctrl Pts',(-16.4495176195312,18.0556904080171,-19.826266454447));
#38632=CARTESIAN_POINT('Ctrl Pts',(-16.4892095738761,17.9772044584704,-19.830652917066));
#38633=CARTESIAN_POINT('Ctrl Pts',(-16.5328893929524,17.9008878144519,-19.8350393796849));
#38634=CARTESIAN_POINT('Ctrl Pts',(-16.5802679097329,17.8271509896836,-19.8394258423038));
#38635=CARTESIAN_POINT('Ctrl Pts',(-16.6254664649228,17.7568069145566,-19.8436104767382));
#38636=CARTESIAN_POINT('Ctrl Pts',(-16.674199069114,17.6885486380897,-19.8477951111725));
#38637=CARTESIAN_POINT('Ctrl Pts',(-16.7262469917063,17.6227532125997,-19.8519797456069));
#38638=CARTESIAN_POINT('Ctrl Pts',(-16.778220830493,17.557051438792,-19.8561584237297));
#38639=CARTESIAN_POINT('Ctrl Pts',(-16.8335003313992,17.493805910514,-19.8603371018525));
#38640=CARTESIAN_POINT('Ctrl Pts',(-16.8918228839634,17.4333657650824,-19.8645157799753));
#38641=CARTESIAN_POINT('Ctrl Pts',(-16.9511908256749,17.3718422741984,-19.8687693578507));
#38642=CARTESIAN_POINT('Ctrl Pts',(-17.0137117247822,17.3132261339235,-19.8730229357261));
#38643=CARTESIAN_POINT('Ctrl Pts',(-17.0790648452608,17.2578513539394,-19.8772765136015));
#38644=CARTESIAN_POINT('Ctrl Pts',(-17.143150968624,17.2035501215685,-19.881447627612));
#38645=CARTESIAN_POINT('Ctrl Pts',(-17.209960109974,17.1523660019996,-19.8856187416225));
#38646=CARTESIAN_POINT('Ctrl Pts',(-17.27915312729,17.1045763538723,-19.8897898556331));
#38647=CARTESIAN_POINT('Ctrl Pts',(-17.3483229261813,17.0568027420502,-19.8939595699836));
#38648=CARTESIAN_POINT('Ctrl Pts',(-17.419874634147,17.0124216007179,-19.8981292843341));
#38649=CARTESIAN_POINT('Ctrl Pts',(-17.4934383352004,16.971668234533,-19.9022989986847));
#38650=CARTESIAN_POINT('Ctrl Pts',(-17.5669994184993,16.9309163185512,-19.9064685646565));
#38651=CARTESIAN_POINT('Ctrl Pts',(-17.642571949712,16.8937921432288,-19.9106381306283));
#38652=CARTESIAN_POINT('Ctrl Pts',(-17.7197607085089,16.8604854479081,-19.9148076966001));
#38653=CARTESIAN_POINT('Ctrl Pts',(-17.7996633275671,16.8260077308186,-19.9191238592988));
#38654=CARTESIAN_POINT('Ctrl Pts',(-17.8812974576374,16.7956211424297,-19.9234400219976));
#38655=CARTESIAN_POINT('Ctrl Pts',(-17.964203228004,16.7694814295557,-19.9277561846964));
#38656=CARTESIAN_POINT('Ctrl Pts',(-18.0444083527806,16.7441932147135,-19.9319317489096));
#38657=CARTESIAN_POINT('Ctrl Pts',(-18.1258030751548,16.7228795141883,-19.9361073131228));
#38658=CARTESIAN_POINT('Ctrl Pts',(-18.2079583914907,16.7056297227522,-19.940282877336));
#38659=CARTESIAN_POINT('Ctrl Pts',(-18.2942631757073,16.6875086857447,-19.9446693392775));
#38660=CARTESIAN_POINT('Ctrl Pts',(-18.3814068314547,16.6738729730813,-19.949055801219));
#38661=CARTESIAN_POINT('Ctrl Pts',(-18.4688855835906,16.6647646718711,-19.9534422631606));
#38662=CARTESIAN_POINT('Ctrl Pts',(-18.5563643357266,16.6556563706608,-19.9578287251021));
#38663=CARTESIAN_POINT('Ctrl Pts',(-18.6441776008593,16.6510754351691,-19.9622151870437));
#38664=CARTESIAN_POINT('Ctrl Pts',(-18.7318236815484,16.6510009250709,-19.9666016489852));
#38665=CARTESIAN_POINT('Ctrl Pts',(-18.8154370558739,16.6509298432759,-19.970786284298));
#38666=CARTESIAN_POINT('Ctrl Pts',(-18.8992095168454,16.6549593424997,-19.9749709196109));
#38667=CARTESIAN_POINT('Ctrl Pts',(-18.9827056282395,16.6631095960615,-19.9791555549237));
#38668=CARTESIAN_POINT('Ctrl Pts',(-19.0660828933656,16.6712482487571,-19.9833342339317));
#38669=CARTESIAN_POINT('Ctrl Pts',(-19.1491841362886,16.6834959609935,-19.9875129129397));
#38670=CARTESIAN_POINT('Ctrl Pts',(-19.2315736415642,16.6998209002103,-19.9916915919477));
#38671=CARTESIAN_POINT('Ctrl Pts',(-19.315439896419,16.7164384476548,-19.9959451696027));
#38672=CARTESIAN_POINT('Ctrl Pts',(-19.3985681651274,16.7372808264551,-20.0001987472577));
#38673=CARTESIAN_POINT('Ctrl Pts',(-19.4805039902948,16.7622591414211,-20.0044523249126));
#38674=CARTESIAN_POINT('Ctrl Pts',(-19.5608513518337,16.7867532097862,-20.0086234398184));
#38675=CARTESIAN_POINT('Ctrl Pts',(-19.6400516319828,16.8152241408902,-20.0127945547243));
#38676=CARTESIAN_POINT('Ctrl Pts',(-19.7176880447478,16.8475368988241,-20.0169656696301));
#38677=CARTESIAN_POINT('Ctrl Pts',(-19.7952984058594,16.8798388138978,-20.0211353848777));
#38678=CARTESIAN_POINT('Ctrl Pts',(-19.8713455174287,16.9159798188825,-20.0253051001254));
#38679=CARTESIAN_POINT('Ctrl Pts',(-19.9454312968482,16.9557762388143,-20.029474815373));
#38680=CARTESIAN_POINT('Ctrl Pts',(-20.019514439946,16.9955712426016,-20.0336443822425));
#38681=CARTESIAN_POINT('Ctrl Pts',(-20.0916359848004,17.0390211842643,-20.037813949112));
#38682=CARTESIAN_POINT('Ctrl Pts',(-20.1614224652661,17.0858964482516,-20.0419835159815));
#38683=CARTESIAN_POINT('Ctrl Pts',(-20.2336625178745,17.1344197655744,-20.0462996776219));
#38684=CARTESIAN_POINT('Ctrl Pts',(-20.3033998138015,17.1866134578917,-20.0506158392624));
#38685=CARTESIAN_POINT('Ctrl Pts',(-20.3702544757157,17.2421751498165,-20.0549320009028));
#38686=CARTESIAN_POINT('Ctrl Pts',(-20.4349313846296,17.295926950885,-20.059107566006));
#38687=CARTESIAN_POINT('Ctrl Pts',(-20.4969102614713,17.3528303456931,-20.0632831311092));
#38688=CARTESIAN_POINT('Ctrl Pts',(-20.5558837277198,17.4125729976811,-20.0674586962124));
#38689=CARTESIAN_POINT('Ctrl Pts',(-20.6178357603196,17.4753330651997,-20.0718451561215));
#38690=CARTESIAN_POINT('Ctrl Pts',(-20.6764704133144,17.5412263089033,-20.0762316160305));
#38691=CARTESIAN_POINT('Ctrl Pts',(-20.731479614623,17.6098519152915,-20.0806180759395));
#38692=CARTESIAN_POINT('Ctrl Pts',(-20.7864888159315,17.6784775216797,-20.0850045358486));
#38693=CARTESIAN_POINT('Ctrl Pts',(-20.8378722882313,17.7498349754592,-20.0893909957576));
#38694=CARTESIAN_POINT('Ctrl Pts',(-20.8853760800034,17.8234910946631,-20.0937774556667));
#38695=CARTESIAN_POINT('Ctrl Pts',(-20.9317208338504,17.8953500892083,-20.0980568909951));
#38696=CARTESIAN_POINT('Ctrl Pts',(-20.9745398785638,17.9696546343097,-20.1023363263235));
#38697=CARTESIAN_POINT('Ctrl Pts',(-21.0135728623478,18.0460332342734,-20.106615761652));
#38698=CARTESIAN_POINT('Ctrl Pts',(-21.0525424990579,18.1222878785374,-20.1108882518361));
#38699=CARTESIAN_POINT('Ctrl Pts',(-21.0877380947942,18.2006095044151,-20.1151607420202));
#38700=CARTESIAN_POINT('Ctrl Pts',(-21.118942960611,18.2805984336684,-20.1194332322043));
#38701=CARTESIAN_POINT('Ctrl Pts',(-21.1500944339135,18.3604504993293,-20.1236984120223));
#38702=CARTESIAN_POINT('Ctrl Pts',(-21.1772686129624,18.4419637894576,-20.1279635918403));
#38703=CARTESIAN_POINT('Ctrl Pts',(-21.2002957124611,18.5247161966825,-20.1322287716583));
#38704=CARTESIAN_POINT('Ctrl Pts',(-21.2232995986398,18.6073851822802,-20.136489651804));
#38705=CARTESIAN_POINT('Ctrl Pts',(-21.2421646000029,18.6912903874225,-20.1407505319496));
#38706=CARTESIAN_POINT('Ctrl Pts',(-21.2567699771926,18.7759923653821,-20.1450114120952));
#38707=CARTESIAN_POINT('Ctrl Pts',(-21.271362764314,18.8606213288853,-20.1492686192942));
#38708=CARTESIAN_POINT('Ctrl Pts',(-21.2817031594057,18.9460452737795,-20.1535258264931));
#38709=CARTESIAN_POINT('Ctrl Pts',(-21.2877212408942,19.0318134385456,-20.1577830336921));
#38710=CARTESIAN_POINT('Ctrl Pts',(-21.2919276409715,19.0917619812152,-20.1607586525376));
#38711=CARTESIAN_POINT('Ctrl Pts',(-21.2940234518455,19.1518784236118,-20.163734271383));
#38712=CARTESIAN_POINT('Ctrl Pts',(-21.293999801981,19.2120069046681,-20.1667098902285));
#38713=CARTESIAN_POINT('Origin',(-18.734,19.211,1.76670989022852));
#38714=CARTESIAN_POINT('',(-17.1744642439897,21.2411350264762,-18.8501886329194));
#38715=CARTESIAN_POINT('',(-17.1746506311395,21.2408837946619,-18.9165758925774));
#38716=CARTESIAN_POINT('',(-17.1744642439897,21.2411350264762,1.76670989022852));
#38717=CARTESIAN_POINT('',(-21.2939990581246,19.2131959965571,-19.4332901097715));
#38718=CARTESIAN_POINT('Ctrl Pts',(-17.1746506311398,21.2408837946621,-18.9165758925774));
#38719=CARTESIAN_POINT('Ctrl Pts',(-17.0075187104224,21.1151430662609,-18.9269774749334));
#38720=CARTESIAN_POINT('Ctrl Pts',(-16.2393386951681,20.375997631509,-18.97977099285));
#38721=CARTESIAN_POINT('Ctrl Pts',(-15.8675519521013,18.2379802926624,-19.074956446327));
#38722=CARTESIAN_POINT('Ctrl Pts',(-18.0006016326409,16.274093700693,-19.2021322530085));
#38723=CARTESIAN_POINT('Ctrl Pts',(-20.635918474416,16.9602241188658,-19.3215765970806));
#38724=CARTESIAN_POINT('Ctrl Pts',(-21.2889869220882,18.5174131978834,-19.3986290055925));
#38725=CARTESIAN_POINT('Ctrl Pts',(-21.2953149015357,19.2131844541912,-19.4332894785437));
#38726=CARTESIAN_POINT('Ctrl Pts',(-21.2939990581246,19.2131959965571,-19.4332901097715));
#38727=CARTESIAN_POINT('Ctrl Pts',(-21.293890587382,19.3396465586196,-19.4395926510263));
#38728=CARTESIAN_POINT('Ctrl Pts',(-21.2844099378551,19.465708927393,-19.4458951922812));
#38729=CARTESIAN_POINT('Ctrl Pts',(-21.2657470116552,19.5902849443033,-19.452197733536));
#38730=CARTESIAN_POINT('Ctrl Pts',(-21.2615163488398,19.618524841776,-19.4536264444811));
#38731=CARTESIAN_POINT('Ctrl Pts',(-21.2568139996567,19.6466884925667,-19.4550551554262));
#38732=CARTESIAN_POINT('Ctrl Pts',(-21.2516424693627,19.6747632978808,-19.4564838663713));
#38733=CARTESIAN_POINT('Ctrl Pts',(-21.2364952751686,19.7569932189831,-19.4606685004935));
#38734=CARTESIAN_POINT('Ctrl Pts',(-21.2172870302474,19.8386332916553,-19.4648531346158));
#38735=CARTESIAN_POINT('Ctrl Pts',(-21.1940771445785,19.9192516803528,-19.469037768738));
#38736=CARTESIAN_POINT('Ctrl Pts',(-21.1709002953099,19.9997553187496,-19.4732164465514));
#38737=CARTESIAN_POINT('Ctrl Pts',(-21.1437332452095,20.0792397234556,-19.4773951243647));
#38738=CARTESIAN_POINT('Ctrl Pts',(-21.1126865924437,20.1572822490824,-19.4815738021781));
#38739=CARTESIAN_POINT('Ctrl Pts',(-21.0810834481907,20.2367236373009,-19.4858273801312));
#38740=CARTESIAN_POINT('Ctrl Pts',(-21.0454603361894,20.3146704722382,-19.4900809580843));
#38741=CARTESIAN_POINT('Ctrl Pts',(-21.0059873753743,20.3906920641166,-19.4943345360374));
#38742=CARTESIAN_POINT('Ctrl Pts',(-20.9672796780334,20.4652398231152,-19.4985056497473));
#38743=CARTESIAN_POINT('Ctrl Pts',(-20.9248702957982,20.5379358953033,-19.5026767634572));
#38744=CARTESIAN_POINT('Ctrl Pts',(-20.8789678616489,20.6083950309391,-19.506847877167));
#38745=CARTESIAN_POINT('Ctrl Pts',(-20.8330808304891,20.6788305233554,-19.5110175912208));
#38746=CARTESIAN_POINT('Ctrl Pts',(-20.7837033261796,20.7470301848417,-19.5151873052746));
#38747=CARTESIAN_POINT('Ctrl Pts',(-20.7310884045781,20.8126360086797,-19.5193570193284));
#38748=CARTESIAN_POINT('Ctrl Pts',(-20.6784753552182,20.8782394980099,-19.5235265850078));
#38749=CARTESIAN_POINT('Ctrl Pts',(-20.6226254060923,20.9412489748611,-19.5276961506871));
#38750=CARTESIAN_POINT('Ctrl Pts',(-20.5638323063888,21.0013389987641,-19.5318657163664));
#38751=CARTESIAN_POINT('Ctrl Pts',(-20.502972105477,21.0635417223146,-19.5361818794236));
#38752=CARTESIAN_POINT('Ctrl Pts',(-20.4389583088965,21.122615499409,-19.5404980424808));
#38753=CARTESIAN_POINT('Ctrl Pts',(-20.3721573780251,21.1782418267264,-19.544814205538));
#38754=CARTESIAN_POINT('Ctrl Pts',(-20.3075324892011,21.2320561249956,-19.5489897694722));
#38755=CARTESIAN_POINT('Ctrl Pts',(-20.2402996648593,21.2826438810762,-19.5531653334064));
#38756=CARTESIAN_POINT('Ctrl Pts',(-20.1708219662268,21.329759693162,-19.5573408973406));
#38757=CARTESIAN_POINT('Ctrl Pts',(-20.0978350996175,21.3792552228008,-19.5617273599593));
#38758=CARTESIAN_POINT('Ctrl Pts',(-20.0223711202591,21.4249185513468,-19.566113822578));
#38759=CARTESIAN_POINT('Ctrl Pts',(-19.9448802161397,21.4665196966911,-19.5705002851967));
#38760=CARTESIAN_POINT('Ctrl Pts',(-19.8673893120203,21.5081208420354,-19.5748867478154));
#38761=CARTESIAN_POINT('Ctrl Pts',(-19.7878720403016,21.5456596252664,-19.579273210434));
#38762=CARTESIAN_POINT('Ctrl Pts',(-19.7068005673304,21.5789651720837,-19.5836596730527));
#38763=CARTESIAN_POINT('Ctrl Pts',(-19.629459322931,21.6107382772446,-19.5878443074871));
#38764=CARTESIAN_POINT('Ctrl Pts',(-19.5504158778411,21.6387774071505,-19.5920289419215));
#38765=CARTESIAN_POINT('Ctrl Pts',(-19.4700654949587,21.6628987717953,-19.5962135763559));
#38766=CARTESIAN_POINT('Ctrl Pts',(-19.3898294809474,21.6869858026491,-19.6003922544787));
#38767=CARTESIAN_POINT('Ctrl Pts',(-19.3082906610537,21.7071660136986,-19.6045709326015));
#38768=CARTESIAN_POINT('Ctrl Pts',(-19.2258642779018,21.7233036305598,-19.6087496107243));
#38769=CARTESIAN_POINT('Ctrl Pts',(-19.1419604620487,21.7397305024139,-19.6130031885997));
#38770=CARTESIAN_POINT('Ctrl Pts',(-19.0571373968166,21.7519682444677,-19.6172567664751));
#38771=CARTESIAN_POINT('Ctrl Pts',(-18.9718493062277,21.7599267756307,-19.6215103443505));
#38772=CARTESIAN_POINT('Ctrl Pts',(-18.8882146908505,21.7677310152166,-19.6256814583611));
#38773=CARTESIAN_POINT('Ctrl Pts',(-18.8041333991885,21.7714204401683,-19.6298525723716));
#38774=CARTESIAN_POINT('Ctrl Pts',(-18.7200422944287,21.7709619494155,-19.6340236863821));
#38775=CARTESIAN_POINT('Ctrl Pts',(-18.6359794072993,21.7705036125139,-19.6381934007327));
#38776=CARTESIAN_POINT('Ctrl Pts',(-18.551907173255,21.7659001267009,-19.6423631150832));
#38777=CARTESIAN_POINT('Ctrl Pts',(-18.4682635936743,21.7571704896477,-19.6465328294338));
#38778=CARTESIAN_POINT('Ctrl Pts',(-18.3846229905396,21.7484411632376,-19.6507023954056));
#38779=CARTESIAN_POINT('Ctrl Pts',(-18.3014114689995,21.7355860261208,-19.6548719613774));
#38780=CARTESIAN_POINT('Ctrl Pts',(-18.2190616739018,21.7186759201131,-19.6590415273492));
#38781=CARTESIAN_POINT('Ctrl Pts',(-18.1338165629591,21.7011712759185,-19.663357690048));
#38782=CARTESIAN_POINT('Ctrl Pts',(-18.0494954191338,21.679321318249,-19.6676738527467));
#38783=CARTESIAN_POINT('Ctrl Pts',(-17.966564411757,21.6532617832448,-19.6719900154455));
#38784=CARTESIAN_POINT('Ctrl Pts',(-17.8863348720621,21.6280511344877,-19.6761655796587));
#38785=CARTESIAN_POINT('Ctrl Pts',(-17.8074067178008,21.5989011580654,-19.6803411438719));
#38786=CARTESIAN_POINT('Ctrl Pts',(-17.7301828112741,21.5659842996543,-19.6845167080851));
#38787=CARTESIAN_POINT('Ctrl Pts',(-17.6490585105433,21.5314048897156,-19.6889031700266));
#38788=CARTESIAN_POINT('Ctrl Pts',(-17.5698156696645,21.4926683234483,-19.6932896319682));
#38789=CARTESIAN_POINT('Ctrl Pts',(-17.492891345209,21.4500286525641,-19.6976760939097));
#38790=CARTESIAN_POINT('Ctrl Pts',(-17.4159670207535,21.4073889816798,-19.7020625558512));
#38791=CARTESIAN_POINT('Ctrl Pts',(-17.341361664738,21.3608465778214,-19.7064490177927));
#38792=CARTESIAN_POINT('Ctrl Pts',(-17.2694745299336,21.3107059669218,-19.7108354797342));
#38793=CARTESIAN_POINT('Ctrl Pts',(-17.2373037292364,21.2882671313154,-19.7127985012577));
#38794=CARTESIAN_POINT('Ctrl Pts',(-17.2056207285748,21.2650692235164,-19.7147615227813));
#38795=CARTESIAN_POINT('Ctrl Pts',(-17.1744642439897,21.2411350264762,-19.7167245443048));
#38796=CARTESIAN_POINT('',(-21.2939989850552,19.2087204131754,-19.3667098901939));
#38797=CARTESIAN_POINT('Ctrl Pts',(-21.2939989850559,19.2087204138716,-19.3667098902285));
#38798=CARTESIAN_POINT('Ctrl Pts',(-21.294073180434,19.292042596975,-19.3708480242597));
#38799=CARTESIAN_POINT('Ctrl Pts',(-21.2900751830218,19.3754486069202,-19.374986158291));
#38800=CARTESIAN_POINT('Ctrl Pts',(-21.2820071809338,19.4585063754929,-19.3791242923222));
#38801=CARTESIAN_POINT('Ctrl Pts',(-21.2739428344705,19.541526510458,-19.3832605513583));
#38802=CARTESIAN_POINT('Ctrl Pts',(-21.2618121886757,19.6241982519104,-19.3873968103944));
#38803=CARTESIAN_POINT('Ctrl Pts',(-21.2456694473256,19.7060925038528,-19.3915330694305));
#38804=CARTESIAN_POINT('Ctrl Pts',(-21.2295289836483,19.7879752008609,-19.3956687448579));
#38805=CARTESIAN_POINT('Ctrl Pts',(-21.2093776397595,19.8690801670299,-19.3998044202852));
#38806=CARTESIAN_POINT('Ctrl Pts',(-21.1853208566118,19.9489878440326,-19.4039400957126));
#38807=CARTESIAN_POINT('Ctrl Pts',(-21.1612599617805,20.0289091785175,-19.4080764779921));
#38808=CARTESIAN_POINT('Ctrl Pts',(-21.1332924395122,20.1076323699233,-19.4122128602716));
#38809=CARTESIAN_POINT('Ctrl Pts',(-21.1015733410929,20.1847538059213,-19.4163492425511));
#38810=CARTESIAN_POINT('Ctrl Pts',(-21.0698191717518,20.2619605129384,-19.420490198313));
#38811=CARTESIAN_POINT('Ctrl Pts',(-21.0343053289548,20.3375614976483,-19.4246311540749));
#38812=CARTESIAN_POINT('Ctrl Pts',(-20.9952344193577,20.4111745292715,-19.4287721098369));
#38813=CARTESIAN_POINT('Ctrl Pts',(-20.956138222721,20.4848352039023,-19.4329157456621));
#38814=CARTESIAN_POINT('Ctrl Pts',(-20.9134806196,20.5565049647657,-19.4370593814874));
#38815=CARTESIAN_POINT('Ctrl Pts',(-20.8675081508492,20.6258296612172,-19.4412030173127));
#38816=CARTESIAN_POINT('Ctrl Pts',(-20.8214607545843,20.6952673454484,-19.4453534065784));
#38817=CARTESIAN_POINT('Ctrl Pts',(-20.7720879921639,20.7623519651645,-19.4495037958442));
#38818=CARTESIAN_POINT('Ctrl Pts',(-20.7196769297106,20.8267620897939,-19.4536541851099));
#38819=CARTESIAN_POINT('Ctrl Pts',(-20.701811538935,20.8487176082006,-19.4550689308264));
#38820=CARTESIAN_POINT('Ctrl Pts',(-20.6835934338612,20.8703626873999,-19.456483676543));
#38821=CARTESIAN_POINT('Ctrl Pts',(-20.665034920053,20.8916856153177,-19.4578984222595));
#38822=CARTESIAN_POINT('Ctrl Pts',(-20.6101412425939,20.9547560712659,-19.4620830566462));
#38823=CARTESIAN_POINT('Ctrl Pts',(-20.5520521994161,21.0152517076034,-19.466267691033));
#38824=CARTESIAN_POINT('Ctrl Pts',(-20.4910387353968,21.0728310563301,-19.4704523254197));
#38825=CARTESIAN_POINT('Ctrl Pts',(-20.4301121164969,21.1303284479757,-19.474631003497));
#38826=CARTESIAN_POINT('Ctrl Pts',(-20.3662696766025,21.1849174841126,-19.4788096815743));
#38827=CARTESIAN_POINT('Ctrl Pts',(-20.2998217436364,21.2362906623878,-19.4829883596516));
#38828=CARTESIAN_POINT('Ctrl Pts',(-20.2321827790938,21.2885846680655,-19.4872419375387));
#38829=CARTESIAN_POINT('Ctrl Pts',(-20.161844312329,21.3375460297091,-19.4914955154257));
#38830=CARTESIAN_POINT('Ctrl Pts',(-20.0891719990913,21.3828906171534,-19.4957490933128));
#38831=CARTESIAN_POINT('Ctrl Pts',(-20.0179085806091,21.4273561111906,-19.4999202072832));
#38832=CARTESIAN_POINT('Ctrl Pts',(-19.9444014087256,21.4683435613089,-19.5040913212537));
#38833=CARTESIAN_POINT('Ctrl Pts',(-19.8690261614781,21.5056275542581,-19.5082624352241));
#38834=CARTESIAN_POINT('Ctrl Pts',(-19.793676207128,21.5428990362007,-19.5124321495367));
#38835=CARTESIAN_POINT('Ctrl Pts',(-19.7164598343519,21.5764693252628,-19.5166018638493));
#38836=CARTESIAN_POINT('Ctrl Pts',(-19.6377770918877,21.6061590694939,-19.5207715781619));
#38837=CARTESIAN_POINT('Ctrl Pts',(-19.5590971492983,21.6358477572345,-19.5249411440979));
#38838=CARTESIAN_POINT('Ctrl Pts',(-19.4789513714795,21.6616560130841,-19.5291107100339));
#38839=CARTESIAN_POINT('Ctrl Pts',(-19.3977582580605,21.6834532300645,-19.5332802759699));
#38840=CARTESIAN_POINT('Ctrl Pts',(-19.313710494605,21.706016810393,-19.5375964387175));
#38841=CARTESIAN_POINT('Ctrl Pts',(-19.2285408859855,21.7242819108903,-19.541912601465));
#38842=CARTESIAN_POINT('Ctrl Pts',(-19.1427269885521,21.7381609067942,-19.5462287642126));
#38843=CARTESIAN_POINT('Ctrl Pts',(-19.0597084701407,21.7515877958115,-19.5504043283956));
#38844=CARTESIAN_POINT('Ctrl Pts',(-18.9760874671013,21.7609099414407,-19.5545798925786));
#38845=CARTESIAN_POINT('Ctrl Pts',(-18.8923014001317,21.7661009112589,-19.5587554567616));
#38846=CARTESIAN_POINT('Ctrl Pts',(-18.8042834975712,21.7715540646552,-19.5631419187915));
#38847=CARTESIAN_POINT('Ctrl Pts',(-18.716084001952,21.7724477372194,-19.5675283808214));
#38848=CARTESIAN_POINT('Ctrl Pts',(-18.6282074804569,21.7688131172564,-19.5719148428513));
#38849=CARTESIAN_POINT('Ctrl Pts',(-18.5403309589617,21.7651784972933,-19.5763013048811));
#38850=CARTESIAN_POINT('Ctrl Pts',(-18.4527779822413,21.7570157144011,-19.580687766911));
#38851=CARTESIAN_POINT('Ctrl Pts',(-18.3660419494175,21.7444180217665,-19.5850742289409));
#38852=CARTESIAN_POINT('Ctrl Pts',(-18.2832980106589,21.7324001478343,-19.5892588006091));
#38853=CARTESIAN_POINT('Ctrl Pts',(-18.2009894838862,21.7163018984357,-19.5934433722773));
#38854=CARTESIAN_POINT('Ctrl Pts',(-18.1195501274672,21.6961662628775,-19.5976279439455));
#38855=CARTESIAN_POINT('Ctrl Pts',(-18.0344368609572,21.6751222641161,-19.6020012909277));
#38856=CARTESIAN_POINT('Ctrl Pts',(-17.9502735392786,21.6496679882501,-19.6063746379099));
#38857=CARTESIAN_POINT('Ctrl Pts',(-17.8675488737407,21.6199131254165,-19.610747984892));
#38858=CARTESIAN_POINT('Ctrl Pts',(-17.7886022149566,21.5915171568379,-19.6149216026359));
#38859=CARTESIAN_POINT('Ctrl Pts',(-17.7109661880779,21.5592049570797,-19.6190952203798));
#38860=CARTESIAN_POINT('Ctrl Pts',(-17.6350528734777,21.5231235289466,-19.6232688381237));
#38861=CARTESIAN_POINT('Ctrl Pts',(-17.5591911030165,21.4870665996271,-19.6274396220362));
#38862=CARTESIAN_POINT('Ctrl Pts',(-17.4850501355258,21.447245722735,-19.6316104059488));
#38863=CARTESIAN_POINT('Ctrl Pts',(-17.413022153431,21.4038560210087,-19.6357811898613));
#38864=CARTESIAN_POINT('Ctrl Pts',(-17.3410199038859,21.3604818205865,-19.6399504837292));
#38865=CARTESIAN_POINT('Ctrl Pts',(-17.2711295331142,21.3135415662574,-19.6441197775971));
#38866=CARTESIAN_POINT('Ctrl Pts',(-17.203717503422,21.2632756833981,-19.6482890714651));
#38867=CARTESIAN_POINT('Ctrl Pts',(-17.1939136908581,21.2559654555921,-19.6488954168873));
#38868=CARTESIAN_POINT('Ctrl Pts',(-17.1841622460799,21.2485849649405,-19.6495017623095));
#38869=CARTESIAN_POINT('Ctrl Pts',(-17.1744642439897,21.2411350264762,-19.6501081077317));
#38870=CARTESIAN_POINT('Ctrl Pts',(-17.1744642439897,21.2411350264762,-18.8501886329194));
#38871=CARTESIAN_POINT('Ctrl Pts',(-17.1079120298185,21.1900100735602,-18.8543616881065));
#38872=CARTESIAN_POINT('Ctrl Pts',(-17.0438081666524,21.1355566463855,-18.8585347432936));
#38873=CARTESIAN_POINT('Ctrl Pts',(-16.9824993407833,21.0780418958244,-18.8627077984807));
#38874=CARTESIAN_POINT('Ctrl Pts',(-16.9212253091811,21.020559786299,-18.8668784853563));
#38875=CARTESIAN_POINT('Ctrl Pts',(-16.8627435002704,20.9600201168211,-18.8710491722319));
#38876=CARTESIAN_POINT('Ctrl Pts',(-16.8073668119571,20.8967296813936,-18.8752198591075));
#38877=CARTESIAN_POINT('Ctrl Pts',(-16.7520049394097,20.833456179017,-18.879389430136));
#38878=CARTESIAN_POINT('Ctrl Pts',(-16.6997468400686,20.7674337185571,-18.8835590011644));
#38879=CARTESIAN_POINT('Ctrl Pts',(-16.6508669315501,20.6990042402932,-18.8877285721929));
#38880=CARTESIAN_POINT('Ctrl Pts',(-16.6019854379048,20.6305725429294,-18.8918982784364));
#38881=CARTESIAN_POINT('Ctrl Pts',(-16.5564826189569,20.559734047872,-18.8960679846799));
#38882=CARTESIAN_POINT('Ctrl Pts',(-16.5145903334575,20.4868607808291,-18.9002376909234));
#38883=CARTESIAN_POINT('Ctrl Pts',(-16.4726553116461,20.4139131723019,-18.9044116508825));
#38884=CARTESIAN_POINT('Ctrl Pts',(-16.4343384099249,20.3389270454576,-18.9085856108416));
#38885=CARTESIAN_POINT('Ctrl Pts',(-16.3998258981524,20.262299796568,-18.9127595708007));
#38886=CARTESIAN_POINT('Ctrl Pts',(-16.3652960666188,20.185634093055,-18.9169356254201));
#38887=CARTESIAN_POINT('Ctrl Pts',(-16.3345745959917,20.1073260557597,-18.9211116800395));
#38888=CARTESIAN_POINT('Ctrl Pts',(-16.3077989545311,20.0277915811058,-18.9252877346589));
#38889=CARTESIAN_POINT('Ctrl Pts',(-16.2809755043854,19.9481150953389,-18.9294712457451));
#38890=CARTESIAN_POINT('Ctrl Pts',(-16.2581120855318,19.8672082404936,-18.9336547568312));
#38891=CARTESIAN_POINT('Ctrl Pts',(-16.239295758604,19.7855004333862,-18.9378382679174));
#38892=CARTESIAN_POINT('Ctrl Pts',(-16.2222689392233,19.7115633637894,-18.9416239104561));
#38893=CARTESIAN_POINT('Ctrl Pts',(-16.2085553993355,19.6369708281993,-18.9454095529949));
#38894=CARTESIAN_POINT('Ctrl Pts',(-16.1981829862585,19.5620442604845,-18.9491951955337));
#38895=CARTESIAN_POINT('Ctrl Pts',(-16.1867173615958,19.4792207269146,-18.9533798299225));
#38896=CARTESIAN_POINT('Ctrl Pts',(-16.1792923755172,19.3956807451282,-18.9575644643113));
#38897=CARTESIAN_POINT('Ctrl Pts',(-16.1759873564286,19.3118529391175,-18.9617490987001));
#38898=CARTESIAN_POINT('Ctrl Pts',(-16.1726870416255,19.2281444516126,-18.9659277767798));
#38899=CARTESIAN_POINT('Ctrl Pts',(-16.173495063509,19.1441494093852,-18.9701064548596));
#38900=CARTESIAN_POINT('Ctrl Pts',(-16.1784392678899,19.0603038006558,-18.9742851329393));
#38901=CARTESIAN_POINT('Ctrl Pts',(-16.1834720935873,18.9749553195411,-18.9785387108258));
#38902=CARTESIAN_POINT('Ctrl Pts',(-16.1927909085457,18.8897621593934,-18.9827922887123));
#38903=CARTESIAN_POINT('Ctrl Pts',(-16.2063695825696,18.8051866526586,-18.9870458665988));
#38904=CARTESIAN_POINT('Ctrl Pts',(-16.2196850074843,18.7222508072609,-18.9912169805725));
#38905=CARTESIAN_POINT('Ctrl Pts',(-16.2370965177706,18.6399093552907,-18.9953880945463));
#38906=CARTESIAN_POINT('Ctrl Pts',(-16.2585271389987,18.5585935971759,-18.9995592085201));
#38907=CARTESIAN_POINT('Ctrl Pts',(-16.279950568975,18.4773051253486,-19.0037289228363));
#38908=CARTESIAN_POINT('Ctrl Pts',(-16.3053903143098,18.3970421083,-19.0078986371526));
#38909=CARTESIAN_POINT('Ctrl Pts',(-16.3347186663499,18.3182239463347,-19.0120683514688));
#38910=CARTESIAN_POINT('Ctrl Pts',(-16.3640459747616,18.2394085890572,-19.0162379174088));
#38911=CARTESIAN_POINT('Ctrl Pts',(-16.3972614535261,18.1620384154931,-19.0204074833487));
#38912=CARTESIAN_POINT('Ctrl Pts',(-16.4341885271975,18.0865147001558,-19.0245770492886));
#38913=CARTESIAN_POINT('Ctrl Pts',(-16.4724139113061,18.0083356639891,-19.0288932120325));
#38914=CARTESIAN_POINT('Ctrl Pts',(-16.5146165141609,17.9321358186698,-19.0332093747764));
#38915=CARTESIAN_POINT('Ctrl Pts',(-16.5605485527344,17.8583327066942,-19.0375255375203));
#38916=CARTESIAN_POINT('Ctrl Pts',(-16.6049843598894,17.7869337234784,-19.041701101708));
#38917=CARTESIAN_POINT('Ctrl Pts',(-16.6529100541822,17.7177780846058,-19.0458766658957));
#38918=CARTESIAN_POINT('Ctrl Pts',(-16.7040581042278,17.651212867155,-19.0500522300834));
#38919=CARTESIAN_POINT('Ctrl Pts',(-16.7577895208549,17.5812855985979,-19.0544386921054));
#38920=CARTESIAN_POINT('Ctrl Pts',(-16.8150769912951,17.5142177570115,-19.0588251541273));
#38921=CARTESIAN_POINT('Ctrl Pts',(-16.8755654265148,17.4503691653061,-19.0632116161493));
#38922=CARTESIAN_POINT('Ctrl Pts',(-16.9360538617345,17.3865205736007,-19.0675980781712));
#38923=CARTESIAN_POINT('Ctrl Pts',(-16.9997427890408,17.3258915767388,-19.0719845401932));
#38924=CARTESIAN_POINT('Ctrl Pts',(-17.0662376770542,17.2687927931957,-19.0763710022152));
#38925=CARTESIAN_POINT('Ctrl Pts',(-17.1296730365262,17.2143212094742,-19.0805556366057));
#38926=CARTESIAN_POINT('Ctrl Pts',(-17.1958979365981,17.1628593635266,-19.0847402709962));
#38927=CARTESIAN_POINT('Ctrl Pts',(-17.2645949112854,17.1147059640261,-19.0889249053867));
#38928=CARTESIAN_POINT('Ctrl Pts',(-17.3331941043313,17.0666211049302,-19.093103583468));
#38929=CARTESIAN_POINT('Ctrl Pts',(-17.4042580092797,17.0218356001939,-19.0972822615493));
#38930=CARTESIAN_POINT('Ctrl Pts',(-17.4774351014431,16.9806088558922,-19.1014609396307));
#38931=CARTESIAN_POINT('Ctrl Pts',(-17.5519238404496,16.9386431517955,-19.1057145175168));
#38932=CARTESIAN_POINT('Ctrl Pts',(-17.6286019037991,16.9003653586862,-19.1099680954028));
#38933=CARTESIAN_POINT('Ctrl Pts',(-17.7070663992917,16.8660037569889,-19.1142216732889));
#38934=CARTESIAN_POINT('Ctrl Pts',(-17.7840097073668,16.8323083220186,-19.1183927872642));
#38935=CARTESIAN_POINT('Ctrl Pts',(-17.862670357959,16.8023787805161,-19.1225639012394));
#38936=CARTESIAN_POINT('Ctrl Pts',(-17.942644030864,16.7763838639094,-19.1267350152146));
#38937=CARTESIAN_POINT('Ctrl Pts',(-18.0225908678302,16.7503976701481,-19.1309047295323));
#38938=CARTESIAN_POINT('Ctrl Pts',(-18.1038494149387,16.7283436212316,-19.1350744438499));
#38939=CARTESIAN_POINT('Ctrl Pts',(-18.185997896633,16.7103413478235,-19.1392441581675));
#38940=CARTESIAN_POINT('Ctrl Pts',(-18.2681434551313,16.6923397150136,-19.1434137241088));
#38941=CARTESIAN_POINT('Ctrl Pts',(-18.3511784357002,16.6783896686898,-19.1475832900501));
#38942=CARTESIAN_POINT('Ctrl Pts',(-18.4346698530371,16.6685599391295,-19.1517528559914));
#38943=CARTESIAN_POINT('Ctrl Pts',(-18.5210967257309,16.6583846083899,-19.1560690187335));
#38944=CARTESIAN_POINT('Ctrl Pts',(-18.6080122052096,16.6526247876704,-19.1603851814756));
#38945=CARTESIAN_POINT('Ctrl Pts',(-18.6949310840593,16.6512981384921,-19.1647013442177));
#38946=CARTESIAN_POINT('Ctrl Pts',(-18.7790185894541,16.650014704773,-19.1688769084065));
#38947=CARTESIAN_POINT('Ctrl Pts',(-18.8631088069912,16.652879993597,-19.1730524725954));
#38948=CARTESIAN_POINT('Ctrl Pts',(-18.946765090109,16.6598569196474,-19.1772280367842));
#38949=CARTESIAN_POINT('Ctrl Pts',(-19.0346466533962,16.6671862336619,-19.181614498803));
#38950=CARTESIAN_POINT('Ctrl Pts',(-19.1220487156005,16.6790533797552,-19.1860009608217));
#38951=CARTESIAN_POINT('Ctrl Pts',(-19.2084765196395,16.6953545495617,-19.1903874228404));
#38952=CARTESIAN_POINT('Ctrl Pts',(-19.2949043236785,16.7116557193682,-19.1947738848591));
#38953=CARTESIAN_POINT('Ctrl Pts',(-19.3803573236336,16.7323907021497,-19.1991603468778));
#38954=CARTESIAN_POINT('Ctrl Pts',(-19.4643607861717,16.7573958913422,-19.2035468088965));
#38955=CARTESIAN_POINT('Ctrl Pts',(-19.5444991251657,16.7812505547997,-19.2077314433106));
#38956=CARTESIAN_POINT('Ctrl Pts',(-19.6236166763879,16.8090798944626,-19.2119160777247));
#38957=CARTESIAN_POINT('Ctrl Pts',(-19.7012904347963,16.8407786570129,-19.2161007121388));
#38958=CARTESIAN_POINT('Ctrl Pts',(-19.7788536342255,16.872432300299,-19.2202793902439));
#38959=CARTESIAN_POINT('Ctrl Pts',(-19.8549767005509,16.907944254222,-19.2244580683489));
#38960=CARTESIAN_POINT('Ctrl Pts',(-19.9292512406659,16.9471593537339,-19.228636746454));
#38961=CARTESIAN_POINT('Ctrl Pts',(-20.0048570980567,16.98707735547,-19.2328903243342));
#38962=CARTESIAN_POINT('Ctrl Pts',(-20.0785470456703,17.0308324287623,-19.2371439022144));
#38963=CARTESIAN_POINT('Ctrl Pts',(-20.1499110578951,17.0782093688947,-19.2413974800945));
#38964=CARTESIAN_POINT('Ctrl Pts',(-20.2198915399285,17.1246678148869,-19.2455685940936));
#38965=CARTESIAN_POINT('Ctrl Pts',(-20.287635066423,17.1746086809011,-19.2497397080927));
#38966=CARTESIAN_POINT('Ctrl Pts',(-20.3527809100897,17.2277833287487,-19.2539108220917));
#38967=CARTESIAN_POINT('Ctrl Pts',(-20.4179048934388,17.2809401333292,-19.2580805364332));
#38968=CARTESIAN_POINT('Ctrl Pts',(-20.4804325690374,17.3373282740108,-19.2622502507746));
#38969=CARTESIAN_POINT('Ctrl Pts',(-20.5400350473177,17.3966578581039,-19.2664199651161));
#38970=CARTESIAN_POINT('Ctrl Pts',(-20.5996354046851,17.4559853309948,-19.2705895310811));
#38971=CARTESIAN_POINT('Ctrl Pts',(-20.6563104462573,17.5182537140387,-19.2747590970462));
#38972=CARTESIAN_POINT('Ctrl Pts',(-20.7097680140133,17.5831361375097,-19.2789286630112));
#38973=CARTESIAN_POINT('Ctrl Pts',(-20.7651050833052,17.6502997462213,-19.2832448257251));
#38974=CARTESIAN_POINT('Ctrl Pts',(-20.8169938810692,17.7202642276974,-19.287560988439));
#38975=CARTESIAN_POINT('Ctrl Pts',(-20.8651569231979,17.7926311591459,-19.2918771511529));
#38976=CARTESIAN_POINT('Ctrl Pts',(-20.9117510597951,17.8626407461655,-19.2960527153652));
#38977=CARTESIAN_POINT('Ctrl Pts',(-20.9548582452775,17.9348982385164,-19.3002282795775));
#38978=CARTESIAN_POINT('Ctrl Pts',(-20.9942733140221,18.0090164119592,-19.3044038437898));
#38979=CARTESIAN_POINT('Ctrl Pts',(-21.0356791435328,18.0868781169101,-19.3087903057545));
#38980=CARTESIAN_POINT('Ctrl Pts',(-21.0730098296529,18.1667928797187,-19.3131767677192));
#38981=CARTESIAN_POINT('Ctrl Pts',(-21.1060848561709,18.2482884984978,-19.3175632296839));
#38982=CARTESIAN_POINT('Ctrl Pts',(-21.1391598826889,18.329784117277,-19.3219496916486));
#38983=CARTESIAN_POINT('Ctrl Pts',(-21.1679791313067,18.4128600189272,-19.3263361536133));
#38984=CARTESIAN_POINT('Ctrl Pts',(-21.1924232051052,18.4970284707355,-19.330722615578));
#38985=CARTESIAN_POINT('Ctrl Pts',(-21.2214742546483,18.5970601546363,-19.3359357942367));
#38986=CARTESIAN_POINT('Ctrl Pts',(-21.2444357643533,18.6989346521836,-19.3411489728953));
#38987=CARTESIAN_POINT('Ctrl Pts',(-21.2611151500594,18.8019901977457,-19.3463621515539));
#38988=CARTESIAN_POINT('Ctrl Pts',(-21.2775287210165,18.9034033756297,-19.3514922492285));
#38989=CARTESIAN_POINT('Ctrl Pts',(-21.2878587863005,19.0059603454814,-19.3566223469032));
#38990=CARTESIAN_POINT('Ctrl Pts',(-21.2919675308107,19.1090092586637,-19.3617524445778));
#38991=CARTESIAN_POINT('Ctrl Pts',(-21.2932910194166,19.1422028685647,-19.3634049264499));
#38992=CARTESIAN_POINT('Ctrl Pts',(-21.2939693565913,19.1754473495009,-19.3650574083219));
#38993=CARTESIAN_POINT('Ctrl Pts',(-21.2939989850552,19.2087204131754,-19.3667098901939));
#38994=CARTESIAN_POINT('Origin',(-18.734,19.211,1.76670989022852));
#38995=CARTESIAN_POINT('',(-17.1744642439897,21.2411350264762,-18.0500683119931));
#38996=CARTESIAN_POINT('',(-17.1744642439897,21.2411350264762,-18.1167065484839));
#38997=CARTESIAN_POINT('',(-17.1744642439897,21.2411350264762,1.76670989022852));
#38998=CARTESIAN_POINT('',(-21.2936055415609,19.2113823947434,-18.6332901348857));
#38999=CARTESIAN_POINT('Ctrl Pts',(-17.1744642439897,21.2411350264762,-18.1167065484839));
#39000=CARTESIAN_POINT('Ctrl Pts',(-17.1077795034155,21.1899082676894,-18.1208760279071));
#39001=CARTESIAN_POINT('Ctrl Pts',(-17.0436130429836,21.1353860024748,-18.1250455073302));
#39002=CARTESIAN_POINT('Ctrl Pts',(-16.9822981323806,21.0778531187478,-18.1292149867534));
#39003=CARTESIAN_POINT('Ctrl Pts',(-16.9209724759196,21.0203101519891,-18.1333851969064));
#39004=CARTESIAN_POINT('Ctrl Pts',(-16.8624996961633,20.9597558347282,-18.1375554070594));
#39005=CARTESIAN_POINT('Ctrl Pts',(-16.807176747738,20.8965124308478,-18.1417256172124));
#39006=CARTESIAN_POINT('Ctrl Pts',(-16.7517926921237,20.8331991712069,-18.145900433588));
#39007=CARTESIAN_POINT('Ctrl Pts',(-16.6995657146274,20.7671912439353,-18.1500752499637));
#39008=CARTESIAN_POINT('Ctrl Pts',(-16.6507525780277,20.6988441379545,-18.1542500663394));
#39009=CARTESIAN_POINT('Ctrl Pts',(-16.6019086931009,20.6304539788262,-18.1584275125116));
#39010=CARTESIAN_POINT('Ctrl Pts',(-16.5564831775601,20.559722095032,-18.1626049586839));
#39011=CARTESIAN_POINT('Ctrl Pts',(-16.5146882374202,20.4870310734755,-18.1667824048561));
#39012=CARTESIAN_POINT('Ctrl Pts',(-16.4728247886002,20.4142208995544,-18.1709666985396));
#39013=CARTESIAN_POINT('Ctrl Pts',(-16.4346040018293,20.3394455874191,-18.1751509922232));
#39014=CARTESIAN_POINT('Ctrl Pts',(-16.4001909244614,20.2631098796863,-18.1793352859067));
#39015=CARTESIAN_POINT('Ctrl Pts',(-16.385413108711,20.2303294627539,-18.1811321237901));
#39016=CARTESIAN_POINT('Ctrl Pts',(-16.371336836165,20.1972615163169,-18.1829289616735));
#39017=CARTESIAN_POINT('Ctrl Pts',(-16.3579723492966,20.1639389293617,-18.184725799557));
#39018=CARTESIAN_POINT('Ctrl Pts',(-16.3268479546498,20.0863343526005,-18.1889104339505));
#39019=CARTESIAN_POINT('Ctrl Pts',(-16.2994716572956,20.00705890033,-18.193095068344));
#39020=CARTESIAN_POINT('Ctrl Pts',(-16.2760239311543,19.926509360513,-18.1972797027374));
#39021=CARTESIAN_POINT('Ctrl Pts',(-16.252609579949,19.846074472996,-18.2014583808218));
#39022=CARTESIAN_POINT('Ctrl Pts',(-16.2331128202905,19.7643695380471,-18.2056370589062));
#39023=CARTESIAN_POINT('Ctrl Pts',(-16.217665944864,19.681810920607,-18.2098157369906));
#39024=CARTESIAN_POINT('Ctrl Pts',(-16.2019421952991,19.5977724992941,-18.2140693148759));
#39025=CARTESIAN_POINT('Ctrl Pts',(-16.190415125853,19.512849937439,-18.2183228927612));
#39026=CARTESIAN_POINT('Ctrl Pts',(-16.1831710111198,19.4274981974256,-18.2225764706466));
#39027=CARTESIAN_POINT('Ctrl Pts',(-16.1760673376856,19.3438011674318,-18.226747584625));
#39028=CARTESIAN_POINT('Ctrl Pts',(-16.1730820747445,19.2596919311862,-18.2309186986033));
#39029=CARTESIAN_POINT('Ctrl Pts',(-16.1742446642318,19.1756076137226,-18.2350898125817));
#39030=CARTESIAN_POINT('Ctrl Pts',(-16.1754068636011,19.0915515115639,-18.2392595269025));
#39031=CARTESIAN_POINT('Ctrl Pts',(-16.180714144804,19.0075207711868,-18.2434292412233));
#39032=CARTESIAN_POINT('Ctrl Pts',(-16.1901438433302,18.9239532195391,-18.2475989555441));
#39033=CARTESIAN_POINT('Ctrl Pts',(-16.1995732063072,18.8403886415836,-18.2517685214886));
#39034=CARTESIAN_POINT('Ctrl Pts',(-16.2131246425145,18.7572876766228,-18.2559380874331));
#39035=CARTESIAN_POINT('Ctrl Pts',(-16.2307236899663,18.675082361156,-18.2601076533775));
#39036=CARTESIAN_POINT('Ctrl Pts',(-16.2489414982118,18.5899868082275,-18.264423816116));
#39037=CARTESIAN_POINT('Ctrl Pts',(-16.2714967310844,18.5058515744436,-18.2687399788544));
#39038=CARTESIAN_POINT('Ctrl Pts',(-16.2982497538328,18.4231416762538,-18.2730561415928));
#39039=CARTESIAN_POINT('Ctrl Pts',(-16.3241312996847,18.3431260442804,-18.2772317057849));
#39040=CARTESIAN_POINT('Ctrl Pts',(-16.3539411382346,18.2644447370891,-18.281407269977));
#39041=CARTESIAN_POINT('Ctrl Pts',(-16.387503456575,18.1874991589185,-18.2855828341691));
#39042=CARTESIAN_POINT('Ctrl Pts',(-16.4227609278166,18.1066672425414,-18.2899692961806));
#39043=CARTESIAN_POINT('Ctrl Pts',(-16.4621596558343,18.0277515290339,-18.2943557581922));
#39044=CARTESIAN_POINT('Ctrl Pts',(-16.5054419382127,17.9511869324211,-18.2987422202037));
#39045=CARTESIAN_POINT('Ctrl Pts',(-16.548724220591,17.8746223358082,-18.3031286822153));
#39046=CARTESIAN_POINT('Ctrl Pts',(-16.5958896819152,17.8004093049792,-18.3075151442268));
#39047=CARTESIAN_POINT('Ctrl Pts',(-16.6466304638567,17.7289445288449,-18.3119016062384));
#39048=CARTESIAN_POINT('Ctrl Pts',(-16.6950365872103,17.6607679529895,-18.3160862406309));
#39049=CARTESIAN_POINT('Ctrl Pts',(-16.7468764264203,17.5948385205843,-18.3202708750235));
#39050=CARTESIAN_POINT('Ctrl Pts',(-16.8019140327136,17.5315227554341,-18.324455509416));
#39051=CARTESIAN_POINT('Ctrl Pts',(-16.8568732997865,17.4682971124385,-18.3286341874995));
#39052=CARTESIAN_POINT('Ctrl Pts',(-16.9150209937605,17.4076780913738,-18.3328128655829));
#39053=CARTESIAN_POINT('Ctrl Pts',(-16.9760786251332,17.3500022998976,-18.3369915436664));
#39054=CARTESIAN_POINT('Ctrl Pts',(-17.0382306706762,17.2912927113013,-18.3412451215519));
#39055=CARTESIAN_POINT('Ctrl Pts',(-17.1033977218496,17.2356332980397,-18.3454986994375));
#39056=CARTESIAN_POINT('Ctrl Pts',(-17.1712439260892,17.1833428659029,-18.3497522773231));
#39057=CARTESIAN_POINT('Ctrl Pts',(-17.2377747992588,17.132066185837,-18.3539233913005));
#39058=CARTESIAN_POINT('Ctrl Pts',(-17.3068814901404,17.0840293178158,-18.358094505278));
#39059=CARTESIAN_POINT('Ctrl Pts',(-17.3782123821184,17.0394936253377,-18.3622656192554));
#39060=CARTESIAN_POINT('Ctrl Pts',(-17.4495193383267,16.9949728772413,-18.3664353335753));
#39061=CARTESIAN_POINT('Ctrl Pts',(-17.5230486234685,16.9539512148435,-18.3706050478952));
#39062=CARTESIAN_POINT('Ctrl Pts',(-17.5984198264988,16.9166465683006,-18.3747747622151));
#39063=CARTESIAN_POINT('Ctrl Pts',(-17.6737883474984,16.879343249217,-18.3789443281587));
#39064=CARTESIAN_POINT('Ctrl Pts',(-17.7509982433954,16.8457568863071,-18.3831138941022));
#39065=CARTESIAN_POINT('Ctrl Pts',(-17.8296459350048,16.8160587219878,-18.3872834600458));
#39066=CARTESIAN_POINT('Ctrl Pts',(-17.9110587824491,16.78531640684,-18.3915996227853));
#39067=CARTESIAN_POINT('Ctrl Pts',(-17.9940119191525,16.7587409819327,-18.3959157855248));
#39068=CARTESIAN_POINT('Ctrl Pts',(-18.0780387582283,16.736466741122,-18.4002319482643));
#39069=CARTESIAN_POINT('Ctrl Pts',(-18.1593284318393,16.7149180813682,-18.4044075124555));
#39070=CARTESIAN_POINT('Ctrl Pts',(-18.241622459801,16.697394738803,-18.4085830766467));
#39071=CARTESIAN_POINT('Ctrl Pts',(-18.3244881604803,16.6839661550954,-18.412758640838));
#39072=CARTESIAN_POINT('Ctrl Pts',(-18.4115392107379,16.6698593255431,-18.4171451028516));
#39073=CARTESIAN_POINT('Ctrl Pts',(-18.4992206213763,16.6602718418454,-18.4215315648652));
#39074=CARTESIAN_POINT('Ctrl Pts',(-18.5870272090961,16.6552224277661,-18.4259180268789));
#39075=CARTESIAN_POINT('Ctrl Pts',(-18.6748337968158,16.6501730136867,-18.4303044888925));
#39076=CARTESIAN_POINT('Ctrl Pts',(-18.7627649809675,16.6496615965365,-18.4346909509062));
#39077=CARTESIAN_POINT('Ctrl Pts',(-18.8503205710793,16.6536440363642,-18.4390774129198));
#39078=CARTESIAN_POINT('Ctrl Pts',(-18.933847598669,16.6574432382305,-18.4432620473123));
#39079=CARTESIAN_POINT('Ctrl Pts',(-19.0173437395032,16.6653459878635,-18.4474466817047));
#39080=CARTESIAN_POINT('Ctrl Pts',(-19.1003730904697,16.6773522820685,-18.4516313160972));
#39081=CARTESIAN_POINT('Ctrl Pts',(-19.1832842594318,16.6893414867997,-18.4558099941806));
#39082=CARTESIAN_POINT('Ctrl Pts',(-19.2657295068654,16.7054225689875,-18.4599886722639));
#39083=CARTESIAN_POINT('Ctrl Pts',(-19.3472750579142,16.7255435623732,-18.4641673503473));
#39084=CARTESIAN_POINT('Ctrl Pts',(-19.4302822543744,16.7460252101083,-18.4684209282328));
#39085=CARTESIAN_POINT('Ctrl Pts',(-19.5123567014427,16.7706930025011,-18.4726745061184));
#39086=CARTESIAN_POINT('Ctrl Pts',(-19.5930485432788,16.7994371042225,-18.476928084004));
#39087=CARTESIAN_POINT('Ctrl Pts',(-19.6721760162895,16.8276239454375,-18.4810991979814));
#39088=CARTESIAN_POINT('Ctrl Pts',(-19.7499735613555,16.8597302905279,-18.4852703119587));
#39089=CARTESIAN_POINT('Ctrl Pts',(-19.8260310897313,16.8956019566692,-18.4894414259361));
#39090=CARTESIAN_POINT('Ctrl Pts',(-19.9020630962689,16.9314615857264,-18.4936111402558));
#39091=CARTESIAN_POINT('Ctrl Pts',(-19.9763558299785,16.9710838304486,-18.4977808545756));
#39092=CARTESIAN_POINT('Ctrl Pts',(-20.0485201368032,17.0142667868085,-18.5019505688954));
#39093=CARTESIAN_POINT('Ctrl Pts',(-20.120681875712,17.0574482065333,-18.5061201348388));
#39094=CARTESIAN_POINT('Ctrl Pts',(-20.1907149440075,17.1041898490219,-18.5102897007822));
#39095=CARTESIAN_POINT('Ctrl Pts',(-20.2582569041587,17.1542450583201,-18.5144592667256));
#39096=CARTESIAN_POINT('Ctrl Pts',(-20.3281735563287,17.2060601470437,-18.5187754294653));
#39097=CARTESIAN_POINT('Ctrl Pts',(-20.3954202425932,17.2614258339343,-18.5230915922049));
#39098=CARTESIAN_POINT('Ctrl Pts',(-20.4596314884394,17.3200224839765,-18.5274077549445));
#39099=CARTESIAN_POINT('Ctrl Pts',(-20.5217510596867,17.3767103542892,-18.5315833191356));
#39100=CARTESIAN_POINT('Ctrl Pts',(-20.5810296141597,17.4364215555164,-18.5357588833267));
#39101=CARTESIAN_POINT('Ctrl Pts',(-20.637174560043,17.4988298583361,-18.5399344475178));
#39102=CARTESIAN_POINT('Ctrl Pts',(-20.6961552536978,17.5643902561997,-18.5443209095317));
#39103=CARTESIAN_POINT('Ctrl Pts',(-20.7516770948088,17.6329269235823,-18.5487073715456));
#39104=CARTESIAN_POINT('Ctrl Pts',(-20.8034508935155,17.7040252160943,-18.5530938335595));
#39105=CARTESIAN_POINT('Ctrl Pts',(-20.8552246922223,17.7751235086063,-18.5574802955734));
#39106=CARTESIAN_POINT('Ctrl Pts',(-20.9032501953501,17.8487828986679,-18.5618667575873));
#39107=CARTESIAN_POINT('Ctrl Pts',(-20.9472937739972,17.9245589131308,-18.5662532196012));
#39108=CARTESIAN_POINT('Ctrl Pts',(-20.9909726387699,17.9997074453438,-18.5706033584188));
#39109=CARTESIAN_POINT('Ctrl Pts',(-21.0308877830075,18.0771985084606,-18.5749534972363));
#39110=CARTESIAN_POINT('Ctrl Pts',(-21.0667913726612,18.1566355413627,-18.5793036360538));
#39111=CARTESIAN_POINT('Ctrl Pts',(-21.1039225287098,18.2387885765656,-18.5838025088636));
#39112=CARTESIAN_POINT('Ctrl Pts',(-21.1367625751612,18.3230227236645,-18.5883013816734));
#39113=CARTESIAN_POINT('Ctrl Pts',(-21.1650869626505,18.4088677290927,-18.5928002544832));
#39114=CARTESIAN_POINT('Ctrl Pts',(-21.1923645588302,18.4915401396792,-18.5971328613513));
#39115=CARTESIAN_POINT('Ctrl Pts',(-21.2154541944225,18.5757060184776,-18.6014654682194));
#39116=CARTESIAN_POINT('Ctrl Pts',(-21.234202937817,18.6609224875245,-18.6057980750875));
#39117=CARTESIAN_POINT('Ctrl Pts',(-21.2529274817652,18.7460289656604,-18.6101250897574));
#39118=CARTESIAN_POINT('Ctrl Pts',(-21.2673221897251,18.8321829392873,-18.6144521044274));
#39119=CARTESIAN_POINT('Ctrl Pts',(-21.2772839154183,18.9189265065526,-18.6187791190974));
#39120=CARTESIAN_POINT('Ctrl Pts',(-21.2872318317724,19.0055498264465,-18.6231001354881));
#39121=CARTESIAN_POINT('Ctrl Pts',(-21.2927589555479,19.0927607071587,-18.6274211518788));
#39122=CARTESIAN_POINT('Ctrl Pts',(-21.2938134141941,19.1800923227686,-18.6317421682696));
#39123=CARTESIAN_POINT('Ctrl Pts',(-21.2939393290371,19.1905207513303,-18.6322581487702));
#39124=CARTESIAN_POINT('Ctrl Pts',(-21.2940015277988,19.2009508929668,-18.6327741292709));
#39125=CARTESIAN_POINT('Ctrl Pts',(-21.2939999715072,19.2113819467094,-18.6332901097715));
#39126=CARTESIAN_POINT('Ctrl Pts',(-21.2898372017813,19.2113866752102,-18.6332903748237));
#39127=CARTESIAN_POINT('Ctrl Pts',(-21.2903732285223,19.6159817978459,-18.6533365919766));
#39128=CARTESIAN_POINT('Ctrl Pts',(-21.0089154443045,20.8754716727687,-18.7157747446901));
#39129=CARTESIAN_POINT('Ctrl Pts',(-19.2309397186665,22.0893674765224,-18.810203250608));
#39130=CARTESIAN_POINT('Ctrl Pts',(-17.688669459474,21.6276028702836,-18.884585539373));
#39131=CARTESIAN_POINT('Ctrl Pts',(-17.1746506311398,21.2408837946621,-18.9165758925774));
#39132=CARTESIAN_POINT('',(-21.2939999971965,19.2111198080496,-18.5667098901964));
#39133=CARTESIAN_POINT('Ctrl Pts',(-21.2939999971965,19.2111198086917,-18.5667098902285));
#39134=CARTESIAN_POINT('Ctrl Pts',(-21.2939996986147,19.2174997239769,-18.5670291853155));
#39135=CARTESIAN_POINT('Ctrl Pts',(-21.2939755504833,19.223879573923,-18.5673484804024));
#39136=CARTESIAN_POINT('Ctrl Pts',(-21.2939275539577,19.2302592442234,-18.5676677754894));
#39137=CARTESIAN_POINT('Ctrl Pts',(-21.2932985185608,19.31387026376,-18.5718524098819));
#39138=CARTESIAN_POINT('Ctrl Pts',(-21.2885677156651,19.3976060296583,-18.5760370442745));
#39139=CARTESIAN_POINT('Ctrl Pts',(-21.2797186185528,19.4810309522135,-18.580221678667));
#39140=CARTESIAN_POINT('Ctrl Pts',(-21.2708821170351,19.5643371297175,-18.5844003567505));
#39141=CARTESIAN_POINT('Ctrl Pts',(-21.2579390129528,19.6473328891638,-18.5885790348339));
#39142=CARTESIAN_POINT('Ctrl Pts',(-21.2409247859828,19.7295827970778,-18.5927577129174));
#39143=CARTESIAN_POINT('Ctrl Pts',(-21.2236055912197,19.8133069754917,-18.5970112908029));
#39144=CARTESIAN_POINT('Ctrl Pts',(-21.2020678918843,19.8962578184688,-18.6012648686885));
#39145=CARTESIAN_POINT('Ctrl Pts',(-21.1764043852928,19.9779816286603,-18.605518446574));
#39146=CARTESIAN_POINT('Ctrl Pts',(-21.1512384158585,20.0581210633086,-18.6096895605515));
#39147=CARTESIAN_POINT('Ctrl Pts',(-21.1221053294156,20.1370801583403,-18.613860674529));
#39148=CARTESIAN_POINT('Ctrl Pts',(-21.0891436468889,20.2144432731942,-18.6180317885065));
#39149=CARTESIAN_POINT('Ctrl Pts',(-21.0561930249731,20.2917804281078,-18.6222015028263));
#39150=CARTESIAN_POINT('Ctrl Pts',(-21.0194165386216,20.3675222435798,-18.6263712171462));
#39151=CARTESIAN_POINT('Ctrl Pts',(-20.9790011895033,20.4412721890413,-18.6305409314661));
#39152=CARTESIAN_POINT('Ctrl Pts',(-20.9385872785366,20.5150195101634,-18.6347104974097));
#39153=CARTESIAN_POINT('Ctrl Pts',(-20.8945349840829,20.5867746991834,-18.6388800633533));
#39154=CARTESIAN_POINT('Ctrl Pts',(-20.8470770406692,20.6561662258013,-18.6430496292968));
#39155=CARTESIAN_POINT('Ctrl Pts',(-20.7979505344985,20.7279974729093,-18.6473657920363));
#39156=CARTESIAN_POINT('Ctrl Pts',(-20.7451747360215,20.7972953169815,-18.6516819547758));
#39157=CARTESIAN_POINT('Ctrl Pts',(-20.6890551911697,20.863682425477,-18.6559981175153));
#39158=CARTESIAN_POINT('Ctrl Pts',(-20.634763734602,20.9279069808801,-18.6601736817066));
#39159=CARTESIAN_POINT('Ctrl Pts',(-20.5773433873057,20.9894072108732,-18.6643492458978));
#39160=CARTESIAN_POINT('Ctrl Pts',(-20.517109048565,21.0478783631274,-18.668524810089));
#39161=CARTESIAN_POINT('Ctrl Pts',(-20.4538324165451,21.1093027543023,-18.6729112721026));
#39162=CARTESIAN_POINT('Ctrl Pts',(-20.3874504923528,21.1673836440657,-18.6772977341163));
#39163=CARTESIAN_POINT('Ctrl Pts',(-20.3183666557521,21.2218163268038,-18.6816841961299));
#39164=CARTESIAN_POINT('Ctrl Pts',(-20.2492828191514,21.276249009542,-18.6860706581436));
#39165=CARTESIAN_POINT('Ctrl Pts',(-20.1774975877418,21.327033212256,-18.6904571201572));
#39166=CARTESIAN_POINT('Ctrl Pts',(-20.1034462555222,21.3739186191894,-18.6948435821709));
#39167=CARTESIAN_POINT('Ctrl Pts',(-20.032802134896,21.4186467590315,-18.6990282165633));
#39168=CARTESIAN_POINT('Ctrl Pts',(-19.9598329133702,21.459993484366,-18.7032128509558));
#39169=CARTESIAN_POINT('Ctrl Pts',(-19.8848959073541,21.497709122393,-18.7073974853483));
#39170=CARTESIAN_POINT('Ctrl Pts',(-19.8100655648908,21.5353710768775,-18.7115761634316));
#39171=CARTESIAN_POINT('Ctrl Pts',(-19.733273408809,21.5694120050826,-18.715754841515));
#39172=CARTESIAN_POINT('Ctrl Pts',(-19.654904774228,21.5996260479204,-18.7199335195984));
#39173=CARTESIAN_POINT('Ctrl Pts',(-19.5751314381808,21.630381655767,-18.7241870974839));
#39174=CARTESIAN_POINT('Ctrl Pts',(-19.493724958338,21.6571715770569,-18.7284406753695));
#39175=CARTESIAN_POINT('Ctrl Pts',(-19.41111699767,21.6798281777933,-18.7326942532551));
#39176=CARTESIAN_POINT('Ctrl Pts',(-19.3301105535301,21.7020455361098,-18.7368653672325));
#39177=CARTESIAN_POINT('Ctrl Pts',(-19.2479492630204,21.7202882813848,-18.7410364812098));
#39178=CARTESIAN_POINT('Ctrl Pts',(-19.1650575928257,21.734447909442,-18.7452075951871));
#39179=CARTESIAN_POINT('Ctrl Pts',(-19.0821937377315,21.7486027860993,-18.7493773095069));
#39180=CARTESIAN_POINT('Ctrl Pts',(-18.9986004427839,21.7586771892408,-18.7535470238267));
#39181=CARTESIAN_POINT('Ctrl Pts',(-18.9147123478954,21.7646137232005,-18.7577167381465));
#39182=CARTESIAN_POINT('Ctrl Pts',(-18.8308272381054,21.7705500459129,-18.7618863040899));
#39183=CARTESIAN_POINT('Ctrl Pts',(-18.7466478081773,21.7723487605766,-18.7660558700333));
#39184=CARTESIAN_POINT('Ctrl Pts',(-18.6626124310825,21.7700044577929,-18.7702254359768));
#39185=CARTESIAN_POINT('Ctrl Pts',(-18.5756224737711,21.7675777322146,-18.7745415987164));
#39186=CARTESIAN_POINT('Ctrl Pts',(-18.4887874147817,21.7607112463061,-18.778857761456));
#39187=CARTESIAN_POINT('Ctrl Pts',(-18.4025899172848,21.749457672894,-18.7831739241957));
#39188=CARTESIAN_POINT('Ctrl Pts',(-18.3192002942283,21.7385706834556,-18.7873494883867));
#39189=CARTESIAN_POINT('Ctrl Pts',(-18.2364077885004,21.7235781663988,-18.7915250525778));
#39190=CARTESIAN_POINT('Ctrl Pts',(-18.1546390975914,21.7045799455322,-18.7957006167689));
#39191=CARTESIAN_POINT('Ctrl Pts',(-18.0687404644519,21.6846221696844,-18.8000870787828));
#39192=CARTESIAN_POINT('Ctrl Pts',(-17.9839723511224,21.6602435606427,-18.8044735407967));
#39193=CARTESIAN_POINT('Ctrl Pts',(-17.9008093086191,21.6316183655827,-18.8088600028106));
#39194=CARTESIAN_POINT('Ctrl Pts',(-17.8176462661158,21.6029931705227,-18.8132464648245));
#39195=CARTESIAN_POINT('Ctrl Pts',(-17.7360888041544,21.5701216768946,-18.8176329268384));
#39196=CARTESIAN_POINT('Ctrl Pts',(-17.6565830150584,21.5332344068933,-18.8220193888523));
#39197=CARTESIAN_POINT('Ctrl Pts',(-17.5807293782392,21.4980415786259,-18.8262043557623));
#39198=CARTESIAN_POINT('Ctrl Pts',(-17.5064606949712,21.4590628106661,-18.8303893226724));
#39199=CARTESIAN_POINT('Ctrl Pts',(-17.4341804046275,21.4164634477782,-18.8345742895824));
#39200=CARTESIAN_POINT('Ctrl Pts',(-17.3620114350738,21.3739296932975,-18.8387528111141));
#39201=CARTESIAN_POINT('Ctrl Pts',(-17.2918251656452,21.3277866569804,-18.8429313326457));
#39202=CARTESIAN_POINT('Ctrl Pts',(-17.2240032215556,21.2782468960159,-18.8471098541774));
#39203=CARTESIAN_POINT('Ctrl Pts',(-17.207345913612,21.2660797565316,-18.848136113758));
#39204=CARTESIAN_POINT('Ctrl Pts',(-17.1908311129492,21.2537079425745,-18.8491623733387));
#39205=CARTESIAN_POINT('Ctrl Pts',(-17.1744642439897,21.2411350264762,-18.8501886329194));
#39206=CARTESIAN_POINT('Ctrl Pts',(-17.1744642439897,21.2411350264762,-18.0500683119931));
#39207=CARTESIAN_POINT('Ctrl Pts',(-17.1273612179385,21.2049508060252,-18.05303372425));
#39208=CARTESIAN_POINT('Ctrl Pts',(-17.0815714415894,21.1671673406356,-18.0559991365068));
#39209=CARTESIAN_POINT('Ctrl Pts',(-17.0372042845896,21.1278944415811,-18.0589645487637));
#39210=CARTESIAN_POINT('Ctrl Pts',(-16.9745956774138,21.0724745842853,-18.0631491831568));
#39211=CARTESIAN_POINT('Ctrl Pts',(-16.9145885551714,21.0138810328614,-18.06733381755));
#39212=CARTESIAN_POINT('Ctrl Pts',(-16.8575221052048,20.9523875818855,-18.0715184519431));
#39213=CARTESIAN_POINT('Ctrl Pts',(-16.8005368822663,20.8909816592257,-18.0756971300271));
#39214=CARTESIAN_POINT('Ctrl Pts',(-16.7464843277716,20.8266843701414,-18.0798758081111));
#39215=CARTESIAN_POINT('Ctrl Pts',(-16.6956693348425,20.759808606471,-18.0840544861951));
#39216=CARTESIAN_POINT('Ctrl Pts',(-16.6439435196862,20.6917341428008,-18.0883080640805));
#39217=CARTESIAN_POINT('Ctrl Pts',(-16.5955728353226,20.6209881765787,-18.0925616419659));
#39218=CARTESIAN_POINT('Ctrl Pts',(-16.5508383402299,20.5479387298264,-18.0968152198513));
#39219=CARTESIAN_POINT('Ctrl Pts',(-16.506971110616,20.4763054891424,-18.1009863338293));
#39220=CARTESIAN_POINT('Ctrl Pts',(-16.4666005905002,20.4024576962093,-18.1051574478073));
#39221=CARTESIAN_POINT('Ctrl Pts',(-16.4299490395871,20.3267729033367,-18.1093285617853));
#39222=CARTESIAN_POINT('Ctrl Pts',(-16.393309787456,20.2511135072274,-18.1134982761058));
#39223=CARTESIAN_POINT('Ctrl Pts',(-16.3603872264447,20.1736187490988,-18.1176679904262));
#39224=CARTESIAN_POINT('Ctrl Pts',(-16.3313573525109,20.0946901654238,-18.1218377047466));
#39225=CARTESIAN_POINT('Ctrl Pts',(-16.3023285115847,20.0157643903665,-18.1260072706907));
#39226=CARTESIAN_POINT('Ctrl Pts',(-16.2771922403253,19.9354053232569,-18.1301768366348));
#39227=CARTESIAN_POINT('Ctrl Pts',(-16.2560756369329,19.854032542659,-18.1343464025789));
#39228=CARTESIAN_POINT('Ctrl Pts',(-16.2342165998161,19.7697987954821,-18.1386625653178));
#39229=CARTESIAN_POINT('Ctrl Pts',(-16.2166652853052,19.6844792346862,-18.1429787280566));
#39230=CARTESIAN_POINT('Ctrl Pts',(-16.203505316394,19.5985521335794,-18.1472948907955));
#39231=CARTESIAN_POINT('Ctrl Pts',(-16.1907740320855,19.5154240987507,-18.1514704549872));
#39232=CARTESIAN_POINT('Ctrl Pts',(-16.1821523920334,19.4317279704213,-18.1556460191789));
#39233=CARTESIAN_POINT('Ctrl Pts',(-16.177663165104,19.3479013752812,-18.1598215833707));
#39234=CARTESIAN_POINT('Ctrl Pts',(-16.1729471979947,19.2598408981034,-18.1642080453831));
#39235=CARTESIAN_POINT('Ctrl Pts',(-16.172792072363,19.1716370118691,-18.1685945073955));
#39236=CARTESIAN_POINT('Ctrl Pts',(-16.1771623761343,19.0837940049179,-18.1729809694079));
#39237=CARTESIAN_POINT('Ctrl Pts',(-16.1815326799056,18.9959509979667,-18.1773674314203));
#39238=CARTESIAN_POINT('Ctrl Pts',(-16.1904282787084,18.9084694398441,-18.1817538934327));
#39239=CARTESIAN_POINT('Ctrl Pts',(-16.2037517912763,18.8218419315364,-18.1861403554451));
#39240=CARTESIAN_POINT('Ctrl Pts',(-16.216462269281,18.7392002832971,-18.190324989838));
#39241=CARTESIAN_POINT('Ctrl Pts',(-16.2332494562526,18.657028211755,-18.194509624231));
#39242=CARTESIAN_POINT('Ctrl Pts',(-16.2540667299568,18.5757591195989,-18.198694258624));
#39243=CARTESIAN_POINT('Ctrl Pts',(-16.2748543728486,18.4946057039363,-18.2028729367079));
#39244=CARTESIAN_POINT('Ctrl Pts',(-16.2996605951405,18.4143531565235,-18.2070516147918));
#39245=CARTESIAN_POINT('Ctrl Pts',(-16.3283873371772,18.3354272066433,-18.2112302928757));
#39246=CARTESIAN_POINT('Ctrl Pts',(-16.3576289854198,18.2550865658331,-18.2154838707611));
#39247=CARTESIAN_POINT('Ctrl Pts',(-16.3909330131971,18.1761210253964,-18.2197374486466));
#39248=CARTESIAN_POINT('Ctrl Pts',(-16.4281421038534,18.0989661143749,-18.223991026532));
#39249=CARTESIAN_POINT('Ctrl Pts',(-16.4646298236791,18.0233070018604,-18.2281621405099));
#39250=CARTESIAN_POINT('Ctrl Pts',(-16.5048723340166,17.9493893735374,-18.2323332544878));
#39251=CARTESIAN_POINT('Ctrl Pts',(-16.5486724780851,17.8776044765483,-18.2365043684657));
#39252=CARTESIAN_POINT('Ctrl Pts',(-16.5924579245922,17.8058436676747,-18.240674082786));
#39253=CARTESIAN_POINT('Ctrl Pts',(-16.6397983945156,17.7362145612029,-18.2448437971064));
#39254=CARTESIAN_POINT('Ctrl Pts',(-16.6904515225,17.6690824859586,-18.2490135114267));
#39255=CARTESIAN_POINT('Ctrl Pts',(-16.7411028480287,17.6019527995617,-18.2531830773707));
#39256=CARTESIAN_POINT('Ctrl Pts',(-16.7950663194821,17.5373203344385,-18.2573526433147));
#39257=CARTESIAN_POINT('Ctrl Pts',(-16.8520579335329,17.4755190699805,-18.2615222092586));
#39258=CARTESIAN_POINT('Ctrl Pts',(-16.9110533024286,17.4115449493023,-18.2658383719976));
#39259=CARTESIAN_POINT('Ctrl Pts',(-16.9732933572886,17.3506052113062,-18.2701545347366));
#39260=CARTESIAN_POINT('Ctrl Pts',(-17.0384212094895,17.2930290499668,-18.2744706974756));
#39261=CARTESIAN_POINT('Ctrl Pts',(-17.1014275287535,17.2373284260287,-18.2786462616672));
#39262=CARTESIAN_POINT('Ctrl Pts',(-17.167135997239,17.1847758643076,-18.2828218258589));
#39263=CARTESIAN_POINT('Ctrl Pts',(-17.2351909645112,17.1356273888438,-18.2869973900505));
#39264=CARTESIAN_POINT('Ctrl Pts',(-17.3066832263981,17.0839965407216,-18.2913838520632));
#39265=CARTESIAN_POINT('Ctrl Pts',(-17.3807647695955,17.0361230139113,-18.2957703140758));
#39266=CARTESIAN_POINT('Ctrl Pts',(-17.4569923995306,16.9922499941761,-18.3001567760885));
#39267=CARTESIAN_POINT('Ctrl Pts',(-17.5332200294657,16.948376974441,-18.3045432381012));
#39268=CARTESIAN_POINT('Ctrl Pts',(-17.6115931945082,16.9085046570798,-18.3089297001138));
#39269=CARTESIAN_POINT('Ctrl Pts',(-17.6916449845519,16.8728177954295,-18.3133161621265));
#39270=CARTESIAN_POINT('Ctrl Pts',(-17.7680134730662,16.8387729391863,-18.3175007965194));
#39271=CARTESIAN_POINT('Ctrl Pts',(-17.8461937671331,16.8084101229908,-18.3216854309124));
#39272=CARTESIAN_POINT('Ctrl Pts',(-17.9257962079479,16.7819247375776,-18.3258700653053));
#39273=CARTESIAN_POINT('Ctrl Pts',(-18.0052853445408,16.7554770508323,-18.3300487433892));
#39274=CARTESIAN_POINT('Ctrl Pts',(-18.0861921743122,16.7328959763057,-18.334227421473));
#39275=CARTESIAN_POINT('Ctrl Pts',(-18.1681056484765,16.714329500532,-18.3384060995568));
#39276=CARTESIAN_POINT('Ctrl Pts',(-18.2514873627979,16.6954302340229,-18.3426596774423));
#39277=CARTESIAN_POINT('Ctrl Pts',(-18.3359117243126,16.6806911015683,-18.3469132553277));
#39278=CARTESIAN_POINT('Ctrl Pts',(-18.4209273694984,16.6702155683666,-18.3511668332132));
#39279=CARTESIAN_POINT('Ctrl Pts',(-18.5042948205052,16.6599431238176,-18.355337947191));
#39280=CARTESIAN_POINT('Ctrl Pts',(-18.5882303557915,16.6537704962434,-18.3595090611689));
#39281=CARTESIAN_POINT('Ctrl Pts',(-18.6722982812007,16.6517436826497,-18.3636801751467));
#39282=CARTESIAN_POINT('Ctrl Pts',(-18.7563379968057,16.649717549173,-18.367849889467));
#39283=CARTESIAN_POINT('Ctrl Pts',(-18.8405095547889,16.6518344778738,-18.3720196037873));
#39284=CARTESIAN_POINT('Ctrl Pts',(-18.9243745836524,16.6580884234077,-18.3761893181075));
#39285=CARTESIAN_POINT('Ctrl Pts',(-19.0082366282384,16.6643421463994,-18.3803588840515));
#39286=CARTESIAN_POINT('Ctrl Pts',(-19.0917917066962,16.6747325584671,-18.3845284499954));
#39287=CARTESIAN_POINT('Ctrl Pts',(-19.1746052695965,16.6892016344672,-18.3886980159393));
#39288=CARTESIAN_POINT('Ctrl Pts',(-19.2603304552117,16.7041794253309,-18.3930141786784));
#39289=CARTESIAN_POINT('Ctrl Pts',(-19.3452604921649,16.723527937402,-18.3973303414174));
#39290=CARTESIAN_POINT('Ctrl Pts',(-19.4289254033766,16.7471252702822,-18.4016465041565));
#39291=CARTESIAN_POINT('Ctrl Pts',(-19.5098649389009,16.7699539225245,-18.405822068348));
#39292=CARTESIAN_POINT('Ctrl Pts',(-19.5896200744158,16.796758641008,-18.4099976325396));
#39293=CARTESIAN_POINT('Ctrl Pts',(-19.667783027385,16.8273789609571,-18.4141731967312));
#39294=CARTESIAN_POINT('Ctrl Pts',(-19.7498938053008,16.8595458404767,-18.418559658744));
#39295=CARTESIAN_POINT('Ctrl Pts',(-19.8302467994661,16.8959236625789,-18.4229461207568));
#39296=CARTESIAN_POINT('Ctrl Pts',(-19.9083976363224,16.9362714026064,-18.4273325827696));
#39297=CARTESIAN_POINT('Ctrl Pts',(-19.9865484731787,16.9766191426339,-18.4317190447824));
#39298=CARTESIAN_POINT('Ctrl Pts',(-20.0624966899236,17.0209364424643,-18.4361055067951));
#39299=CARTESIAN_POINT('Ctrl Pts',(-20.1358342086536,17.0689307080656,-18.4404919688079));
#39300=CARTESIAN_POINT('Ctrl Pts',(-20.2057039471168,17.1146555545475,-18.4446710160258));
#39301=CARTESIAN_POINT('Ctrl Pts',(-20.2734659150699,17.1638887348098,-18.4488500632436));
#39302=CARTESIAN_POINT('Ctrl Pts',(-20.3387454860834,17.2164093339998,-18.4530291104615));
#39303=CARTESIAN_POINT('Ctrl Pts',(-20.4039320790894,17.2688551278475,-18.4572022054423));
#39304=CARTESIAN_POINT('Ctrl Pts',(-20.4666429412498,17.3245787540421,-18.461375300423));
#39305=CARTESIAN_POINT('Ctrl Pts',(-20.5265316718114,17.3833156165374,-18.4655483954038));
#39306=CARTESIAN_POINT('Ctrl Pts',(-20.5870226816091,17.4426431743496,-18.4697634576868));
#39307=CARTESIAN_POINT('Ctrl Pts',(-20.6446340707896,17.5050446643085,-18.4739785199699));
#39308=CARTESIAN_POINT('Ctrl Pts',(-20.6990425114803,17.5702050926228,-18.4781935822529));
#39309=CARTESIAN_POINT('Ctrl Pts',(-20.7528122887529,17.6346006473008,-18.4823591668069));
#39310=CARTESIAN_POINT('Ctrl Pts',(-20.8034536124378,17.701690347722,-18.4865247513609));
#39311=CARTESIAN_POINT('Ctrl Pts',(-20.8506921231952,17.7711338758054,-18.4906903359149));
#39312=CARTESIAN_POINT('Ctrl Pts',(-20.8979149500342,17.84055434756,-18.4948545374302));
#39313=CARTESIAN_POINT('Ctrl Pts',(-20.9417369482813,17.9123267137653,-18.4990187389455));
#39314=CARTESIAN_POINT('Ctrl Pts',(-20.9819260328715,17.9860801859964,-18.5031829404608));
#39315=CARTESIAN_POINT('Ctrl Pts',(-21.0221139173364,18.0598314558035,-18.5073470176248));
#39316=CARTESIAN_POINT('Ctrl Pts',(-21.0586688839109,18.1355633083682,-18.5115110947889));
#39317=CARTESIAN_POINT('Ctrl Pts',(-21.0914046022626,18.2128799965779,-18.5156751719529));
#39318=CARTESIAN_POINT('Ctrl Pts',(-21.1248385440613,18.2918457802491,-18.5199280651399));
#39319=CARTESIAN_POINT('Ctrl Pts',(-21.1542882228968,18.3724643312946,-18.5241809583268));
#39320=CARTESIAN_POINT('Ctrl Pts',(-21.1796074785073,18.4542939401135,-18.5284338515138));
#39321=CARTESIAN_POINT('Ctrl Pts',(-21.2044336791702,18.5345300386761,-18.5326039259141));
#39322=CARTESIAN_POINT('Ctrl Pts',(-21.2252888283686,18.6159299801768,-18.5367740003144));
#39323=CARTESIAN_POINT('Ctrl Pts',(-21.2420864983912,18.6980651926534,-18.5409440747148));
#39324=CARTESIAN_POINT('Ctrl Pts',(-21.2593845777047,18.7826472458753,-18.545238377295));
#39325=CARTESIAN_POINT('Ctrl Pts',(-21.2723795196075,18.8680085473307,-18.5495326798753));
#39326=CARTESIAN_POINT('Ctrl Pts',(-21.2810343673868,18.9536754357808,-18.5538269824556));
#39327=CARTESIAN_POINT('Ctrl Pts',(-21.2896892151661,19.0393423242309,-18.5581212850358));
#39328=CARTESIAN_POINT('Ctrl Pts',(-21.2940040128973,19.125314270194,-18.5624155876161));
#39329=CARTESIAN_POINT('Ctrl Pts',(-21.2939999971965,19.2111198080496,-18.5667098901964));
#39330=CARTESIAN_POINT('Origin',(-18.734,19.211,1.76670989022852));
#39331=CARTESIAN_POINT('',(-17.1762220931371,21.2388106152247,-17.2500265334082));
#39332=CARTESIAN_POINT('',(-17.1735447521835,21.2423105972199,-17.3168006939262));
#39333=CARTESIAN_POINT('',(-17.1744642439897,21.2411350264762,1.76670989022852));
#39334=CARTESIAN_POINT('',(-21.2939989159607,19.2086440968075,-17.8332901097715));
#39335=CARTESIAN_POINT('Ctrl Pts',(-17.1735447521834,21.2423105972199,-17.3168006939262));
#39336=CARTESIAN_POINT('Ctrl Pts',(-16.6213792194418,20.8094283882808,-17.3517574491069));
#39337=CARTESIAN_POINT('Ctrl Pts',(-15.7867860156331,19.3312717594939,-17.4291061398481));
#39338=CARTESIAN_POINT('Ctrl Pts',(-16.8703561089868,16.8256020863163,-17.5488467661498));
#39339=CARTESIAN_POINT('Ctrl Pts',(-19.7309870566021,16.3527997676692,-17.6760225728313));
#39340=CARTESIAN_POINT('Ctrl Pts',(-21.1817726888933,17.9552739588088,-17.7708370080137));
#39341=CARTESIAN_POINT('Ctrl Pts',(-21.2957665006941,19.0070072439541,-17.8232595076358));
#39342=CARTESIAN_POINT('Ctrl Pts',(-21.2939118038754,19.2086434116094,-17.8332900716974));
#39343=CARTESIAN_POINT('Ctrl Pts',(-21.2939989159607,19.2086440968075,-17.8332901097715));
#39344=CARTESIAN_POINT('Ctrl Pts',(-21.2940751741219,19.2915086264566,-17.837412174938));
#39345=CARTESIAN_POINT('Ctrl Pts',(-21.290123839502,19.3744847533444,-17.8415342401044));
#39346=CARTESIAN_POINT('Ctrl Pts',(-21.2821391268744,19.457144246514,-17.8456563052709));
#39347=CARTESIAN_POINT('Ctrl Pts',(-21.2741597741335,19.5397482529613,-17.8497756034244));
#39348=CARTESIAN_POINT('Ctrl Pts',(-21.262152459652,19.6220355783688,-17.8538949015779));
#39349=CARTESIAN_POINT('Ctrl Pts',(-21.2461634417033,19.7035797825424,-17.8580141997315));
#39350=CARTESIAN_POINT('Ctrl Pts',(-21.2301800733889,19.7850951735057,-17.862132042353));
#39351=CARTESIAN_POINT('Ctrl Pts',(-21.2102178848107,19.8658675009386,-17.8662498849744));
#39352=CARTESIAN_POINT('Ctrl Pts',(-21.1863745538874,19.9454787590158,-17.8703677275959));
#39353=CARTESIAN_POINT('Ctrl Pts',(-21.1625320679642,20.0250871956953,-17.8744854242823));
#39354=CARTESIAN_POINT('Ctrl Pts',(-21.1348088500427,20.1035341923717,-17.8786031209688));
#39355=CARTESIAN_POINT('Ctrl Pts',(-21.1033525053491,20.1804166830605,-17.8827208176552));
#39356=CARTESIAN_POINT('Ctrl Pts',(-21.0718661219911,20.2573725912857,-17.8868424464612));
#39357=CARTESIAN_POINT('Ctrl Pts',(-21.0366396717685,20.3327605713694,-17.8909640752672));
#39358=CARTESIAN_POINT('Ctrl Pts',(-20.9978687619912,20.4061979871471,-17.8950857040732));
#39359=CARTESIAN_POINT('Ctrl Pts',(-20.9590794967267,20.4796701707327,-17.8992092842006));
#39360=CARTESIAN_POINT('Ctrl Pts',(-20.9167426732501,20.551189545137,-17.9033328643279));
#39361=CARTESIAN_POINT('Ctrl Pts',(-20.8710983794445,20.6204007650685,-17.9074564444553));
#39362=CARTESIAN_POINT('Ctrl Pts',(-20.8253741239694,20.6897332322411,-17.9115872484506));
#39363=CARTESIAN_POINT('Ctrl Pts',(-20.7763311058832,20.7567490876314,-17.9157180524459));
#39364=CARTESIAN_POINT('Ctrl Pts',(-20.7242507920073,20.8211247730888,-17.9198488564413));
#39365=CARTESIAN_POINT('Ctrl Pts',(-20.6800170723896,20.8758014024867,-17.9233572996922));
#39366=CARTESIAN_POINT('Ctrl Pts',(-20.6335931281538,20.9285739549631,-17.9268657429431));
#39367=CARTESIAN_POINT('Ctrl Pts',(-20.5851713910723,20.9792659530951,-17.9303741861941));
#39368=CARTESIAN_POINT('Ctrl Pts',(-20.5274172101246,21.0397279482481,-17.9345588205871));
#39369=CARTESIAN_POINT('Ctrl Pts',(-20.4665902688467,21.0974699797564,-17.9387434549801));
#39370=CARTESIAN_POINT('Ctrl Pts',(-20.4029770272298,21.1521634868241,-17.9429280893731));
#39371=CARTESIAN_POINT('Ctrl Pts',(-20.3394543311886,21.2067791444542,-17.947106767457));
#39372=CARTESIAN_POINT('Ctrl Pts',(-20.2731535582846,21.2583545993042,-17.9512854455408));
#39373=CARTESIAN_POINT('Ctrl Pts',(-20.2043989371767,21.3065970427421,-17.9554641236247));
#39374=CARTESIAN_POINT('Ctrl Pts',(-20.1344119388974,21.3557041973082,-17.9597177015102));
#39375=CARTESIAN_POINT('Ctrl Pts',(-20.0618825897101,21.4013573280785,-17.9639712793956));
#39376=CARTESIAN_POINT('Ctrl Pts',(-19.9871893049689,21.4432895345164,-17.9682248572811));
#39377=CARTESIAN_POINT('Ctrl Pts',(-19.9139440953056,21.4844088033079,-17.972395971259));
#39378=CARTESIAN_POINT('Ctrl Pts',(-19.8386185251855,21.5219498994727,-17.9765670852369));
#39379=CARTESIAN_POINT('Ctrl Pts',(-19.7615983036838,21.555705040355,-17.9807381992148));
#39380=CARTESIAN_POINT('Ctrl Pts',(-19.6846039270612,21.5894488543738,-17.9849079135351));
#39381=CARTESIAN_POINT('Ctrl Pts',(-19.6059164494116,21.619409051666,-17.9890776278554));
#39382=CARTESIAN_POINT('Ctrl Pts',(-19.5259437923522,21.6454249895519,-17.9932473421757));
#39383=CARTESIAN_POINT('Ctrl Pts',(-19.4459739810633,21.6714400016791,-17.9974169081197));
#39384=CARTESIAN_POINT('Ctrl Pts',(-19.3647195190225,21.6935108919569,-18.0015864740637));
#39385=CARTESIAN_POINT('Ctrl Pts',(-19.2826045027058,21.7115265644681,-18.0057560400077));
#39386=CARTESIAN_POINT('Ctrl Pts',(-19.1976024237129,21.7301756458007,-18.0100722027467));
#39387=CARTESIAN_POINT('Ctrl Pts',(-19.1116786655147,21.7444789277004,-18.0143883654857));
#39388=CARTESIAN_POINT('Ctrl Pts',(-19.0253143284886,21.7543709839536,-18.0187045282247));
#39389=CARTESIAN_POINT('Ctrl Pts',(-18.9417633006594,21.7639408075146,-18.0228800924163));
#39390=CARTESIAN_POINT('Ctrl Pts',(-18.857800430025,21.7693824000208,-18.0270556566079));
#39391=CARTESIAN_POINT('Ctrl Pts',(-18.7738638919265,21.7706896042529,-18.0312312207996));
#39392=CARTESIAN_POINT('Ctrl Pts',(-18.6856879188254,21.7720628322632,-18.0356176828122));
#39393=CARTESIAN_POINT('Ctrl Pts',(-18.5975415917828,21.7688730610124,-18.0400041448249));
#39394=CARTESIAN_POINT('Ctrl Pts',(-18.5099274935593,21.7611748002553,-18.0443906068375));
#39395=CARTESIAN_POINT('Ctrl Pts',(-18.4223133953359,21.7534765394983,-18.0487770688502));
#39396=CARTESIAN_POINT('Ctrl Pts',(-18.3352320899719,21.7412699451077,-18.0531635308629));
#39397=CARTESIAN_POINT('Ctrl Pts',(-18.2491721313432,21.7246710082613,-18.0575499928755));
#39398=CARTESIAN_POINT('Ctrl Pts',(-18.167067998592,21.7088350569539,-18.0617348270903));
#39399=CARTESIAN_POINT('Ctrl Pts',(-18.0855877575544,21.6889427479729,-18.0659196613052));
#39400=CARTESIAN_POINT('Ctrl Pts',(-18.005162792895,21.6650571153784,-18.07010449552));
#39401=CARTESIAN_POINT('Ctrl Pts',(-17.9248712290094,21.6412111018485,-18.0742823883563));
#39402=CARTESIAN_POINT('Ctrl Pts',(-17.8456318987017,21.6133850633005,-18.0784602811926));
#39403=CARTESIAN_POINT('Ctrl Pts',(-17.7678662694045,21.5816930663006,-18.0826381740289));
#39404=CARTESIAN_POINT('Ctrl Pts',(-17.6901757082992,21.5500316620051,-18.0868120338899));
#39405=CARTESIAN_POINT('Ctrl Pts',(-17.6139564476223,21.5145118802857,-18.0909858937509));
#39406=CARTESIAN_POINT('Ctrl Pts',(-17.5396142320322,21.4752973826942,-18.0951597536119));
#39407=CARTESIAN_POINT('Ctrl Pts',(-17.4653211999168,21.4361088287101,-18.0993308521222));
#39408=CARTESIAN_POINT('Ctrl Pts',(-17.3929031526805,21.3932306267404,-18.1035019506325));
#39409=CARTESIAN_POINT('Ctrl Pts',(-17.3227440412582,21.346873736651,-18.1076730491428));
#39410=CARTESIAN_POINT('Ctrl Pts',(-17.2720953304333,21.3134081371975,-18.1106842155898));
#39411=CARTESIAN_POINT('Ctrl Pts',(-17.2226234583587,21.2781306035241,-18.1136953820369));
#39412=CARTESIAN_POINT('Ctrl Pts',(-17.1744642439897,21.2411350264762,-18.1167065484839));
#39413=CARTESIAN_POINT('',(-21.2939990418858,19.2132148462352,-17.7667099127482));
#39414=CARTESIAN_POINT('Ctrl Pts',(-21.2939990418858,19.2132148462352,-17.7667099127482));
#39415=CARTESIAN_POINT('Ctrl Pts',(-21.2939112972768,19.3146332252686,-17.7717442924635));
#39416=CARTESIAN_POINT('Ctrl Pts',(-21.2877929815477,19.415787678657,-17.7767786721789));
#39417=CARTESIAN_POINT('Ctrl Pts',(-21.2757605528227,19.5160463769891,-17.7818130518942));
#39418=CARTESIAN_POINT('Ctrl Pts',(-21.2635573150943,19.6177283198494,-17.7869188982603));
#39419=CARTESIAN_POINT('Ctrl Pts',(-21.245270932932,19.7184889031551,-17.7920247446265));
#39420=CARTESIAN_POINT('Ctrl Pts',(-21.2210717431444,19.8176911442014,-17.7971305909926));
#39421=CARTESIAN_POINT('Ctrl Pts',(-21.2092508709255,19.866149668042,-17.7996247057953));
#39422=CARTESIAN_POINT('Ctrl Pts',(-21.1960198419246,19.9142366801055,-17.8021188205981));
#39423=CARTESIAN_POINT('Ctrl Pts',(-21.1814026084241,19.9618797988219,-17.8046129354008));
#39424=CARTESIAN_POINT('Ctrl Pts',(-21.1568777637899,20.0418155872439,-17.8087975697939));
#39425=CARTESIAN_POINT('Ctrl Pts',(-21.1283869296254,20.1206973427815,-17.8129822041869));
#39426=CARTESIAN_POINT('Ctrl Pts',(-21.0960388974778,20.1981029565359,-17.8171668385799));
#39427=CARTESIAN_POINT('Ctrl Pts',(-21.0637369087501,20.27539839298,-17.8213455166639));
#39428=CARTESIAN_POINT('Ctrl Pts',(-21.0275888032569,20.3512214402681,-17.8255241947478));
#39429=CARTESIAN_POINT('Ctrl Pts',(-20.9877531601769,20.4251650188473,-17.8297028728318));
#39430=CARTESIAN_POINT('Ctrl Pts',(-20.947203491824,20.5004339829303,-17.8339564507172));
#39431=CARTESIAN_POINT('Ctrl Pts',(-20.9028329287837,20.5737549756818,-17.8382100286026));
#39432=CARTESIAN_POINT('Ctrl Pts',(-20.8548601014715,20.6447197878198,-17.8424636064881));
#39433=CARTESIAN_POINT('Ctrl Pts',(-20.8078173210281,20.714308808598,-17.846634720466));
#39434=CARTESIAN_POINT('Ctrl Pts',(-20.7573109732373,20.7816317931437,-17.850805834444));
#39435=CARTESIAN_POINT('Ctrl Pts',(-20.7035927080245,20.8463301087233,-17.8549769484219));
#39436=CARTESIAN_POINT('Ctrl Pts',(-20.6498924684943,20.9110067141582,-17.8591466627423));
#39437=CARTESIAN_POINT('Ctrl Pts',(-20.5929827456749,20.9730600461347,-17.8633163770627));
#39438=CARTESIAN_POINT('Ctrl Pts',(-20.5331561759619,21.0321636539581,-17.867486091383));
#39439=CARTESIAN_POINT('Ctrl Pts',(-20.4733317351351,21.0912651586215,-17.8716556573271));
#39440=CARTESIAN_POINT('Ctrl Pts',(-20.4105909816462,21.147416825124,-17.8758252232711));
#39441=CARTESIAN_POINT('Ctrl Pts',(-20.345263220069,21.2003292426476,-17.8799947892152));
#39442=CARTESIAN_POINT('Ctrl Pts',(-20.2776386149851,21.2551019954969,-17.8843109519541));
#39443=CARTESIAN_POINT('Ctrl Pts',(-20.2072421084911,21.3064031452814,-17.888627114693));
#39444=CARTESIAN_POINT('Ctrl Pts',(-20.134474432863,21.3539585537049,-17.8929432774319));
#39445=CARTESIAN_POINT('Ctrl Pts',(-20.0640771566147,21.3999648497009,-17.8971188416236));
#39446=CARTESIAN_POINT('Ctrl Pts',(-19.9914612509378,21.4424654946024,-17.9012944058153));
#39447=CARTESIAN_POINT('Ctrl Pts',(-19.9170156443951,21.4812585723032,-17.905469970007));
#39448=CARTESIAN_POINT('Ctrl Pts',(-19.8388099672434,21.5220109961371,-17.9098564320195));
#39449=CARTESIAN_POINT('Ctrl Pts',(-19.7585854263164,21.5586712286021,-17.9142428940321));
#39450=CARTESIAN_POINT('Ctrl Pts',(-19.6768157184723,21.5910627136699,-17.9186293560446));
#39451=CARTESIAN_POINT('Ctrl Pts',(-19.5950460106282,21.6234541987377,-17.9230158180572));
#39452=CARTESIAN_POINT('Ctrl Pts',(-19.5117317099373,21.6515768229132,-17.9274022800697));
#39453=CARTESIAN_POINT('Ctrl Pts',(-19.427361531773,21.6753152773656,-17.9317887420823));
#39454=CARTESIAN_POINT('Ctrl Pts',(-19.3468694922151,21.69796257593,-17.9359735770739));
#39455=CARTESIAN_POINT('Ctrl Pts',(-19.2651168916007,21.7167042021081,-17.9401584120656));
#39456=CARTESIAN_POINT('Ctrl Pts',(-19.1825176034779,21.7314031342963,-17.9443432470572));
#39457=CARTESIAN_POINT('Ctrl Pts',(-19.1000369486759,21.7460809551264,-17.9485220715749));
#39458=CARTESIAN_POINT('Ctrl Pts',(-19.0167124711172,21.756727535891,-17.9527008960926));
#39459=CARTESIAN_POINT('Ctrl Pts',(-18.9329723420235,21.7632558663092,-17.9568797206103));
#39460=CARTESIAN_POINT('Ctrl Pts',(-18.8493333890532,21.7697763090973,-17.9610534962073));
#39461=CARTESIAN_POINT('Ctrl Pts',(-18.7652802392241,21.7721883584653,-17.9652272718043));
#39462=CARTESIAN_POINT('Ctrl Pts',(-18.6812489272003,21.7704564509517,-17.9694010474014));
#39463=CARTESIAN_POINT('Ctrl Pts',(-18.5972730476195,21.7687256859154,-17.9735720697083));
#39464=CARTESIAN_POINT('Ctrl Pts',(-18.5133194358117,21.7628564016069,-17.9777430920153));
#39465=CARTESIAN_POINT('Ctrl Pts',(-18.4298258472869,21.7528650799799,-17.9819141143222));
#39466=CARTESIAN_POINT('Ctrl Pts',(-18.3463622898504,21.7428773520452,-17.9860836363902));
#39467=CARTESIAN_POINT('Ctrl Pts',(-18.2633588832453,21.7287705870398,-17.9902531584581));
#39468=CARTESIAN_POINT('Ctrl Pts',(-18.1812486084931,21.7106131499068,-17.9944226805261));
#39469=CARTESIAN_POINT('Ctrl Pts',(-18.0991432365396,21.6924567969531,-17.9985919536321));
#39470=CARTESIAN_POINT('Ctrl Pts',(-18.0179313390517,21.6702503538478,-18.0027612267382));
#39471=CARTESIAN_POINT('Ctrl Pts',(-17.9380347007106,21.6441130763545,-18.0069304998443));
#39472=CARTESIAN_POINT('Ctrl Pts',(-17.8580775669164,21.6179560084609,-18.0111029298049));
#39473=CARTESIAN_POINT('Ctrl Pts',(-17.7794381185932,21.5878623064786,-18.0152753597655));
#39474=CARTESIAN_POINT('Ctrl Pts',(-17.7025213244531,21.5540005851241,-18.0194477897261));
#39475=CARTESIAN_POINT('Ctrl Pts',(-17.6255715835556,21.520124359344,-18.0236220069172));
#39476=CARTESIAN_POINT('Ctrl Pts',(-17.5503463788393,21.482477103769,-18.0277962241083));
#39477=CARTESIAN_POINT('Ctrl Pts',(-17.477227106474,21.4412739504595,-18.0319704412993));
#39478=CARTESIAN_POINT('Ctrl Pts',(-17.4040091462788,21.4000151859594,-18.0361502923599));
#39479=CARTESIAN_POINT('Ctrl Pts',(-17.3329031825643,21.3551911865764,-18.0403301434204));
#39480=CARTESIAN_POINT('Ctrl Pts',(-17.2642621217254,21.3070607264974,-18.044509994481));
#39481=CARTESIAN_POINT('Ctrl Pts',(-17.2338360925851,21.2857262837746,-18.046362766985));
#39482=CARTESIAN_POINT('Ctrl Pts',(-17.2038939434596,21.2637427190746,-18.048215539489));
#39483=CARTESIAN_POINT('Ctrl Pts',(-17.1744642439897,21.2411350264762,-18.0500683119931));
#39484=CARTESIAN_POINT('Ctrl Pts',(-17.1762220931372,21.2388106152247,-17.2500265334081));
#39485=CARTESIAN_POINT('Ctrl Pts',(-16.9304195186111,21.0526898980001,-17.2653209251638));
#39486=CARTESIAN_POINT('Ctrl Pts',(-16.1279939956761,20.1920438763241,-17.3230072524799));
#39487=CARTESIAN_POINT('Ctrl Pts',(-15.9988187087053,17.9140516790705,-17.4230855153565));
#39488=CARTESIAN_POINT('Ctrl Pts',(-18.3440265352185,16.209131858296,-17.5502613220379));
#39489=CARTESIAN_POINT('Ctrl Pts',(-20.7784813956588,17.1540155580924,-17.6648027803286));
#39490=CARTESIAN_POINT('Ctrl Pts',(-21.2874613721703,18.6141143669069,-17.7369523030588));
#39491=CARTESIAN_POINT('Ctrl Pts',(-21.2923873719166,19.2132129984815,-17.7667098902285));
#39492=CARTESIAN_POINT('Origin',(-18.734,19.211,1.76670989022852));
#39493=CARTESIAN_POINT('',(-17.1744642439897,21.2411350264762,-16.4501666835217));
#39494=CARTESIAN_POINT('',(-17.1744642439897,21.2411350264762,-16.5166303489465));
#39495=CARTESIAN_POINT('',(-17.1744642439897,21.2411350264762,1.76670989022852));
#39496=CARTESIAN_POINT('',(-21.2942631180427,19.2118355653576,-17.0332901097715));
#39497=CARTESIAN_POINT('Ctrl Pts',(-17.1744642439897,21.2411350264762,-16.5166303489465));
#39498=CARTESIAN_POINT('Ctrl Pts',(-17.1078975357866,21.1899989393446,-16.5208151793057));
#39499=CARTESIAN_POINT('Ctrl Pts',(-17.0439434920722,21.1356584139567,-16.5250000096648));
#39500=CARTESIAN_POINT('Ctrl Pts',(-16.982907842272,21.0784250333396,-16.5291848400239));
#39501=CARTESIAN_POINT('Ctrl Pts',(-16.9719425040963,21.0681427904953,-16.5299366642487));
#39502=CARTESIAN_POINT('Ctrl Pts',(-16.961071256108,21.0577672665176,-16.5306884884735));
#39503=CARTESIAN_POINT('Ctrl Pts',(-16.9502957329767,21.047300380603,-16.5314403126983));
#39504=CARTESIAN_POINT('Ctrl Pts',(-16.8903194470162,20.9890419614915,-16.5356249470914));
#39505=CARTESIAN_POINT('Ctrl Pts',(-16.8330887583091,20.9277336646777,-16.5398095814844));
#39506=CARTESIAN_POINT('Ctrl Pts',(-16.7789298175349,20.8636646912292,-16.5439942158775));
#39507=CARTESIAN_POINT('Ctrl Pts',(-16.7248479653093,20.7996869120342,-16.5481728939614));
#39508=CARTESIAN_POINT('Ctrl Pts',(-16.6738294707906,20.7329566097132,-16.5523515720454));
#39509=CARTESIAN_POINT('Ctrl Pts',(-16.6261644175017,20.6638004533156,-16.5565302501293));
#39510=CARTESIAN_POINT('Ctrl Pts',(-16.577645002389,20.5934047225164,-16.5607838280147));
#39511=CARTESIAN_POINT('Ctrl Pts',(-16.5326007777018,20.520495651305,-16.5650374059002));
#39512=CARTESIAN_POINT('Ctrl Pts',(-16.4912954660574,20.4454538765921,-16.5692909837856));
#39513=CARTESIAN_POINT('Ctrl Pts',(-16.4507909384799,20.3718669331139,-16.5734620977636));
#39514=CARTESIAN_POINT('Ctrl Pts',(-16.4138818774498,20.2962296630071,-16.5776332117415));
#39515=CARTESIAN_POINT('Ctrl Pts',(-16.3807728287042,20.2189295016394,-16.5818043257195));
#39516=CARTESIAN_POINT('Ctrl Pts',(-16.3476748900196,20.1416552790873,-16.5859740400399));
#39517=CARTESIAN_POINT('Ctrl Pts',(-16.3183746121639,20.0627196959935,-16.5901437543602));
#39518=CARTESIAN_POINT('Ctrl Pts',(-16.2930292165598,19.9825320047744,-16.5943134686806));
#39519=CARTESIAN_POINT('Ctrl Pts',(-16.2676847228536,19.9023471669775,-16.5984830346247));
#39520=CARTESIAN_POINT('Ctrl Pts',(-16.2462949694201,19.820910748543,-16.6026526005687));
#39521=CARTESIAN_POINT('Ctrl Pts',(-16.2289674972205,19.7386477613126,-16.6068221665128));
#39522=CARTESIAN_POINT('Ctrl Pts',(-16.2110308124741,19.6534925089336,-16.6111383292517));
#39523=CARTESIAN_POINT('Ctrl Pts',(-16.1974474922546,19.5674519980823,-16.6154544919906));
#39524=CARTESIAN_POINT('Ctrl Pts',(-16.1882789321129,19.4810078600997,-16.6197706547295));
#39525=CARTESIAN_POINT('Ctrl Pts',(-16.1794090368535,19.3973796308195,-16.6239462189212));
#39526=CARTESIAN_POINT('Ctrl Pts',(-16.1746706763875,19.3133741398416,-16.6281217831129));
#39527=CARTESIAN_POINT('Ctrl Pts',(-16.1740663387713,19.2294295987024,-16.6322973473046));
#39528=CARTESIAN_POINT('Ctrl Pts',(-16.1734314774988,19.1412452183496,-16.6366838093171));
#39529=CARTESIAN_POINT('Ctrl Pts',(-16.1773592072922,19.0531286901045,-16.6410702713296));
#39530=CARTESIAN_POINT('Ctrl Pts',(-16.1857908120614,18.965582122686,-16.6454567333422));
#39531=CARTESIAN_POINT('Ctrl Pts',(-16.1942224168306,18.8780355552674,-16.6498431953547));
#39532=CARTESIAN_POINT('Ctrl Pts',(-16.2071577359856,18.7910595113906,-16.6542296573673));
#39533=CARTESIAN_POINT('Ctrl Pts',(-16.2244766916358,18.7051415565825,-16.6586161193798));
#39534=CARTESIAN_POINT('Ctrl Pts',(-16.2409987764637,18.6231768142361,-16.6628007537728));
#39535=CARTESIAN_POINT('Ctrl Pts',(-16.2615714655045,18.5418698437248,-16.6669853881659));
#39536=CARTESIAN_POINT('Ctrl Pts',(-16.2861281256042,18.4616514252084,-16.6711700225589));
#39537=CARTESIAN_POINT('Ctrl Pts',(-16.3106498323378,18.3815471876818,-16.6753487006429));
#39538=CARTESIAN_POINT('Ctrl Pts',(-16.3391441128498,18.3025288606374,-16.6795273787268));
#39539=CARTESIAN_POINT('Ctrl Pts',(-16.3714933068751,18.225017178172,-16.6837060568108));
#39540=CARTESIAN_POINT('Ctrl Pts',(-16.4044223369543,18.1461161545051,-16.6879596346962));
#39541=CARTESIAN_POINT('Ctrl Pts',(-16.4413457432405,18.0687767925294,-16.6922132125816));
#39542=CARTESIAN_POINT('Ctrl Pts',(-16.4820862183798,17.9934268727714,-16.6964667904671));
#39543=CARTESIAN_POINT('Ctrl Pts',(-16.5220368599101,17.9195377582413,-16.700637904445));
#39544=CARTESIAN_POINT('Ctrl Pts',(-16.5656576595125,17.8475620591661,-16.704809018423));
#39545=CARTESIAN_POINT('Ctrl Pts',(-16.6127335620837,17.7778814775568,-16.7089801324009));
#39546=CARTESIAN_POINT('Ctrl Pts',(-16.6597936678812,17.7082242779395,-16.7131498467213));
#39547=CARTESIAN_POINT('Ctrl Pts',(-16.7103063167567,17.6408610471355,-16.7173195610417));
#39548=CARTESIAN_POINT('Ctrl Pts',(-16.7640124931676,17.5761455040512,-16.721489275362));
#39549=CARTESIAN_POINT('Ctrl Pts',(-16.8177167584822,17.5114322638236,-16.7256588413061));
#39550=CARTESIAN_POINT('Ctrl Pts',(-16.8746140309481,17.4493668774532,-16.7298284072501));
#39551=CARTESIAN_POINT('Ctrl Pts',(-16.9344051527487,17.3902698207185,-16.7339979731942));
#39552=CARTESIAN_POINT('Ctrl Pts',(-16.9962984566316,17.3290949843729,-16.7383141359331));
#39553=CARTESIAN_POINT('Ctrl Pts',(-17.0612925164448,17.2711014650387,-16.742630298672));
#39554=CARTESIAN_POINT('Ctrl Pts',(-17.1290155886976,17.2166015845683,-16.7469464614109));
#39555=CARTESIAN_POINT('Ctrl Pts',(-17.194532588995,17.163877031972,-16.7511220256026));
#39556=CARTESIAN_POINT('Ctrl Pts',(-17.2626031281001,17.1144222417058,-16.7552975897943));
#39557=CARTESIAN_POINT('Ctrl Pts',(-17.3328600861969,17.0684765014246,-16.759473153986));
#39558=CARTESIAN_POINT('Ctrl Pts',(-17.4066655562273,17.0202101510273,-16.7638596159985));
#39559=CARTESIAN_POINT('Ctrl Pts',(-17.4828836173806,16.9758169447298,-16.7682460780111));
#39560=CARTESIAN_POINT('Ctrl Pts',(-17.5610602937787,16.9355192935185,-16.7726325400236));
#39561=CARTESIAN_POINT('Ctrl Pts',(-17.6392369701768,16.8952216423073,-16.7770190020362));
#39562=CARTESIAN_POINT('Ctrl Pts',(-17.7193717017408,16.8590197157385,-16.7814054640487));
#39563=CARTESIAN_POINT('Ctrl Pts',(-17.800989527137,16.8270764572814,-16.7857919260613));
#39564=CARTESIAN_POINT('Ctrl Pts',(-17.8788519953999,16.7966029554973,-16.7899765604543));
#39565=CARTESIAN_POINT('Ctrl Pts',(-17.9583538968788,16.7698914102528,-16.7941611948474));
#39566=CARTESIAN_POINT('Ctrl Pts',(-18.0390969463692,16.7471189667408,-16.7983458292404));
#39567=CARTESIAN_POINT('Ctrl Pts',(-18.1197250681227,16.7243789369834,-16.8025245073243));
#39568=CARTESIAN_POINT('Ctrl Pts',(-18.2015903898501,16.7055669958483,-16.8067031854083));
#39569=CARTESIAN_POINT('Ctrl Pts',(-18.2842754534886,16.6908119450594,-16.8108818634922));
#39570=CARTESIAN_POINT('Ctrl Pts',(-18.3684425874682,16.6757924205895,-16.8151354413777));
#39571=CARTESIAN_POINT('Ctrl Pts',(-18.4534586911852,16.66497683224,-16.8193890192631));
#39572=CARTESIAN_POINT('Ctrl Pts',(-18.5388680958069,16.6584476420716,-16.8236425971485));
#39573=CARTESIAN_POINT('Ctrl Pts',(-18.6226216724573,16.6520450329952,-16.8278137111265));
#39574=CARTESIAN_POINT('Ctrl Pts',(-18.7067529564691,16.6497641415373,-16.8319848251044));
#39575=CARTESIAN_POINT('Ctrl Pts',(-18.7908245916081,16.6516307484483,-16.8361559390824));
#39576=CARTESIAN_POINT('Ctrl Pts',(-18.874868015698,16.6534967290012,-16.8403256534027));
#39577=CARTESIAN_POINT('Ctrl Pts',(-18.95885137113,16.659507433716,-16.8444953677231));
#39578=CARTESIAN_POINT('Ctrl Pts',(-19.0423370360802,16.6696365328467,-16.8486650820435));
#39579=CARTESIAN_POINT('Ctrl Pts',(-19.1258197302521,16.6797652715406,-16.8528346479875));
#39580=CARTESIAN_POINT('Ctrl Pts',(-19.2088043125729,16.6940120570168,-16.8570042139316));
#39581=CARTESIAN_POINT('Ctrl Pts',(-19.2908593851772,16.7122988123547,-16.8611737798756));
#39582=CARTESIAN_POINT('Ctrl Pts',(-19.3757994129083,16.7312285074512,-16.8654899426145));
#39583=CARTESIAN_POINT('Ctrl Pts',(-19.4597428368619,16.7544874341396,-16.8698061053534));
#39584=CARTESIAN_POINT('Ctrl Pts',(-19.542225826085,16.781932068869,-16.8741222680924));
#39585=CARTESIAN_POINT('Ctrl Pts',(-19.62202194061,16.8084826975088,-16.878297832284));
#39586=CARTESIAN_POINT('Ctrl Pts',(-19.7004508845913,16.838950308513,-16.8824733964757));
#39587=CARTESIAN_POINT('Ctrl Pts',(-19.777112739986,16.8731557340834,-16.8866489606674));
#39588=CARTESIAN_POINT('Ctrl Pts',(-19.8576466034503,16.9090887943838,-16.8910354226799));
#39589=CARTESIAN_POINT('Ctrl Pts',(-19.9362296554815,16.9491469214587,-16.8954218846925));
#39590=CARTESIAN_POINT('Ctrl Pts',(-20.0124291551047,16.9930687802869,-16.899808346705));
#39591=CARTESIAN_POINT('Ctrl Pts',(-20.088628654728,17.036990639115,-16.9041948087175));
#39592=CARTESIAN_POINT('Ctrl Pts',(-20.1624441562133,17.0847758505361,-16.9085812707301));
#39593=CARTESIAN_POINT('Ctrl Pts',(-20.2334815623277,17.1361132454422,-16.9129677327426));
#39594=CARTESIAN_POINT('Ctrl Pts',(-20.3007008312569,17.1846913445463,-16.9171184300414));
#39595=CARTESIAN_POINT('Ctrl Pts',(-20.3656920487853,17.2366370916662,-16.9212691273401));
#39596=CARTESIAN_POINT('Ctrl Pts',(-20.4280939407347,17.2917173944502,-16.9254198246388));
#39597=CARTESIAN_POINT('Ctrl Pts',(-20.4904067758308,17.3467190893862,-16.9295645982704));
#39598=CARTESIAN_POINT('Ctrl Pts',(-20.5501372744549,17.4048461509353,-16.9337093719019));
#39599=CARTESIAN_POINT('Ctrl Pts',(-20.6069541187605,17.4658229691467,-16.9378541455335));
#39600=CARTESIAN_POINT('Ctrl Pts',(-20.6637057912848,17.5267298438773,-16.9419941649009));
#39601=CARTESIAN_POINT('Ctrl Pts',(-20.7175501324578,17.5904796396565,-16.9461341842684));
#39602=CARTESIAN_POINT('Ctrl Pts',(-20.7681909845745,17.6567583719782,-16.9502742036359));
#39603=CARTESIAN_POINT('Ctrl Pts',(-20.8188004163149,17.7229959813208,-16.9544116543072));
#39604=CARTESIAN_POINT('Ctrl Pts',(-20.8662100198437,17.7917590422704,-16.9585491049784));
#39605=CARTESIAN_POINT('Ctrl Pts',(-20.9101632231195,17.8626997269368,-16.9626865556497));
#39606=CARTESIAN_POINT('Ctrl Pts',(-20.9541028768145,17.9336185425138,-16.9668227308571));
#39607=CARTESIAN_POINT('Ctrl Pts',(-20.994587999437,18.0067132510727,-16.9709589060645));
#39608=CARTESIAN_POINT('Ctrl Pts',(-21.031405596239,18.0816074524906,-16.9750950812719));
#39609=CARTESIAN_POINT('Ctrl Pts',(-21.0682233367814,18.1565019463047,-16.9792312726275));
#39610=CARTESIAN_POINT('Ctrl Pts',(-21.1013733182381,18.2331955257884,-16.983367463983));
#39611=CARTESIAN_POINT('Ctrl Pts',(-21.1306893947115,18.3112889656799,-16.9875036553386));
#39612=CARTESIAN_POINT('Ctrl Pts',(-21.1600333335746,18.3894566266172,-16.9916437777855));
#39613=CARTESIAN_POINT('Ctrl Pts',(-21.1855359272154,18.4690263650883,-16.9957839002324));
#39614=CARTESIAN_POINT('Ctrl Pts',(-21.2070801670876,18.549581458411,-16.9999240226793));
#39615=CARTESIAN_POINT('Ctrl Pts',(-21.2286351815299,18.6301768384412,-17.0040662156583));
#39616=CARTESIAN_POINT('Ctrl Pts',(-21.2462278030767,18.7117580962757,-17.0082084086373));
#39617=CARTESIAN_POINT('Ctrl Pts',(-21.2597921942375,18.7938983438909,-17.0123506016163));
#39618=CARTESIAN_POINT('Ctrl Pts',(-21.2733789861849,18.8761742412481,-17.016499635181));
#39619=CARTESIAN_POINT('Ctrl Pts',(-21.2829242114339,18.95901050629,-17.0206486687457));
#39620=CARTESIAN_POINT('Ctrl Pts',(-21.2884139728529,19.0419755778182,-17.0247977023105));
#39621=CARTESIAN_POINT('Ctrl Pts',(-21.2921595270972,19.0985809841503,-17.0276285047975));
#39622=CARTESIAN_POINT('Ctrl Pts',(-21.2940183320645,19.1552463005707,-17.0304593072845));
#39623=CARTESIAN_POINT('Ctrl Pts',(-21.2939998636668,19.2118354794421,-17.0332901097715));
#39624=CARTESIAN_POINT('Ctrl Pts',(-21.2979002849781,19.2118367523804,-17.0332901097715));
#39625=CARTESIAN_POINT('Ctrl Pts',(-21.2980949927007,19.2575742464713,-17.0355745863224));
#39626=CARTESIAN_POINT('Ctrl Pts',(-21.2762381497003,20.1518505805258,-17.0802509984337));
#39627=CARTESIAN_POINT('Ctrl Pts',(-20.2331956316243,21.8407726550478,-17.1673193461055));
#39628=CARTESIAN_POINT('Ctrl Pts',(-18.1310916553567,21.8801180010893,-17.2595383976062));
#39629=CARTESIAN_POINT('Ctrl Pts',(-17.2909884426572,21.3343831391365,-17.3093655135464));
#39630=CARTESIAN_POINT('Ctrl Pts',(-17.1735447521834,21.2423105972199,-17.3168006939262));
#39631=CARTESIAN_POINT('',(-21.2938494856171,19.209803254918,-16.9667098397541));
#39632=CARTESIAN_POINT('Ctrl Pts',(-21.2903253208441,19.2098059207881,-16.9667098902285));
#39633=CARTESIAN_POINT('Ctrl Pts',(-21.2882103114883,19.7131225250721,-16.9916592919231));
#39634=CARTESIAN_POINT('Ctrl Pts',(-20.9008595718265,21.0746360886269,-17.0590006291781));
#39635=CARTESIAN_POINT('Ctrl Pts',(-18.9946006269605,22.075603620026,-17.153439510238));
#39636=CARTESIAN_POINT('Ctrl Pts',(-17.6117180668893,21.5685664086269,-17.2229289896033));
#39637=CARTESIAN_POINT('Ctrl Pts',(-17.1762220931372,21.2388106152247,-17.2500265334081));
#39638=CARTESIAN_POINT('Ctrl Pts',(-17.1744642439897,21.2411350264762,-16.4501666835217));
#39639=CARTESIAN_POINT('Ctrl Pts',(-17.1078207226257,21.189939932003,-16.4543368993101));
#39640=CARTESIAN_POINT('Ctrl Pts',(-17.0436640483384,21.1354316379633,-16.4585071150985));
#39641=CARTESIAN_POINT('Ctrl Pts',(-16.9823341196667,21.0778868856136,-16.4626773308869));
#39642=CARTESIAN_POINT('Ctrl Pts',(-16.9210150140795,21.0203522883665,-16.4668468107442));
#39643=CARTESIAN_POINT('Ctrl Pts',(-16.8625219983004,20.9597826122461,-16.4710162906016));
#39644=CARTESIAN_POINT('Ctrl Pts',(-16.8071598200507,20.8964930794675,-16.4751857704589));
#39645=CARTESIAN_POINT('Ctrl Pts',(-16.7517908046024,20.8331957304664,-16.4793557652448));
#39646=CARTESIAN_POINT('Ctrl Pts',(-16.6995536963249,20.7671782049408,-16.4835257600306));
#39647=CARTESIAN_POINT('Ctrl Pts',(-16.6507135780857,20.6987895295596,-16.4876957548164));
#39648=CARTESIAN_POINT('Ctrl Pts',(-16.6018209673368,20.6303273512197,-16.4918702314401));
#39649=CARTESIAN_POINT('Ctrl Pts',(-16.5563329029902,20.5594893105763,-16.4960447080638));
#39650=CARTESIAN_POINT('Ctrl Pts',(-16.5144713431402,20.4866537701814,-16.5002191846875));
#39651=CARTESIAN_POINT('Ctrl Pts',(-16.4725853567887,20.4137757297593,-16.5043960971463));
#39652=CARTESIAN_POINT('Ctrl Pts',(-16.4343302969003,20.3388982788379,-16.5085730096052));
#39653=CARTESIAN_POINT('Ctrl Pts',(-16.3998812075074,20.262422589891,-16.512749922064));
#39654=CARTESIAN_POINT('Ctrl Pts',(-16.3653738793192,20.1858176129984,-16.5169338959098));
#39655=CARTESIAN_POINT('Ctrl Pts',(-16.3346855367979,20.1076094313179,-16.5211178697556));
#39656=CARTESIAN_POINT('Ctrl Pts',(-16.3079422109483,20.0282169872081,-16.5253018436014));
#39657=CARTESIAN_POINT('Ctrl Pts',(-16.2918496144703,19.980443177262,-16.5278195185964));
#39658=CARTESIAN_POINT('Ctrl Pts',(-16.2771845117736,19.9322408260174,-16.5303371935914));
#39659=CARTESIAN_POINT('Ctrl Pts',(-16.2639654295305,19.8837029215676,-16.5328548685864));
#39660=CARTESIAN_POINT('Ctrl Pts',(-16.2419939573158,19.803027939797,-16.5370395029795));
#39661=CARTESIAN_POINT('Ctrl Pts',(-16.223938199736,19.7211252621465,-16.5412241373725));
#39662=CARTESIAN_POINT('Ctrl Pts',(-16.2099316900943,19.638409834854,-16.5454087717656));
#39663=CARTESIAN_POINT('Ctrl Pts',(-16.1959451169855,19.5558121427341,-16.5495874498495));
#39664=CARTESIAN_POINT('Ctrl Pts',(-16.1859964196337,19.4724044485338,-16.5537661279335));
#39665=CARTESIAN_POINT('Ctrl Pts',(-16.18016901464,19.3886155911377,-16.5579448060174));
#39666=CARTESIAN_POINT('Ctrl Pts',(-16.1742371575999,19.3033248786908,-16.5621983839028));
#39667=CARTESIAN_POINT('Ctrl Pts',(-16.1725759211884,19.2176396691377,-16.5664519617883));
#39668=CARTESIAN_POINT('Ctrl Pts',(-16.1752185615464,19.1320218370346,-16.5707055396737));
#39669=CARTESIAN_POINT('Ctrl Pts',(-16.1778099691644,19.0480638736762,-16.5748766536517));
#39670=CARTESIAN_POINT('Ctrl Pts',(-16.1845398497979,18.9641711795844,-16.5790477676296));
#39671=CARTESIAN_POINT('Ctrl Pts',(-16.1953870618677,18.8807813597822,-16.5832188816076));
#39672=CARTESIAN_POINT('Ctrl Pts',(-16.2062306340507,18.7974195222395,-16.5873885959279));
#39673=CARTESIAN_POINT('Ctrl Pts',(-16.221188734479,18.7145606796676,-16.5915583102483));
#39674=CARTESIAN_POINT('Ctrl Pts',(-16.2401883815475,18.6326371280316,-16.5957280245687));
#39675=CARTESIAN_POINT('Ctrl Pts',(-16.2591873525271,18.5507164915873,-16.5998975905127));
#39676=CARTESIAN_POINT('Ctrl Pts',(-16.2822274794424,18.4697315278527,-16.6040671564568));
#39677=CARTESIAN_POINT('Ctrl Pts',(-16.3091849959464,18.3901028102639,-16.6082367224008));
#39678=CARTESIAN_POINT('Ctrl Pts',(-16.337090305475,18.3076744451974,-16.6125528851397));
#39679=CARTESIAN_POINT('Ctrl Pts',(-16.3691934316988,18.2266999715504,-16.6168690478787));
#39680=CARTESIAN_POINT('Ctrl Pts',(-16.4053020683426,18.1476252104293,-16.6211852106176));
#39681=CARTESIAN_POINT('Ctrl Pts',(-16.4402344699457,18.0711263013346,-16.6253607748093));
#39682=CARTESIAN_POINT('Ctrl Pts',(-16.4789151719813,17.9964056357569,-16.629536339001));
#39683=CARTESIAN_POINT('Ctrl Pts',(-16.5211232637327,17.9238416763712,-16.6337119031926));
#39684=CARTESIAN_POINT('Ctrl Pts',(-16.5654631858581,17.8476126839014,-16.6380983652052));
#39685=CARTESIAN_POINT('Ctrl Pts',(-16.613695880029,17.7737644826753,-16.6424848272177));
#39686=CARTESIAN_POINT('Ctrl Pts',(-16.6655152292137,17.7026993824091,-16.6468712892303));
#39687=CARTESIAN_POINT('Ctrl Pts',(-16.7173345783984,17.6316342821429,-16.6512577512428));
#39688=CARTESIAN_POINT('Ctrl Pts',(-16.7727401579415,17.5633526854597,-16.6556442132553));
#39689=CARTESIAN_POINT('Ctrl Pts',(-16.8313804354227,17.4982131503051,-16.6600306752679));
#39690=CARTESIAN_POINT('Ctrl Pts',(-16.8873225868114,17.4360707817228,-16.6642153096609));
#39691=CARTESIAN_POINT('Ctrl Pts',(-16.9464165382124,17.3765563809787,-16.668399944054));
#39692=CARTESIAN_POINT('Ctrl Pts',(-17.0083856645508,17.3200068309768,-16.6725845784471));
#39693=CARTESIAN_POINT('Ctrl Pts',(-17.070266585508,17.2635377722601,-16.676763256531));
#39694=CARTESIAN_POINT('Ctrl Pts',(-17.1350142155921,17.2100254892842,-16.6809419346149));
#39695=CARTESIAN_POINT('Ctrl Pts',(-17.2023131209905,17.1597722445643,-16.6851206126989));
#39696=CARTESIAN_POINT('Ctrl Pts',(-17.2708183109012,17.108618246549,-16.6893741905843));
#39697=CARTESIAN_POINT('Ctrl Pts',(-17.3419668163953,17.0608416308408,-16.6936277684698));
#39698=CARTESIAN_POINT('Ctrl Pts',(-17.4153882749825,17.0167203645282,-16.6978813463552));
#39699=CARTESIAN_POINT('Ctrl Pts',(-17.4873863153249,16.9734544750586,-16.7020524603332));
#39700=CARTESIAN_POINT('Ctrl Pts',(-17.5615695514942,16.9337037154835,-16.7062235743111));
#39701=CARTESIAN_POINT('Ctrl Pts',(-17.6375585833825,16.8976871763798,-16.7103946882891));
#39702=CARTESIAN_POINT('Ctrl Pts',(-17.7135221164171,16.8616827229737,-16.7145644026094));
#39703=CARTESIAN_POINT('Ctrl Pts',(-17.7912898263828,16.8294101983213,-16.7187341169298));
#39704=CARTESIAN_POINT('Ctrl Pts',(-17.8704587172267,16.8010422300492,-16.7229038312502));
#39705=CARTESIAN_POINT('Ctrl Pts',(-17.9496247909019,16.7726752712311,-16.7270733971942));
#39706=CARTESIAN_POINT('Ctrl Pts',(-18.0301915129629,16.7482127469196,-16.7312429631382));
#39707=CARTESIAN_POINT('Ctrl Pts',(-18.1117382553311,16.7277782376273,-16.7354125290823));
#39708=CARTESIAN_POINT('Ctrl Pts',(-18.1961520805622,16.7066252761969,-16.7397286918212));
#39709=CARTESIAN_POINT('Ctrl Pts',(-18.2816156117521,16.6897889781385,-16.7440448545601));
#39710=CARTESIAN_POINT('Ctrl Pts',(-18.3676498921635,16.6773489588169,-16.748361017299));
#39711=CARTESIAN_POINT('Ctrl Pts',(-18.4508816149397,16.6653141718163,-16.7525365814907));
#39712=CARTESIAN_POINT('Ctrl Pts',(-18.5346470002632,16.6573936417868,-16.7567121456824));
#39713=CARTESIAN_POINT('Ctrl Pts',(-18.6185082461362,16.6536064724432,-16.7608877098741));
#39714=CARTESIAN_POINT('Ctrl Pts',(-18.7066051241772,16.6496280221792,-16.7652741718866));
#39715=CARTESIAN_POINT('Ctrl Pts',(-18.7948072172264,16.6502114543057,-16.7696606338992));
#39716=CARTESIAN_POINT('Ctrl Pts',(-18.8826105511364,16.6553171354624,-16.7740470959117));
#39717=CARTESIAN_POINT('Ctrl Pts',(-18.9704138850463,16.6604228166191,-16.7784335579242));
#39718=CARTESIAN_POINT('Ctrl Pts',(-19.0578178914166,16.6700506076701,-16.7828200199368));
#39719=CARTESIAN_POINT('Ctrl Pts',(-19.1443308019264,16.6840990060965,-16.7872064819493));
#39720=CARTESIAN_POINT('Ctrl Pts',(-19.2268631251808,16.6975010168866,-16.7913911163424));
#39721=CARTESIAN_POINT('Ctrl Pts',(-19.3088917529363,16.7149756618514,-16.7955757507354));
#39722=CARTESIAN_POINT('Ctrl Pts',(-19.389983688077,16.7364726914061,-16.7997603851285));
#39723=CARTESIAN_POINT('Ctrl Pts',(-19.4709601988852,16.7579391226001,-16.8039390632124));
#39724=CARTESIAN_POINT('Ctrl Pts',(-19.5510022244943,16.7834164491322,-16.8081177412964));
#39725=CARTESIAN_POINT('Ctrl Pts',(-19.6296848716229,16.8128030500508,-16.8122964193803));
#39726=CARTESIAN_POINT('Ctrl Pts',(-19.709777848653,16.842716384671,-16.8165499972657));
#39727=CARTESIAN_POINT('Ctrl Pts',(-19.7884617582361,16.8766804423688,-16.8208035751512));
#39728=CARTESIAN_POINT('Ctrl Pts',(-19.8653024038484,16.9145342652139,-16.8250571530366));
#39729=CARTESIAN_POINT('Ctrl Pts',(-19.9406533436033,16.9516542178375,-16.8292282670146));
#39730=CARTESIAN_POINT('Ctrl Pts',(-20.0142314204538,16.9925142474789,-16.8333993809925));
#39731=CARTESIAN_POINT('Ctrl Pts',(-20.0856470518142,17.0369139282627,-16.8375704949705));
#39732=CARTESIAN_POINT('Ctrl Pts',(-20.15703871897,17.081298710305,-16.8417402092909));
#39733=CARTESIAN_POINT('Ctrl Pts',(-20.2262689913884,17.129220541882,-16.8459099236112));
#39734=CARTESIAN_POINT('Ctrl Pts',(-20.2929745824343,17.1804340071488,-16.8500796379316));
#39735=CARTESIAN_POINT('Ctrl Pts',(-20.3596777998089,17.2316456500206,-16.8542492038757));
#39736=CARTESIAN_POINT('Ctrl Pts',(-20.4238561500595,17.2861484128726,-16.8584187698197));
#39737=CARTESIAN_POINT('Ctrl Pts',(-20.4851780435309,17.3436555058438,-16.8625883357638));
#39738=CARTESIAN_POINT('Ctrl Pts',(-20.5486559391278,17.4031844772611,-16.8669044985027));
#39739=CARTESIAN_POINT('Ctrl Pts',(-20.6090723898819,17.4659326132814,-16.8712206612416));
#39740=CARTESIAN_POINT('Ctrl Pts',(-20.6661012016731,17.5315402813722,-16.8755368239805));
#39741=CARTESIAN_POINT('Ctrl Pts',(-20.7212723059185,17.5950107865757,-16.8797123881722));
#39742=CARTESIAN_POINT('Ctrl Pts',(-20.7732728325617,17.6611569867929,-16.8838879523639));
#39743=CARTESIAN_POINT('Ctrl Pts',(-20.8218497444838,17.7296211003059,-16.8880635165556));
#39744=CARTESIAN_POINT('Ctrl Pts',(-20.8728801607464,17.8015431734344,-16.8924499785681));
#39745=CARTESIAN_POINT('Ctrl Pts',(-20.9201317067406,17.8760229761494,-16.8968364405807));
#39746=CARTESIAN_POINT('Ctrl Pts',(-20.9633649162028,17.952615293162,-16.9012229025932));
#39747=CARTESIAN_POINT('Ctrl Pts',(-21.0065981256651,18.0292076101745,-16.9056093646057));
#39748=CARTESIAN_POINT('Ctrl Pts',(-21.0458128079223,18.1079118882385,-16.9099958266183));
#39749=CARTESIAN_POINT('Ctrl Pts',(-21.0808281256647,18.1882596866315,-16.9143822886308));
#39750=CARTESIAN_POINT('Ctrl Pts',(-21.117652895614,18.2727595393394,-16.9189954255354));
#39751=CARTESIAN_POINT('Ctrl Pts',(-21.1499518315869,18.3593459986734,-16.92360856244));
#39752=CARTESIAN_POINT('Ctrl Pts',(-21.1775079602936,18.4475415217695,-16.9282216993445));
#39753=CARTESIAN_POINT('Ctrl Pts',(-21.204985218715,18.5354846144123,-16.9328216326737));
#39754=CARTESIAN_POINT('Ctrl Pts',(-21.2277466226995,18.6250273148932,-16.9374215660029));
#39755=CARTESIAN_POINT('Ctrl Pts',(-21.2456232056939,18.7156729639725,-16.942021499332));
#39756=CARTESIAN_POINT('Ctrl Pts',(-21.263411741867,18.8058721596512,-16.946598776793));
#39757=CARTESIAN_POINT('Ctrl Pts',(-21.2763633328307,18.897163189666,-16.951176054254));
#39758=CARTESIAN_POINT('Ctrl Pts',(-21.2843593339857,18.9890376888929,-16.955753331715));
#39759=CARTESIAN_POINT('Ctrl Pts',(-21.2907392715853,19.0623435277363,-16.9594055003441));
#39760=CARTESIAN_POINT('Ctrl Pts',(-21.2939652250926,19.136020399912,-16.9630576689733));
#39761=CARTESIAN_POINT('Ctrl Pts',(-21.2939997202205,19.2098031412724,-16.9667098376024));
#39762=CARTESIAN_POINT('Origin',(-18.734,19.211,1.76670989022852));
#39763=CARTESIAN_POINT('',(-17.1721129955817,21.2441651167962,-15.6501589752972));
#39764=CARTESIAN_POINT('',(-17.1744642439897,21.2411350264762,-15.7166572006354));
#39765=CARTESIAN_POINT('',(-17.1744642439897,21.2411350264762,1.76670989022852));
#39766=CARTESIAN_POINT('',(-21.2939992944986,19.2129005700935,-16.2332901098004));
#39767=CARTESIAN_POINT('Ctrl Pts',(-17.1744642439897,21.2411350264762,-15.7166572006354));
#39768=CARTESIAN_POINT('Ctrl Pts',(-17.105540262146,21.1881880979566,-15.7209678899666));
#39769=CARTESIAN_POINT('Ctrl Pts',(-17.0393403283499,21.1317462119357,-15.7252785792978));
#39770=CARTESIAN_POINT('Ctrl Pts',(-16.9762229643503,21.0721340341153,-15.729589268629));
#39771=CARTESIAN_POINT('Ctrl Pts',(-16.9150839698182,21.0143903581622,-15.7337648424291));
#39772=CARTESIAN_POINT('Ctrl Pts',(-16.8568374435405,20.9536725741277,-15.7379404162292));
#39773=CARTESIAN_POINT('Ctrl Pts',(-16.8017703156805,20.8903118968895,-15.7421159900293));
#39774=CARTESIAN_POINT('Ctrl Pts',(-16.7440303488595,20.8238758297897,-15.7464942371261));
#39775=CARTESIAN_POINT('Ctrl Pts',(-16.6897865983678,20.7545342647742,-15.7508724842228));
#39776=CARTESIAN_POINT('Ctrl Pts',(-16.6393195365599,20.6827043711569,-15.7552507313195));
#39777=CARTESIAN_POINT('Ctrl Pts',(-16.588852474752,20.6108744775396,-15.7596289784163));
#39778=CARTESIAN_POINT('Ctrl Pts',(-16.5421623435021,20.5365567821694,-15.764007225513));
#39779=CARTESIAN_POINT('Ctrl Pts',(-16.499473974098,20.4601971179787,-15.7683854726097));
#39780=CARTESIAN_POINT('Ctrl Pts',(-16.458673348906,20.3872141935449,-15.7725701070028));
#39781=CARTESIAN_POINT('Ctrl Pts',(-16.4213761508429,20.3120944357929,-15.7767547413958));
#39782=CARTESIAN_POINT('Ctrl Pts',(-16.3878121523982,20.235208271674,-15.7809393757889));
#39783=CARTESIAN_POINT('Ctrl Pts',(-16.3542959281508,20.1584315454929,-15.7851180538728));
#39784=CARTESIAN_POINT('Ctrl Pts',(-16.3245025312235,20.0798938250627,-15.7892967319568));
#39785=CARTESIAN_POINT('Ctrl Pts',(-16.2986164546583,19.9999911197719,-15.7934754100407));
#39786=CARTESIAN_POINT('Ctrl Pts',(-16.2722663887748,19.918656215914,-15.7977289879262));
#39787=CARTESIAN_POINT('Ctrl Pts',(-16.2499653337518,19.8359073320096,-15.8019825658116));
#39788=CARTESIAN_POINT('Ctrl Pts',(-16.2318570828657,19.7521846470793,-15.806236143697));
#39789=CARTESIAN_POINT('Ctrl Pts',(-16.2140998957582,19.6700850897677,-15.810407257675));
#39790=CARTESIAN_POINT('Ctrl Pts',(-16.2003744938965,19.5870496228932,-15.8145783716529));
#39791=CARTESIAN_POINT('Ctrl Pts',(-16.1907660223745,19.5035080085245,-15.8187494856309));
#39792=CARTESIAN_POINT('Ctrl Pts',(-16.1811607750678,19.4199944273513,-15.8229191999512));
#39793=CARTESIAN_POINT('Ctrl Pts',(-16.1756697669882,19.3359754926339,-15.8270889142716));
#39794=CARTESIAN_POINT('Ctrl Pts',(-16.1743265551335,19.2518883314064,-15.831258628592));
#39795=CARTESIAN_POINT('Ctrl Pts',(-16.172983391076,19.167804162361,-15.835428194536));
#39796=CARTESIAN_POINT('Ctrl Pts',(-16.1757877362796,19.0836522316205,-15.8395977604801));
#39797=CARTESIAN_POINT('Ctrl Pts',(-16.1827210351531,18.9998705526709,-15.8437673264241));
#39798=CARTESIAN_POINT('Ctrl Pts',(-16.1898981002618,18.9131432132454,-15.848083489163));
#39799=CARTESIAN_POINT('Ctrl Pts',(-16.2014998257648,18.8268131717704,-15.8523996519019));
#39800=CARTESIAN_POINT('Ctrl Pts',(-16.2174472402026,18.7413594915726,-15.8567158146409));
#39801=CARTESIAN_POINT('Ctrl Pts',(-16.2328751692925,18.6586894560189,-15.8608913788325));
#39802=CARTESIAN_POINT('Ctrl Pts',(-16.2523698584566,18.5768400108849,-15.8650669430242));
#39803=CARTESIAN_POINT('Ctrl Pts',(-16.2758083142182,18.4962317606711,-15.8692425072159));
#39804=CARTESIAN_POINT('Ctrl Pts',(-16.3004305906606,18.4115521793672,-15.8736289692284));
#39805=CARTESIAN_POINT('Ctrl Pts',(-16.3294053113243,18.328243025166,-15.878015431241));
#39806=CARTESIAN_POINT('Ctrl Pts',(-16.3625325554083,18.2467686173736,-15.8824018932535));
#39807=CARTESIAN_POINT('Ctrl Pts',(-16.3956597994923,18.1652942095812,-15.886788355266));
#39808=CARTESIAN_POINT('Ctrl Pts',(-16.4329392521204,18.0856550414425,-15.8911748172785));
#39809=CARTESIAN_POINT('Ctrl Pts',(-16.4741163568262,18.0082839406928,-15.8955612792911));
#39810=CARTESIAN_POINT('Ctrl Pts',(-16.5133988419055,17.9344727989798,-15.8997459136841));
#39811=CARTESIAN_POINT('Ctrl Pts',(-16.5563744043013,17.8624508577059,-15.9039305480772));
#39812=CARTESIAN_POINT('Ctrl Pts',(-16.6028559450595,17.7926118242556,-15.9081151824702));
#39813=CARTESIAN_POINT('Ctrl Pts',(-16.6492713250977,17.722872198025,-15.9122938605542));
#39814=CARTESIAN_POINT('Ctrl Pts',(-16.6991825184353,17.6553096876334,-15.9164725386381));
#39815=CARTESIAN_POINT('Ctrl Pts',(-16.752356406431,17.5902937749033,-15.9206512167221));
#39816=CARTESIAN_POINT('Ctrl Pts',(-16.8064833981537,17.5241124986637,-15.9249047946075));
#39817=CARTESIAN_POINT('Ctrl Pts',(-16.8639909761116,17.460570439207,-15.9291583724929));
#39818=CARTESIAN_POINT('Ctrl Pts',(-16.9245868519813,17.400026764478,-15.9334119503784));
#39819=CARTESIAN_POINT('Ctrl Pts',(-16.9840079585542,17.3406568470249,-15.9375830643563));
#39820=CARTESIAN_POINT('Ctrl Pts',(-17.0463983458432,17.2841704328241,-15.9417541783343));
#39821=CARTESIAN_POINT('Ctrl Pts',(-17.1114427393843,17.2308717374818,-15.9459252923122));
#39822=CARTESIAN_POINT('Ctrl Pts',(-17.176465306651,17.1775909270316,-15.9500950066326));
#39823=CARTESIAN_POINT('Ctrl Pts',(-17.2441397559353,17.12749600239,-15.954264720953));
#39824=CARTESIAN_POINT('Ctrl Pts',(-17.3141166963449,17.0808517882548,-15.9584344352734));
#39825=CARTESIAN_POINT('Ctrl Pts',(-17.3840911466745,17.0342092339209,-15.9626040012174));
#39826=CARTESIAN_POINT('Ctrl Pts',(-17.4563675419654,16.9910174003976,-15.9667735671614));
#39827=CARTESIAN_POINT('Ctrl Pts',(-17.5305675384036,16.9514977737617,-15.9709431331055));
#39828=CARTESIAN_POINT('Ctrl Pts',(-17.6073763151811,16.9105886858059,-15.9752592958444));
#39829=CARTESIAN_POINT('Ctrl Pts',(-17.6862460120071,16.8736150868692,-15.9795754585833));
#39830=CARTESIAN_POINT('Ctrl Pts',(-17.7667310666841,16.8407698823443,-15.9838916213223));
#39831=CARTESIAN_POINT('Ctrl Pts',(-17.8445943291705,16.8089946069022,-15.9880671855139));
#39832=CARTESIAN_POINT('Ctrl Pts',(-17.923968865071,16.7810830031343,-15.9922427497056));
#39833=CARTESIAN_POINT('Ctrl Pts',(-18.0044344385269,16.7571593182294,-15.9964183138973));
#39834=CARTESIAN_POINT('Ctrl Pts',(-18.0889641368094,16.732027304873,-16.0008047759098));
#39835=CARTESIAN_POINT('Ctrl Pts',(-18.1746974182797,16.711296794516,-16.0051912379224));
#39836=CARTESIAN_POINT('Ctrl Pts',(-18.2611356505437,16.6950510126369,-16.0095776999349));
#39837=CARTESIAN_POINT('Ctrl Pts',(-18.3475738828078,16.6788052307578,-16.0139641619475));
#39838=CARTESIAN_POINT('Ctrl Pts',(-18.434716480688,16.6670441795795,-16.01835062396));
#39839=CARTESIAN_POINT('Ctrl Pts',(-18.5220617179684,16.6597880988421,-16.0227370859726));
#39840=CARTESIAN_POINT('Ctrl Pts',(-18.6053880714047,16.6528658811356,-16.0269217203656));
#39841=CARTESIAN_POINT('Ctrl Pts',(-18.6892089831255,16.6500174172729,-16.0311063547587));
#39842=CARTESIAN_POINT('Ctrl Pts',(-18.7730921344107,16.6512984929826,-16.0352909891517));
#39843=CARTESIAN_POINT('Ctrl Pts',(-18.856855888413,16.6525777452396,-16.0394696672357));
#39844=CARTESIAN_POINT('Ctrl Pts',(-18.9406812499664,16.6579748547684,-16.0436483453196));
#39845=CARTESIAN_POINT('Ctrl Pts',(-19.0241313606307,16.6674937991861,-16.0478270234036));
#39846=CARTESIAN_POINT('Ctrl Pts',(-19.1090772545541,16.6771833638415,-16.052080601289));
#39847=CARTESIAN_POINT('Ctrl Pts',(-19.1936338320393,16.6911440245191,-16.0563341791744));
#39848=CARTESIAN_POINT('Ctrl Pts',(-19.2773408795587,16.7093244237911,-16.0605877570599));
#39849=CARTESIAN_POINT('Ctrl Pts',(-19.359425102621,16.727152360547,-16.0647588710378));
#39850=CARTESIAN_POINT('Ctrl Pts',(-19.4406919711072,16.7490377781069,-16.0689299850158));
#39851=CARTESIAN_POINT('Ctrl Pts',(-19.5207150357479,16.7748802466775,-16.0731010989937));
#39852=CARTESIAN_POINT('Ctrl Pts',(-19.6007112478765,16.8007140435582,-16.0772708133141));
#39853=CARTESIAN_POINT('Ctrl Pts',(-19.6794640476567,16.8305021131095,-16.0814405276345));
#39854=CARTESIAN_POINT('Ctrl Pts',(-19.7565616407636,16.8640940174692,-16.0856102419549));
#39855=CARTESIAN_POINT('Ctrl Pts',(-19.8336564904072,16.8976847264848,-16.0897798078989));
#39856=CARTESIAN_POINT('Ctrl Pts',(-19.9090958290854,16.9350788166487,-16.093949373843));
#39857=CARTESIAN_POINT('Ctrl Pts',(-19.9824886317276,16.9760780469003,-16.098118939787));
#39858=CARTESIAN_POINT('Ctrl Pts',(-20.0584618347708,17.0185187595094,-16.1024351025259));
#39859=CARTESIAN_POINT('Ctrl Pts',(-20.1322414512874,17.0648225852953,-16.1067512652649));
#39860=CARTESIAN_POINT('Ctrl Pts',(-20.2034241040032,17.1147192929919,-16.1110674280038));
#39861=CARTESIAN_POINT('Ctrl Pts',(-20.272287989294,17.1629906206835,-16.1152429921955));
#39862=CARTESIAN_POINT('Ctrl Pts',(-20.3387211617817,17.2146240223492,-16.1194185563871));
#39863=CARTESIAN_POINT('Ctrl Pts',(-20.4023916835429,17.2693333987821,-16.1235941205788));
#39864=CARTESIAN_POINT('Ctrl Pts',(-20.4692780519958,17.3268060157594,-16.1279805825913));
#39865=CARTESIAN_POINT('Ctrl Pts',(-20.5331149297311,17.3876731058189,-16.1323670446039));
#39866=CARTESIAN_POINT('Ctrl Pts',(-20.5935624370344,17.4515604464004,-16.1367535066164));
#39867=CARTESIAN_POINT('Ctrl Pts',(-20.6540099443376,17.515447786982,-16.141139968629));
#39868=CARTESIAN_POINT('Ctrl Pts',(-20.7110677625942,17.5823548872471,-16.1455264306415));
#39869=CARTESIAN_POINT('Ctrl Pts',(-20.764447298501,17.6518708302357,-16.149912892654));
#39870=CARTESIAN_POINT('Ctrl Pts',(-20.8154455601759,17.7182856499018,-16.1541036735168));
#39871=CARTESIAN_POINT('Ctrl Pts',(-20.8632791399794,17.7873320135741,-16.1582944543796));
#39872=CARTESIAN_POINT('Ctrl Pts',(-20.9076654294934,17.8586765917041,-16.1624852352424));
#39873=CARTESIAN_POINT('Ctrl Pts',(-20.9519891627481,17.929920619642,-16.1666701097864));
#39874=CARTESIAN_POINT('Ctrl Pts',(-20.9928750133147,18.0034560458724,-16.1708549843304));
#39875=CARTESIAN_POINT('Ctrl Pts',(-21.0300812471761,18.0789174471947,-16.1750398588744));
#39876=CARTESIAN_POINT('Ctrl Pts',(-21.0672460755937,18.1542948703099,-16.1792200762261));
#39877=CARTESIAN_POINT('Ctrl Pts',(-21.1007392197539,18.2315936031769,-16.1834002935778));
#39878=CARTESIAN_POINT('Ctrl Pts',(-21.1303635397438,18.310421416318,-16.1875805109295));
#39879=CARTESIAN_POINT('Ctrl Pts',(-21.1599640139561,18.3891857778594,-16.1917573634602));
#39880=CARTESIAN_POINT('Ctrl Pts',(-21.1857016914127,18.4694763469324,-16.1959342159909));
#39881=CARTESIAN_POINT('Ctrl Pts',(-21.2074270380287,18.550879793107,-16.2001110685216));
#39882=CARTESIAN_POINT('Ctrl Pts',(-21.2291418983469,18.6322439478127,-16.2042859049869));
#39883=CARTESIAN_POINT('Ctrl Pts',(-21.2468481598048,18.7147194701813,-16.2084607414522));
#39884=CARTESIAN_POINT('Ctrl Pts',(-21.2604461548154,18.7978779516678,-16.2126355779175));
#39885=CARTESIAN_POINT('Ctrl Pts',(-21.2740449836496,18.881041532398,-16.2168106703821));
#39886=CARTESIAN_POINT('Ctrl Pts',(-21.2835349604935,18.9648877054714,-16.2209857628466));
#39887=CARTESIAN_POINT('Ctrl Pts',(-21.2888677421723,19.0489789519614,-16.2251608553112));
#39888=CARTESIAN_POINT('Ctrl Pts',(-21.2923288662564,19.1035565169218,-16.227870606798));
#39889=CARTESIAN_POINT('Ctrl Pts',(-21.2940398771788,19.1582371483247,-16.2305803582847));
#39890=CARTESIAN_POINT('Ctrl Pts',(-21.293999294499,19.2129005695107,-16.2332901097715));
#39891=CARTESIAN_POINT('Ctrl Pts',(-21.2939992944986,19.2129005700935,-16.2332901098004));
#39892=CARTESIAN_POINT('Ctrl Pts',(-21.2939272486892,19.3099436741152,-16.2381006886061));
#39893=CARTESIAN_POINT('Ctrl Pts',(-21.2883332378637,19.4067618611679,-16.2429112674118));
#39894=CARTESIAN_POINT('Ctrl Pts',(-21.2773175036261,19.5027808694022,-16.2477218462175));
#39895=CARTESIAN_POINT('Ctrl Pts',(-21.2661096544807,19.6004744535223,-16.2526163217372));
#39896=CARTESIAN_POINT('Ctrl Pts',(-21.2492893600036,19.6973405506026,-16.2575107972568));
#39897=CARTESIAN_POINT('Ctrl Pts',(-21.2270132516536,19.792794574639,-16.2624052727765));
#39898=CARTESIAN_POINT('Ctrl Pts',(-21.2047371433036,19.8882485986755,-16.2672997482961));
#39899=CARTESIAN_POINT('Ctrl Pts',(-21.1770053785922,19.9822904288902,-16.2721942238158));
#39900=CARTESIAN_POINT('Ctrl Pts',(-21.1440235064311,20.074357804418,-16.2770886993354));
#39901=CARTESIAN_POINT('Ctrl Pts',(-21.1158249638011,20.1530727360925,-16.2812733337285));
#39902=CARTESIAN_POINT('Ctrl Pts',(-21.0837134704203,20.2305511910393,-16.2854579681215));
#39903=CARTESIAN_POINT('Ctrl Pts',(-21.0478172393665,20.3063765484118,-16.2896426025146));
#39904=CARTESIAN_POINT('Ctrl Pts',(-21.0119721021545,20.3820939777732,-16.2938212805985));
#39905=CARTESIAN_POINT('Ctrl Pts',(-20.9723531229123,20.4561625710811,-16.2979999586825));
#39906=CARTESIAN_POINT('Ctrl Pts',(-20.9291375533232,20.5281830252437,-16.3021786367664));
#39907=CARTESIAN_POINT('Ctrl Pts',(-20.8851473757077,20.601494394287,-16.3064322146518));
#39908=CARTESIAN_POINT('Ctrl Pts',(-20.8374305643565,20.6726830222908,-16.3106857925373));
#39909=CARTESIAN_POINT('Ctrl Pts',(-20.7862244101177,20.7413512572338,-16.3149393704227));
#39910=CARTESIAN_POINT('Ctrl Pts',(-20.7360109870995,20.8086882244473,-16.3191104844007));
#39911=CARTESIAN_POINT('Ctrl Pts',(-20.6824425969519,20.873601266221,-16.3232815983786));
#39912=CARTESIAN_POINT('Ctrl Pts',(-20.6257872198946,20.9357437823176,-16.3274527123566));
#39913=CARTESIAN_POINT('Ctrl Pts',(-20.5691508540963,20.9978654458928,-16.331622426677));
#39914=CARTESIAN_POINT('Ctrl Pts',(-20.5094298683183,21.0572180904716,-16.3357921409973));
#39915=CARTESIAN_POINT('Ctrl Pts',(-20.4469316957122,21.1134891605011,-16.3399618553177));
#39916=CARTESIAN_POINT('Ctrl Pts',(-20.3844357470594,21.1697582281645,-16.3441314212617));
#39917=CARTESIAN_POINT('Ctrl Pts',(-20.3191631505145,21.2229456321213,-16.3483009872058));
#39918=CARTESIAN_POINT('Ctrl Pts',(-20.2514562536424,21.2727775142535,-16.3524705531498));
#39919=CARTESIAN_POINT('Ctrl Pts',(-20.1813688658018,21.3243614238873,-16.3567867158888));
#39920=CARTESIAN_POINT('Ctrl Pts',(-20.1086732374466,21.372349148503,-16.3611028786277));
#39921=CARTESIAN_POINT('Ctrl Pts',(-20.0337823603681,21.4164853923062,-16.3654190413666));
#39922=CARTESIAN_POINT('Ctrl Pts',(-19.9613310457333,21.4591839026097,-16.3695946055583));
#39923=CARTESIAN_POINT('Ctrl Pts',(-19.8868257455395,21.498277825633,-16.37377016975));
#39924=CARTESIAN_POINT('Ctrl Pts',(-19.8106643175712,21.5335834640049,-16.3779457339416));
#39925=CARTESIAN_POINT('Ctrl Pts',(-19.7306561569328,21.5706723062398,-16.3823321959542));
#39926=CARTESIAN_POINT('Ctrl Pts',(-19.6488207114389,21.6035798961264,-16.3867186579667));
#39927=CARTESIAN_POINT('Ctrl Pts',(-19.565639342473,21.6321517928562,-16.3911051199793));
#39928=CARTESIAN_POINT('Ctrl Pts',(-19.4824579735071,21.6607236895861,-16.3954915819918));
#39929=CARTESIAN_POINT('Ctrl Pts',(-19.3979312597773,21.6849598063577,-16.3998780440043));
#39930=CARTESIAN_POINT('Ctrl Pts',(-19.3125527301391,21.7047675790756,-16.4042645060169));
#39931=CARTESIAN_POINT('Ctrl Pts',(-19.2310959760761,21.7236655019802,-16.4084494803761));
#39932=CARTESIAN_POINT('Ctrl Pts',(-19.1485607217984,21.7386033270999,-16.4126344547353));
#39933=CARTESIAN_POINT('Ctrl Pts',(-19.0653667817849,21.7494633257011,-16.4168194290945));
#39934=CARTESIAN_POINT('Ctrl Pts',(-18.9823149545843,21.760304773132,-16.420997254634));
#39935=CARTESIAN_POINT('Ctrl Pts',(-18.8986071312342,21.767082185981,-16.4251750801735));
#39936=CARTESIAN_POINT('Ctrl Pts',(-18.8146747410986,21.7697285096603,-16.4293529057129));
#39937=CARTESIAN_POINT('Ctrl Pts',(-18.7308239310027,21.7723722611837,-16.4335266705177));
#39938=CARTESIAN_POINT('Ctrl Pts',(-18.6467494445132,21.7708928806729,-16.4377004353224));
#39939=CARTESIAN_POINT('Ctrl Pts',(-18.5628884909282,21.7652750148453,-16.4418742001271));
#39940=CARTESIAN_POINT('Ctrl Pts',(-18.4790838891784,21.759660924041,-16.4460451602976));
#39941=CARTESIAN_POINT('Ctrl Pts',(-18.395492992995,21.7499139014376,-16.450216120468));
#39942=CARTESIAN_POINT('Ctrl Pts',(-18.3125523069991,21.7360706608062,-16.4543870806384));
#39943=CARTESIAN_POINT('Ctrl Pts',(-18.2296424734748,21.722232569616,-16.4585564892853));
#39944=CARTESIAN_POINT('Ctrl Pts',(-18.147382822705,21.7043013640785,-16.4627258979321));
#39945=CARTESIAN_POINT('Ctrl Pts',(-18.0662026746013,21.6823653578923,-16.466895306579));
#39946=CARTESIAN_POINT('Ctrl Pts',(-17.9849897282951,21.6604204891752,-16.47106639974));
#39947=CARTESIAN_POINT('Ctrl Pts',(-17.904857603049,21.6344676983622,-16.475237492901));
#39948=CARTESIAN_POINT('Ctrl Pts',(-17.826222656682,21.6046458165231,-16.479408586062));
#39949=CARTESIAN_POINT('Ctrl Pts',(-17.747575565893,21.5748193289771,-16.4835803234088));
#39950=CARTESIAN_POINT('Ctrl Pts',(-17.670426540659,21.5411227351731,-16.4877520607556));
#39951=CARTESIAN_POINT('Ctrl Pts',(-17.5951721111185,21.5037431254953,-16.4919237981024));
#39952=CARTESIAN_POINT('Ctrl Pts',(-17.5198228509081,21.466316412498,-16.4961007923975));
#39953=CARTESIAN_POINT('Ctrl Pts',(-17.4463733641076,21.4251976266706,-16.5002777866927));
#39954=CARTESIAN_POINT('Ctrl Pts',(-17.3751954108584,21.3806198027598,-16.5044547809878));
#39955=CARTESIAN_POINT('Ctrl Pts',(-17.3060362702805,21.3373063348984,-16.5085133036407));
#39956=CARTESIAN_POINT('Ctrl Pts',(-17.2390218174128,21.2907277100965,-16.5125718262936));
#39957=CARTESIAN_POINT('Ctrl Pts',(-17.1744642439897,21.2411350264762,-16.5166303489465));
#39958=CARTESIAN_POINT('',(-21.2939994369002,19.2093020392337,-16.1667098902285));
#39959=CARTESIAN_POINT('Ctrl Pts',(-21.2939994369002,19.2093020392337,-16.1667098902285));
#39960=CARTESIAN_POINT('Ctrl Pts',(-21.2940542005915,19.2918687402816,-16.1708335669039));
#39961=CARTESIAN_POINT('Ctrl Pts',(-21.2901102644712,19.37459277435,-16.1749572435793));
#39962=CARTESIAN_POINT('Ctrl Pts',(-21.282148407848,19.4570481489096,-16.1790809202548));
#39963=CARTESIAN_POINT('Ctrl Pts',(-21.2741500199359,19.5398818524497,-16.1832235175451));
#39964=CARTESIAN_POINT('Ctrl Pts',(-21.2620966823448,19.6224439445467,-16.1873661148355));
#39965=CARTESIAN_POINT('Ctrl Pts',(-21.2460219433305,19.7043008779902,-16.1915087121259));
#39966=CARTESIAN_POINT('Ctrl Pts',(-21.23005430851,19.7856124078128,-16.1956237077524));
#39967=CARTESIAN_POINT('Ctrl Pts',(-21.2101187777554,19.8662276743518,-16.1997387033789));
#39968=CARTESIAN_POINT('Ctrl Pts',(-21.1863001253011,19.9457272251988,-16.2038536990054));
#39969=CARTESIAN_POINT('Ctrl Pts',(-21.1624916905597,20.0251926723701,-16.2079669293832));
#39970=CARTESIAN_POINT('Ctrl Pts',(-21.13480357533,20.1035429002386,-16.2120801597611));
#39971=CARTESIAN_POINT('Ctrl Pts',(-21.1033710027996,20.1803714721883,-16.2161933901389));
#39972=CARTESIAN_POINT('Ctrl Pts',(-21.0719418753925,20.2571916234494,-16.2203061696919));
#39973=CARTESIAN_POINT('Ctrl Pts',(-21.0367692860285,20.3324900117991,-16.2244189492448));
#39974=CARTESIAN_POINT('Ctrl Pts',(-20.998036835518,20.405879578626,-16.2285317287978));
#39975=CARTESIAN_POINT('Ctrl Pts',(-20.9588192445656,20.48018838104,-16.2326960226666));
#39976=CARTESIAN_POINT('Ctrl Pts',(-20.9159522062818,20.5525397612551,-16.2368603165354));
#39977=CARTESIAN_POINT('Ctrl Pts',(-20.8696736494983,20.6225587351713,-16.2410246104042));
#39978=CARTESIAN_POINT('Ctrl Pts',(-20.8239074514183,20.6918025157111,-16.2451428005837));
#39979=CARTESIAN_POINT('Ctrl Pts',(-20.7748052350545,20.7587649302322,-16.2492609907631));
#39980=CARTESIAN_POINT('Ctrl Pts',(-20.7226388747276,20.823115202435,-16.2533791809425));
#39981=CARTESIAN_POINT('Ctrl Pts',(-20.6695965003383,20.8885460894827,-16.257566526656));
#39982=CARTESIAN_POINT('Ctrl Pts',(-20.6133864683218,20.9512759179512,-16.2617538723695));
#39983=CARTESIAN_POINT('Ctrl Pts',(-20.5543334369044,21.0109961606869,-16.265941218083));
#39984=CARTESIAN_POINT('Ctrl Pts',(-20.495280405487,21.0707164034227,-16.2701285637965));
#39985=CARTESIAN_POINT('Ctrl Pts',(-20.4333847973435,21.1274267716985,-16.2743159095101));
#39986=CARTESIAN_POINT('Ctrl Pts',(-20.369004471075,21.1808630357374,-16.2785032552236));
#39987=CARTESIAN_POINT('Ctrl Pts',(-20.3046658312849,21.2342646996152,-16.2826878896166));
#39988=CARTESIAN_POINT('Ctrl Pts',(-20.2375884427955,21.2846103343966,-16.2868725240096));
#39989=CARTESIAN_POINT('Ctrl Pts',(-20.1680947292201,21.3316065895453,-16.2910571584027));
#39990=CARTESIAN_POINT('Ctrl Pts',(-20.0986999313442,21.378535951342,-16.2952358364866));
#39991=CARTESIAN_POINT('Ctrl Pts',(-20.0268960178075,21.4221251476138,-16.2994145145706));
#39992=CARTESIAN_POINT('Ctrl Pts',(-19.9530388079931,21.4621206952553,-16.3035931926545));
#39993=CARTESIAN_POINT('Ctrl Pts',(-19.877857760773,21.502833134344,-16.30784677054));
#39994=CARTESIAN_POINT('Ctrl Pts',(-19.800549453568,21.5398215173808,-16.3121003484254));
#39995=CARTESIAN_POINT('Ctrl Pts',(-19.7215205448428,21.5728643427414,-16.3163539263108));
#39996=CARTESIAN_POINT('Ctrl Pts',(-19.6440237657254,21.6052665684547,-16.3205250402888));
#39997=CARTESIAN_POINT('Ctrl Pts',(-19.5648729481498,21.6338746703222,-16.3246961542667));
#39998=CARTESIAN_POINT('Ctrl Pts',(-19.4844751811847,21.6585267112793,-16.3288672682447));
#39999=CARTESIAN_POINT('Ctrl Pts',(-19.4041043924667,21.683170480006,-16.3330369825651));
#40000=CARTESIAN_POINT('Ctrl Pts',(-19.3224879248151,21.7038606894987,-16.3372066968855));
#40001=CARTESIAN_POINT('Ctrl Pts',(-19.2400494979668,21.7204847888775,-16.3413764112058));
#40002=CARTESIAN_POINT('Ctrl Pts',(-19.1576140046316,21.7371082966994,-16.3455459771499));
#40003=CARTESIAN_POINT('Ctrl Pts',(-19.0743570613777,21.7496658919856,-16.3497155430939));
#40004=CARTESIAN_POINT('Ctrl Pts',(-18.9907127437439,21.758096104822,-16.3538851090379));
#40005=CARTESIAN_POINT('Ctrl Pts',(-18.9041275950885,21.7668227135419,-16.3582012717769));
#40006=CARTESIAN_POINT('Ctrl Pts',(-18.8171278498233,21.7711262492444,-16.3625174345158));
#40007=CARTESIAN_POINT('Ctrl Pts',(-18.7301989430818,21.7709971781169,-16.3668335972547));
#40008=CARTESIAN_POINT('Ctrl Pts',(-18.646101736334,21.7708723114677,-16.3710091614464));
#40009=CARTESIAN_POINT('Ctrl Pts',(-18.5620712918898,21.7665992585964,-16.3751847256381));
#40010=CARTESIAN_POINT('Ctrl Pts',(-18.478543574057,21.7582224116563,-16.3793602898297));
#40011=CARTESIAN_POINT('Ctrl Pts',(-18.3907970697647,21.7494224700914,-16.3837467518423));
#40012=CARTESIAN_POINT('Ctrl Pts',(-18.3036059893692,21.7360933624401,-16.3881332138548));
#40013=CARTESIAN_POINT('Ctrl Pts',(-18.2174632822105,21.7183471676605,-16.3925196758674));
#40014=CARTESIAN_POINT('Ctrl Pts',(-18.1313205750519,21.700600972881,-16.3969061378799));
#40015=CARTESIAN_POINT('Ctrl Pts',(-18.0462267834431,21.6784379108237,-16.4012925998925));
#40016=CARTESIAN_POINT('Ctrl Pts',(-17.9626538344088,21.652029514944,-16.405679061905));
#40017=CARTESIAN_POINT('Ctrl Pts',(-17.8829440436939,21.6268418467689,-16.4098627597766));
#40018=CARTESIAN_POINT('Ctrl Pts',(-17.804320970107,21.5976989266328,-16.4140464576482));
#40019=CARTESIAN_POINT('Ctrl Pts',(-17.7272055153236,21.5647129955934,-16.4182301555198));
#40020=CARTESIAN_POINT('Ctrl Pts',(-17.6501861872981,21.5317681825194,-16.4224086382849));
#40021=CARTESIAN_POINT('Ctrl Pts',(-17.5746711676834,21.4949900441651,-16.42658712105));
#40022=CARTESIAN_POINT('Ctrl Pts',(-17.501066141267,21.4545405278242,-16.430765603815));
#40023=CARTESIAN_POINT('Ctrl Pts',(-17.4275438124869,21.4141364578278,-16.4349393919191));
#40024=CARTESIAN_POINT('Ctrl Pts',(-17.3559276132931,21.3700694275063,-16.4391131800231));
#40025=CARTESIAN_POINT('Ctrl Pts',(-17.286601701979,21.3225487602435,-16.4432869681272));
#40026=CARTESIAN_POINT('Ctrl Pts',(-17.2485114006814,21.2964390921614,-16.445580206592));
#40027=CARTESIAN_POINT('Ctrl Pts',(-17.2111121045273,21.2692876607317,-16.4478734450569));
#40028=CARTESIAN_POINT('Ctrl Pts',(-17.1744642439897,21.2411350264762,-16.4501666835217));
#40029=CARTESIAN_POINT('Ctrl Pts',(-17.1721129955817,21.2441651167962,-15.6501589752972));
#40030=CARTESIAN_POINT('Ctrl Pts',(-16.5413044024314,20.7545799890971,-15.6900393263641));
#40031=CARTESIAN_POINT('Ctrl Pts',(-15.7364333696473,19.087953254603,-15.7723116129914));
#40032=CARTESIAN_POINT('Ctrl Pts',(-17.157742779603,16.6266809758552,-15.8969758351793));
#40033=CARTESIAN_POINT('Ctrl Pts',(-20.0538051846353,16.4867742534768,-16.0241516418607));
#40034=CARTESIAN_POINT('Ctrl Pts',(-21.2452321357866,18.1548349245933,-16.1140629935438));
#40035=CARTESIAN_POINT('Ctrl Pts',(-21.2975540665632,19.1065231701483,-16.1615824096664));
#40036=CARTESIAN_POINT('Ctrl Pts',(-21.2967674646518,19.2093002032948,-16.1667098902285));
#40037=CARTESIAN_POINT('Origin',(-18.734,19.211,1.76670989022852));
#40038=CARTESIAN_POINT('',(-17.1744642439897,21.2411350264762,-14.8500370213226));
#40039=CARTESIAN_POINT('',(-17.1744642439897,21.2411350264762,-14.9167585741126));
#40040=CARTESIAN_POINT('',(-17.1744642439897,21.2411350264762,1.76670989022852));
#40041=CARTESIAN_POINT('',(-21.293999428374,19.2092892327452,-15.4332901097416));
#40042=CARTESIAN_POINT('Ctrl Pts',(-17.1744642439897,21.2411350264762,-14.9167585741126));
#40043=CARTESIAN_POINT('Ctrl Pts',(-17.1078481116885,21.1899609720926,-14.9209295684745));
#40044=CARTESIAN_POINT('Ctrl Pts',(-17.043705379627,21.1354676782673,-14.9251005628365));
#40045=CARTESIAN_POINT('Ctrl Pts',(-16.9823784647263,21.0779284927831,-14.9292715571984));
#40046=CARTESIAN_POINT('Ctrl Pts',(-16.9210710217901,21.020407576618,-14.9334412272241));
#40047=CARTESIAN_POINT('Ctrl Pts',(-16.8625779555852,20.9598430040762,-14.9376108972499));
#40048=CARTESIAN_POINT('Ctrl Pts',(-16.8072070152721,20.8965470310861,-14.9417805672756));
#40049=CARTESIAN_POINT('Ctrl Pts',(-16.7518370459354,20.8332521680447,-14.9459501641826));
#40050=CARTESIAN_POINT('Ctrl Pts',(-16.6995893957288,20.7672263467399,-14.9501197610897));
#40051=CARTESIAN_POINT('Ctrl Pts',(-16.6507325669181,20.69881611843,-14.9542893579967));
#40052=CARTESIAN_POINT('Ctrl Pts',(-16.6008933205169,20.6290302909808,-14.9585427975404));
#40053=CARTESIAN_POINT('Ctrl Pts',(-16.5545830529723,20.5567635132021,-14.9627962370841));
#40054=CARTESIAN_POINT('Ctrl Pts',(-16.5120402532923,20.4824145209217,-14.9670496766278));
#40055=CARTESIAN_POINT('Ctrl Pts',(-16.4702752492726,20.4094248261953,-14.9712253519706));
#40056=CARTESIAN_POINT('Ctrl Pts',(-16.4321412641796,20.3344288611474,-14.9754010273135));
#40057=CARTESIAN_POINT('Ctrl Pts',(-16.3978164930544,20.2578269302399,-14.9795767026564));
#40058=CARTESIAN_POINT('Ctrl Pts',(-16.3625328692254,20.1790851462127,-14.9838690243005));
#40059=CARTESIAN_POINT('Ctrl Pts',(-16.3312746389474,20.0986468241009,-14.9881613459446));
#40060=CARTESIAN_POINT('Ctrl Pts',(-16.3041808829601,20.0169646756945,-14.9924536675887));
#40061=CARTESIAN_POINT('Ctrl Pts',(-16.2770871269728,19.9352825272881,-14.9967459892329));
#40062=CARTESIAN_POINT('Ctrl Pts',(-16.254157917113,19.8523570726247,-15.001038310877));
#40063=CARTESIAN_POINT('Ctrl Pts',(-16.2354754819719,19.7686515334978,-15.0053306325211));
#40064=CARTESIAN_POINT('Ctrl Pts',(-16.2172617582301,19.6870460279087,-15.0095152669141));
#40065=CARTESIAN_POINT('Ctrl Pts',(-16.2030163785017,19.6043953888035,-15.0136999013072));
#40066=CARTESIAN_POINT('Ctrl Pts',(-16.1928535263698,19.5211202985238,-15.0178845357002));
#40067=CARTESIAN_POINT('Ctrl Pts',(-16.1827051397999,19.4379637400279,-15.0220632137842));
#40068=CARTESIAN_POINT('Ctrl Pts',(-16.1766277936582,19.3541849485908,-15.0262418918681));
#40069=CARTESIAN_POINT('Ctrl Pts',(-16.1746849654928,19.2702161645613,-15.0304205699521));
#40070=CARTESIAN_POINT('Ctrl Pts',(-16.1727073135288,19.1847423004251,-15.0346741478375));
#40071=CARTESIAN_POINT('Ctrl Pts',(-16.1750139649456,19.0990720360283,-15.0389277257229));
#40072=CARTESIAN_POINT('Ctrl Pts',(-16.1816167614736,19.0136682902081,-15.0431813036084));
#40073=CARTESIAN_POINT('Ctrl Pts',(-16.1880915499065,18.9299202626523,-15.0473524175863));
#40074=CARTESIAN_POINT('Ctrl Pts',(-16.1986973545604,18.8464289917134,-15.0515235315643));
#40075=CARTESIAN_POINT('Ctrl Pts',(-16.2133928011125,18.7636306348036,-15.0556946455422));
#40076=CARTESIAN_POINT('Ctrl Pts',(-16.2280833164655,18.6808600616823,-15.0598643598626));
#40077=CARTESIAN_POINT('Ctrl Pts',(-16.2468606679443,18.5987823933906,-15.064034074183));
#40078=CARTESIAN_POINT('Ctrl Pts',(-16.2696319425034,18.517826084456,-15.0682037885033));
#40079=CARTESIAN_POINT('Ctrl Pts',(-16.292402406763,18.4368726562941,-15.0723733544474));
#40080=CARTESIAN_POINT('Ctrl Pts',(-16.3191663861462,18.3570409507695,-15.0765429203914));
#40081=CARTESIAN_POINT('Ctrl Pts',(-16.3497807798975,18.278745361774,-15.0807124863355));
#40082=CARTESIAN_POINT('Ctrl Pts',(-16.3814715379662,18.1976969964576,-15.0850286490744));
#40083=CARTESIAN_POINT('Ctrl Pts',(-16.4172883172412,18.1182952684026,-15.0893448118133));
#40084=CARTESIAN_POINT('Ctrl Pts',(-16.4570183818635,18.040976619606,-15.0936609745523));
#40085=CARTESIAN_POINT('Ctrl Pts',(-16.4954542438097,17.9661766176614,-15.0978365387439));
#40086=CARTESIAN_POINT('Ctrl Pts',(-16.5375520792277,17.893326450692,-15.1020121029356));
#40087=CARTESIAN_POINT('Ctrl Pts',(-16.5830736962919,17.8227939504466,-15.1061876671273));
#40088=CARTESIAN_POINT('Ctrl Pts',(-16.6308945020167,17.7486990212889,-15.1105741291398));
#40089=CARTESIAN_POINT('Ctrl Pts',(-16.6824937078807,17.6771625161639,-15.1149605911524));
#40090=CARTESIAN_POINT('Ctrl Pts',(-16.7375469032624,17.6085721443613,-15.1193470531649));
#40091=CARTESIAN_POINT('Ctrl Pts',(-16.7926000986442,17.5399817725586,-15.1237335151774));
#40092=CARTESIAN_POINT('Ctrl Pts',(-16.851106840707,17.4743379166139,-15.12811997719));
#40093=CARTESIAN_POINT('Ctrl Pts',(-16.9126993772537,17.4119824788001,-15.1325064392025));
#40094=CARTESIAN_POINT('Ctrl Pts',(-16.971457949892,17.352496107113,-15.1366910735956));
#40095=CARTESIAN_POINT('Ctrl Pts',(-17.0332433037703,17.2957807737874,-15.1408757079886));
#40096=CARTESIAN_POINT('Ctrl Pts',(-17.0977635170214,17.2421601965193,-15.1450603423817));
#40097=CARTESIAN_POINT('Ctrl Pts',(-17.1621918937349,17.1886159415061,-15.1492390204656));
#40098=CARTESIAN_POINT('Ctrl Pts',(-17.2293470468518,17.1381579843473,-15.1534176985496));
#40099=CARTESIAN_POINT('Ctrl Pts',(-17.2988998898353,17.0910736631182,-15.1575963766335));
#40100=CARTESIAN_POINT('Ctrl Pts',(-17.3696994175425,17.0431453892699,-15.1618499545189));
#40101=CARTESIAN_POINT('Ctrl Pts',(-17.4429830989498,16.998713228823,-15.1661035324044));
#40102=CARTESIAN_POINT('Ctrl Pts',(-17.5183681022774,16.9580377079855,-15.1703571102898));
#40103=CARTESIAN_POINT('Ctrl Pts',(-17.5922916202138,16.9181507614911,-15.1745282242678));
#40104=CARTESIAN_POINT('Ctrl Pts',(-17.6682352871974,16.881876323378,-15.1786993382457));
#40105=CARTESIAN_POINT('Ctrl Pts',(-17.7458099687319,16.8494156881233,-15.1828704522237));
#40106=CARTESIAN_POINT('Ctrl Pts',(-17.8233586193327,16.8169659453482,-15.187040166544));
#40107=CARTESIAN_POINT('Ctrl Pts',(-17.9025367735083,16.7883276412413,-15.1912098808644));
#40108=CARTESIAN_POINT('Ctrl Pts',(-17.9829338767361,16.7636545649448,-15.1953795951848));
#40109=CARTESIAN_POINT('Ctrl Pts',(-18.0633281190899,16.7389823666223,-15.1995491611288));
#40110=CARTESIAN_POINT('Ctrl Pts',(-18.1449407842156,16.7182752497196,-15.2037187270729));
#40111=CARTESIAN_POINT('Ctrl Pts',(-18.2273459747046,16.7016371927017,-15.2078882930169));
#40112=CARTESIAN_POINT('Ctrl Pts',(-18.3126484300336,16.6844141621243,-15.2122044557558));
#40113=CARTESIAN_POINT('Ctrl Pts',(-18.3987996610347,16.671551755943,-15.2165206184947));
#40114=CARTESIAN_POINT('Ctrl Pts',(-18.485317539171,16.6631073347419,-15.2208367812337));
#40115=CARTESIAN_POINT('Ctrl Pts',(-18.5690171065272,16.6549379896732,-15.2250123454254));
#40116=CARTESIAN_POINT('Ctrl Pts',(-18.6530593280227,16.650903193465,-15.229187909617));
#40117=CARTESIAN_POINT('Ctrl Pts',(-18.7370059866502,16.6510017648357,-15.2333634738087));
#40118=CARTESIAN_POINT('Ctrl Pts',(-18.8251925914406,16.6511053148121,-15.2377499358213));
#40119=CARTESIAN_POINT('Ctrl Pts',(-18.9132731428314,16.6557707277653,-15.2421363978338));
#40120=CARTESIAN_POINT('Ctrl Pts',(-19.0007460413496,16.6649350853868,-15.2465228598464));
#40121=CARTESIAN_POINT('Ctrl Pts',(-19.0882189398677,16.6740994430083,-15.2509093218589));
#40122=CARTESIAN_POINT('Ctrl Pts',(-19.1750836241624,16.6877625800018,-15.2552957838714));
#40123=CARTESIAN_POINT('Ctrl Pts',(-19.2608535512398,16.7058003401833,-15.259682245884));
#40124=CARTESIAN_POINT('Ctrl Pts',(-19.3426770768309,16.7230081562804,-15.263866880277));
#40125=CARTESIAN_POINT('Ctrl Pts',(-19.4238089369641,16.74426092691,-15.2680515146701));
#40126=CARTESIAN_POINT('Ctrl Pts',(-19.5038189245164,16.7694884142285,-15.2722361490631));
#40127=CARTESIAN_POINT('Ctrl Pts',(-19.5837150277545,16.7946799933413,-15.2764148271471));
#40128=CARTESIAN_POINT('Ctrl Pts',(-19.662491995264,16.82383491438,-15.280593505231));
#40129=CARTESIAN_POINT('Ctrl Pts',(-19.7397300928951,16.8568319982964,-15.2847721833149));
#40130=CARTESIAN_POINT('Ctrl Pts',(-19.8183526279165,16.8904205312276,-15.2890257612004));
#40131=CARTESIAN_POINT('Ctrl Pts',(-19.8953801101213,16.9279902241697,-15.2932793390858));
#40132=CARTESIAN_POINT('Ctrl Pts',(-19.9703862586165,16.9693601940757,-15.2975329169713));
#40133=CARTESIAN_POINT('Ctrl Pts',(-20.0439382665606,17.0099281263882,-15.3017040309492));
#40134=CARTESIAN_POINT('Ctrl Pts',(-20.1155461950119,17.0541500666239,-15.3058751449272));
#40135=CARTESIAN_POINT('Ctrl Pts',(-20.1848301560486,17.1018077711361,-15.3100462589051));
#40136=CARTESIAN_POINT('Ctrl Pts',(-20.2540908681831,17.1494494836452,-15.3142159732255));
#40137=CARTESIAN_POINT('Ctrl Pts',(-20.3210287829499,17.2005244102477,-15.3183856875458));
#40138=CARTESIAN_POINT('Ctrl Pts',(-20.3852923626418,17.2547705827075,-15.3225554018662));
#40139=CARTESIAN_POINT('Ctrl Pts',(-20.4495536555597,17.3090148248555,-15.3267249678102));
#40140=CARTESIAN_POINT('Ctrl Pts',(-20.5111404516285,17.3664297911041,-15.3308945337543));
#40141=CARTESIAN_POINT('Ctrl Pts',(-20.5697347912246,17.4267136507031,-15.3350640996983));
#40142=CARTESIAN_POINT('Ctrl Pts',(-20.6303892355173,17.4891170164376,-15.3393802624373));
#40143=CARTESIAN_POINT('Ctrl Pts',(-20.6878365109494,17.5545943914706,-15.3436964251762));
#40144=CARTESIAN_POINT('Ctrl Pts',(-20.7417674193149,17.6227714301973,-15.3480125879151));
#40145=CARTESIAN_POINT('Ctrl Pts',(-20.7939415340127,17.6887276090582,-15.3521881521068));
#40146=CARTESIAN_POINT('Ctrl Pts',(-20.8428246196122,17.7572098587043,-15.3563637162985));
#40147=CARTESIAN_POINT('Ctrl Pts',(-20.8881804708293,17.8278490685766,-15.3605392804901));
#40148=CARTESIAN_POINT('Ctrl Pts',(-20.9358271382683,17.902056097011,-15.3649257425027));
#40149=CARTESIAN_POINT('Ctrl Pts',(-20.9795805961805,17.9786432012264,-15.3693122045152));
#40150=CARTESIAN_POINT('Ctrl Pts',(-21.0192222426251,18.0571545589588,-15.3736986665278));
#40151=CARTESIAN_POINT('Ctrl Pts',(-21.0588638890696,18.1356659166911,-15.3780851285404));
#40152=CARTESIAN_POINT('Ctrl Pts',(-21.0943935591861,18.2161009664615,-15.3824715905529));
#40153=CARTESIAN_POINT('Ctrl Pts',(-21.1256522921828,18.2979833992217,-15.3868580525655));
#40154=CARTESIAN_POINT('Ctrl Pts',(-21.1596866697224,18.3871366489942,-15.3916340140292));
#40155=CARTESIAN_POINT('Ctrl Pts',(-21.188765023978,18.4782809296074,-15.396409975493));
#40156=CARTESIAN_POINT('Ctrl Pts',(-21.2126811308611,18.5708907503299,-15.4011859369568));
#40157=CARTESIAN_POINT('Ctrl Pts',(-21.236499376369,18.6631216245769,-15.4059423558521));
#40158=CARTESIAN_POINT('Ctrl Pts',(-21.2551974088383,18.7568058878157,-15.4106987747474));
#40159=CARTESIAN_POINT('Ctrl Pts',(-21.2686182636666,18.8514026453274,-15.4154551936427));
#40160=CARTESIAN_POINT('Ctrl Pts',(-21.2819450244393,18.9453361818536,-15.4201782651283));
#40161=CARTESIAN_POINT('Ctrl Pts',(-21.2900682365864,19.0401692636774,-15.4249013366139));
#40162=CARTESIAN_POINT('Ctrl Pts',(-21.2928821031966,19.1353535728531,-15.4296244080995));
#40163=CARTESIAN_POINT('Ctrl Pts',(-21.2936100754836,19.1599785991387,-15.4308463086469));
#40164=CARTESIAN_POINT('Ctrl Pts',(-21.2939829474075,19.1846270439602,-15.4320682091942));
#40165=CARTESIAN_POINT('Ctrl Pts',(-21.293999428374,19.2092892327452,-15.4332901097416));
#40166=CARTESIAN_POINT('Ctrl Pts',(-21.2939994283744,19.2092892333484,-15.4332901097715));
#40167=CARTESIAN_POINT('Ctrl Pts',(-21.2940559692553,19.2938972788889,-15.437482057942));
#40168=CARTESIAN_POINT('Ctrl Pts',(-21.2899137324165,19.3785303101354,-15.4416740061124));
#40169=CARTESIAN_POINT('Ctrl Pts',(-21.2815918669692,19.4627452667924,-15.4458659542829));
#40170=CARTESIAN_POINT('Ctrl Pts',(-21.2732695913204,19.546964374574,-15.4500581090829));
#40171=CARTESIAN_POINT('Ctrl Pts',(-21.2607673227297,19.6307649161162,-15.4542502638829));
#40172=CARTESIAN_POINT('Ctrl Pts',(-21.2441560631152,19.7137091990464,-15.4584424186829));
#40173=CARTESIAN_POINT('Ctrl Pts',(-21.2275392030058,19.7966814466854,-15.4626359868702));
#40174=CARTESIAN_POINT('Ctrl Pts',(-21.2068106889623,19.878796418332,-15.4668295550574));
#40175=CARTESIAN_POINT('Ctrl Pts',(-21.1820923104738,19.9596281048684,-15.4710231232446));
#40176=CARTESIAN_POINT('Ctrl Pts',(-21.157341575289,20.0405656011908,-15.4752221808701));
#40177=CARTESIAN_POINT('Ctrl Pts',(-21.1285906849039,20.1202160261787,-15.4794212384956));
#40178=CARTESIAN_POINT('Ctrl Pts',(-21.0960107310932,20.1981703531815,-15.483620296121));
#40179=CARTESIAN_POINT('Ctrl Pts',(-21.0634063961448,20.2761830171356,-15.4878224961022));
#40180=CARTESIAN_POINT('Ctrl Pts',(-21.0269674888695,20.3524966484648,-15.4920246960833));
#40181=CARTESIAN_POINT('Ctrl Pts',(-20.9869114421225,20.4267261344371,-15.4962268960644));
#40182=CARTESIAN_POINT('Ctrl Pts',(-20.9467843119665,20.5010873479597,-15.5004365532642));
#40183=CARTESIAN_POINT('Ctrl Pts',(-20.903027463882,20.5733566470828,-15.504646210464));
#40184=CARTESIAN_POINT('Ctrl Pts',(-20.8559018807143,20.6431775059751,-15.5088558676638));
#40185=CARTESIAN_POINT('Ctrl Pts',(-20.8365799691026,20.6718046841124,-15.5105818648582));
#40186=CARTESIAN_POINT('Ctrl Pts',(-20.8166922183619,20.7000206489315,-15.5123078620525));
#40187=CARTESIAN_POINT('Ctrl Pts',(-20.7962584977301,20.7278025212729,-15.5140338592469));
#40188=CARTESIAN_POINT('Ctrl Pts',(-20.7467174843304,20.7951589334867,-15.5182184936399));
#40189=CARTESIAN_POINT('Ctrl Pts',(-20.6937808669813,20.8602110167103,-15.522403128033));
#40190=CARTESIAN_POINT('Ctrl Pts',(-20.6376906991395,20.9225962497066,-15.526587762426));
#40191=CARTESIAN_POINT('Ctrl Pts',(-20.5816803687091,20.9848926850455,-15.53076644051));
#40192=CARTESIAN_POINT('Ctrl Pts',(-20.5225257086781,21.0445294709031,-15.5349451185939));
#40193=CARTESIAN_POINT('Ctrl Pts',(-20.4605108062945,21.1011747103769,-15.5391237966779));
#40194=CARTESIAN_POINT('Ctrl Pts',(-20.397384331355,21.158835275058,-15.5433773745633));
#40195=CARTESIAN_POINT('Ctrl Pts',(-20.3312943514668,21.213395603145,-15.5476309524487));
#40196=CARTESIAN_POINT('Ctrl Pts',(-20.2625820107879,21.2645425577026,-15.5518845303342));
#40197=CARTESIAN_POINT('Ctrl Pts',(-20.195201792914,21.3146979287411,-15.5560556443121));
#40198=CARTESIAN_POINT('Ctrl Pts',(-20.1253003720614,21.3615708076597,-15.5602267582901));
#40199=CARTESIAN_POINT('Ctrl Pts',(-20.0532336923063,21.4049057557434,-15.564397872268));
#40200=CARTESIAN_POINT('Ctrl Pts',(-19.9811911952218,21.4482261623666,-15.5685675865884));
#40201=CARTESIAN_POINT('Ctrl Pts',(-19.9069852761389,21.4880107590573,-15.5727373009088));
#40202=CARTESIAN_POINT('Ctrl Pts',(-19.8309999421958,21.5240480165406,-15.5769070152291));
#40203=CARTESIAN_POINT('Ctrl Pts',(-19.7550173121369,21.5600839916636,-15.5810765811732));
#40204=CARTESIAN_POINT('Ctrl Pts',(-19.6772558091333,21.5923726963449,-15.5852461471172));
#40205=CARTESIAN_POINT('Ctrl Pts',(-19.5981218233864,21.6207496704736,-15.5894157130613));
#40206=CARTESIAN_POINT('Ctrl Pts',(-19.5162055843229,21.6501243440057,-15.5937318758002));
#40207=CARTESIAN_POINT('Ctrl Pts',(-19.4328190502827,21.6753069180702,-15.5980480385391));
#40208=CARTESIAN_POINT('Ctrl Pts',(-19.3484309915969,21.6961709310559,-15.602364201278));
#40209=CARTESIAN_POINT('Ctrl Pts',(-19.2667918650467,21.7163553010131,-15.6065397654697));
#40210=CARTESIAN_POINT('Ctrl Pts',(-19.1842159325103,21.7324980994093,-15.6107153296614));
#40211=CARTESIAN_POINT('Ctrl Pts',(-19.1011369778118,21.7445371399534,-15.6148908938531));
#40212=CARTESIAN_POINT('Ctrl Pts',(-19.0138619026129,21.7571842438152,-15.6192773558656));
#40213=CARTESIAN_POINT('Ctrl Pts',(-18.9260322359072,21.7653020795901,-15.6236638178781));
#40214=CARTESIAN_POINT('Ctrl Pts',(-18.8381534037015,21.7688803858854,-15.6280502798907));
#40215=CARTESIAN_POINT('Ctrl Pts',(-18.7502745714959,21.7724586921808,-15.6324367419032));
#40216=CARTESIAN_POINT('Ctrl Pts',(-18.6623471531412,21.771497551399,-15.6368232039158));
#40217=CARTESIAN_POINT('Ctrl Pts',(-18.5748705298081,21.7660494734381,-15.6412096659283));
#40218=CARTESIAN_POINT('Ctrl Pts',(-18.491428440693,21.76085266783,-15.6453938186791));
#40219=CARTESIAN_POINT('Ctrl Pts',(-18.4080859286806,21.7515543524013,-15.6495779714299));
#40220=CARTESIAN_POINT('Ctrl Pts',(-18.3252786851367,21.7381618244142,-15.6537621241807));
#40221=CARTESIAN_POINT('Ctrl Pts',(-18.2425831161031,21.7247873576973,-15.6579406341497));
#40222=CARTESIAN_POINT('Ctrl Pts',(-18.1604218322389,21.7073297146472,-15.6621191441187));
#40223=CARTESIAN_POINT('Ctrl Pts',(-18.0792276257493,21.6858481040092,-15.6662976540877));
#40224=CARTESIAN_POINT('Ctrl Pts',(-17.9976813438716,21.6642733445281,-15.6704942829666));
#40225=CARTESIAN_POINT('Ctrl Pts',(-17.9171110155243,21.6386396626604,-15.6746909118456));
#40226=CARTESIAN_POINT('Ctrl Pts',(-17.8379469276443,21.6090594011662,-15.6788875407246));
#40227=CARTESIAN_POINT('Ctrl Pts',(-17.7592671225618,21.5796600956102,-15.6830584969125));
#40228=CARTESIAN_POINT('Ctrl Pts',(-17.6819768376045,21.546362521027,-15.6872294531003));
#40229=CARTESIAN_POINT('Ctrl Pts',(-17.6064837261605,21.509327011595,-15.6914004092882));
#40230=CARTESIAN_POINT('Ctrl Pts',(-17.5302936121915,21.4719495657518,-15.6956098745127));
#40231=CARTESIAN_POINT('Ctrl Pts',(-17.4559344801737,21.4307649580337,-15.6998193397373));
#40232=CARTESIAN_POINT('Ctrl Pts',(-17.3838034107058,21.3859871655388,-15.7040288049618));
#40233=CARTESIAN_POINT('Ctrl Pts',(-17.311672341238,21.3412093730438,-15.7082382701863));
#40234=CARTESIAN_POINT('Ctrl Pts',(-17.2417697449005,21.2928386490813,-15.7124477354108));
#40235=CARTESIAN_POINT('Ctrl Pts',(-17.1744642439897,21.2411350264762,-15.7166572006354));
#40236=CARTESIAN_POINT('',(-21.2939991231355,19.2131188547121,-15.3667098902285));
#40237=CARTESIAN_POINT('Ctrl Pts',(-21.2956374879243,19.2131202107504,-15.3667098902285));
#40238=CARTESIAN_POINT('Ctrl Pts',(-21.2969229026965,19.3573559385303,-15.3738974629702));
#40239=CARTESIAN_POINT('Ctrl Pts',(-21.2201492855026,20.3509180416766,-15.4234769712724));
#40240=CARTESIAN_POINT('Ctrl Pts',(-19.9200692925299,21.9960549863024,-15.515448415135));
#40241=CARTESIAN_POINT('Ctrl Pts',(-17.9391679704133,21.803679489263,-15.6027438707495));
#40242=CARTESIAN_POINT('Ctrl Pts',(-17.2118400551136,21.274998205827,-15.6476473908036));
#40243=CARTESIAN_POINT('Ctrl Pts',(-17.1721129955817,21.2441651167962,-15.6501589752972));
#40244=CARTESIAN_POINT('Ctrl Pts',(-17.1744642439897,21.2411350264762,-14.8500370213225));
#40245=CARTESIAN_POINT('Ctrl Pts',(-17.107823551684,21.1899421052662,-14.8542147110807));
#40246=CARTESIAN_POINT('Ctrl Pts',(-17.0437722960728,21.1355152892009,-14.8583924008388));
#40247=CARTESIAN_POINT('Ctrl Pts',(-16.9826243815685,21.0781591906325,-14.8625700905969));
#40248=CARTESIAN_POINT('Ctrl Pts',(-16.921377573247,21.0207103307072,-14.8667545368845));
#40249=CARTESIAN_POINT('Ctrl Pts',(-16.8630437949045,20.9603230647298,-14.8709389831721));
#40250=CARTESIAN_POINT('Ctrl Pts',(-16.8078981922149,20.8973368068232,-14.8751234294598));
#40251=CARTESIAN_POINT('Ctrl Pts',(-16.7883675541886,20.8750292837606,-14.8766054135491));
#40252=CARTESIAN_POINT('Ctrl Pts',(-16.7692364298418,20.8523960399785,-14.8780873976385));
#40253=CARTESIAN_POINT('Ctrl Pts',(-16.7505157350919,20.8294530178111,-14.8795693817278));
#40254=CARTESIAN_POINT('Ctrl Pts',(-16.697654666154,20.764669488533,-14.8837540161209));
#40255=CARTESIAN_POINT('Ctrl Pts',(-16.6478724513804,20.6971728954314,-14.8879386505139));
#40256=CARTESIAN_POINT('Ctrl Pts',(-16.6014597312931,20.6272881071108,-14.892123284907));
#40257=CARTESIAN_POINT('Ctrl Pts',(-16.5551130739681,20.5575027911364,-14.8963019629909));
#40258=CARTESIAN_POINT('Ctrl Pts',(-16.5121266371783,20.4853364119635,-14.9004806410748));
#40259=CARTESIAN_POINT('Ctrl Pts',(-16.4727509157821,20.4111468989768,-14.9046593191588));
#40260=CARTESIAN_POINT('Ctrl Pts',(-16.4326694128786,20.3356275922887,-14.9089128970442));
#40261=CARTESIAN_POINT('Ctrl Pts',(-16.3963296475344,20.2580122826049,-14.9131664749297));
#40262=CARTESIAN_POINT('Ctrl Pts',(-16.3639497085599,20.1787094688205,-14.9174200528151));
#40263=CARTESIAN_POINT('Ctrl Pts',(-16.3321975178868,20.1009440948281,-14.9215911667931));
#40264=CARTESIAN_POINT('Ctrl Pts',(-16.3042531677129,20.0215565094719,-14.925762280771));
#40265=CARTESIAN_POINT('Ctrl Pts',(-16.2802751807719,19.9409551434874,-14.929933394749));
#40266=CARTESIAN_POINT('Ctrl Pts',(-16.2563052398759,19.8603808240697,-14.9341031090693));
#40267=CARTESIAN_POINT('Ctrl Pts',(-16.2362991499858,19.7785939734879,-14.9382728233897));
#40268=CARTESIAN_POINT('Ctrl Pts',(-16.2203659101292,19.6960192390406,-14.9424425377101));
#40269=CARTESIAN_POINT('Ctrl Pts',(-16.2044332372457,19.6134474429568,-14.9466121036541));
#40270=CARTESIAN_POINT('Ctrl Pts',(-16.1925732125599,19.5300882706131,-14.9507816695982));
#40271=CARTESIAN_POINT('Ctrl Pts',(-16.1848436692124,19.4463762970339,-14.9549512355422));
#40272=CARTESIAN_POINT('Ctrl Pts',(-16.1768423646562,19.3597211137334,-14.9592673982811));
#40273=CARTESIAN_POINT('Ctrl Pts',(-16.1732674495782,19.2726883838098,-14.9635835610201));
#40274=CARTESIAN_POINT('Ctrl Pts',(-16.1741243927921,19.185763605208,-14.967899723759));
#40275=CARTESIAN_POINT('Ctrl Pts',(-16.174953421171,19.1016703921264,-14.9720752879507));
#40276=CARTESIAN_POINT('Ctrl Pts',(-16.1799299313355,19.0176786727672,-14.9762508521424));
#40277=CARTESIAN_POINT('Ctrl Pts',(-16.1890058822548,18.9342240244489,-14.980426416334));
#40278=CARTESIAN_POINT('Ctrl Pts',(-16.198540237879,18.8465542802385,-14.9848128783466));
#40279=CARTESIAN_POINT('Ctrl Pts',(-16.2125989501167,18.7594778642492,-14.9891993403591));
#40280=CARTESIAN_POINT('Ctrl Pts',(-16.2310658163554,18.6734867700759,-14.9935858023717));
#40281=CARTESIAN_POINT('Ctrl Pts',(-16.2495326825942,18.5874956759026,-14.9979722643842));
#40282=CARTESIAN_POINT('Ctrl Pts',(-16.2724074784504,18.5025904439986,-15.0023587263968));
#40283=CARTESIAN_POINT('Ctrl Pts',(-16.2995147249237,18.4192415485537,-15.0067451884093));
#40284=CARTESIAN_POINT('Ctrl Pts',(-16.3253747268042,18.3397276593411,-15.0109298228024));
#40285=CARTESIAN_POINT('Ctrl Pts',(-16.3551825113727,18.2613340692511,-15.0151144571954));
#40286=CARTESIAN_POINT('Ctrl Pts',(-16.3888222337464,18.1844810061817,-15.0192990915885));
#40287=CARTESIAN_POINT('Ctrl Pts',(-16.4224140741391,18.1077373339352,-15.0234777696724));
#40288=CARTESIAN_POINT('Ctrl Pts',(-16.4598268355143,18.0325302510435,-15.0276564477563));
#40289=CARTESIAN_POINT('Ctrl Pts',(-16.5008951440191,17.9592641244279,-15.0318351258403));
#40290=CARTESIAN_POINT('Ctrl Pts',(-16.5426995724385,17.8846847551482,-15.0360887037257));
#40291=CARTESIAN_POINT('Ctrl Pts',(-16.5882917392508,17.8121170683453,-15.0403422816112));
#40292=CARTESIAN_POINT('Ctrl Pts',(-16.6374462088683,17.7419655548996,-15.0445958594966));
#40293=CARTESIAN_POINT('Ctrl Pts',(-16.6856477231752,17.6731740654315,-15.0487669734745));
#40294=CARTESIAN_POINT('Ctrl Pts',(-16.7372743723595,17.606706294976,-15.0529380874525));
#40295=CARTESIAN_POINT('Ctrl Pts',(-16.792068536157,17.5429166118756,-15.0571092014304));
#40296=CARTESIAN_POINT('Ctrl Pts',(-16.8468443132437,17.4791483340195,-15.0612789157508));
#40297=CARTESIAN_POINT('Ctrl Pts',(-16.9047851945213,17.4180567074448,-15.0654486300712));
#40298=CARTESIAN_POINT('Ctrl Pts',(-16.9655931179199,17.3599632366126,-15.0696183443915));
#40299=CARTESIAN_POINT('Ctrl Pts',(-17.0263988775115,17.3018718329955,-15.0737879103356));
#40300=CARTESIAN_POINT('Ctrl Pts',(-17.0900711431583,17.2467786901665,-15.0779574762796));
#40301=CARTESIAN_POINT('Ctrl Pts',(-17.1562758100197,17.1949676638628,-15.0821270422237));
#40302=CARTESIAN_POINT('Ctrl Pts',(-17.2248081512957,17.14133502579,-15.0864432049626));
#40303=CARTESIAN_POINT('Ctrl Pts',(-17.2960538702051,17.0912199219507,-15.0907593677015));
#40304=CARTESIAN_POINT('Ctrl Pts',(-17.3696076999732,17.0448897415811,-15.0950755304404));
#40305=CARTESIAN_POINT('Ctrl Pts',(-17.440765521473,17.000068761964,-15.0992510946321));
#40306=CARTESIAN_POINT('Ctrl Pts',(-17.5140829560414,16.9587900948024,-15.1034266588238));
#40307=CARTESIAN_POINT('Ctrl Pts',(-17.5891677483861,16.9212491149331,-15.1076022230154));
#40308=CARTESIAN_POINT('Ctrl Pts',(-17.6680448950951,16.8818120294158,-15.111988685028));
#40309=CARTESIAN_POINT('Ctrl Pts',(-17.74887209509,16.8465003691281,-15.1163751470405));
#40310=CARTESIAN_POINT('Ctrl Pts',(-17.831172761347,16.8154827328641,-15.120761609053));
#40311=CARTESIAN_POINT('Ctrl Pts',(-17.913473427604,16.7844650966001,-15.1251480710656));
#40312=CARTESIAN_POINT('Ctrl Pts',(-17.9972469842329,16.7577415882257,-15.1295345330781));
#40313=CARTESIAN_POINT('Ctrl Pts',(-18.0820028534396,16.7354193164275,-15.1339209950906));
#40314=CARTESIAN_POINT('Ctrl Pts',(-18.1628589794658,16.7141241254443,-15.1381056294837));
#40315=CARTESIAN_POINT('Ctrl Pts',(-18.2449099711144,16.6967547916185,-15.1422902638767));
#40316=CARTESIAN_POINT('Ctrl Pts',(-18.3277397785879,16.6834413691275,-15.1464748982698));
#40317=CARTESIAN_POINT('Ctrl Pts',(-18.4104516880828,16.6701468966455,-15.1506535763537));
#40318=CARTESIAN_POINT('Ctrl Pts',(-18.4939397611591,16.66089694071,-15.1548322544377));
#40319=CARTESIAN_POINT('Ctrl Pts',(-18.5777744754985,16.6557713242267,-15.1590109325216));
#40320=CARTESIAN_POINT('Ctrl Pts',(-18.6631118668416,16.6505538347517,-15.163264510407));
#40321=CARTESIAN_POINT('Ctrl Pts',(-18.7488079825292,16.6496101194126,-15.1675180882925));
#40322=CARTESIAN_POINT('Ctrl Pts',(-18.8344006857351,16.652969565798,-15.1717716661779));
#40323=CARTESIAN_POINT('Ctrl Pts',(-18.9183340073688,16.6562638827597,-15.1759427801559));
#40324=CARTESIAN_POINT('Ctrl Pts',(-19.0021674095958,16.6636959811426,-15.1801138941338));
#40325=CARTESIAN_POINT('Ctrl Pts',(-19.085463479757,16.6752410559367,-15.1842850081118));
#40326=CARTESIAN_POINT('Ctrl Pts',(-19.1687315991175,16.6867822566694,-15.1884547224321));
#40327=CARTESIAN_POINT('Ctrl Pts',(-19.2514622892072,16.70243362971,-15.1926244367525));
#40328=CARTESIAN_POINT('Ctrl Pts',(-19.3332238803081,16.7221185762941,-15.1967941510729));
#40329=CARTESIAN_POINT('Ctrl Pts',(-19.4149825619807,16.7418028224032,-15.2009637170169));
#40330=CARTESIAN_POINT('Ctrl Pts',(-19.4957717661756,16.7655202481684,-15.205133282961));
#40331=CARTESIAN_POINT('Ctrl Pts',(-19.5751719705257,16.7931435700187,-15.209302848905));
#40332=CARTESIAN_POINT('Ctrl Pts',(-19.6573637881101,16.8217380937883,-15.2136190116439));
#40333=CARTESIAN_POINT('Ctrl Pts',(-19.7380666159157,16.8545181133117,-15.2179351743828));
#40334=CARTESIAN_POINT('Ctrl Pts',(-19.8168362586914,16.891287596088,-15.2222513371218));
#40335=CARTESIAN_POINT('Ctrl Pts',(-19.8930399886387,16.9268593168303,-15.2264269013134));
#40336=CARTESIAN_POINT('Ctrl Pts',(-19.9674341519876,16.966164316944,-15.2306024655051));
#40337=CARTESIAN_POINT('Ctrl Pts',(-20.0396421490694,17.0089785244977,-15.2347780296968));
#40338=CARTESIAN_POINT('Ctrl Pts',(-20.1154972004257,17.0539551758939,-15.2391644917093));
#40339=CARTESIAN_POINT('Ctrl Pts',(-20.1889389488847,17.1028045279329,-15.2435509537219));
#40340=CARTESIAN_POINT('Ctrl Pts',(-20.2595676620248,17.1552171056787,-15.2479374157344));
#40341=CARTESIAN_POINT('Ctrl Pts',(-20.330196375165,17.2076296834245,-15.252323877747));
#40342=CARTESIAN_POINT('Ctrl Pts',(-20.3980116539332,17.2636050588652,-15.2567103397595));
#40343=CARTESIAN_POINT('Ctrl Pts',(-20.4626578964189,17.3227887096121,-15.2610968017721));
#40344=CARTESIAN_POINT('Ctrl Pts',(-20.5234100187947,17.3784072924496,-15.2652190348167));
#40345=CARTESIAN_POINT('Ctrl Pts',(-20.5816044022757,17.4370795204071,-15.2693412678613));
#40346=CARTESIAN_POINT('Ctrl Pts',(-20.6369112461388,17.498537215202,-15.2734635009059));
#40347=CARTESIAN_POINT('Ctrl Pts',(-20.6921256485485,17.5598921878337,-15.2775788439313));
#40348=CARTESIAN_POINT('Ctrl Pts',(-20.7444617859859,17.6240230272318,-15.2816941869567));
#40349=CARTESIAN_POINT('Ctrl Pts',(-20.793624524071,17.6906228034315,-15.2858095299821));
#40350=CARTESIAN_POINT('Ctrl Pts',(-20.8427410076366,17.7571599195604,-15.2899210011074));
#40351=CARTESIAN_POINT('Ctrl Pts',(-20.8886897335868,17.8261609852054,-15.2940324722326));
#40352=CARTESIAN_POINT('Ctrl Pts',(-20.9312146121396,17.8972846776412,-15.2981439433579));
#40353=CARTESIAN_POINT('Ctrl Pts',(-20.9737131282073,17.9683642783043,-15.3022528656552));
#40354=CARTESIAN_POINT('Ctrl Pts',(-21.0127917657825,18.0415634879279,-15.3063617879526));
#40355=CARTESIAN_POINT('Ctrl Pts',(-21.0482376124066,18.1165118669796,-15.3104707102499));
#40356=CARTESIAN_POINT('Ctrl Pts',(-21.0836728562224,18.1914378269505,-15.3145784034579));
#40357=CARTESIAN_POINT('Ctrl Pts',(-21.1154772648512,18.2681114878987,-15.3186860966658));
#40358=CARTESIAN_POINT('Ctrl Pts',(-21.1434845038954,18.3461390715913,-15.3227937898737));
#40359=CARTESIAN_POINT('Ctrl Pts',(-21.1715053065244,18.4242044431482,-15.3269034723903));
#40360=CARTESIAN_POINT('Ctrl Pts',(-21.1957251016689,18.5036246009545,-15.331013154907));
#40361=CARTESIAN_POINT('Ctrl Pts',(-21.2160265895475,18.5839880313906,-15.3351228374236));
#40362=CARTESIAN_POINT('Ctrl Pts',(-21.2363332616047,18.6643719833958,-15.339233569387));
#40363=CARTESIAN_POINT('Ctrl Pts',(-21.2527195357628,18.7456992225568,-15.3433443013503));
#40364=CARTESIAN_POINT('Ctrl Pts',(-21.2651191757883,18.827547632741,-15.3474550333136));
#40365=CARTESIAN_POINT('Ctrl Pts',(-21.2775338661873,18.9094953884813,-15.3515707547807));
#40366=CARTESIAN_POINT('Ctrl Pts',(-21.2859522113273,18.9919651056503,-15.3556864762478));
#40367=CARTESIAN_POINT('Ctrl Pts',(-21.2903598951031,19.0745299054426,-15.3598021977149));
#40368=CARTESIAN_POINT('Ctrl Pts',(-21.292825799276,19.1207212600627,-15.3621047618861));
#40369=CARTESIAN_POINT('Ctrl Pts',(-21.294037342402,19.1669423575626,-15.3644073260573));
#40370=CARTESIAN_POINT('Ctrl Pts',(-21.2939991231355,19.2131188547121,-15.3667098902285));
#40371=CARTESIAN_POINT('Origin',(-18.734,19.211,1.76670989022852));
#40372=CARTESIAN_POINT('',(-17.1770151058749,21.2378231662188,-14.0501277782861));
#40373=CARTESIAN_POINT('',(-17.1718944362858,21.2444720185936,-14.1167030376167));
#40374=CARTESIAN_POINT('',(-17.1744642439897,21.2411350264762,1.76670989022852));
#40375=CARTESIAN_POINT('',(-21.2941234937244,19.2098698166564,-14.6332901097715));
#40376=CARTESIAN_POINT('Ctrl Pts',(-17.1718944362858,21.2444720185936,-14.1167030376167));
#40377=CARTESIAN_POINT('Ctrl Pts',(-16.5081485897239,20.7333156289599,-14.1585606225553));
#40378=CARTESIAN_POINT('Ctrl Pts',(-15.721016264389,18.9872885886645,-14.2428101430544));
#40379=CARTESIAN_POINT('Ctrl Pts',(-17.2790524810781,16.55649072778,-14.3694515991139));
#40380=CARTESIAN_POINT('Ctrl Pts',(-20.1784867160069,16.5507838647211,-14.4966274057954));
#40381=CARTESIAN_POINT('Ctrl Pts',(-21.2671018326456,18.2345793421635,-14.5845735760146));
#40382=CARTESIAN_POINT('Ctrl Pts',(-21.2979709281649,19.1465375840163,-14.6301278106733));
#40383=CARTESIAN_POINT('Ctrl Pts',(-21.2976211493107,19.2098682725933,-14.6332901097715));
#40384=CARTESIAN_POINT('Ctrl Pts',(-21.2939997505486,19.2098698712836,-14.6332901097715));
#40385=CARTESIAN_POINT('Ctrl Pts',(-21.2940362985033,19.2926593390013,-14.6374299052976));
#40386=CARTESIAN_POINT('Ctrl Pts',(-21.2900525381051,19.3756125071059,-14.6415697008237));
#40387=CARTESIAN_POINT('Ctrl Pts',(-21.2820270867845,19.4583013647603,-14.6457094963498));
#40388=CARTESIAN_POINT('Ctrl Pts',(-21.2740124509524,19.5408787868902,-14.6498437128862));
#40389=CARTESIAN_POINT('Ctrl Pts',(-21.2619669829652,19.623192141297,-14.6539779294226));
#40390=CARTESIAN_POINT('Ctrl Pts',(-21.2459213201026,19.7048130026779,-14.658112145959));
#40391=CARTESIAN_POINT('Ctrl Pts',(-21.2298921267197,19.7863500873319,-14.6622421190811));
#40392=CARTESIAN_POINT('Ctrl Pts',(-21.209870984755,19.8671956313595,-14.6663720922032));
#40393=CARTESIAN_POINT('Ctrl Pts',(-21.1859402178855,19.9469274202771,-14.6705020653253));
#40394=CARTESIAN_POINT('Ctrl Pts',(-21.1620224032908,20.026616055206,-14.6746298031431));
#40395=CARTESIAN_POINT('Ctrl Pts',(-21.1341992976676,20.105191681447,-14.6787575409609));
#40396=CARTESIAN_POINT('Ctrl Pts',(-21.1026037847566,20.1822446194635,-14.6828852787786));
#40397=CARTESIAN_POINT('Ctrl Pts',(-21.0710154147152,20.2592801379466,-14.6870120834293));
#40398=CARTESIAN_POINT('Ctrl Pts',(-21.0356565094082,20.3347932165768,-14.69113888808));
#40399=CARTESIAN_POINT('Ctrl Pts',(-20.9967085276621,20.4083930511094,-14.6952656927306));
#40400=CARTESIAN_POINT('Ctrl Pts',(-20.9577570758468,20.481999443017,-14.6993928650588));
#40401=CARTESIAN_POINT('Ctrl Pts',(-20.915216134864,20.5536918375766,-14.703520037387));
#40402=CARTESIAN_POINT('Ctrl Pts',(-20.8693129406042,20.6231043324372,-14.7076472097152));
#40403=CARTESIAN_POINT('Ctrl Pts',(-20.82336222789,20.6925886823078,-14.7117786544443));
#40404=CARTESIAN_POINT('Ctrl Pts',(-20.7740425759679,20.7597880294049,-14.7159100991735));
#40405=CARTESIAN_POINT('Ctrl Pts',(-20.7216239583874,20.8243663564251,-14.7200415439026));
#40406=CARTESIAN_POINT('Ctrl Pts',(-20.6691749218121,20.8889821588287,-14.7241753861462));
#40407=CARTESIAN_POINT('Ctrl Pts',(-20.6136236562298,20.9509735655346,-14.7283092283899));
#40408=CARTESIAN_POINT('Ctrl Pts',(-20.5552780488243,21.0100403744415,-14.7324430706335));
#40409=CARTESIAN_POINT('Ctrl Pts',(-20.496836459412,21.0692043517748,-14.7365837132944));
#40410=CARTESIAN_POINT('Ctrl Pts',(-20.4355917013479,21.1254338132407,-14.7407243559553));
#40411=CARTESIAN_POINT('Ctrl Pts',(-20.3718854170609,21.1784682616447,-14.7448649986162));
#40412=CARTESIAN_POINT('Ctrl Pts',(-20.340529452726,21.2045715933849,-14.7469030054635));
#40413=CARTESIAN_POINT('Ctrl Pts',(-20.3085776248467,21.2299015689541,-14.7489410123109));
#40414=CARTESIAN_POINT('Ctrl Pts',(-20.2760730898184,21.2544310817001,-14.7509790191583));
#40415=CARTESIAN_POINT('Ctrl Pts',(-20.2093316088543,21.3047974692387,-14.7551636535513));
#40416=CARTESIAN_POINT('Ctrl Pts',(-20.1399957689001,21.3519843348468,-14.7593482879444));
#40417=CARTESIAN_POINT('Ctrl Pts',(-20.0684012262927,21.3957135664129,-14.7635329223374));
#40418=CARTESIAN_POINT('Ctrl Pts',(-19.9969085896549,21.4393805548305,-14.7677116004214));
#40419=CARTESIAN_POINT('Ctrl Pts',(-19.9231640255691,21.4795994471402,-14.7718902785053));
#40420=CARTESIAN_POINT('Ctrl Pts',(-19.8475347050064,21.5161335017188,-14.7760689565893));
#40421=CARTESIAN_POINT('Ctrl Pts',(-19.7705497832267,21.553322402969,-14.7803225344747));
#40422=CARTESIAN_POINT('Ctrl Pts',(-19.6916122567004,21.5866927752846,-14.7845761123602));
#40423=CARTESIAN_POINT('Ctrl Pts',(-19.6111386006649,21.6160421774313,-14.7888296902456));
#40424=CARTESIAN_POINT('Ctrl Pts',(-19.532225083483,21.6448225841468,-14.7930008042235));
#40425=CARTESIAN_POINT('Ctrl Pts',(-19.4518349191,21.6697363732163,-14.7971719182015));
#40426=CARTESIAN_POINT('Ctrl Pts',(-19.3703822558334,21.6906406240543,-14.8013430321794));
#40427=CARTESIAN_POINT('Ctrl Pts',(-19.2889569247947,21.711537860269,-14.8055127464998));
#40428=CARTESIAN_POINT('Ctrl Pts',(-19.2064702481715,21.728428116053,-14.8096824608202));
#40429=CARTESIAN_POINT('Ctrl Pts',(-19.1233507011891,21.7412185738555,-14.8138521751405));
#40430=CARTESIAN_POINT('Ctrl Pts',(-19.0402341119568,21.7540085765187,-14.8180217410846));
#40431=CARTESIAN_POINT('Ctrl Pts',(-18.9564851519519,21.7626990021399,-14.8221913070286));
#40432=CARTESIAN_POINT('Ctrl Pts',(-18.8725402767196,21.7672485387236,-14.8263608729727));
#40433=CARTESIAN_POINT('Ctrl Pts',(-18.7856440032314,21.7719580314011,-14.8306770357116));
#40434=CARTESIAN_POINT('Ctrl Pts',(-18.6985383080786,21.7722300013651,-14.8349931984505));
#40435=CARTESIAN_POINT('Ctrl Pts',(-18.6117085473887,21.7680773943348,-14.8393093611894));
#40436=CARTESIAN_POINT('Ctrl Pts',(-18.5277072570202,21.7640600580418,-14.8434849253811));
#40437=CARTESIAN_POINT('Ctrl Pts',(-18.4439646643002,21.7559020718402,-14.8476604895728));
#40438=CARTESIAN_POINT('Ctrl Pts',(-18.3609142114856,21.7436679597627,-14.8518360537645));
#40439=CARTESIAN_POINT('Ctrl Pts',(-18.2736690777334,21.7308159317681,-14.856222515777));
#40440=CARTESIAN_POINT('Ctrl Pts',(-18.187188413865,21.713465300997,-14.8606089777895));
#40441=CARTESIAN_POINT('Ctrl Pts',(-18.1019594530762,21.6917508434029,-14.8649954398021));
#40442=CARTESIAN_POINT('Ctrl Pts',(-18.0167304922875,21.6700363858088,-14.8693819018146));
#40443=CARTESIAN_POINT('Ctrl Pts',(-17.932753766134,21.6439583461084,-14.8737683638271));
#40444=CARTESIAN_POINT('Ctrl Pts',(-17.8504927560607,21.613709917969,-14.8781548258396));
#40445=CARTESIAN_POINT('Ctrl Pts',(-17.7720269461522,21.5848570335916,-14.8823389137099));
#40446=CARTESIAN_POINT('Ctrl Pts',(-17.6948300019125,21.5521027093235,-14.8865230015802));
#40447=CARTESIAN_POINT('Ctrl Pts',(-17.6193172941086,21.5155785873314,-14.8907070894505));
#40448=CARTESIAN_POINT('Ctrl Pts',(-17.5409562028295,21.4776767541096,-14.8950490035609));
#40449=CARTESIAN_POINT('Ctrl Pts',(-17.4644094236413,21.4357151583199,-14.8993909176712));
#40450=CARTESIAN_POINT('Ctrl Pts',(-17.3901227910456,21.3898974384429,-14.9037328317816));
#40451=CARTESIAN_POINT('Ctrl Pts',(-17.31583615845,21.3440797185659,-14.9080747458919));
#40452=CARTESIAN_POINT('Ctrl Pts',(-17.2438101840022,21.2944061003571,-14.9124166600022));
#40453=CARTESIAN_POINT('Ctrl Pts',(-17.1744642439897,21.2411350264762,-14.9167585741126));
#40454=CARTESIAN_POINT('',(-21.2936354898062,19.2115601738724,-14.5667099150531));
#40455=CARTESIAN_POINT('Ctrl Pts',(-21.2939999386838,19.2115603024813,-14.5667099174733));
#40456=CARTESIAN_POINT('Ctrl Pts',(-21.2939802627011,19.301459091566,-14.5711571992722));
#40457=CARTESIAN_POINT('Ctrl Pts',(-21.2892209204019,19.3912344818061,-14.5756044810712));
#40458=CARTESIAN_POINT('Ctrl Pts',(-21.2797861099485,19.4803939167712,-14.5800517628701));
#40459=CARTESIAN_POINT('Ctrl Pts',(-21.270316767046,19.5698796851229,-14.584515322212));
#40460=CARTESIAN_POINT('Ctrl Pts',(-21.2561377674645,19.6587446305213,-14.5889788815539));
#40461=CARTESIAN_POINT('Ctrl Pts',(-21.2373647797492,19.7465042292186,-14.5934424408958));
#40462=CARTESIAN_POINT('Ctrl Pts',(-21.2185553401057,19.8344342326829,-14.5979146672303));
#40463=CARTESIAN_POINT('Ctrl Pts',(-21.1951342035234,19.9212542602487,-14.6023868935647));
#40464=CARTESIAN_POINT('Ctrl Pts',(-21.1672666877215,20.0064955854214,-14.6068591198992));
#40465=CARTESIAN_POINT('Ctrl Pts',(-21.1393161596827,20.0919908289243,-14.6113446681786));
#40466=CARTESIAN_POINT('Ctrl Pts',(-21.1068928974848,20.1758976314735,-14.615830216458));
#40467=CARTESIAN_POINT('Ctrl Pts',(-21.0702104967872,20.2577666954491,-14.6203157647375));
#40468=CARTESIAN_POINT('Ctrl Pts',(-21.0568477853949,20.2875900617789,-14.6219497659466));
#40469=CARTESIAN_POINT('Ctrl Pts',(-21.0429203172376,20.3171432681498,-14.6235837671558));
#40470=CARTESIAN_POINT('Ctrl Pts',(-21.0284398795323,20.3464054955,-14.6252177683649));
#40471=CARTESIAN_POINT('Ctrl Pts',(-20.9913558570061,20.4213452949944,-14.6294024027579));
#40472=CARTESIAN_POINT('Ctrl Pts',(-20.9505274948145,20.4946058152548,-14.633587037151));
#40473=CARTESIAN_POINT('Ctrl Pts',(-20.9061301751472,20.5657879916116,-14.637771671544));
#40474=CARTESIAN_POINT('Ctrl Pts',(-20.8617960495691,20.636868848951,-14.641950349628));
#40475=CARTESIAN_POINT('Ctrl Pts',(-20.8139032983065,20.7058768514385,-14.6461290277119));
#40476=CARTESIAN_POINT('Ctrl Pts',(-20.7626740190628,20.7724357893874,-14.6503077057959));
#40477=CARTESIAN_POINT('Ctrl Pts',(-20.7105264918065,20.8401877484639,-14.6545612836813));
#40478=CARTESIAN_POINT('Ctrl Pts',(-20.6549218593555,20.9054015483268,-14.6588148615668));
#40479=CARTESIAN_POINT('Ctrl Pts',(-20.5961416680528,20.9677095400496,-14.6630684394522));
#40480=CARTESIAN_POINT('Ctrl Pts',(-20.5385010454587,21.0288095697688,-14.6672395534301));
#40481=CARTESIAN_POINT('Ctrl Pts',(-20.4778072242622,21.0871151053885,-14.6714106674081));
#40482=CARTESIAN_POINT('Ctrl Pts',(-20.4143663508875,21.1423127470208,-14.6755817813861));
#40483=CARTESIAN_POINT('Ctrl Pts',(-20.3509467657105,21.1974918665513,-14.6797514957064));
#40484=CARTESIAN_POINT('Ctrl Pts',(-20.2847823058331,21.2495648615672,-14.6839212100268));
#40485=CARTESIAN_POINT('Ctrl Pts',(-20.2162143833073,21.2982566976577,-14.6880909243472));
#40486=CARTESIAN_POINT('Ctrl Pts',(-20.1476489007224,21.3469468010838,-14.6922604902912));
#40487=CARTESIAN_POINT('Ctrl Pts',(-20.0766805011099,21.3922557191444,-14.6964300562353));
#40488=CARTESIAN_POINT('Ctrl Pts',(-20.0036808175629,21.433950881489,-14.7005996221793));
#40489=CARTESIAN_POINT('Ctrl Pts',(-19.9281145551974,21.477111994305,-14.7049157849182));
#40490=CARTESIAN_POINT('Ctrl Pts',(-19.850371969323,21.5164002423867,-14.7092319476572));
#40491=CARTESIAN_POINT('Ctrl Pts',(-19.7708927266886,21.5516096371117,-14.7135481103961));
#40492=CARTESIAN_POINT('Ctrl Pts',(-19.6940025120233,21.5856720895069,-14.7177236745878));
#40493=CARTESIAN_POINT('Ctrl Pts',(-19.6154875027973,21.6159172197028,-14.7218992387794));
#40494=CARTESIAN_POINT('Ctrl Pts',(-19.5357640795052,21.6422084157503,-14.7260748029711));
#40495=CARTESIAN_POINT('Ctrl Pts',(-19.4520140156271,21.6698275176088,-14.7304612649837));
#40496=CARTESIAN_POINT('Ctrl Pts',(-19.3669308187544,21.6930826078309,-14.7348477269962));
#40497=CARTESIAN_POINT('Ctrl Pts',(-19.2810104439706,21.7118757614458,-14.7392341890088));
#40498=CARTESIAN_POINT('Ctrl Pts',(-19.1950900691869,21.7306689150607,-14.7436206510213));
#40499=CARTESIAN_POINT('Ctrl Pts',(-19.1083331013483,21.7450001125529,-14.7480071130338));
#40500=CARTESIAN_POINT('Ctrl Pts',(-19.021240449396,21.7548342957494,-14.7523935750464));
#40501=CARTESIAN_POINT('Ctrl Pts',(-18.9381783893849,21.7642133592698,-14.756577034417));
#40502=CARTESIAN_POINT('Ctrl Pts',(-18.8545019430903,21.7695373443223,-14.7607604937876));
#40503=CARTESIAN_POINT('Ctrl Pts',(-18.7706412277764,21.7707377639959,-14.7649439531582));
#40504=CARTESIAN_POINT('Ctrl Pts',(-18.6868897531641,21.7719366199495,-14.7691219629684));
#40505=CARTESIAN_POINT('Ctrl Pts',(-18.6029549415235,21.7690225671098,-14.7732999727786));
#40506=CARTESIAN_POINT('Ctrl Pts',(-18.5192731319562,21.7619787086803,-14.7774779825888));
#40507=CARTESIAN_POINT('Ctrl Pts',(-18.4356752189388,21.7549419121848,-14.7816518036677));
#40508=CARTESIAN_POINT('Ctrl Pts',(-18.3523302600542,21.7437835702215,-14.7858256247467));
#40509=CARTESIAN_POINT('Ctrl Pts',(-18.2696743384136,21.7285388139992,-14.7899994458256));
#40510=CARTESIAN_POINT('Ctrl Pts',(-18.1870764857601,21.7133047678086,-14.7941703346336));
#40511=CARTESIAN_POINT('Ctrl Pts',(-18.1051671597161,21.6939900938571,-14.7983412234415));
#40512=CARTESIAN_POINT('Ctrl Pts',(-18.0243757041524,21.6706815563692,-14.8025121122494));
#40513=CARTESIAN_POINT('Ctrl Pts',(-17.9435959999342,21.6473764091739,-14.8066823943898));
#40514=CARTESIAN_POINT('Ctrl Pts',(-17.8639342884426,21.6200786673611,-14.8108526765302));
#40515=CARTESIAN_POINT('Ctrl Pts',(-17.7858071130466,21.5889256189231,-14.8150229586706));
#40516=CARTESIAN_POINT('Ctrl Pts',(-17.7076898406079,21.5577765192687,-14.8191927122097));
#40517=CARTESIAN_POINT('Ctrl Pts',(-17.6311071429207,21.5227732602774,-14.8233624657488));
#40518=CARTESIAN_POINT('Ctrl Pts',(-17.556456222726,21.4841015491181,-14.8275322192879));
#40519=CARTESIAN_POINT('Ctrl Pts',(-17.4817531860181,21.4454028398357,-14.831704883883));
#40520=CARTESIAN_POINT('Ctrl Pts',(-17.408985028084,21.403030778009,-14.8358775484782));
#40521=CARTESIAN_POINT('Ctrl Pts',(-17.3385243274801,21.3572170550541,-14.8400502130733));
#40522=CARTESIAN_POINT('Ctrl Pts',(-17.2823110461754,21.3206670395985,-14.8433791491564));
#40523=CARTESIAN_POINT('Ctrl Pts',(-17.2275659863547,21.2819274195164,-14.8467080852395));
#40524=CARTESIAN_POINT('Ctrl Pts',(-17.1744642439897,21.2411350264762,-14.8500370213225));
#40525=CARTESIAN_POINT('Ctrl Pts',(-17.1770151058749,21.2378231662188,-14.0501277782861));
#40526=CARTESIAN_POINT('Ctrl Pts',(-16.8231471434315,20.9653100508297,-14.0722566994038));
#40527=CARTESIAN_POINT('Ctrl Pts',(-15.9876140958797,19.9142911360265,-14.136777556082));
#40528=CARTESIAN_POINT('Ctrl Pts',(-16.2435265724331,17.4902926599815,-14.2436903483207));
#40529=CARTESIAN_POINT('Ctrl Pts',(-18.8327965343378,16.1855197260249,-14.3708661550021));
#40530=CARTESIAN_POINT('Ctrl Pts',(-20.9482576099774,17.4308694729993,-14.4785393356381));
#40531=CARTESIAN_POINT('Ctrl Pts',(-21.2889976010488,18.7496082874005,-14.5438205807135));
#40532=CARTESIAN_POINT('Ctrl Pts',(-21.2898971100035,19.211558854651,-14.5667098902285));
#40533=CARTESIAN_POINT('Origin',(-18.734,19.211,1.76670989022852));
#40534=CARTESIAN_POINT('',(-17.1744642439897,21.2411350264762,-13.2501880045741));
#40535=CARTESIAN_POINT('',(-17.1744642439897,21.2411350264762,-13.3166223692584));
#40536=CARTESIAN_POINT('',(-17.1744642439897,21.2411350264762,1.76670989022852));
#40537=CARTESIAN_POINT('',(-21.2939989424941,19.2133268925441,-13.8332901097715));
#40538=CARTESIAN_POINT('Ctrl Pts',(-17.1744642439897,21.2411350264762,-13.3166223692584));
#40539=CARTESIAN_POINT('Ctrl Pts',(-17.1077897971069,21.1899161752323,-13.3207986424165));
#40540=CARTESIAN_POINT('Ctrl Pts',(-17.0436959027707,21.1354513017812,-13.3249749155745));
#40541=CARTESIAN_POINT('Ctrl Pts',(-16.9824997973296,21.0780423241173,-13.3291511887325));
#40542=CARTESIAN_POINT('Ctrl Pts',(-16.9211960076474,21.0205323262636,-13.3333348107047));
#40543=CARTESIAN_POINT('Ctrl Pts',(-16.8628005132386,20.960068206441,-13.3375184326769));
#40544=CARTESIAN_POINT('Ctrl Pts',(-16.8075924183714,20.8969874938575,-13.3417020546491));
#40545=CARTESIAN_POINT('Ctrl Pts',(-16.7620957686836,20.8450030685775,-13.3451497516536));
#40546=CARTESIAN_POINT('Ctrl Pts',(-16.7187631096113,20.7912423596748,-13.348597448658));
#40547=CARTESIAN_POINT('Ctrl Pts',(-16.6777284049171,20.7359088914604,-13.3520451456625));
#40548=CARTESIAN_POINT('Ctrl Pts',(-16.6279226254793,20.6687480203406,-13.3562297800555));
#40549=CARTESIAN_POINT('Ctrl Pts',(-16.5813179797009,20.5990195040796,-13.3604144144486));
#40550=CARTESIAN_POINT('Ctrl Pts',(-16.5381897594128,20.5270613159471,-13.3645990488416));
#40551=CARTESIAN_POINT('Ctrl Pts',(-16.4951229268081,20.4552055513886,-13.3687777269256));
#40552=CARTESIAN_POINT('Ctrl Pts',(-16.4555229253634,20.3811268100629,-13.3729564050095));
#40553=CARTESIAN_POINT('Ctrl Pts',(-16.4196234139921,20.3051942323638,-13.3771350830935));
#40554=CARTESIAN_POINT('Ctrl Pts',(-16.38308042968,20.2279006177814,-13.3813886609789));
#40555=CARTESIAN_POINT('Ctrl Pts',(-16.350372190068,20.1486864403631,-13.3856422388643));
#40556=CARTESIAN_POINT('Ctrl Pts',(-16.3216976420462,20.0679698558353,-13.3898958167498));
#40557=CARTESIAN_POINT('Ctrl Pts',(-16.2935790060915,19.9888181198039,-13.3940669307277));
#40558=CARTESIAN_POINT('Ctrl Pts',(-16.2693392165556,19.9082221644551,-13.3982380447057));
#40559=CARTESIAN_POINT('Ctrl Pts',(-16.2491177212504,19.8265973202963,-13.4024091586836));
#40560=CARTESIAN_POINT('Ctrl Pts',(-16.2289030114632,19.7449998661423,-13.406578873004));
#40561=CARTESIAN_POINT('Ctrl Pts',(-16.2127040285387,19.6623746550199,-13.4107485873244));
#40562=CARTESIAN_POINT('Ctrl Pts',(-16.2006099990479,19.5791509243174,-13.4149183016448));
#40563=CARTESIAN_POINT('Ctrl Pts',(-16.1885163999145,19.4959301550723,-13.4190878675888));
#40564=CARTESIAN_POINT('Ctrl Pts',(-16.1805275290999,19.4121113639662,-13.4232574335329));
#40565=CARTESIAN_POINT('Ctrl Pts',(-16.1766810426043,19.3281313371591,-13.4274269994769));
#40566=CARTESIAN_POINT('Ctrl Pts',(-16.1726993183887,19.24119867621,-13.4317431622158));
#40567=CARTESIAN_POINT('Ctrl Pts',(-16.1731567148618,19.154093757381,-13.4360593249547));
#40568=CARTESIAN_POINT('Ctrl Pts',(-16.1780362227548,19.0673018113875,-13.4403754876937));
#40569=CARTESIAN_POINT('Ctrl Pts',(-16.1827567811915,18.9833371039057,-13.4445510518853));
#40570=CARTESIAN_POINT('Ctrl Pts',(-16.1916156782438,18.8996657556595,-13.448726616077));
#40571=CARTESIAN_POINT('Ctrl Pts',(-16.2045447628248,18.8167206534358,-13.4529021802687));
#40572=CARTESIAN_POINT('Ctrl Pts',(-16.2181268647321,18.729586191282,-13.4572886422812));
#40573=CARTESIAN_POINT('Ctrl Pts',(-16.236201010622,18.643253840094,-13.4616751042938));
#40574=CARTESIAN_POINT('Ctrl Pts',(-16.2586283495454,18.5582096874756,-13.4660615663063));
#40575=CARTESIAN_POINT('Ctrl Pts',(-16.2810556884688,18.4731655348573,-13.4704480283188));
#40576=CARTESIAN_POINT('Ctrl Pts',(-16.3078359712666,18.3894101102965,-13.4748344903314));
#40577=CARTESIAN_POINT('Ctrl Pts',(-16.3387721302027,18.3074052613332,-13.4792209523439));
#40578=CARTESIAN_POINT('Ctrl Pts',(-16.3682848706079,18.229173577031,-13.4834055867369));
#40579=CARTESIAN_POINT('Ctrl Pts',(-16.4016893071736,18.1522437219302,-13.48759022113));
#40580=CARTESIAN_POINT('Ctrl Pts',(-16.4388502681124,18.0770301114156,-13.491774855523));
#40581=CARTESIAN_POINT('Ctrl Pts',(-16.4759583350228,18.0019235581661,-13.495953533607));
#40582=CARTESIAN_POINT('Ctrl Pts',(-16.5168121035541,17.9285288061221,-13.5001322116909));
#40583=CARTESIAN_POINT('Ctrl Pts',(-16.5612276601908,17.8572421341466,-13.5043108897749));
#40584=CARTESIAN_POINT('Ctrl Pts',(-16.6064393337593,17.7846776998087,-13.5085644676603));
#40585=CARTESIAN_POINT('Ctrl Pts',(-16.6553415713116,17.7142981146653,-13.5128180455457));
#40586=CARTESIAN_POINT('Ctrl Pts',(-16.7076904562346,17.6464970013307,-13.5170716234312));
#40587=CARTESIAN_POINT('Ctrl Pts',(-16.7590244558731,17.580010344881,-13.5212427374091));
#40588=CARTESIAN_POINT('Ctrl Pts',(-16.8136723614031,17.5160034559041,-13.5254138513871));
#40589=CARTESIAN_POINT('Ctrl Pts',(-16.8713604260513,17.4548183984679,-13.529584965365));
#40590=CARTESIAN_POINT('Ctrl Pts',(-16.9290291329122,17.3936538722685,-13.5337546796854));
#40591=CARTESIAN_POINT('Ctrl Pts',(-16.9897356575239,17.3353096315042,-13.5379243940058));
#40592=CARTESIAN_POINT('Ctrl Pts',(-17.0531673758219,17.2800930396577,-13.5420941083262));
#40593=CARTESIAN_POINT('Ctrl Pts',(-17.116596836947,17.2248784126545,-13.5462636742702));
#40594=CARTESIAN_POINT('Ctrl Pts',(-17.1827509514049,17.172791514689,-13.5504332402142));
#40595=CARTESIAN_POINT('Ctrl Pts',(-17.2512828336366,17.1241004325624,-13.5546028061583));
#40596=CARTESIAN_POINT('Ctrl Pts',(-17.3222242123044,17.0736974320551,-13.5589189688972));
#40597=CARTESIAN_POINT('Ctrl Pts',(-17.395713244423,17.0269337896177,-13.5632351316361));
#40598=CARTESIAN_POINT('Ctrl Pts',(-17.4713327209557,16.98405784933,-13.567551294375));
#40599=CARTESIAN_POINT('Ctrl Pts',(-17.5444889009941,16.9425785882874,-13.5717268585667));
#40600=CARTESIAN_POINT('Ctrl Pts',(-17.6196384165434,16.9047378049044,-13.5759024227584));
#40601=CARTESIAN_POINT('Ctrl Pts',(-17.6963803894308,16.8707125083097,-13.5800779869501));
#40602=CARTESIAN_POINT('Ctrl Pts',(-17.7769984169321,16.8349686748714,-13.5844644489626));
#40603=CARTESIAN_POINT('Ctrl Pts',(-17.8593734542574,16.8034361069936,-13.5888509109752));
#40604=CARTESIAN_POINT('Ctrl Pts',(-17.9430216212717,16.7762611630024,-13.5932373729877));
#40605=CARTESIAN_POINT('Ctrl Pts',(-18.026669788286,16.7490862190113,-13.5976238350002));
#40606=CARTESIAN_POINT('Ctrl Pts',(-18.1115905049086,16.726268976005,-13.6020102970128));
#40607=CARTESIAN_POINT('Ctrl Pts',(-18.1972887614196,16.7078937205182,-13.6063967590253));
#40608=CARTESIAN_POINT('Ctrl Pts',(-18.2790439141132,16.6903639377749,-13.6105813934184));
#40609=CARTESIAN_POINT('Ctrl Pts',(-18.3618109357872,16.6768111110841,-13.6147660278114));
#40610=CARTESIAN_POINT('Ctrl Pts',(-18.4451682027608,16.6673458975514,-13.6189506622045));
#40611=CARTESIAN_POINT('Ctrl Pts',(-18.5284068209825,16.6578941565786,-13.6231293402884));
#40612=CARTESIAN_POINT('Ctrl Pts',(-18.6122335625331,16.6525185234246,-13.6273080183724));
#40613=CARTESIAN_POINT('Ctrl Pts',(-18.696215670704,16.6512788541602,-13.6314866964563));
#40614=CARTESIAN_POINT('Ctrl Pts',(-18.7817030978069,16.6500169647151,-13.6357402743417));
#40615=CARTESIAN_POINT('Ctrl Pts',(-18.8673510447845,16.6530408729659,-13.6399938522272));
#40616=CARTESIAN_POINT('Ctrl Pts',(-18.9526965098738,16.6603585440974,-13.6442474301126));
#40617=CARTESIAN_POINT('Ctrl Pts',(-19.0363873865844,16.6675343478947,-13.6484185440906));
#40618=CARTESIAN_POINT('Ctrl Pts',(-19.1197869256881,16.6788388732104,-13.6525896580685));
#40619=CARTESIAN_POINT('Ctrl Pts',(-19.2024593315,16.6942270951215,-13.6567607720465));
#40620=CARTESIAN_POINT('Ctrl Pts',(-19.2851039957877,16.7096101533661,-13.6609304863668));
#40621=CARTESIAN_POINT('Ctrl Pts',(-19.3670215594762,16.7290741026091,-13.6651002006872));
#40622=CARTESIAN_POINT('Ctrl Pts',(-19.4477843610411,16.7525224455096,-13.6692699150076));
#40623=CARTESIAN_POINT('Ctrl Pts',(-19.5285442887189,16.7759699540174,-13.6734394809516));
#40624=CARTESIAN_POINT('Ctrl Pts',(-19.6081490944216,16.8034014451984,-13.6776090468957));
#40625=CARTESIAN_POINT('Ctrl Pts',(-19.6861855970015,16.8346703534941,-13.6817786128397));
#40626=CARTESIAN_POINT('Ctrl Pts',(-19.7669657667436,16.8670386380311,-13.6860947755787));
#40627=CARTESIAN_POINT('Ctrl Pts',(-19.8460648087827,16.9035190114426,-13.6904109383176));
#40628=CARTESIAN_POINT('Ctrl Pts',(-19.9230480777103,16.9438950908938,-13.6947271010565));
#40629=CARTESIAN_POINT('Ctrl Pts',(-19.9975236247499,16.9829559238037,-13.6989026652482));
#40630=CARTESIAN_POINT('Ctrl Pts',(-20.0700187425847,17.025662275374,-13.7030782294399));
#40631=CARTESIAN_POINT('Ctrl Pts',(-20.1401676067983,17.0717728821859,-13.7072537936315));
#40632=CARTESIAN_POINT('Ctrl Pts',(-20.2138595233803,17.1202124261303,-13.7116402556441));
#40633=CARTESIAN_POINT('Ctrl Pts',(-20.2849614681664,17.1724088154589,-13.7160267176566));
#40634=CARTESIAN_POINT('Ctrl Pts',(-20.3530884618268,17.2280344045396,-13.7204131796692));
#40635=CARTESIAN_POINT('Ctrl Pts',(-20.4212154554871,17.2836599936204,-13.7247996416817));
#40636=CARTESIAN_POINT('Ctrl Pts',(-20.4863671192074,17.3427143364292,-13.7291861036943));
#40637=CARTESIAN_POINT('Ctrl Pts',(-20.548204641978,17.4048268308311,-13.7335725657068));
#40638=CARTESIAN_POINT('Ctrl Pts',(-20.6067777194386,17.4636603639817,-13.7377274633762));
#40639=CARTESIAN_POINT('Ctrl Pts',(-20.6626103382647,17.5254713783546,-13.7418823610455));
#40640=CARTESIAN_POINT('Ctrl Pts',(-20.7153787245625,17.5899699725634,-13.7460372587149));
#40641=CARTESIAN_POINT('Ctrl Pts',(-20.7677053791601,17.6539286398258,-13.7501573751423));
#40642=CARTESIAN_POINT('Ctrl Pts',(-20.8170185699061,17.7205297194409,-13.7542774915697));
#40643=CARTESIAN_POINT('Ctrl Pts',(-20.8630375889925,17.7894519196816,-13.7583976079971));
#40644=CARTESIAN_POINT('Ctrl Pts',(-20.9090125260321,17.8583080987051,-13.7625137777266));
#40645=CARTESIAN_POINT('Ctrl Pts',(-20.951699290088,17.9294805955782,-13.7666299474561));
#40646=CARTESIAN_POINT('Ctrl Pts',(-20.9908578231797,18.0026156381546,-13.7707461171856));
#40647=CARTESIAN_POINT('Ctrl Pts',(-21.0299913601116,18.0757039962649,-13.7748596594307));
#40648=CARTESIAN_POINT('Ctrl Pts',(-21.0656009133711,18.1507519968574,-13.7789732016758));
#40649=CARTESIAN_POINT('Ctrl Pts',(-21.0974909394082,18.2273788435911,-13.7830867439209));
#40650=CARTESIAN_POINT('Ctrl Pts',(-21.1299241917558,18.3053109799219,-13.7872703577417));
#40651=CARTESIAN_POINT('Ctrl Pts',(-21.1585097661409,18.3848758167557,-13.7914539715626));
#40652=CARTESIAN_POINT('Ctrl Pts',(-21.1830923574767,18.4656499986255,-13.7956375853835));
#40653=CARTESIAN_POINT('Ctrl Pts',(-21.2072638620762,18.5450734199364,-13.7997512379815));
#40654=CARTESIAN_POINT('Ctrl Pts',(-21.2275651518659,18.6256655681997,-13.8038648905795));
#40655=CARTESIAN_POINT('Ctrl Pts',(-21.2438990336338,18.7070090864272,-13.8079785431775));
#40656=CARTESIAN_POINT('Ctrl Pts',(-21.260649602877,18.7904277283589,-13.8121971376098));
#40657=CARTESIAN_POINT('Ctrl Pts',(-21.2732274574716,18.8746360871023,-13.8164157320421));
#40658=CARTESIAN_POINT('Ctrl Pts',(-21.2815840465261,18.9591756050627,-13.8206343264745));
#40659=CARTESIAN_POINT('Ctrl Pts',(-21.2899406355806,19.043715123023,-13.8248529209068));
#40660=CARTESIAN_POINT('Ctrl Pts',(-21.2940759677847,19.1285852645553,-13.8290715153392));
#40661=CARTESIAN_POINT('Ctrl Pts',(-21.2939989424941,19.2133268925441,-13.8332901097715));
#40662=CARTESIAN_POINT('Ctrl Pts',(-21.2944497455462,19.2133273022983,-13.8332901097715));
#40663=CARTESIAN_POINT('Ctrl Pts',(-21.2961552640167,19.3972186594194,-13.8424428639771));
#40664=CARTESIAN_POINT('Ctrl Pts',(-21.1940977855363,20.4309438993384,-13.8939875537431));
#40665=CARTESIAN_POINT('Ctrl Pts',(-19.7898863418736,22.047969473252,-13.9879241790696));
#40666=CARTESIAN_POINT('Ctrl Pts',(-17.8646300978083,21.7705396626413,-14.0732424008125));
#40667=CARTESIAN_POINT('Ctrl Pts',(-17.1803677633157,21.2509974006736,-14.1161686869948));
#40668=CARTESIAN_POINT('Ctrl Pts',(-17.1718944362858,21.2444720185936,-14.1167030376167));
#40669=CARTESIAN_POINT('',(-21.2939989173812,19.2086456408557,-13.7667098774912));
#40670=CARTESIAN_POINT('Ctrl Pts',(-21.2935817003363,19.2086462806877,-13.7667098902285));
#40671=CARTESIAN_POINT('Ctrl Pts',(-21.2877698482561,19.8484613719781,-13.7985275695778));
#40672=CARTESIAN_POINT('Ctrl Pts',(-20.7208250258792,21.3499116215441,-13.8727371844875));
#40673=CARTESIAN_POINT('Ctrl Pts',(-18.6774627206427,22.0308987559626,-13.9672098138401));
#40674=CARTESIAN_POINT('Ctrl Pts',(-17.5010449849498,21.4873580244075,-14.0298647638434));
#40675=CARTESIAN_POINT('Ctrl Pts',(-17.1770151058749,21.2378231662188,-14.0501277782861));
#40676=CARTESIAN_POINT('Ctrl Pts',(-17.1744642439897,21.2411350264762,-13.2501880045741));
#40677=CARTESIAN_POINT('Ctrl Pts',(-17.1058906060324,21.1884572297191,-13.2544909919482));
#40678=CARTESIAN_POINT('Ctrl Pts',(-17.0399076063725,21.1322386433023,-13.2587939793222));
#40679=CARTESIAN_POINT('Ctrl Pts',(-16.9768963495314,21.0727697928342,-13.2630969666962));
#40680=CARTESIAN_POINT('Ctrl Pts',(-16.9158136728346,21.0151211003818,-13.267268252904));
#40681=CARTESIAN_POINT('Ctrl Pts',(-16.8575238163474,20.9544185704731,-13.2714395391118));
#40682=CARTESIAN_POINT('Ctrl Pts',(-16.8023406084374,20.8909678553436,-13.2756108253196));
#40683=CARTESIAN_POINT('Ctrl Pts',(-16.7471772900096,20.827540009524,-13.279780608086));
#40684=CARTESIAN_POINT('Ctrl Pts',(-16.6951186980832,20.7613662923708,-13.2839503908523));
#40685=CARTESIAN_POINT('Ctrl Pts',(-16.6464403664802,20.6927876961625,-13.2881201736186));
#40686=CARTESIAN_POINT('Ctrl Pts',(-16.5977649775094,20.6242132455685,-13.2922897043193));
#40687=CARTESIAN_POINT('Ctrl Pts',(-16.552469708406,20.5532345804094,-13.2964592350199));
#40688=CARTESIAN_POINT('Ctrl Pts',(-16.5107876884942,20.4802229977308,-13.3006287657206));
#40689=CARTESIAN_POINT('Ctrl Pts',(-16.469095684905,20.4071939273181,-13.3047992951072));
#40690=CARTESIAN_POINT('Ctrl Pts',(-16.4310188759036,20.3321313725595,-13.3089698244939));
#40691=CARTESIAN_POINT('Ctrl Pts',(-16.3967445544524,20.2554314157751,-13.3131403538805));
#40692=CARTESIAN_POINT('Ctrl Pts',(-16.3624311523989,20.1786440034151,-13.317315638629));
#40693=CARTESIAN_POINT('Ctrl Pts',(-16.3319290757362,20.1002158846929,-13.3214909233775));
#40694=CARTESIAN_POINT('Ctrl Pts',(-16.3053773193722,20.0205627678817,-13.325666208126));
#40695=CARTESIAN_POINT('Ctrl Pts',(-16.2788073074776,19.9408548859585,-13.3298443635711));
#40696=CARTESIAN_POINT('Ctrl Pts',(-16.2561931439568,19.8599207723268,-13.3340225190163));
#40697=CARTESIAN_POINT('Ctrl Pts',(-16.2376232149648,19.7781886345276,-13.3382006744614));
#40698=CARTESIAN_POINT('Ctrl Pts',(-16.2190239845482,19.6963275318802,-13.3423854226031));
#40699=CARTESIAN_POINT('Ctrl Pts',(-16.2044817977587,19.6136663447483,-13.3465701707449));
#40700=CARTESIAN_POINT('Ctrl Pts',(-16.1940334279964,19.5306401306222,-13.3507549188866));
#40701=CARTESIAN_POINT('Ctrl Pts',(-16.191782351114,19.5127523265437,-13.3516565131079));
#40702=CARTESIAN_POINT('Ctrl Pts',(-16.1897211074132,19.4948475818153,-13.3525581073293));
#40703=CARTESIAN_POINT('Ctrl Pts',(-16.1878497481282,19.4769302444118,-13.3534597015506));
#40704=CARTESIAN_POINT('Ctrl Pts',(-16.1791640730867,19.3937692119263,-13.3576443359437));
#40705=CARTESIAN_POINT('Ctrl Pts',(-16.1745407622114,19.3100274422731,-13.3618289703367));
#40706=CARTESIAN_POINT('Ctrl Pts',(-16.1740447460464,19.2261359755289,-13.3660136047298));
#40707=CARTESIAN_POINT('Ctrl Pts',(-16.173549435899,19.1423639179039,-13.3701922828137));
#40708=CARTESIAN_POINT('Ctrl Pts',(-16.1771697541693,19.0584430425126,-13.3743709608977));
#40709=CARTESIAN_POINT('Ctrl Pts',(-16.1849189310737,18.9748100255276,-13.3785496389816));
#40710=CARTESIAN_POINT('Ctrl Pts',(-16.1928070064048,18.8896779468192,-13.382803216867));
#40711=CARTESIAN_POINT('Ctrl Pts',(-16.2049734659499,18.804844627276,-13.3870567947525));
#40712=CARTESIAN_POINT('Ctrl Pts',(-16.2213767120001,18.7207712650195,-13.3913103726379));
#40713=CARTESIAN_POINT('Ctrl Pts',(-16.2374619491174,18.6383278289459,-13.3954814866159));
#40714=CARTESIAN_POINT('Ctrl Pts',(-16.2576210698179,18.5566156189164,-13.3996526005938));
#40715=CARTESIAN_POINT('Ctrl Pts',(-16.2817626998464,18.4760631158151,-13.4038237145718));
#40716=CARTESIAN_POINT('Ctrl Pts',(-16.3058962289179,18.3955376428842,-13.4079934288921));
#40717=CARTESIAN_POINT('Ctrl Pts',(-16.3340094813079,18.3161715443229,-13.4121631432125));
#40718=CARTESIAN_POINT('Ctrl Pts',(-16.3659607754927,18.2383797086247,-13.4163328575329));
#40719=CARTESIAN_POINT('Ctrl Pts',(-16.3979109327134,18.1605906410939,-13.4205024234769));
#40720=CARTESIAN_POINT('Ctrl Pts',(-16.4336986846161,18.0843761502596,-13.424671989421));
#40721=CARTESIAN_POINT('Ctrl Pts',(-16.4731341172713,18.0101313725834,-13.428841555365));
#40722=CARTESIAN_POINT('Ctrl Pts',(-16.5139560510898,17.933276240115,-13.433157718104));
#40723=CARTESIAN_POINT('Ctrl Pts',(-16.5586866956794,17.8585323739429,-13.4374738808429));
#40724=CARTESIAN_POINT('Ctrl Pts',(-16.6070644247003,17.7863087848504,-13.4417900435818));
#40725=CARTESIAN_POINT('Ctrl Pts',(-16.6538662542868,17.7164378715759,-13.4459656077735));
#40726=CARTESIAN_POINT('Ctrl Pts',(-16.7040808906405,17.6489259106341,-13.4501411719652));
#40727=CARTESIAN_POINT('Ctrl Pts',(-16.7574293298199,17.5841108255988,-13.4543167361568));
#40728=CARTESIAN_POINT('Ctrl Pts',(-16.8134722718384,17.5160220847016,-13.4587031981694));
#40729=CARTESIAN_POINT('Ctrl Pts',(-16.8729735193545,17.450910248947,-13.4630896601819));
#40730=CARTESIAN_POINT('Ctrl Pts',(-16.9355661330671,17.3891230485379,-13.4674761221945));
#40731=CARTESIAN_POINT('Ctrl Pts',(-16.9981587467797,17.3273358481289,-13.471862584207));
#40732=CARTESIAN_POINT('Ctrl Pts',(-17.0638422427094,17.2688736120054,-13.4762490462195));
#40733=CARTESIAN_POINT('Ctrl Pts',(-17.1322119090441,17.2140335727229,-13.4806355082321));
#40734=CARTESIAN_POINT('Ctrl Pts',(-17.1974357856826,17.1617168049403,-13.4848201426251));
#40735=CARTESIAN_POINT('Ctrl Pts',(-17.2653468510498,17.112501500524,-13.4890047770182));
#40736=CARTESIAN_POINT('Ctrl Pts',(-17.3356178143268,17.0666755696043,-13.4931894114112));
#40737=CARTESIAN_POINT('Ctrl Pts',(-17.4057887555853,17.0209148662252,-13.4973680894952));
#40738=CARTESIAN_POINT('Ctrl Pts',(-17.4783125406378,16.9785342027988,-13.5015467675791));
#40739=CARTESIAN_POINT('Ctrl Pts',(-17.5528291551938,16.9397810683732,-13.5057254456631));
#40740=CARTESIAN_POINT('Ctrl Pts',(-17.6286814265116,16.9003333118645,-13.5099790235485));
#40741=CARTESIAN_POINT('Ctrl Pts',(-17.7065982968802,16.8646447120803,-13.5142326014339));
#40742=CARTESIAN_POINT('Ctrl Pts',(-17.7861694556147,16.8329299297266,-13.5184861793194));
#40743=CARTESIAN_POINT('Ctrl Pts',(-17.8641979721668,16.8018300003151,-13.5226572932973));
#40744=CARTESIAN_POINT('Ctrl Pts',(-17.9438167592513,16.7745513610798,-13.5268284072753));
#40745=CARTESIAN_POINT('Ctrl Pts',(-18.0246160731017,16.7512491093084,-13.5309995212532));
#40746=CARTESIAN_POINT('Ctrl Pts',(-18.105388273962,16.7279546768326,-13.5351692355736));
#40747=CARTESIAN_POINT('Ctrl Pts',(-18.1873397732034,16.7086341092198,-13.539338949894));
#40748=CARTESIAN_POINT('Ctrl Pts',(-18.2700450257387,16.6933928460027,-13.5435086642143));
#40749=CARTESIAN_POINT('Ctrl Pts',(-18.3527473352662,16.6781521251352,-13.5476782301584));
#40750=CARTESIAN_POINT('Ctrl Pts',(-18.4362028921897,16.6669905025844,-13.5518477961024));
#40751=CARTESIAN_POINT('Ctrl Pts',(-18.5199766524687,16.6599621706624,-13.5560173620465));
#40752=CARTESIAN_POINT('Ctrl Pts',(-18.606695794813,16.6526867312604,-13.5603335247854));
#40753=CARTESIAN_POINT('Ctrl Pts',(-18.693755407323,16.6498406874529,-13.5646496875243));
#40754=CARTESIAN_POINT('Ctrl Pts',(-18.7806699632819,16.6514254426708,-13.5689658502632));
#40755=CARTESIAN_POINT('Ctrl Pts',(-18.8647532867223,16.6529585746541,-13.5731414144549));
#40756=CARTESIAN_POINT('Ctrl Pts',(-18.9487003921372,16.6586381931969,-13.5773169786466));
#40757=CARTESIAN_POINT('Ctrl Pts',(-19.032076119737,16.6684126117589,-13.5814925428383));
#40758=CARTESIAN_POINT('Ctrl Pts',(-19.1196629571308,16.6786807129661,-13.5858790048508));
#40759=CARTESIAN_POINT('Ctrl Pts',(-19.2066186035791,16.6934680441002,-13.5902654668633));
#40760=CARTESIAN_POINT('Ctrl Pts',(-19.2924520557265,16.7126542870422,-13.5946519288759));
#40761=CARTESIAN_POINT('Ctrl Pts',(-19.3782855078739,16.7318405299841,-13.5990383908884));
#40762=CARTESIAN_POINT('Ctrl Pts',(-19.462996227165,16.7554254558327,-13.603424852901));
#40763=CARTESIAN_POINT('Ctrl Pts',(-19.5461152252309,16.783229652346,-13.6078113149135));
#40764=CARTESIAN_POINT('Ctrl Pts',(-19.6254097949838,16.809754536562,-13.6119959493065));
#40765=CARTESIAN_POINT('Ctrl Pts',(-19.7035510491552,16.8402176845382,-13.6161805836996));
#40766=CARTESIAN_POINT('Ctrl Pts',(-19.7801197445754,16.8744997367838,-13.6203652180926));
#40767=CARTESIAN_POINT('Ctrl Pts',(-19.856579453935,16.9087329927713,-13.6245438961766));
#40768=CARTESIAN_POINT('Ctrl Pts',(-19.9314706343179,16.9467741695628,-13.6287225742605));
#40769=CARTESIAN_POINT('Ctrl Pts',(-20.0043903176931,16.9884545132413,-13.6329012523445));
#40770=CARTESIAN_POINT('Ctrl Pts',(-20.0786170339864,17.0308819471251,-13.6371548302299));
#40771=CARTESIAN_POINT('Ctrl Pts',(-20.1508004226817,17.0770801423177,-13.6414084081153));
#40772=CARTESIAN_POINT('Ctrl Pts',(-20.2205378947047,17.1268202842349,-13.6456619860008));
#40773=CARTESIAN_POINT('Ctrl Pts',(-20.288923369751,17.1755961164411,-13.6498330999787));
#40774=CARTESIAN_POINT('Ctrl Pts',(-20.3549565277687,17.2277775063951,-13.6540042139567));
#40775=CARTESIAN_POINT('Ctrl Pts',(-20.4182851699542,17.283103875653,-13.6581753279346));
#40776=CARTESIAN_POINT('Ctrl Pts',(-20.4815925616022,17.3384116796133,-13.662345042255));
#40777=CARTESIAN_POINT('Ctrl Pts',(-20.5421968936246,17.3968620645641,-13.6665147565753));
#40778=CARTESIAN_POINT('Ctrl Pts',(-20.5997791685761,17.4581542868503,-13.6706844708957));
#40779=CARTESIAN_POINT('Ctrl Pts',(-20.6573593945032,17.5194443280962,-13.6748540368398));
#40780=CARTESIAN_POINT('Ctrl Pts',(-20.7119174628062,17.5835756697508,-13.6790236027838));
#40781=CARTESIAN_POINT('Ctrl Pts',(-20.763172325239,17.6502118418939,-13.6831931687278));
#40782=CARTESIAN_POINT('Ctrl Pts',(-20.8162292454052,17.719190859645,-13.6875093314668));
#40783=CARTESIAN_POINT('Ctrl Pts',(-20.8657460348867,17.79085370675,-13.6918254942057));
#40784=CARTESIAN_POINT('Ctrl Pts',(-20.911458707217,17.864792891727,-13.6961416569446));
#40785=CARTESIAN_POINT('Ctrl Pts',(-20.9556822940543,17.9363235155303,-13.7003172211363));
#40786=CARTESIAN_POINT('Ctrl Pts',(-20.9963456096572,18.0099840160616,-13.704492785328));
#40787=CARTESIAN_POINT('Ctrl Pts',(-21.0332565704859,18.0853805158591,-13.7086683495196));
#40788=CARTESIAN_POINT('Ctrl Pts',(-21.0720318161985,18.1645851136233,-13.7130548115322));
#40789=CARTESIAN_POINT('Ctrl Pts',(-21.1066654530387,18.245705153136,-13.7174412735447));
#40790=CARTESIAN_POINT('Ctrl Pts',(-21.1369928787006,18.3282626523623,-13.7218277355573));
#40791=CARTESIAN_POINT('Ctrl Pts',(-21.1673203043624,18.4108201515887,-13.7262141975698));
#40792=CARTESIAN_POINT('Ctrl Pts',(-21.1933414198056,18.494814533789,-13.7306006595824));
#40793=CARTESIAN_POINT('Ctrl Pts',(-21.214953227824,18.5797543415201,-13.7349871215949));
#40794=CARTESIAN_POINT('Ctrl Pts',(-21.2416966549181,18.6848626949492,-13.740415127754));
#40795=CARTESIAN_POINT('Ctrl Pts',(-21.2617718479477,18.7917315462695,-13.7458431339131));
#40796=CARTESIAN_POINT('Ctrl Pts',(-21.2749934581325,18.8996284442541,-13.7512711400722));
#40797=CARTESIAN_POINT('Ctrl Pts',(-21.2875287526721,19.0019245622934,-13.7564173858785));
#40798=CARTESIAN_POINT('Ctrl Pts',(-21.2939037306914,19.1051449394058,-13.7615636316849));
#40799=CARTESIAN_POINT('Ctrl Pts',(-21.2939989173812,19.2086456408557,-13.7667098774912));
#40800=CARTESIAN_POINT('Origin',(-18.734,19.211,1.76670989022852));
#40801=CARTESIAN_POINT('',(-17.1725834302249,21.2436206685575,-12.4500366781978));
#40802=CARTESIAN_POINT('',(-17.1744642439897,21.2411350264762,-12.5167193432124));
#40803=CARTESIAN_POINT('',(-17.1744642439897,21.2411350264762,1.76670989022852));
#40804=CARTESIAN_POINT('',(-21.293999998394,19.2109093211998,-13.0332901097364));
#40805=CARTESIAN_POINT('Ctrl Pts',(-17.1744642439897,21.2411350264762,-12.5167193432124));
#40806=CARTESIAN_POINT('Ctrl Pts',(-17.1077874800253,21.1899143952662,-12.5208888590638));
#40807=CARTESIAN_POINT('Ctrl Pts',(-17.0436201898523,21.1353927403986,-12.5250583749152));
#40808=CARTESIAN_POINT('Ctrl Pts',(-16.9822976161262,21.077852634337,-12.5292278907666));
#40809=CARTESIAN_POINT('Ctrl Pts',(-16.9209705475262,21.0203083106519,-12.5333977122387));
#40810=CARTESIAN_POINT('Ctrl Pts',(-16.8624889439855,20.9597454121972,-12.5375675337108));
#40811=CARTESIAN_POINT('Ctrl Pts',(-16.8071520646769,20.8964842135544,-12.5417373551829));
#40812=CARTESIAN_POINT('Ctrl Pts',(-16.7517573571547,20.833156905616,-12.545911534207));
#40813=CARTESIAN_POINT('Ctrl Pts',(-16.6995142397073,20.7671260137235,-12.550085713231));
#40814=CARTESIAN_POINT('Ctrl Pts',(-16.6506820992389,20.6987454501252,-12.5542598922551));
#40815=CARTESIAN_POINT('Ctrl Pts',(-16.6018236631547,20.6303280642822,-12.5584363190325));
#40816=CARTESIAN_POINT('Ctrl Pts',(-16.5563801103552,20.559558874473,-12.5626127458099));
#40817=CARTESIAN_POINT('Ctrl Pts',(-16.5145664970211,20.4868193155203,-12.5667891725874));
#40818=CARTESIAN_POINT('Ctrl Pts',(-16.4726800356492,20.4139530290807,-12.5709728755716));
#40819=CARTESIAN_POINT('Ctrl Pts',(-16.4344363552231,20.3391099268244,-12.5751565785557));
#40820=CARTESIAN_POINT('Ctrl Pts',(-16.400003615296,20.2626942883692,-12.5793402815399));
#40821=CARTESIAN_POINT('Ctrl Pts',(-16.3735297181201,20.2039414920662,-12.5825569562179));
#40822=CARTESIAN_POINT('Ctrl Pts',(-16.3493076693354,20.1442595816972,-12.5857736308959));
#40823=CARTESIAN_POINT('Ctrl Pts',(-16.3273937923111,20.0838382216157,-12.5889903055739));
#40824=CARTESIAN_POINT('Ctrl Pts',(-16.2988856052357,20.0052349039716,-12.5931749399669));
#40825=CARTESIAN_POINT('Ctrl Pts',(-16.274179366091,19.9250871608004,-12.59735957436));
#40826=CARTESIAN_POINT('Ctrl Pts',(-16.2534421603042,19.8437976010729,-12.601544208753));
#40827=CARTESIAN_POINT('Ctrl Pts',(-16.2327344713631,19.7626237469723,-12.605722886837));
#40828=CARTESIAN_POINT('Ctrl Pts',(-16.2159847069801,19.680311746487,-12.6099015649209));
#40829=CARTESIAN_POINT('Ctrl Pts',(-16.2033111427938,19.5972821611364,-12.6140802430048));
#40830=CARTESIAN_POINT('Ctrl Pts',(-16.1904104140777,19.5127643301405,-12.6183338208903));
#40831=CARTESIAN_POINT('Ctrl Pts',(-16.1817336190672,19.4275033890776,-12.6225873987757));
#40832=CARTESIAN_POINT('Ctrl Pts',(-16.177351748603,19.3419569342513,-12.6268409766612));
#40833=CARTESIAN_POINT('Ctrl Pts',(-16.1730548292483,19.2580689643821,-12.6310120906391));
#40834=CARTESIAN_POINT('Ctrl Pts',(-16.1728878141637,19.1739069330302,-12.6351832046171));
#40835=CARTESIAN_POINT('Ctrl Pts',(-16.1768654907269,19.0899087059925,-12.639354318595));
#40836=CARTESIAN_POINT('Ctrl Pts',(-16.1808418325422,19.0059386653711,-12.6435240329154));
#40837=CARTESIAN_POINT('Ctrl Pts',(-16.1889600821296,18.922132779036,-12.6476937472358));
#40838=CARTESIAN_POINT('Ctrl Pts',(-16.2011829261396,18.8389278694111,-12.6518634615561));
#40839=CARTESIAN_POINT('Ctrl Pts',(-16.2134053352083,18.7557259205741,-12.6560330275002));
#40840=CARTESIAN_POINT('Ctrl Pts',(-16.229731980592,18.673125360952,-12.6602025934442));
#40841=CARTESIAN_POINT('Ctrl Pts',(-16.250073974422,18.5915554912213,-12.6643721593882));
#40842=CARTESIAN_POINT('Ctrl Pts',(-16.2711311676605,18.5071177254979,-12.6686883221272));
#40843=CARTESIAN_POINT('Ctrl Pts',(-16.2964911945896,18.4237849880538,-12.6730044848661));
#40844=CARTESIAN_POINT('Ctrl Pts',(-16.325998926724,18.3420173585728,-12.677320647605));
#40845=CARTESIAN_POINT('Ctrl Pts',(-16.3545454475878,18.2629133010219,-12.6814962117967));
#40846=CARTESIAN_POINT('Ctrl Pts',(-16.3869733753121,18.1852743669885,-12.6856717759884));
#40847=CARTESIAN_POINT('Ctrl Pts',(-16.4230935537342,18.1094958481209,-12.6898473401801));
#40848=CARTESIAN_POINT('Ctrl Pts',(-16.4610380765009,18.0298899364114,-12.6942338021926));
#40849=CARTESIAN_POINT('Ctrl Pts',(-16.5030573653642,17.9523378315092,-12.6986202642051));
#40850=CARTESIAN_POINT('Ctrl Pts',(-16.5488792984353,17.8772655738142,-12.7030067262177));
#40851=CARTESIAN_POINT('Ctrl Pts',(-16.5947012315064,17.8021933161192,-12.7073931882302));
#40852=CARTESIAN_POINT('Ctrl Pts',(-16.6443254185491,17.7296013416972,-12.7117796502428));
#40853=CARTESIAN_POINT('Ctrl Pts',(-16.6974308899397,17.6598758076968,-12.7161661122553));
#40854=CARTESIAN_POINT('Ctrl Pts',(-16.7480928998703,17.593358448874,-12.7203507466484));
#40855=CARTESIAN_POINT('Ctrl Pts',(-16.8021114495637,17.5292019583441,-12.7245353810414));
#40856=CARTESIAN_POINT('Ctrl Pts',(-16.8592384487626,17.4677647531094,-12.7287200154345));
#40857=CARTESIAN_POINT('Ctrl Pts',(-16.9162841347489,17.4064149961321,-12.7328986935184));
#40858=CARTESIAN_POINT('Ctrl Pts',(-16.9764291712243,17.3477771703016,-12.7370773716023));
#40859=CARTESIAN_POINT('Ctrl Pts',(-17.0393839528664,17.2921783686863,-12.7412560496863));
#40860=CARTESIAN_POINT('Ctrl Pts',(-17.1034671537248,17.2355829985101,-12.7455096275717));
#40861=CARTESIAN_POINT('Ctrl Pts',(-17.1704615277515,17.1821370567432,-12.7497632054571));
#40862=CARTESIAN_POINT('Ctrl Pts',(-17.2400207348668,17.1321479236482,-12.7540167833426));
#40863=CARTESIAN_POINT('Ctrl Pts',(-17.3082314010186,17.0831279274441,-12.7581878973205));
#40864=CARTESIAN_POINT('Ctrl Pts',(-17.3789079483578,17.0374321828771,-12.7623590112985));
#40865=CARTESIAN_POINT('Ctrl Pts',(-17.4516902051699,16.9953101322426,-12.7665301252764));
#40866=CARTESIAN_POINT('Ctrl Pts',(-17.5244480391927,16.9532022160691,-12.7706998395968));
#40867=CARTESIAN_POINT('Ctrl Pts',(-17.5993097815583,16.9146658424624,-12.7748695539171));
#40868=CARTESIAN_POINT('Ctrl Pts',(-17.6758879367283,16.8799060804938,-12.7790392682375));
#40869=CARTESIAN_POINT('Ctrl Pts',(-17.7524633669187,16.8451475554268,-12.7832088341815));
#40870=CARTESIAN_POINT('Ctrl Pts',(-17.8307546692255,16.814165564167,-12.7873784001256));
#40871=CARTESIAN_POINT('Ctrl Pts',(-17.9103527564008,16.7871177383975,-12.7915479660696));
#40872=CARTESIAN_POINT('Ctrl Pts',(-17.9927494141267,16.7591189444408,-12.7958641288085));
#40873=CARTESIAN_POINT('Ctrl Pts',(-18.0765459602113,16.7353362835288,-12.8001802915474));
#40874=CARTESIAN_POINT('Ctrl Pts',(-18.1612715723428,16.7158883495616,-12.8044964542864));
#40875=CARTESIAN_POINT('Ctrl Pts',(-18.2432372565706,16.6970739299979,-12.808672018478));
#40876=CARTESIAN_POINT('Ctrl Pts',(-18.3260719356978,16.6823162029297,-12.8128475826697));
#40877=CARTESIAN_POINT('Ctrl Pts',(-18.4093408453614,16.6716700818308,-12.8170231468614));
#40878=CARTESIAN_POINT('Ctrl Pts',(-18.4968154696991,16.6604862504638,-12.8214096088739));
#40879=CARTESIAN_POINT('Ctrl Pts',(-18.584768761138,16.6538403392096,-12.8257960708865));
#40880=CARTESIAN_POINT('Ctrl Pts',(-18.6726951927067,16.6517341442119,-12.830182532899));
#40881=CARTESIAN_POINT('Ctrl Pts',(-18.7606216242755,16.6496279492142,-12.8345689949116));
#40882=CARTESIAN_POINT('Ctrl Pts',(-18.8485206180843,16.6520613783803,-12.8389554569241));
#40883=CARTESIAN_POINT('Ctrl Pts',(-18.9358937423124,16.6589735665916,-12.8433419189367));
#40884=CARTESIAN_POINT('Ctrl Pts',(-19.0192466995765,16.665567714777,-12.8475265533297));
#40885=CARTESIAN_POINT('Ctrl Pts',(-19.1024313715336,16.6762620749485,-12.8517111877228));
#40886=CARTESIAN_POINT('Ctrl Pts',(-19.1850120996546,16.6910420467863,-12.8558958221158));
#40887=CARTESIAN_POINT('Ctrl Pts',(-19.2674752843308,16.7058009811636,-12.8600745001998));
#40888=CARTESIAN_POINT('Ctrl Pts',(-19.3493357837208,16.7246338957134,-12.8642531782837));
#40889=CARTESIAN_POINT('Ctrl Pts',(-19.4301618064496,16.7474743274646,-12.8684318563677));
#40890=CARTESIAN_POINT('Ctrl Pts',(-19.5124365775469,16.7707241575398,-12.8726854342531));
#40891=CARTESIAN_POINT('Ctrl Pts',(-19.5936389405811,16.7981265494107,-12.8769390121385));
#40892=CARTESIAN_POINT('Ctrl Pts',(-19.673322970079,16.8295566649861,-12.881192590024));
#40893=CARTESIAN_POINT('Ctrl Pts',(-19.7514621691743,16.8603774464402,-12.8853637040019));
#40894=CARTESIAN_POINT('Ctrl Pts',(-19.8281409334347,16.8950709981006,-12.8895348179799));
#40895=CARTESIAN_POINT('Ctrl Pts',(-19.9029545672469,16.933469490937,-12.8937059319578));
#40896=CARTESIAN_POINT('Ctrl Pts',(-19.9777430966217,16.9718550987884,-12.8978756462782));
#40897=CARTESIAN_POINT('Ctrl Pts',(-20.0506673295888,17.013942968857,-12.9020453605985));
#40898=CARTESIAN_POINT('Ctrl Pts',(-20.1213450915267,17.0595182787166,-12.9062150749189));
#40899=CARTESIAN_POINT('Ctrl Pts',(-20.1920203384466,17.1050919668111,-12.9103846408629));
#40900=CARTESIAN_POINT('Ctrl Pts',(-20.2604488871165,17.154152597935,-12.914554206807));
#40901=CARTESIAN_POINT('Ctrl Pts',(-20.3262767630686,17.2064415174927,-12.918723772751));
#40902=CARTESIAN_POINT('Ctrl Pts',(-20.3944190659318,17.2605688509569,-12.9230399354899));
#40903=CARTESIAN_POINT('Ctrl Pts',(-20.4597740011395,17.3181553818452,-12.9273560982289));
#40904=CARTESIAN_POINT('Ctrl Pts',(-20.5219870028021,17.3788694157318,-12.9316722609678));
#40905=CARTESIAN_POINT('Ctrl Pts',(-20.5821734224789,17.4376056963504,-12.9358478251595));
#40906=CARTESIAN_POINT('Ctrl Pts',(-20.6394191762099,17.4992684748645,-12.9400233893511));
#40907=CARTESIAN_POINT('Ctrl Pts',(-20.69344276075,17.5635219068696,-12.9441989535428));
#40908=CARTESIAN_POINT('Ctrl Pts',(-20.7501949481165,17.6310206269775,-12.9485854155554));
#40909=CARTESIAN_POINT('Ctrl Pts',(-20.8033905562328,17.7013781204553,-12.9529718775679));
#40910=CARTESIAN_POINT('Ctrl Pts',(-20.8527544426649,17.7741702913401,-12.9573583395805));
#40911=CARTESIAN_POINT('Ctrl Pts',(-20.902118329097,17.8469624622249,-12.961744801593));
#40912=CARTESIAN_POINT('Ctrl Pts',(-20.9476502584793,17.9221887747549,-12.9661312636056));
#40913=CARTESIAN_POINT('Ctrl Pts',(-20.9891316170534,17.9993971815128,-12.9705177256181));
#40914=CARTESIAN_POINT('Ctrl Pts',(-21.030861876244,18.0770688619123,-12.9749305077209));
#40915=CARTESIAN_POINT('Ctrl Pts',(-21.0686351706118,18.1570094498411,-12.9793432898236));
#40916=CARTESIAN_POINT('Ctrl Pts',(-21.1022126120114,18.2388019624017,-12.9837560719264));
#40917=CARTESIAN_POINT('Ctrl Pts',(-21.1356929152443,18.3203578525637,-12.9881560880307));
#40918=CARTESIAN_POINT('Ctrl Pts',(-21.1650014030465,18.4037546379829,-12.992556104135));
#40919=CARTESIAN_POINT('Ctrl Pts',(-21.1899457627446,18.4885524860192,-12.9969561202393));
#40920=CARTESIAN_POINT('Ctrl Pts',(-21.2148467487812,18.5732028861678,-13.0013484855235));
#40921=CARTESIAN_POINT('Ctrl Pts',(-21.2353985968836,18.6592491335648,-13.0057408508078));
#40922=CARTESIAN_POINT('Ctrl Pts',(-21.2514572537725,18.7462323425323,-13.010133216092));
#40923=CARTESIAN_POINT('Ctrl Pts',(-21.267478998332,18.8330156124333,-13.0145154851125));
#40924=CARTESIAN_POINT('Ctrl Pts',(-21.2790280568695,18.9207311752703,-13.018897754133));
#40925=CARTESIAN_POINT('Ctrl Pts',(-21.28601069243,19.0089073833049,-13.0232800231535));
#40926=CARTESIAN_POINT('Ctrl Pts',(-21.291327328341,19.0760454703582,-13.0266167186811));
#40927=CARTESIAN_POINT('Ctrl Pts',(-21.2939976088987,19.1434502453364,-13.0299534142087));
#40928=CARTESIAN_POINT('Ctrl Pts',(-21.293999998394,19.2109093211998,-13.0332901097364));
#40929=CARTESIAN_POINT('Ctrl Pts',(-21.293999998394,19.2109093219103,-13.0332901097715));
#40930=CARTESIAN_POINT('Ctrl Pts',(-21.2940031178915,19.2989781543512,-13.0376462156856));
#40931=CARTESIAN_POINT('Ctrl Pts',(-21.2894573285641,19.3869643923453,-13.0420023215996));
#40932=CARTESIAN_POINT('Ctrl Pts',(-21.2804139262415,19.4743934627951,-13.0463584275137));
#40933=CARTESIAN_POINT('Ctrl Pts',(-21.2713470661107,19.5620493167382,-13.0507258327921));
#40934=CARTESIAN_POINT('Ctrl Pts',(-21.2577593163574,19.6491447181139,-13.0550932380704));
#40935=CARTESIAN_POINT('Ctrl Pts',(-21.2397536148681,19.7352125728896,-13.0594606433488));
#40936=CARTESIAN_POINT('Ctrl Pts',(-21.2217244341811,19.8213926590148,-13.0638337436661));
#40937=CARTESIAN_POINT('Ctrl Pts',(-21.1992659159006,19.9065421429604,-13.0682068439834));
#40938=CARTESIAN_POINT('Ctrl Pts',(-21.1725309633218,19.9902090482796,-13.0725799443008));
#40939=CARTESIAN_POINT('Ctrl Pts',(-21.1457232584227,20.0741036316349,-13.0769649448896));
#40940=CARTESIAN_POINT('Ctrl Pts',(-21.1146159900528,20.1565071961892,-13.0813499454785));
#40941=CARTESIAN_POINT('Ctrl Pts',(-21.0794107185111,20.2369866283209,-13.0857349460674));
#40942=CARTESIAN_POINT('Ctrl Pts',(-21.0474072811092,20.3101466511123,-13.0897211414781));
#40943=CARTESIAN_POINT('Ctrl Pts',(-21.0120180507083,20.3817167133685,-13.0937073368888));
#40944=CARTESIAN_POINT('Ctrl Pts',(-20.9734262024017,20.4513911818442,-13.0976935322996));
#40945=CARTESIAN_POINT('Ctrl Pts',(-20.9329131921061,20.524534153289,-13.1018781666926));
#40946=CARTESIAN_POINT('Ctrl Pts',(-20.8887375841055,20.5958263313022,-13.1060628010856));
#40947=CARTESIAN_POINT('Ctrl Pts',(-20.8410930441,20.6648771968448,-13.1102474354787));
#40948=CARTESIAN_POINT('Ctrl Pts',(-20.7935163201999,20.7338297770273,-13.1144261135626));
#40949=CARTESIAN_POINT('Ctrl Pts',(-20.7424807309407,20.8005470061349,-13.1186047916466));
#40950=CARTESIAN_POINT('Ctrl Pts',(-20.6882255495784,20.8646633579344,-13.1227834697305));
#40951=CARTESIAN_POINT('Ctrl Pts',(-20.6329978830828,20.9299289492601,-13.127037047616));
#40952=CARTESIAN_POINT('Ctrl Pts',(-20.574434300428,20.992499082944,-13.1312906255014));
#40953=CARTESIAN_POINT('Ctrl Pts',(-20.51283306354,21.0520195360334,-13.1355442033868));
#40954=CARTESIAN_POINT('Ctrl Pts',(-20.4524260868341,21.1103860689951,-13.1397153173648));
#40955=CARTESIAN_POINT('Ctrl Pts',(-20.3890985326089,21.1658197797782,-13.1438864313427));
#40956=CARTESIAN_POINT('Ctrl Pts',(-20.3231707254821,21.2180217749867,-13.1480575453207));
#40957=CARTESIAN_POINT('Ctrl Pts',(-20.2572650410675,21.2702062533116,-13.1522272596411));
#40958=CARTESIAN_POINT('Ctrl Pts',(-20.1887611969919,21.319160884427,-13.1563969739614));
#40959=CARTESIAN_POINT('Ctrl Pts',(-20.1180129698813,21.3646267316321,-13.1605666882818));
#40960=CARTESIAN_POINT('Ctrl Pts',(-20.0472672602961,21.4100909609673,-13.1647362542259));
#40961=CARTESIAN_POINT('Ctrl Pts',(-19.9742777139359,21.4520664052354,-13.1689058201699));
#40962=CARTESIAN_POINT('Ctrl Pts',(-19.8994263305446,21.4903379451221,-13.1730753861139));
#40963=CARTESIAN_POINT('Ctrl Pts',(-19.8219432648524,21.5299550651381,-13.1773915488529));
#40964=CARTESIAN_POINT('Ctrl Pts',(-19.7424654713774,21.5656027360313,-13.1817077115918));
#40965=CARTESIAN_POINT('Ctrl Pts',(-19.6614416802126,21.5970955407955,-13.1860238743307));
#40966=CARTESIAN_POINT('Ctrl Pts',(-19.5830572305228,21.627562470757,-13.1901994385224));
#40967=CARTESIAN_POINT('Ctrl Pts',(-19.5032264199663,21.6541409631941,-13.1943750027141));
#40968=CARTESIAN_POINT('Ctrl Pts',(-19.4223715061057,21.6767138255649,-13.1985505669058));
#40969=CARTESIAN_POINT('Ctrl Pts',(-19.3374328027603,21.7004267895521,-13.2029370289183));
#40970=CARTESIAN_POINT('Ctrl Pts',(-19.2513643920955,21.7197187126534,-13.2073234909308));
#40971=CARTESIAN_POINT('Ctrl Pts',(-19.1646662302709,21.7345147311051,-13.2117099529434));
#40972=CARTESIAN_POINT('Ctrl Pts',(-19.0779680684463,21.7493107495567,-13.2160964149559));
#40973=CARTESIAN_POINT('Ctrl Pts',(-18.9906407405947,21.7596108709354,-13.2204828769685));
#40974=CARTESIAN_POINT('Ctrl Pts',(-18.9031862415114,21.7654032601927,-13.224869338981));
#40975=CARTESIAN_POINT('Ctrl Pts',(-18.8197759389833,21.7709277894665,-13.229052955917));
#40976=CARTESIAN_POINT('Ctrl Pts',(-18.7359395737635,21.7723728408953,-13.233236572853));
#40977=CARTESIAN_POINT('Ctrl Pts',(-18.6521100212236,21.7696899052789,-13.237420189789));
#40978=CARTESIAN_POINT('Ctrl Pts',(-18.5683906915354,21.7670104973064,-13.241598305918));
#40979=CARTESIAN_POINT('Ctrl Pts',(-18.4846786121261,21.7602138920958,-13.245776422047));
#40980=CARTESIAN_POINT('Ctrl Pts',(-18.4014104699563,21.7493034106476,-13.249954538176));
#40981=CARTESIAN_POINT('Ctrl Pts',(-18.3182268241359,21.7384040006107,-13.2541284145615));
#40982=CARTESIAN_POINT('Ctrl Pts',(-18.2354866744585,21.7233990640566,-13.2583022909471));
#40983=CARTESIAN_POINT('Ctrl Pts',(-18.153624027431,21.7043438853204,-13.2624761673326));
#40984=CARTESIAN_POINT('Ctrl Pts',(-18.071819888646,21.6853023255552,-13.2666470605973));
#40985=CARTESIAN_POINT('Ctrl Pts',(-17.9908924531492,21.6622163790631,-13.2708179538619));
#40986=CARTESIAN_POINT('Ctrl Pts',(-17.9112665890495,21.6351925943509,-13.2749888471266));
#40987=CARTESIAN_POINT('Ctrl Pts',(-17.8316596834536,21.6081752438612,-13.2791587473233));
#40988=CARTESIAN_POINT('Ctrl Pts',(-17.753354171139,21.5772220585794,-13.2833286475199));
#40989=CARTESIAN_POINT('Ctrl Pts',(-17.6767596812528,21.5424894184652,-13.2874985477166));
#40990=CARTESIAN_POINT('Ctrl Pts',(-17.6001752728601,21.5077613499186,-13.2916678990641));
#40991=CARTESIAN_POINT('Ctrl Pts',(-17.5253018556168,21.469255010947,-13.2958372504116));
#40992=CARTESIAN_POINT('Ctrl Pts',(-17.4525274999561,21.4271742331394,-13.3000066017591));
#40993=CARTESIAN_POINT('Ctrl Pts',(-17.3797189214394,21.3850736664325,-13.3041779137851));
#40994=CARTESIAN_POINT('Ctrl Pts',(-17.3090117699117,21.339395541617,-13.3083492258111));
#40995=CARTESIAN_POINT('Ctrl Pts',(-17.2407671572916,21.2903882940559,-13.312520537837));
#40996=CARTESIAN_POINT('Ctrl Pts',(-17.2183978647968,21.2743246457625,-13.3138878149775));
#40997=CARTESIAN_POINT('Ctrl Pts',(-17.1962929040477,21.2579036529085,-13.315255092118));
#40998=CARTESIAN_POINT('Ctrl Pts',(-17.1744642439897,21.2411350264762,-13.3166223692584));
#40999=CARTESIAN_POINT('',(-21.2943302428071,19.2116425108278,-12.9667098340901));
#41000=CARTESIAN_POINT('Ctrl Pts',(-21.2939999191096,19.2116435515775,-12.9667098902285));
#41001=CARTESIAN_POINT('Ctrl Pts',(-21.2939911726516,19.2464363059257,-12.9684506873211));
#41002=CARTESIAN_POINT('Ctrl Pts',(-21.2932731600888,19.281219269613,-12.9701914844137));
#41003=CARTESIAN_POINT('Ctrl Pts',(-21.2918468828523,19.3159729673895,-12.9719322815063));
#41004=CARTESIAN_POINT('Ctrl Pts',(-21.2884183105029,19.3995160291397,-12.9761169158993));
#41005=CARTESIAN_POINT('Ctrl Pts',(-21.2808860937369,19.4830464110296,-12.9803015502924));
#41006=CARTESIAN_POINT('Ctrl Pts',(-21.2692483017375,19.5661282142231,-12.9844861846854));
#41007=CARTESIAN_POINT('Ctrl Pts',(-21.2576270746945,19.6490917607532,-12.9886648627693));
#41008=CARTESIAN_POINT('Ctrl Pts',(-21.2419119432712,19.7316075451531,-12.9928435408533));
#41009=CARTESIAN_POINT('Ctrl Pts',(-21.2221529486456,19.8132415662722,-12.9970222189372));
#41010=CARTESIAN_POINT('Ctrl Pts',(-21.2020397882419,19.8963388185507,-13.0012757968227));
#41011=CARTESIAN_POINT('Ctrl Pts',(-21.1777363859676,19.9785219036746,-13.0055293747081));
#41012=CARTESIAN_POINT('Ctrl Pts',(-21.1493505801535,20.0593404829147,-13.0097829525936));
#41013=CARTESIAN_POINT('Ctrl Pts',(-21.1215150885756,20.1385922362917,-13.0139540665715));
#41014=CARTESIAN_POINT('Ctrl Pts',(-21.0897542310845,20.2165314648403,-13.0181251805494));
#41015=CARTESIAN_POINT('Ctrl Pts',(-21.0542203695085,20.292747399774,-13.0222962945274));
#41016=CARTESIAN_POINT('Ctrl Pts',(-21.018698431663,20.3689377597145,-13.0264660088478));
#41017=CARTESIAN_POINT('Ctrl Pts',(-20.9794061983923,20.4434055578918,-13.0306357231681));
#41018=CARTESIAN_POINT('Ctrl Pts',(-20.9365438451405,20.5157607482728,-13.0348054374885));
#41019=CARTESIAN_POINT('Ctrl Pts',(-20.8936830171152,20.5881133639457,-13.0389750034325));
#41020=CARTESIAN_POINT('Ctrl Pts',(-20.8472525568965,20.6583531259272,-13.0431445693766));
#41021=CARTESIAN_POINT('Ctrl Pts',(-20.7974975099507,20.7261165058923,-13.0473141353206));
#41022=CARTESIAN_POINT('Ctrl Pts',(-20.7459931369336,20.796262362702,-13.0516302980595));
#41023=CARTESIAN_POINT('Ctrl Pts',(-20.6909263546122,20.8637540331552,-13.0559464607985));
#41024=CARTESIAN_POINT('Ctrl Pts',(-20.6326151733211,20.928224628182,-13.0602626235374));
#41025=CARTESIAN_POINT('Ctrl Pts',(-20.5762034726275,20.9905951003567,-13.0644381877291));
#41026=CARTESIAN_POINT('Ctrl Pts',(-20.5167558657732,21.0501379976125,-13.0686137519207));
#41027=CARTESIAN_POINT('Ctrl Pts',(-20.4545972806998,21.1065592836016,-13.0727893161124));
#41028=CARTESIAN_POINT('Ctrl Pts',(-20.389299213262,21.1658302746175,-13.077175778125));
#41029=CARTESIAN_POINT('Ctrl Pts',(-20.321009559389,21.2216556522273,-13.0815622401375));
#41030=CARTESIAN_POINT('Ctrl Pts',(-20.2501416763133,21.2737443897259,-13.0859487021501));
#41031=CARTESIAN_POINT('Ctrl Pts',(-20.1792737932376,21.3258331272245,-13.0903351641626));
#41032=CARTESIAN_POINT('Ctrl Pts',(-20.1058282074104,21.3741849690991,-13.0947216261752));
#41033=CARTESIAN_POINT('Ctrl Pts',(-20.0302483510418,21.4185643167123,-13.0991080881878));
#41034=CARTESIAN_POINT('Ctrl Pts',(-19.9581460359011,21.4609017047557,-13.1032927225808));
#41035=CARTESIAN_POINT('Ctrl Pts',(-19.8838331576255,21.4997817138927,-13.1074773569739));
#41036=CARTESIAN_POINT('Ctrl Pts',(-19.8076751930389,21.5349667768393,-13.1116619913669));
#41037=CARTESIAN_POINT('Ctrl Pts',(-19.7316256298885,21.5701017582038,-13.1158406694508));
#41038=CARTESIAN_POINT('Ctrl Pts',(-19.6537366110357,21.6015520487104,-13.1200193475348));
#41039=CARTESIAN_POINT('Ctrl Pts',(-19.5744001491065,21.629124808479,-13.1241980256187));
#41040=CARTESIAN_POINT('Ctrl Pts',(-19.4936416381154,21.6571917901503,-13.1284516035042));
#41041=CARTESIAN_POINT('Ctrl Pts',(-19.4113836985809,21.6812406201864,-13.1327051813896));
#41042=CARTESIAN_POINT('Ctrl Pts',(-19.3280633649497,21.701118213745,-13.136958759275));
#41043=CARTESIAN_POINT('Ctrl Pts',(-19.2463583585722,21.7206104413645,-13.141129873253));
#41044=CARTESIAN_POINT('Ctrl Pts',(-19.1636322517455,21.7360916126581,-13.1453009872309));
#41045=CARTESIAN_POINT('Ctrl Pts',(-19.0803129065814,21.7474674984583,-13.1494721012089));
#41046=CARTESIAN_POINT('Ctrl Pts',(-18.9970215200282,21.7588395669701,-13.1536418155293));
#41047=CARTESIAN_POINT('Ctrl Pts',(-18.9131377459123,21.76610902368,-13.1578115298496));
#41048=CARTESIAN_POINT('Ctrl Pts',(-18.8290979023926,21.7692330599381,-13.16198124417));
#41049=CARTESIAN_POINT('Ctrl Pts',(-18.7450610493711,21.7723569850297,-13.166150810114));
#41050=CARTESIAN_POINT('Ctrl Pts',(-18.6608685977348,21.7713357667235,-13.1703203760581));
#41051=CARTESIAN_POINT('Ctrl Pts',(-18.5769588557388,21.7661786784898,-13.1744899420021));
#41052=CARTESIAN_POINT('Ctrl Pts',(-18.4900989507282,21.7608402733959,-13.178806104741));
#41053=CARTESIAN_POINT('Ctrl Pts',(-18.4035425318193,21.7510697851063,-13.18312226748));
#41054=CARTESIAN_POINT('Ctrl Pts',(-18.3177702276211,21.7369360198915,-13.1874384302189));
#41055=CARTESIAN_POINT('Ctrl Pts',(-18.2347919472105,21.7232626605919,-13.1916139944106));
#41056=CARTESIAN_POINT('Ctrl Pts',(-18.1525479314088,21.7055060719794,-13.1957895586022));
#41057=CARTESIAN_POINT('Ctrl Pts',(-18.0714612955845,21.6837803107335,-13.1999651227939));
#41058=CARTESIAN_POINT('Ctrl Pts',(-17.98627916655,21.6609572329353,-13.2043515848065));
#41059=CARTESIAN_POINT('Ctrl Pts',(-17.9023749641125,21.6337536591884,-13.208738046819));
#41060=CARTESIAN_POINT('Ctrl Pts',(-17.8202171381048,21.6023596302745,-13.2131245088315));
#41061=CARTESIAN_POINT('Ctrl Pts',(-17.7380593120971,21.5709656013606,-13.2175109708441));
#41062=CARTESIAN_POINT('Ctrl Pts',(-17.6576483623233,21.5353814216376,-13.2218974328566));
#41063=CARTESIAN_POINT('Ctrl Pts',(-17.579422411398,21.4958524223455,-13.2262838948691));
#41064=CARTESIAN_POINT('Ctrl Pts',(-17.5048157787013,21.4581523305451,-13.2304674063041));
#41065=CARTESIAN_POINT('Ctrl Pts',(-17.4319187998215,21.4167240952405,-13.2346509177391));
#41066=CARTESIAN_POINT('Ctrl Pts',(-17.361128739488,21.3717462835928,-13.238834429174));
#41067=CARTESIAN_POINT('Ctrl Pts',(-17.2970900087018,21.3310580576203,-13.2426189543074));
#41068=CARTESIAN_POINT('Ctrl Pts',(-17.2347755193382,21.2874657331385,-13.2464034794408));
#41069=CARTESIAN_POINT('Ctrl Pts',(-17.1744642439897,21.2411350264762,-13.2501880045741));
#41070=CARTESIAN_POINT('Ctrl Pts',(-17.1725834302249,21.2436206685575,-12.4500366781978));
#41071=CARTESIAN_POINT('Ctrl Pts',(-17.1023021618046,21.1904720651656,-12.4544341370588));
#41072=CARTESIAN_POINT('Ctrl Pts',(-16.3858468952195,20.5851355922428,-12.5012235314802));
#41073=CARTESIAN_POINT('Ctrl Pts',(-15.7591748512996,18.6509044920109,-12.590404861462));
#41074=CARTESIAN_POINT('Ctrl Pts',(-17.5947352542129,16.4064737508063,-12.7175806681434));
#41075=CARTESIAN_POINT('Ctrl Pts',(-20.4360629288883,16.7305239810473,-12.8430154491748));
#41076=CARTESIAN_POINT('Ctrl Pts',(-21.2952860172943,18.397872866616,-12.9260582946456));
#41077=CARTESIAN_POINT('Ctrl Pts',(-21.2980344808449,19.2116308398979,-12.9667092045559));
#41078=CARTESIAN_POINT('Origin',(-18.734,19.211,1.76670989022852));
#41079=CARTESIAN_POINT('',(-17.1744642439897,21.2411350264762,-11.6500725230732));
#41080=CARTESIAN_POINT('',(-17.1744642439897,21.2411350264762,-11.7167617806966));
#41081=CARTESIAN_POINT('',(-17.1744642439897,21.2411350264762,1.76670989022852));
#41082=CARTESIAN_POINT('',(-21.2939989766127,19.2087109517328,-12.2332901098107));
#41083=CARTESIAN_POINT('Ctrl Pts',(-17.1744642439897,21.2411350264762,-11.7167617806966));
#41084=CARTESIAN_POINT('Ctrl Pts',(-17.1079833326068,21.1900648478714,-11.7209383054901));
#41085=CARTESIAN_POINT('Ctrl Pts',(-17.0439255876479,21.1356580021043,-11.7251148302835));
#41086=CARTESIAN_POINT('Ctrl Pts',(-16.9826417696875,21.0781755003525,-11.7292913550769));
#41087=CARTESIAN_POINT('Ctrl Pts',(-16.9214168264467,21.0207482214358,-11.7334638675269));
#41088=CARTESIAN_POINT('Ctrl Pts',(-16.8629608482341,20.960251472191,-11.7376363799769));
#41089=CARTESIAN_POINT('Ctrl Pts',(-16.807591531515,20.8969864805358,-11.7418088924268));
#41090=CARTESIAN_POINT('Ctrl Pts',(-16.7522505048174,20.8337538130643,-11.7459792730017));
#41091=CARTESIAN_POINT('Ctrl Pts',(-16.6999933106994,20.7677560570195,-11.7501496535766));
#41092=CARTESIAN_POINT('Ctrl Pts',(-16.6510999429969,20.6993303909201,-11.7543200341515));
#41093=CARTESIAN_POINT('Ctrl Pts',(-16.6022168895844,20.6309191595426,-11.7584895349646));
#41094=CARTESIAN_POINT('Ctrl Pts',(-16.5566965201686,20.5600814098146,-11.7626590357778));
#41095=CARTESIAN_POINT('Ctrl Pts',(-16.5147769260435,20.4871853110027,-11.7668285365909));
#41096=CARTESIAN_POINT('Ctrl Pts',(-16.4728536003033,20.4142827230967,-11.7709984085663));
#41097=CARTESIAN_POINT('Ctrl Pts',(-16.4345319145091,20.3393218217299,-11.7751682805418));
#41098=CARTESIAN_POINT('Ctrl Pts',(-16.4000045262528,20.2626963100285,-11.7793381525172));
#41099=CARTESIAN_POINT('Ctrl Pts',(-16.3654407311331,20.185990001757,-11.7835124213488));
#41100=CARTESIAN_POINT('Ctrl Pts',(-16.3346794113464,20.1076159987801,-11.7876866901803));
#41101=CARTESIAN_POINT('Ctrl Pts',(-16.3078652590156,20.0279885057873,-11.7918609590119));
#41102=CARTESIAN_POINT('Ctrl Pts',(-16.2810362895517,19.948317011733,-11.7960375344873));
#41103=CARTESIAN_POINT('Ctrl Pts',(-16.2581589557103,19.86739109131,-11.8002141099626));
#41104=CARTESIAN_POINT('Ctrl Pts',(-16.2393275127547,19.785638304833,-11.8043906854379));
#41105=CARTESIAN_POINT('Ctrl Pts',(-16.2204635694863,19.7037444250189,-11.8085744690709));
#41106=CARTESIAN_POINT('Ctrl Pts',(-16.2056595438309,19.621021282185,-11.8127582527039));
#41107=CARTESIAN_POINT('Ctrl Pts',(-16.1949581671405,19.5379045288606,-11.8169420363368));
#41108=CARTESIAN_POINT('Ctrl Pts',(-16.1872903014398,19.4783488174401,-11.819939846053));
#41109=CARTESIAN_POINT('Ctrl Pts',(-16.1817277091854,19.4185911599263,-11.8229376557691));
#41110=CARTESIAN_POINT('Ctrl Pts',(-16.1782696504243,19.3587916785811,-11.8259354654852));
#41111=CARTESIAN_POINT('Ctrl Pts',(-16.1734425556468,19.2753177459375,-11.8301200998783));
#41112=CARTESIAN_POINT('Ctrl Pts',(-16.172700351485,19.1914517330296,-11.8343047342713));
#41113=CARTESIAN_POINT('Ctrl Pts',(-16.1760879473577,19.1076272233757,-11.8384893686644));
#41114=CARTESIAN_POINT('Ctrl Pts',(-16.1794707214069,19.0239220275358,-11.8426680467483));
#41115=CARTESIAN_POINT('Ctrl Pts',(-16.1869716010008,18.940258673335,-11.8468467248323));
#41116=CARTESIAN_POINT('Ctrl Pts',(-16.1985835897659,18.8570739812961,-11.8510254029162));
#41117=CARTESIAN_POINT('Ctrl Pts',(-16.2104037150842,18.772398263436,-11.8552789808016));
#41118=CARTESIAN_POINT('Ctrl Pts',(-16.2264838103268,18.6882190178967,-11.8595325586871));
#41119=CARTESIAN_POINT('Ctrl Pts',(-16.246760974914,18.604995023049,-11.8637861365725));
#41120=CARTESIAN_POINT('Ctrl Pts',(-16.2666450270981,18.5233844877397,-11.8679572505505));
#41121=CARTESIAN_POINT('Ctrl Pts',(-16.2905647501885,18.4426929623941,-11.8721283645284));
#41122=CARTESIAN_POINT('Ctrl Pts',(-16.3184090347916,18.3633442392081,-11.8762994785064));
#41123=CARTESIAN_POINT('Ctrl Pts',(-16.3462439759762,18.2840221422525,-11.8804691928267));
#41124=CARTESIAN_POINT('Ctrl Pts',(-16.3780007110433,18.2060423862984,-11.8846389071471));
#41125=CARTESIAN_POINT('Ctrl Pts',(-16.4135185064012,18.1298128571494,-11.8888086214675));
#41126=CARTESIAN_POINT('Ctrl Pts',(-16.4490350378836,18.0535860405741,-11.8929781874115));
#41127=CARTESIAN_POINT('Ctrl Pts',(-16.4883121684969,17.9791097436056,-11.8971477533556));
#41128=CARTESIAN_POINT('Ctrl Pts',(-16.5311418982014,17.9067698886546,-11.9013173192996));
#41129=CARTESIAN_POINT('Ctrl Pts',(-16.5754774683661,17.8318866536443,-11.9056334820385));
#41130=CARTESIAN_POINT('Ctrl Pts',(-16.6236198358012,17.7592933443554,-11.9099496447775));
#41131=CARTESIAN_POINT('Ctrl Pts',(-16.6752887227188,17.6893864233008,-11.9142658075164));
#41132=CARTESIAN_POINT('Ctrl Pts',(-16.7252745010797,17.6217567128467,-11.9184413717081));
#41133=CARTESIAN_POINT('Ctrl Pts',(-16.7785602395925,17.5566413947911,-11.9226169358997));
#41134=CARTESIAN_POINT('Ctrl Pts',(-16.8348515919039,17.4943651162737,-11.9267925000914));
#41135=CARTESIAN_POINT('Ctrl Pts',(-16.8939860866005,17.4289434109761,-11.931178962104));
#41136=CARTESIAN_POINT('Ctrl Pts',(-16.9564373882605,17.3666554945532,-11.9355654241165));
#41137=CARTESIAN_POINT('Ctrl Pts',(-17.0218228555023,17.3078317400031,-11.9399518861291));
#41138=CARTESIAN_POINT('Ctrl Pts',(-17.087208322744,17.249007985453,-11.9443383481416));
#41139=CARTESIAN_POINT('Ctrl Pts',(-17.1555274568811,17.1936486989612,-11.9487248101541));
#41140=CARTESIAN_POINT('Ctrl Pts',(-17.2263622218886,17.142032061628,-11.9531112721667));
#41141=CARTESIAN_POINT('Ctrl Pts',(-17.2939377743557,17.0927903822928,-11.9572959065597));
#41142=CARTESIAN_POINT('Ctrl Pts',(-17.3640540780912,17.0467712239068,-11.9614805409528));
#41143=CARTESIAN_POINT('Ctrl Pts',(-17.436370866589,17.0042470387189,-11.9656651753458));
#41144=CARTESIAN_POINT('Ctrl Pts',(-17.5085847210893,16.9617833814452,-11.9698438534298));
#41145=CARTESIAN_POINT('Ctrl Pts',(-17.5829924458181,16.9228050473159,-11.9740225315137));
#41146=CARTESIAN_POINT('Ctrl Pts',(-17.6592229568397,16.8875425961521,-11.9782012095977));
#41147=CARTESIAN_POINT('Ctrl Pts',(-17.7368198449855,16.8516480908938,-11.9824547874831));
#41148=CARTESIAN_POINT('Ctrl Pts',(-17.8163051194014,16.8196042772378,-11.9867083653685));
#41149=CARTESIAN_POINT('Ctrl Pts',(-17.8972589731898,16.7916065937817,-11.990961943254));
#41150=CARTESIAN_POINT('Ctrl Pts',(-17.9766433785541,16.7641517000524,-11.9951330572319));
#41151=CARTESIAN_POINT('Ctrl Pts',(-18.0574394740944,16.7405876095594,-11.9993041712099));
#41152=CARTESIAN_POINT('Ctrl Pts',(-18.1392307762333,16.721050287564,-12.0034752851878));
#41153=CARTESIAN_POINT('Ctrl Pts',(-18.2209946325108,16.7015195215058,-12.0076449995082));
#41154=CARTESIAN_POINT('Ctrl Pts',(-18.303752585082,16.6860129471901,-12.0118147138286));
#41155=CARTESIAN_POINT('Ctrl Pts',(-18.3870746644909,16.6746161939521,-12.0159844281489));
#41156=CARTESIAN_POINT('Ctrl Pts',(-18.4703937789426,16.6632198462596,-12.020153994093));
#41157=CARTESIAN_POINT('Ctrl Pts',(-18.554276524415,16.6559330903703,-12.024323560037));
#41158=CARTESIAN_POINT('Ctrl Pts',(-18.6382858147575,16.6527899236491,-12.0284931259811));
#41159=CARTESIAN_POINT('Ctrl Pts',(-18.7252487681118,16.6495362470634,-12.03280928872));
#41160=CARTESIAN_POINT('Ctrl Pts',(-18.8123468034838,16.6507229779045,-12.0371254514589));
#41161=CARTESIAN_POINT('Ctrl Pts',(-18.8990948495911,16.6563290445464,-12.0414416141978));
#41162=CARTESIAN_POINT('Ctrl Pts',(-18.9830170872208,16.6617524941571,-12.0456171783895));
#41163=CARTESIAN_POINT('Ctrl Pts',(-19.066611324596,16.6713116809416,-12.0497927425812));
#41164=CARTESIAN_POINT('Ctrl Pts',(-19.1494452607506,16.6849348315374,-12.0539683067729));
#41165=CARTESIAN_POINT('Ctrl Pts',(-19.2364629421014,16.6992460550838,-12.0583547687854));
#41166=CARTESIAN_POINT('Ctrl Pts',(-19.3226409276423,16.7180424488712,-12.0627412307979));
#41167=CARTESIAN_POINT('Ctrl Pts',(-19.4074943094423,16.7411810966897,-12.0671276928105));
#41168=CARTESIAN_POINT('Ctrl Pts',(-19.4923476912424,16.7643197445083,-12.071514154823));
#41169=CARTESIAN_POINT('Ctrl Pts',(-19.5758759419184,16.7918003927741,-12.0759006168356));
#41170=CARTESIAN_POINT('Ctrl Pts',(-19.6576188802165,16.8234221134992,-12.0802870788481));
#41171=CARTESIAN_POINT('Ctrl Pts',(-19.7356007047514,16.8535888719792,-12.0844717132412));
#41172=CARTESIAN_POINT('Ctrl Pts',(-19.8122481596155,16.8876362896631,-12.0886563476342));
#41173=CARTESIAN_POINT('Ctrl Pts',(-19.8871479757777,16.9254257295026,-12.0928409820273));
#41174=CARTESIAN_POINT('Ctrl Pts',(-19.9619411813225,16.9631613807519,-12.0970196601112));
#41175=CARTESIAN_POINT('Ctrl Pts',(-20.0349912820117,17.0046282689895,-12.1011983381951));
#41176=CARTESIAN_POINT('Ctrl Pts',(-20.1059035528266,17.0496391690091,-12.1053770162791));
#41177=CARTESIAN_POINT('Ctrl Pts',(-20.1780868751321,17.0954568570628,-12.1096305941645));
#41178=CARTESIAN_POINT('Ctrl Pts',(-20.2480545228571,17.1449466854561,-12.11388417205));
#41179=CARTESIAN_POINT('Ctrl Pts',(-20.3154149295587,17.1978614502303,-12.1181377499354));
#41180=CARTESIAN_POINT('Ctrl Pts',(-20.3814694233333,17.2497503590347,-12.1223088639133));
#41181=CARTESIAN_POINT('Ctrl Pts',(-20.4450164884365,17.3049322938692,-12.1264799778913));
#41182=CARTESIAN_POINT('Ctrl Pts',(-20.5057163649394,17.3631306533724,-12.1306510918693));
#41183=CARTESIAN_POINT('Ctrl Pts',(-20.5663958730124,17.4213094838539,-12.1348208061896));
#41184=CARTESIAN_POINT('Ctrl Pts',(-20.6242297581414,17.4825024106647,-12.13899052051));
#41185=CARTESIAN_POINT('Ctrl Pts',(-20.678913285295,17.5463942470714,-12.1431602348304));
#41186=CARTESIAN_POINT('Ctrl Pts',(-20.733594866574,17.6102838099324,-12.1473298007744));
#41187=CARTESIAN_POINT('Ctrl Pts',(-20.7851260142849,17.6768717413838,-12.1514993667185));
#41188=CARTESIAN_POINT('Ctrl Pts',(-20.8332415555807,17.7458089232721,-12.1556689326625));
#41189=CARTESIAN_POINT('Ctrl Pts',(-20.8830487799516,17.8171698514324,-12.1599850954014));
#41190=CARTESIAN_POINT('Ctrl Pts',(-20.9291954417205,17.8910478705134,-12.1643012581404));
#41191=CARTESIAN_POINT('Ctrl Pts',(-20.971436698905,17.9670237066595,-12.1686174208793));
#41192=CARTESIAN_POINT('Ctrl Pts',(-21.0123019515797,18.0405246379345,-12.172792985071));
#41193=CARTESIAN_POINT('Ctrl Pts',(-21.0495121634691,18.1159883689943,-12.1769685492626));
#41194=CARTESIAN_POINT('Ctrl Pts',(-21.082893688299,18.1930125535797,-12.1811441134543));
#41195=CARTESIAN_POINT('Ctrl Pts',(-21.117961234591,18.2739270466209,-12.1855305754669));
#41196=CARTESIAN_POINT('Ctrl Pts',(-21.1488029510882,18.3565632259543,-12.1899170374794));
#41197=CARTESIAN_POINT('Ctrl Pts',(-21.1752765362398,18.4404360029143,-12.1943034994919));
#41198=CARTESIAN_POINT('Ctrl Pts',(-21.2017501213915,18.5243087798743,-12.1986899615045));
#41199=CARTESIAN_POINT('Ctrl Pts',(-21.2238555029592,18.6094175737551,-12.203076423517));
#41200=CARTESIAN_POINT('Ctrl Pts',(-21.2415125421985,18.6952666864385,-12.2074628855296));
#41201=CARTESIAN_POINT('Ctrl Pts',(-21.2654843862328,18.8118185902907,-12.2134181072291));
#41202=CARTESIAN_POINT('Ctrl Pts',(-21.2813366135111,18.9300931627089,-12.2193733289286));
#41203=CARTESIAN_POINT('Ctrl Pts',(-21.2888788651003,19.0491544419404,-12.2253285506281));
#41204=CARTESIAN_POINT('Ctrl Pts',(-21.2922399536336,19.1022122716411,-12.2279824036759));
#41205=CARTESIAN_POINT('Ctrl Pts',(-21.2939513313562,19.1554260264004,-12.2306362567237));
#41206=CARTESIAN_POINT('Ctrl Pts',(-21.293998976612,19.2087109509454,-12.2332901097715));
#41207=CARTESIAN_POINT('Ctrl Pts',(-21.2939989766127,19.2087109517328,-12.2332901098107));
#41208=CARTESIAN_POINT('Ctrl Pts',(-21.2940747905548,19.2934988599292,-12.2375129674107));
#41209=CARTESIAN_POINT('Ctrl Pts',(-21.2899336304853,19.3784221563149,-12.2417358250107));
#41210=CARTESIAN_POINT('Ctrl Pts',(-21.2815646644668,19.4630203967141,-12.2459586826108));
#41211=CARTESIAN_POINT('Ctrl Pts',(-21.2734134565487,19.5454174151129,-12.2500716626647));
#41212=CARTESIAN_POINT('Ctrl Pts',(-21.2612518149666,19.6275055813485,-12.2541846427187));
#41213=CARTESIAN_POINT('Ctrl Pts',(-21.2451224198776,19.7088596111236,-12.2582976227727));
#41214=CARTESIAN_POINT('Ctrl Pts',(-21.2290007459442,19.7901746966529,-12.2624086339395));
#41215=CARTESIAN_POINT('Ctrl Pts',(-21.20891517906,19.8707558783839,-12.2665196451063));
#41216=CARTESIAN_POINT('Ctrl Pts',(-21.18495989447,19.9501857653523,-12.2706306562731));
#41217=CARTESIAN_POINT('Ctrl Pts',(-21.1610084101081,20.0296030516903,-12.2747410152757));
#41218=CARTESIAN_POINT('Ctrl Pts',(-21.1331885645307,20.1078689519367,-12.2788513742782));
#41219=CARTESIAN_POINT('Ctrl Pts',(-21.1016446063279,20.184580514455,-12.2829617332808));
#41220=CARTESIAN_POINT('Ctrl Pts',(-21.0685960771618,20.2649510340633,-12.2872681465249));
#41221=CARTESIAN_POINT('Ctrl Pts',(-21.0314595036716,20.3436147061448,-12.2915745597691));
#41222=CARTESIAN_POINT('Ctrl Pts',(-20.9904568914614,20.4201328698601,-12.2958809730133));
#41223=CARTESIAN_POINT('Ctrl Pts',(-20.9512718262788,20.4932591677037,-12.2999964933322));
#41224=CARTESIAN_POINT('Ctrl Pts',(-20.9085564982548,20.5644257408166,-12.304112013651));
#41225=CARTESIAN_POINT('Ctrl Pts',(-20.8625501361321,20.6332778624348,-12.3082275339699));
#41226=CARTESIAN_POINT('Ctrl Pts',(-20.8165130556112,20.70217595654,-12.3123458022172));
#41227=CARTESIAN_POINT('Ctrl Pts',(-20.7671808550876,20.768756147345,-12.3164640704645));
#41228=CARTESIAN_POINT('Ctrl Pts',(-20.7148334041511,20.8326963417974,-12.3205823387118));
#41229=CARTESIAN_POINT('Ctrl Pts',(-20.662405465351,20.8967348487665,-12.3247069390843));
#41230=CARTESIAN_POINT('Ctrl Pts',(-20.6069533520093,20.9581249187391,-12.3288315394568));
#41231=CARTESIAN_POINT('Ctrl Pts',(-20.5487934990216,21.0165815007661,-12.3329561398293));
#41232=CARTESIAN_POINT('Ctrl Pts',(-20.5408850965646,21.0245302515484,-12.3335169906232));
#41233=CARTESIAN_POINT('Ctrl Pts',(-20.5329266770598,21.0324248251517,-12.3340778414171));
#41234=CARTESIAN_POINT('Ctrl Pts',(-20.5249190804941,21.040264564551,-12.334638692211));
#41235=CARTESIAN_POINT('Ctrl Pts',(-20.4651725946906,21.0987586301398,-12.338823326604));
#41236=CARTESIAN_POINT('Ctrl Pts',(-20.4024461555817,21.154431359773,-12.3430079609971));
#41237=CARTESIAN_POINT('Ctrl Pts',(-20.3370370650428,21.2069639696395,-12.3471925953901));
#41238=CARTESIAN_POINT('Ctrl Pts',(-20.2717210762482,21.2594218058381,-12.3513712734741));
#41239=CARTESIAN_POINT('Ctrl Pts',(-20.2037303762194,21.3087481146436,-12.355549951558));
#41240=CARTESIAN_POINT('Ctrl Pts',(-20.1333988170805,21.35466110912,-12.3597286296419));
#41241=CARTESIAN_POINT('Ctrl Pts',(-20.0618066152904,21.4013970610254,-12.3639822075274));
#41242=CARTESIAN_POINT('Ctrl Pts',(-19.9877891536758,21.4445957903898,-12.3682357854128));
#41243=CARTESIAN_POINT('Ctrl Pts',(-19.9117335730787,21.484003218397,-12.3724893632982));
#41244=CARTESIAN_POINT('Ctrl Pts',(-19.8371524783218,21.522646656515,-12.3766604772762));
#41245=CARTESIAN_POINT('Ctrl Pts',(-19.7606120124672,21.5576442636059,-12.3808315912541));
#41246=CARTESIAN_POINT('Ctrl Pts',(-19.6825046263017,21.5888012898231,-12.3850027052321));
#41247=CARTESIAN_POINT('Ctrl Pts',(-19.604423449824,21.6199478609992,-12.3891724195525));
#41248=CARTESIAN_POINT('Ctrl Pts',(-19.5247768242091,21.647256240463,-12.3933421338728));
#41249=CARTESIAN_POINT('Ctrl Pts',(-19.4439778217472,21.6705795357392,-12.3975118481932));
#41250=CARTESIAN_POINT('Ctrl Pts',(-19.3631816944606,21.6939020010724,-12.4016814141372));
#41251=CARTESIAN_POINT('Ctrl Pts',(-19.2812337140822,21.713239537401,-12.4058509800813));
#41252=CARTESIAN_POINT('Ctrl Pts',(-19.1985614595125,21.7284953128726,-12.4100205460253));
#41253=CARTESIAN_POINT('Ctrl Pts',(-19.1129825504592,21.7442874625898,-12.4143367087642));
#41254=CARTESIAN_POINT('Ctrl Pts',(-19.0266280073017,21.7557053858608,-12.4186528715032));
#41255=CARTESIAN_POINT('Ctrl Pts',(-18.9399808515256,21.762699803818,-12.4229690342421));
#41256=CARTESIAN_POINT('Ctrl Pts',(-18.8561562177353,21.7694663793458,-12.4271445984338));
#41257=CARTESIAN_POINT('Ctrl Pts',(-18.7720582145671,21.7720932477196,-12.4313201626255));
#41258=CARTESIAN_POINT('Ctrl Pts',(-18.688124977799,21.7705889283903,-12.4354957268171));
#41259=CARTESIAN_POINT('Ctrl Pts',(-18.599952472774,21.7690086294678,-12.4398821888297));
#41260=CARTESIAN_POINT('Ctrl Pts',(-18.5119623987478,21.7628688832023,-12.4442686508422));
#41261=CARTESIAN_POINT('Ctrl Pts',(-18.4246552312347,21.7522409988109,-12.4486551128548));
#41262=CARTESIAN_POINT('Ctrl Pts',(-18.3373480637217,21.7416131144196,-12.4530415748673));
#41263=CARTESIAN_POINT('Ctrl Pts',(-18.2507243612258,21.7264972665758,-12.4574280368799));
#41264=CARTESIAN_POINT('Ctrl Pts',(-18.1652685194105,21.7070257416514,-12.4618144988924));
#41265=CARTESIAN_POINT('Ctrl Pts',(-18.0837368018496,21.6884483473282,-12.4659995349801));
#41266=CARTESIAN_POINT('Ctrl Pts',(-18.0029645350277,21.6658373731168,-12.4701845710677));
#41267=CARTESIAN_POINT('Ctrl Pts',(-17.9233808127673,21.6392702759969,-12.4743696071554));
#41268=CARTESIAN_POINT('Ctrl Pts',(-17.8439306160917,21.6127477531578,-12.4785476215887));
#41269=CARTESIAN_POINT('Ctrl Pts',(-17.7656654318222,21.5822824489659,-12.482725636022));
#41270=CARTESIAN_POINT('Ctrl Pts',(-17.6890027068815,21.5480024940883,-12.4869036504553));
#41271=CARTESIAN_POINT('Ctrl Pts',(-17.6124142566805,21.5137557513712,-12.4910776170161));
#41272=CARTESIAN_POINT('Ctrl Pts',(-17.5374256011855,21.4757018817769,-12.4952515835769));
#41273=CARTESIAN_POINT('Ctrl Pts',(-17.4644368058601,21.4340180602247,-12.4994255501377));
#41274=CARTESIAN_POINT('Ctrl Pts',(-17.3915013099496,21.3923646779103,-12.5035964686968));
#41275=CARTESIAN_POINT('Ctrl Pts',(-17.3205631705258,21.3470868385412,-12.5077673872559));
#41276=CARTESIAN_POINT('Ctrl Pts',(-17.251999007923,21.2984082158224,-12.511938305815));
#41277=CARTESIAN_POINT('Ctrl Pts',(-17.2258011156292,21.2798084507762,-12.5135319849474));
#41278=CARTESIAN_POINT('Ctrl Pts',(-17.1999495451948,21.2607126594728,-12.5151256640799));
#41279=CARTESIAN_POINT('Ctrl Pts',(-17.1744642439897,21.2411350264762,-12.5167193432124));
#41280=CARTESIAN_POINT('',(-21.2939992159918,19.2130035272629,-12.1667098902285));
#41281=CARTESIAN_POINT('Ctrl Pts',(-21.2916489709697,19.2130199896839,-12.1667107986323));
#41282=CARTESIAN_POINT('Ctrl Pts',(-21.2937097175741,19.4962014444643,-12.1807663462274));
#41283=CARTESIAN_POINT('Ctrl Pts',(-21.1196060444512,20.6310006101477,-12.2372138293831));
#41284=CARTESIAN_POINT('Ctrl Pts',(-19.5298543885185,22.0831545624874,-12.3316557892382));
#41285=CARTESIAN_POINT('Ctrl Pts',(-17.7798204959642,21.7028298248134,-12.4120422014983));
#41286=CARTESIAN_POINT('Ctrl Pts',(-17.1725834302249,21.2436206685575,-12.4500366781978));
#41287=CARTESIAN_POINT('Ctrl Pts',(-17.1744642439897,21.2411350264762,-11.6500725230732));
#41288=CARTESIAN_POINT('Ctrl Pts',(-17.1077138936498,21.189857866719,-11.6542476640414));
#41289=CARTESIAN_POINT('Ctrl Pts',(-17.0435214358735,21.1353053413385,-11.6584228050097));
#41290=CARTESIAN_POINT('Ctrl Pts',(-16.9822123288039,21.0777726040001,-11.6625979459779));
#41291=CARTESIAN_POINT('Ctrl Pts',(-16.9208932902774,21.0202305469385,-11.6667737632768));
#41292=CARTESIAN_POINT('Ctrl Pts',(-16.8624588433937,20.9597076574843,-11.6709495805758));
#41293=CARTESIAN_POINT('Ctrl Pts',(-16.807196255566,20.8965347313049,-11.6751253978747));
#41294=CARTESIAN_POINT('Ctrl Pts',(-16.7518333577028,20.8332471366179,-11.6793087949197));
#41295=CARTESIAN_POINT('Ctrl Pts',(-16.6996541106652,20.7673002542451,-11.6834921919647));
#41296=CARTESIAN_POINT('Ctrl Pts',(-16.6509045356354,20.6990568827647,-11.6876755890097));
#41297=CARTESIAN_POINT('Ctrl Pts',(-16.6023552598585,20.6310939054482,-11.6918417975705));
#41298=CARTESIAN_POINT('Ctrl Pts',(-16.5572076916088,20.5608537004042,-11.6960080061312));
#41299=CARTESIAN_POINT('Ctrl Pts',(-16.5156592733602,20.4887184433712,-11.7001742146919));
#41300=CARTESIAN_POINT('Ctrl Pts',(-16.4739270995035,20.4162641547462,-11.704358849085));
#41301=CARTESIAN_POINT('Ctrl Pts',(-16.4356706929266,20.341628329944,-11.708543483478));
#41302=CARTESIAN_POINT('Ctrl Pts',(-16.4011245523601,20.2651784221843,-11.712728117871));
#41303=CARTESIAN_POINT('Ctrl Pts',(-16.3666275839488,20.1888373314056,-11.716906795955));
#41304=CARTESIAN_POINT('Ctrl Pts',(-16.3358305794285,20.1106877022102,-11.7210854740389));
#41305=CARTESIAN_POINT('Ctrl Pts',(-16.3089230895031,20.0311231481764,-11.7252641521229));
#41306=CARTESIAN_POINT('Ctrl Pts',(-16.2815333021588,19.9501324566934,-11.7295177300083));
#41307=CARTESIAN_POINT('Ctrl Pts',(-16.258174080664,19.8676760341798,-11.7337713078938));
#41308=CARTESIAN_POINT('Ctrl Pts',(-16.2389948450999,19.7841921815777,-11.7380248857792));
#41309=CARTESIAN_POINT('Ctrl Pts',(-16.2201874364424,19.7023268263637,-11.7421959997571));
#41310=CARTESIAN_POINT('Ctrl Pts',(-16.2053994934178,19.6194739920342,-11.7463671137351));
#41311=CARTESIAN_POINT('Ctrl Pts',(-16.194721659298,19.5360623147052,-11.7505382277131));
#41312=CARTESIAN_POINT('Ctrl Pts',(-16.1840474082286,19.4526786269702,-11.7547079420334));
#41313=CARTESIAN_POINT('Ctrl Pts',(-16.1774805853424,19.3687369245932,-11.7588776563538));
#41314=CARTESIAN_POINT('Ctrl Pts',(-16.1750603443919,19.2846738688843,-11.7630473706742));
#41315=CARTESIAN_POINT('Ctrl Pts',(-16.172640189564,19.2006138044998,-11.7672169366182));
#41316=CARTESIAN_POINT('Ctrl Pts',(-16.1743663356855,19.1164328552362,-11.7713865025623));
#41317=CARTESIAN_POINT('Ctrl Pts',(-16.1802258395509,19.0325692363342,-11.7755560685063));
#41318=CARTESIAN_POINT('Ctrl Pts',(-16.1862913563437,18.9457570760485,-11.7798722312452));
#41319=CARTESIAN_POINT('Ctrl Pts',(-16.1967862597981,18.8592855021225,-11.7841883939841));
#41320=CARTESIAN_POINT('Ctrl Pts',(-16.2116377216372,18.7736345501845,-11.7885045567231));
#41321=CARTESIAN_POINT('Ctrl Pts',(-16.226005398669,18.6907736689971,-11.7926801209147));
#41322=CARTESIAN_POINT('Ctrl Pts',(-16.2444500136974,18.6086812165377,-11.7968556851064));
#41323=CARTESIAN_POINT('Ctrl Pts',(-16.2668539711945,18.527779338318,-11.8010312492981));
#41324=CARTESIAN_POINT('Ctrl Pts',(-16.2903894993245,18.4427912985553,-11.8054177113106));
#41325=CARTESIAN_POINT('Ctrl Pts',(-16.3182946694534,18.3591178195347,-11.8098041733232));
#41326=CARTESIAN_POINT('Ctrl Pts',(-16.3503755250187,18.2772257434101,-11.8141906353357));
#41327=CARTESIAN_POINT('Ctrl Pts',(-16.382456380584,18.1953336672856,-11.8185770973483));
#41328=CARTESIAN_POINT('Ctrl Pts',(-16.4187126130535,18.1152234912951,-11.8229635593608));
#41329=CARTESIAN_POINT('Ctrl Pts',(-16.4588952312817,18.0373312684769,-11.8273500213734));
#41330=CARTESIAN_POINT('Ctrl Pts',(-16.4972289876803,17.9630229822945,-11.8315346557664));
#41331=CARTESIAN_POINT('Ctrl Pts',(-16.5392784376737,17.8904564421858,-11.8357192901595));
#41332=CARTESIAN_POINT('Ctrl Pts',(-16.5848615409703,17.8200277199314,-11.8399039245525));
#41333=CARTESIAN_POINT('Ctrl Pts',(-16.6303797623612,17.749699244246,-11.8440826026365));
#41334=CARTESIAN_POINT('Ctrl Pts',(-16.6794213986321,17.6815029251176,-11.8482612807204));
#41335=CARTESIAN_POINT('Ctrl Pts',(-16.7317580832552,17.6158112002556,-11.8524399588043));
#41336=CARTESIAN_POINT('Ctrl Pts',(-16.7850328653365,17.5489419984372,-11.8566935366898));
#41337=CARTESIAN_POINT('Ctrl Pts',(-16.8417217641062,17.4846684922401,-11.8609471145752));
#41338=CARTESIAN_POINT('Ctrl Pts',(-16.9015371160905,17.4233535642935,-11.8652006924606));
#41339=CARTESIAN_POINT('Ctrl Pts',(-16.9601928307565,17.3632273458715,-11.8693718064386));
#41340=CARTESIAN_POINT('Ctrl Pts',(-17.0218545195986,17.3059463582363,-11.8735429204166));
#41341=CARTESIAN_POINT('Ctrl Pts',(-17.0862108309601,17.2518188306349,-11.8777140343945));
#41342=CARTESIAN_POINT('Ctrl Pts',(-17.15054554694,17.1977094660481,-11.8818837487149));
#41343=CARTESIAN_POINT('Ctrl Pts',(-17.2175727378981,17.1467517558066,-11.8860534630352));
#41344=CARTESIAN_POINT('Ctrl Pts',(-17.2869464339594,17.0992149785054,-11.8902231773556));
#41345=CARTESIAN_POINT('Ctrl Pts',(-17.3563176614068,17.0516798927667,-11.8943927432997));
#41346=CARTESIAN_POINT('Ctrl Pts',(-17.4280348479702,17.0075657572679,-11.8985623092437));
#41347=CARTESIAN_POINT('Ctrl Pts',(-17.5017225180694,16.9670988864198,-11.9027318751878));
#41348=CARTESIAN_POINT('Ctrl Pts',(-17.5780009557457,16.9252092503139,-11.9070480379267));
#41349=CARTESIAN_POINT('Ctrl Pts',(-17.6563905571825,16.8872283803615,-11.9113642006656));
#41350=CARTESIAN_POINT('Ctrl Pts',(-17.7364482678186,16.8533548736882,-11.9156803634045));
#41351=CARTESIAN_POINT('Ctrl Pts',(-17.8138981069513,16.8205847929319,-11.9198559275962));
#41352=CARTESIAN_POINT('Ctrl Pts',(-17.8929085883425,16.7916587077374,-11.9240314917879));
#41353=CARTESIAN_POINT('Ctrl Pts',(-17.9730611021941,16.7667062382345,-11.9282070559796));
#41354=CARTESIAN_POINT('Ctrl Pts',(-18.0572619289758,16.7404934788158,-11.9325935179921));
#41355=CARTESIAN_POINT('Ctrl Pts',(-18.1427226225442,16.7186664436046,-11.9369799800047));
#41356=CARTESIAN_POINT('Ctrl Pts',(-18.2289456575188,16.7013147386294,-11.9413664420172));
#41357=CARTESIAN_POINT('Ctrl Pts',(-18.3151686924934,16.6839630336542,-11.9457529040297));
#41358=CARTESIAN_POINT('Ctrl Pts',(-18.4021534837731,16.6710866686339,-11.9501393660423));
#41359=CARTESIAN_POINT('Ctrl Pts',(-18.4893986055749,16.662712308658,-11.9545258280548));
#41360=CARTESIAN_POINT('Ctrl Pts',(-18.5726294499944,16.6547232653983,-11.9587104624479));
#41361=CARTESIAN_POINT('Ctrl Pts',(-18.6564069960725,16.6508013065455,-11.9628950968409));
#41362=CARTESIAN_POINT('Ctrl Pts',(-18.740299675164,16.6510077511655,-11.967079731234));
#41363=CARTESIAN_POINT('Ctrl Pts',(-18.8240729434104,16.6512139019371,-11.9712584093179));
#41364=CARTESIAN_POINT('Ctrl Pts',(-18.907960563061,16.655536782935,-11.9754370874018));
#41365=CARTESIAN_POINT('Ctrl Pts',(-18.9915257624718,16.6639859675174,-11.9796157654858));
#41366=CARTESIAN_POINT('Ctrl Pts',(-19.076588808025,16.6725865976611,-11.9838693433712));
#41367=CARTESIAN_POINT('Ctrl Pts',(-19.1613172809479,16.6854629604527,-11.9881229212567));
#41368=CARTESIAN_POINT('Ctrl Pts',(-19.2452503475945,16.702569597919,-11.9923764991421));
#41369=CARTESIAN_POINT('Ctrl Pts',(-19.3275562079622,16.7193445898371,-11.99654761312));
#41370=CARTESIAN_POINT('Ctrl Pts',(-19.4090967563144,16.7401871997923,-12.000718727098));
#41371=CARTESIAN_POINT('Ctrl Pts',(-19.4894442918863,16.7650024689595,-12.004889841076));
#41372=CARTESIAN_POINT('Ctrl Pts',(-19.5697648660668,16.7898094111234,-12.0090595553963));
#41373=CARTESIAN_POINT('Ctrl Pts',(-19.6488927833418,16.818586229372,-12.0132292697167));
#41374=CARTESIAN_POINT('Ctrl Pts',(-19.7264143560957,16.8511877731872,-12.0173989840371));
#41375=CARTESIAN_POINT('Ctrl Pts',(-19.8039331702993,16.8837881568995,-12.0215685499811));
#41376=CARTESIAN_POINT('Ctrl Pts',(-19.8798453299031,16.9202128164537,-12.0257381159252));
#41377=CARTESIAN_POINT('Ctrl Pts',(-19.9537573024926,16.9602685360053,-12.0299076818692));
#41378=CARTESIAN_POINT('Ctrl Pts',(-20.0302679288583,17.0017325652423,-12.0342238446081));
#41379=CARTESIAN_POINT('Ctrl Pts',(-20.1046346343667,17.0470874900863,-12.038540007347));
#41380=CARTESIAN_POINT('Ctrl Pts',(-20.1764506132331,17.0960682686234,-12.042856170086));
#41381=CARTESIAN_POINT('Ctrl Pts',(-20.2459271941416,17.1434535034516,-12.0470317342777));
#41382=CARTESIAN_POINT('Ctrl Pts',(-20.3130163291627,17.1942316733327,-12.0512072984693));
#41383=CARTESIAN_POINT('Ctrl Pts',(-20.377382442736,17.2481209545907,-12.055382862661));
#41384=CARTESIAN_POINT('Ctrl Pts',(-20.44499953569,17.3047320553354,-12.0597693246736));
#41385=CARTESIAN_POINT('Ctrl Pts',(-20.5096108706378,17.3647764140011,-12.0641557866861));
#41386=CARTESIAN_POINT('Ctrl Pts',(-20.5708718020377,17.4278841925218,-12.0685422486987));
#41387=CARTESIAN_POINT('Ctrl Pts',(-20.6321327334376,17.4909919710424,-12.0729287107112));
#41388=CARTESIAN_POINT('Ctrl Pts',(-20.6900429364134,17.5571626827011,-12.0773151727237));
#41389=CARTESIAN_POINT('Ctrl Pts',(-20.7443085775788,17.625989141074,-12.0817016347363));
#41390=CARTESIAN_POINT('Ctrl Pts',(-20.796026764239,17.6915845997261,-12.0858821780095));
#41391=CARTESIAN_POINT('Ctrl Pts',(-20.8446312405901,17.7598411080022,-12.0900627212828));
#41392=CARTESIAN_POINT('Ctrl Pts',(-20.8898359348525,17.8304307616065,-12.0942432645561));
#41393=CARTESIAN_POINT('Ctrl Pts',(-20.934977871844,17.9009224162288,-12.0984180040186));
#41394=CARTESIAN_POINT('Ctrl Pts',(-20.9767291512529,17.9737404018926,-12.1025927434812));
#41395=CARTESIAN_POINT('Ctrl Pts',(-21.0148441174676,18.0485241457073,-12.1067674829438));
#41396=CARTESIAN_POINT('Ctrl Pts',(-21.0529176328928,18.1232265607022,-12.1109376822936));
#41397=CARTESIAN_POINT('Ctrl Pts',(-21.087362480976,18.199890080528,-12.1151078816434));
#41398=CARTESIAN_POINT('Ctrl Pts',(-21.1179772351417,18.2781267276172,-12.1192780809931));
#41399=CARTESIAN_POINT('Ctrl Pts',(-21.1485693987601,18.3563056440885,-12.1234452031637));
#41400=CARTESIAN_POINT('Ctrl Pts',(-21.1753369141585,18.436054955007,-12.1276123253342));
#41401=CARTESIAN_POINT('Ctrl Pts',(-21.198125670353,18.5169649283305,-12.1317794475048));
#41402=CARTESIAN_POINT('Ctrl Pts',(-21.2209040463211,18.5978380473459,-12.1359446715607));
#41403=CARTESIAN_POINT('Ctrl Pts',(-21.2397071410263,18.6798703351908,-12.1401098956166));
#41404=CARTESIAN_POINT('Ctrl Pts',(-21.2544305326007,18.7626363860277,-12.1442751196726));
#41405=CARTESIAN_POINT('Ctrl Pts',(-21.2691564647158,18.8454167182569,-12.1484410624434));
#41406=CARTESIAN_POINT('Ctrl Pts',(-21.279801198365,18.9289306143289,-12.1526070052143));
#41407=CARTESIAN_POINT('Ctrl Pts',(-21.2863115236392,19.0127428783158,-12.1567729479852));
#41408=CARTESIAN_POINT('Ctrl Pts',(-21.2914878410454,19.0793814658917,-12.1600852620663));
#41409=CARTESIAN_POINT('Ctrl Pts',(-21.2940514917317,19.1462084026767,-12.1633975761474));
#41410=CARTESIAN_POINT('Ctrl Pts',(-21.2939992159918,19.2130035272629,-12.1667098902285));
#41411=CARTESIAN_POINT('Origin',(-18.734,19.211,1.76670989022852));
#41412=CARTESIAN_POINT('',(-17.1757181329867,21.2395346319231,-10.8502164826864));
#41413=CARTESIAN_POINT('',(-17.173194974388,21.2428171613069,-10.9165936635695));
#41414=CARTESIAN_POINT('',(-17.1744642439897,21.2411350264762,1.76670989022852));
#41415=CARTESIAN_POINT('',(-21.2940197026037,19.2123010442705,-11.4332901032639));
#41416=CARTESIAN_POINT('Ctrl Pts',(-17.173194974388,21.2428171613069,-10.9165936635695));
#41417=CARTESIAN_POINT('Ctrl Pts',(-17.0711420934188,21.1659200956527,-10.9229640486181));
#41418=CARTESIAN_POINT('Ctrl Pts',(-16.3366272634488,20.5183600625041,-10.9717263692271));
#41419=CARTESIAN_POINT('Ctrl Pts',(-15.788288410751,18.513809214,-11.0628806253966));
#41420=CARTESIAN_POINT('Ctrl Pts',(-17.7257693047706,16.3567465732145,-11.1900564320781));
#41421=CARTESIAN_POINT('Ctrl Pts',(-20.5048168878155,16.8048334715693,-11.3135258905415));
#41422=CARTESIAN_POINT('Ctrl Pts',(-21.2925957841654,18.43736680388,-11.3946034134446));
#41423=CARTESIAN_POINT('Ctrl Pts',(-21.297413587737,19.2122806855485,-11.4332890007871));
#41424=CARTESIAN_POINT('Ctrl Pts',(-21.2939996693303,19.212301164443,-11.4332901097715));
#41425=CARTESIAN_POINT('Ctrl Pts',(-21.293961988618,19.2864367677247,-11.436996088328));
#41426=CARTESIAN_POINT('Ctrl Pts',(-21.2907042434478,19.3604881810636,-11.4407020668845));
#41427=CARTESIAN_POINT('Ctrl Pts',(-21.2842464642989,19.4342553948533,-11.444408045441));
#41428=CARTESIAN_POINT('Ctrl Pts',(-21.2769546129518,19.5175502156942,-11.4485926798341));
#41429=CARTESIAN_POINT('Ctrl Pts',(-21.2655641024497,19.6006424250678,-11.4527773142271));
#41430=CARTESIAN_POINT('Ctrl Pts',(-21.250093180474,19.6830965019697,-11.4569619486202));
#41431=CARTESIAN_POINT('Ctrl Pts',(-21.2346442794409,19.7654332156989,-11.4611406267041));
#41432=CARTESIAN_POINT('Ctrl Pts',(-21.2151265874821,19.8471331528555,-11.465319304788));
#41433=CARTESIAN_POINT('Ctrl Pts',(-21.1916101807318,19.9277650937117,-11.469497982872));
#41434=CARTESIAN_POINT('Ctrl Pts',(-21.1676722592913,20.0098423041587,-11.4737515607574));
#41435=CARTESIAN_POINT('Ctrl Pts',(-21.1395909011584,20.0908123737399,-11.4780051386429));
#41436=CARTESIAN_POINT('Ctrl Pts',(-21.107494673889,20.170230437914,-11.4822587165283));
#41437=CARTESIAN_POINT('Ctrl Pts',(-21.0760206946157,20.2481088279425,-11.4864298305062));
#41438=CARTESIAN_POINT('Ctrl Pts',(-21.0406863094725,20.3244944066984,-11.4906009444842));
#41439=CARTESIAN_POINT('Ctrl Pts',(-21.0016627302193,20.3989838980282,-11.4947720584621));
#41440=CARTESIAN_POINT('Ctrl Pts',(-20.962652245705,20.4734483936899,-11.4989417727825));
#41441=CARTESIAN_POINT('Ctrl Pts',(-20.9199552389621,20.5460176583684,-11.5031114871029));
#41442=CARTESIAN_POINT('Ctrl Pts',(-20.873789724926,20.6163113295996,-11.5072812014233));
#41443=CARTESIAN_POINT('Ctrl Pts',(-20.827625853657,20.6866024994803,-11.5114507673673));
#41444=CARTESIAN_POINT('Ctrl Pts',(-20.7779939737414,20.7546178528605,-11.5156203333114));
#41445=CARTESIAN_POINT('Ctrl Pts',(-20.7251556946207,20.8200055934581,-11.5197898992554));
#41446=CARTESIAN_POINT('Ctrl Pts',(-20.6704596867893,20.8876922863505,-11.5241060619943));
#41447=CARTESIAN_POINT('Ctrl Pts',(-20.6123279420986,20.9525627446113,-11.5284222247332));
#41448=CARTESIAN_POINT('Ctrl Pts',(-20.5510951122121,21.0142651921375,-11.5327383874721));
#41449=CARTESIAN_POINT('Ctrl Pts',(-20.4918569353186,21.0739576889255,-11.5369139516638));
#41450=CARTESIAN_POINT('Ctrl Pts',(-20.4297169860235,21.1306851185865,-11.5410895158555));
#41451=CARTESIAN_POINT('Ctrl Pts',(-20.3650134540522,21.1841687998498,-11.5452650800472));
#41452=CARTESIAN_POINT('Ctrl Pts',(-20.2970419004992,21.2403538147082,-11.5496515420597));
#41453=CARTESIAN_POINT('Ctrl Pts',(-20.2262414538862,21.2929584378006,-11.5540380040723));
#41454=CARTESIAN_POINT('Ctrl Pts',(-20.1530384991425,21.3417110873958,-11.5584244660848));
#41455=CARTESIAN_POINT('Ctrl Pts',(-20.0798355443987,21.390463736991,-11.5628109280973));
#41456=CARTESIAN_POINT('Ctrl Pts',(-20.0042306192381,21.4353641822177,-11.5671973901099));
#41457=CARTESIAN_POINT('Ctrl Pts',(-19.9266775857363,21.4761976020829,-11.5715838521224));
#41458=CARTESIAN_POINT('Ctrl Pts',(-19.852692882267,21.5151522157705,-11.5757684865155));
#41459=CARTESIAN_POINT('Ctrl Pts',(-19.7766600165144,21.5505508359911,-11.5799531209085));
#41460=CARTESIAN_POINT('Ctrl Pts',(-19.6989550698443,21.5821730668978,-11.5841377553015));
#41461=CARTESIAN_POINT('Ctrl Pts',(-19.6213607265478,21.6137502874729,-11.5883164333855));
#41462=CARTESIAN_POINT('Ctrl Pts',(-19.5420994522195,21.6415616236984,-11.5924951114694));
#41463=CARTESIAN_POINT('Ctrl Pts',(-19.4615717652906,21.6654325874531,-11.5966737895534));
#41464=CARTESIAN_POINT('Ctrl Pts',(-19.3796006774477,21.6897314210775,-11.6009273674388));
#41465=CARTESIAN_POINT('Ctrl Pts',(-19.2963177561689,21.7099470058045,-11.6051809453242));
#41466=CARTESIAN_POINT('Ctrl Pts',(-19.2121666533117,21.7259466498637,-11.6094345232097));
#41467=CARTESIAN_POINT('Ctrl Pts',(-19.1296469837908,21.7416361096021,-11.6136056371876));
#41468=CARTESIAN_POINT('Ctrl Pts',(-19.0462929678286,21.7532715484977,-11.6177767511656));
#41469=CARTESIAN_POINT('Ctrl Pts',(-18.9625363705288,21.760778642813,-11.6219478651435));
#41470=CARTESIAN_POINT('Ctrl Pts',(-18.878807878564,21.7682832180503,-11.6261175794639));
#41471=CARTESIAN_POINT('Ctrl Pts',(-18.7946775313674,21.7716621589129,-11.6302872937843));
#41472=CARTESIAN_POINT('Ctrl Pts',(-18.7105831609272,21.7708928984721,-11.6344570081046));
#41473=CARTESIAN_POINT('Ctrl Pts',(-18.6264917829255,21.7701236654048,-11.6386265740487));
#41474=CARTESIAN_POINT('Ctrl Pts',(-18.5424368391406,21.7652065295826,-11.6427961399927));
#41475=CARTESIAN_POINT('Ctrl Pts',(-18.4588557388016,21.75617104249,-11.6469657059368));
#41476=CARTESIAN_POINT('Ctrl Pts',(-18.372336030083,21.7468178788176,-11.6512818686757));
#41477=CARTESIAN_POINT('Ctrl Pts',(-18.2863246298128,21.7330514297719,-11.6555980314146));
#41478=CARTESIAN_POINT('Ctrl Pts',(-18.2012984666221,21.7149626747092,-11.6599141941535));
#41479=CARTESIAN_POINT('Ctrl Pts',(-18.1190420217543,21.6974631589401,-11.6640897583452));
#41480=CARTESIAN_POINT('Ctrl Pts',(-18.0377080547437,21.6759187771978,-11.6682653225369));
#41481=CARTESIAN_POINT('Ctrl Pts',(-17.957713948121,21.6504630486355,-11.6724408867286));
#41482=CARTESIAN_POINT('Ctrl Pts',(-17.8736795293404,21.6237216117387,-11.6768273487411));
#41483=CARTESIAN_POINT('Ctrl Pts',(-17.7911244272666,21.592663525305,-11.6812138107537));
#41484=CARTESIAN_POINT('Ctrl Pts',(-17.710507793232,21.5575003095429,-11.6856002727662));
#41485=CARTESIAN_POINT('Ctrl Pts',(-17.6298911591974,21.5223370937809,-11.6899867347788));
#41486=CARTESIAN_POINT('Ctrl Pts',(-17.5512134783825,21.4830690758564,-11.6943731967913));
#41487=CARTESIAN_POINT('Ctrl Pts',(-17.4749010481796,21.4399616034209,-11.6987596588039));
#41488=CARTESIAN_POINT('Ctrl Pts',(-17.4021059540594,21.3988410087172,-11.7029439432541));
#41489=CARTESIAN_POINT('Ctrl Pts',(-17.3311919413494,21.3540740524414,-11.7071282277043));
#41490=CARTESIAN_POINT('Ctrl Pts',(-17.2625477971258,21.3058576120244,-11.7113125121546));
#41491=CARTESIAN_POINT('Ctrl Pts',(-17.2327489645208,21.2849265675333,-11.7131289350019));
#41492=CARTESIAN_POINT('Ctrl Pts',(-17.2033776234909,21.263346085628,-11.7149453578493));
#41493=CARTESIAN_POINT('Ctrl Pts',(-17.1744642439897,21.2411350264762,-11.7167617806966));
#41494=CARTESIAN_POINT('',(-21.2939995125392,19.2094201902091,-11.3667098902285));
#41495=CARTESIAN_POINT('Ctrl Pts',(-21.2939995125392,19.2094201902091,-11.3667098902285));
#41496=CARTESIAN_POINT('Ctrl Pts',(-21.2940518853803,19.2942876523606,-11.3709134538372));
#41497=CARTESIAN_POINT('Ctrl Pts',(-21.2898797137862,19.3791700299233,-11.3751170174459));
#41498=CARTESIAN_POINT('Ctrl Pts',(-21.2815050782104,19.4636220031829,-11.3793205810546));
#41499=CARTESIAN_POINT('Ctrl Pts',(-21.2731292177987,19.5480863280015,-11.3835247594572));
#41500=CARTESIAN_POINT('Ctrl Pts',(-21.2605497166712,19.6321196761629,-11.3877289378599));
#41501=CARTESIAN_POINT('Ctrl Pts',(-21.2438404672875,19.7152824890537,-11.3919331162626));
#41502=CARTESIAN_POINT('Ctrl Pts',(-21.2271240709727,19.7984808725961,-11.3961390928892));
#41503=CARTESIAN_POINT('Ctrl Pts',(-21.2062745049673,19.880807540606,-11.4003450695159));
#41504=CARTESIAN_POINT('Ctrl Pts',(-21.1814163656275,19.9618349574033,-11.4045510461425));
#41505=CARTESIAN_POINT('Ctrl Pts',(-21.1565238219895,20.0429745182095,-11.408762843948));
#41506=CARTESIAN_POINT('Ctrl Pts',(-21.1276117659035,20.1228108093803,-11.4129746417534));
#41507=CARTESIAN_POINT('Ctrl Pts',(-21.0948539828414,20.2009335693377,-11.4171864395589));
#41508=CARTESIAN_POINT('Ctrl Pts',(-21.0620694457195,20.2791201340097,-11.4214016772397));
#41509=CARTESIAN_POINT('Ctrl Pts',(-21.0254331231615,20.3555899771933,-11.4256169149205));
#41510=CARTESIAN_POINT('Ctrl Pts',(-20.9851650013542,20.4299569872141,-11.4298321526013));
#41511=CARTESIAN_POINT('Ctrl Pts',(-20.9448260993909,20.5044547137502,-11.4340547994973));
#41512=CARTESIAN_POINT('Ctrl Pts',(-20.9008428915854,20.5768418481601,-11.4382774463933));
#41513=CARTESIAN_POINT('Ctrl Pts',(-20.8534787082554,20.6467611240217,-11.4425000932893));
#41514=CARTESIAN_POINT('Ctrl Pts',(-20.8410561777284,20.6650993339886,-11.4436075959693));
#41515=CARTESIAN_POINT('Ctrl Pts',(-20.8284012848672,20.6832679625288,-11.4447150986492));
#41516=CARTESIAN_POINT('Ctrl Pts',(-20.8155192213964,20.7012609606902,-11.4458226013291));
#41517=CARTESIAN_POINT('Ctrl Pts',(-20.7668450946151,20.7692464566218,-11.4500072357222));
#41518=CARTESIAN_POINT('Ctrl Pts',(-20.7147461245074,20.8349713096213,-11.4541918701152));
#41519=CARTESIAN_POINT('Ctrl Pts',(-20.6594597008472,20.8980699275411,-11.4583765045082));
#41520=CARTESIAN_POINT('Ctrl Pts',(-20.6042519705679,20.9610787323882,-11.4625551825922));
#41521=CARTESIAN_POINT('Ctrl Pts',(-20.5458660991118,21.0214683841929,-11.4667338606761));
#41522=CARTESIAN_POINT('Ctrl Pts',(-20.4845818988862,21.0789033741851,-11.4709125387601));
#41523=CARTESIAN_POINT('Ctrl Pts',(-20.4221992234157,21.1373678450951,-11.4751661166455));
#41524=CARTESIAN_POINT('Ctrl Pts',(-20.356813572753,21.1927702956727,-11.4794196945309));
#41525=CARTESIAN_POINT('Ctrl Pts',(-20.2887620518457,21.2447932446885,-11.4836732724164));
#41526=CARTESIAN_POINT('Ctrl Pts',(-20.2220298424627,21.2958076273232,-11.4878443863943));
#41527=CARTESIAN_POINT('Ctrl Pts',(-20.1527345889112,21.3435720832561,-11.4920155003723));
#41528=CARTESIAN_POINT('Ctrl Pts',(-20.0812289339452,21.3878266351598,-11.4961866143502));
#41529=CARTESIAN_POINT('Ctrl Pts',(-20.0097472733922,21.4320663370212,-11.5003563286706));
#41530=CARTESIAN_POINT('Ctrl Pts',(-19.9360570753464,21.4727982320515,-11.504526042991));
#41531=CARTESIAN_POINT('Ctrl Pts',(-19.8605396057917,21.5098058892787,-11.5086957573114));
#41532=CARTESIAN_POINT('Ctrl Pts',(-19.7850248234728,21.5468122296147,-11.5128653232554));
#41533=CARTESIAN_POINT('Ctrl Pts',(-19.7076833123971,21.5800943939658,-11.5170348891994));
#41534=CARTESIAN_POINT('Ctrl Pts',(-19.6289193227218,21.6094827299397,-11.5212044551435));
#41535=CARTESIAN_POINT('Ctrl Pts',(-19.5473860883354,21.639904323552,-11.5255206178824));
#41536=CARTESIAN_POINT('Ctrl Pts',(-19.464328979673,21.6661529958307,-11.5298367806213));
#41537=CARTESIAN_POINT('Ctrl Pts',(-19.3802151086564,21.6880962906888,-11.5341529433602));
#41538=CARTESIAN_POINT('Ctrl Pts',(-19.2988412381409,21.7093247850249,-11.5383285075519));
#41539=CARTESIAN_POINT('Ctrl Pts',(-19.2164788667994,21.7265240396989,-11.5425040717436));
#41540=CARTESIAN_POINT('Ctrl Pts',(-19.1335609462711,21.7396263168398,-11.5466796359353));
#41541=CARTESIAN_POINT('Ctrl Pts',(-19.0464550386955,21.7533903588514,-11.5510660979478));
#41542=CARTESIAN_POINT('Ctrl Pts',(-18.9587365661206,21.7626326086006,-11.5554525599603));
#41543=CARTESIAN_POINT('Ctrl Pts',(-18.8709107816373,21.7673363311332,-11.5598390219729));
#41544=CARTESIAN_POINT('Ctrl Pts',(-18.783084997154,21.7720400536657,-11.5642254839854));
#41545=CARTESIAN_POINT('Ctrl Pts',(-18.6951524811213,21.7722053239559,-11.568611945998));
#41546=CARTESIAN_POINT('Ctrl Pts',(-18.6076132463771,21.7678782506229,-11.5729984080105));
#41547=CARTESIAN_POINT('Ctrl Pts',(-18.5241126314324,21.76375080668,-11.5771825007382));
#41548=CARTESIAN_POINT('Ctrl Pts',(-18.440659044576,21.7555210317039,-11.5813665934658));
#41549=CARTESIAN_POINT('Ctrl Pts',(-18.3576882161332,21.7431906407936,-11.5855506861935));
#41550=CARTESIAN_POINT('Ctrl Pts',(-18.2748290034154,21.7308768372256,-11.5897291503099));
#41551=CARTESIAN_POINT('Ctrl Pts',(-18.1924517105385,21.7144734377133,-11.5939076144262));
#41552=CARTESIAN_POINT('Ctrl Pts',(-18.1109898384596,21.6940340993666,-11.5980860785426));
#41553=CARTESIAN_POINT('Ctrl Pts',(-18.0265307131236,21.6728427297706,-11.6024182822535));
#41554=CARTESIAN_POINT('Ctrl Pts',(-17.9430561814231,21.6473126765418,-11.6067504859644));
#41555=CARTESIAN_POINT('Ctrl Pts',(-17.8610409295545,21.6175623742855,-11.6110826896752));
#41556=CARTESIAN_POINT('Ctrl Pts',(-17.7820790900159,21.5889196701608,-11.6152536062606));
#41557=CARTESIAN_POINT('Ctrl Pts',(-17.7044702726561,21.5563655566265,-11.6194245228459));
#41558=CARTESIAN_POINT('Ctrl Pts',(-17.6286235702152,21.5200567226632,-11.6235954394312));
#41559=CARTESIAN_POINT('Ctrl Pts',(-17.5528073927267,21.4837625014041,-11.6277646774065));
#41560=CARTESIAN_POINT('Ctrl Pts',(-17.4787523341875,21.4437167634057,-11.6319339153819));
#41561=CARTESIAN_POINT('Ctrl Pts',(-17.4068461738869,21.4001237337879,-11.6361031533573));
#41562=CARTESIAN_POINT('Ctrl Pts',(-17.3349387846982,21.356529959158,-11.6402724625856));
#41563=CARTESIAN_POINT('Ctrl Pts',(-17.2651807609245,21.309389009247,-11.6444417718139));
#41564=CARTESIAN_POINT('Ctrl Pts',(-17.1979329485559,21.2589497097018,-11.6486110810422));
#41565=CARTESIAN_POINT('Ctrl Pts',(-17.1900756294251,21.2530563183884,-11.6490982283859));
#41566=CARTESIAN_POINT('Ctrl Pts',(-17.1822525452959,21.2471179459407,-11.6495853757296));
#41567=CARTESIAN_POINT('Ctrl Pts',(-17.1744642439897,21.2411350264762,-11.6500725230732));
#41568=CARTESIAN_POINT('Ctrl Pts',(-17.1757181329864,21.2395346319229,-10.8502164826864));
#41569=CARTESIAN_POINT('Ctrl Pts',(-16.7160809592132,20.8801557260842,-10.8791841133254));
#41570=CARTESIAN_POINT('Ctrl Pts',(-15.8690423976421,19.6129801926267,-10.9505436795248));
#41571=CARTESIAN_POINT('Ctrl Pts',(-16.5533150821545,17.1114988848558,-11.0642951812848));
#41572=CARTESIAN_POINT('Ctrl Pts',(-19.3189847985123,16.2409689515226,-11.1914709879662));
#41573=CARTESIAN_POINT('Ctrl Pts',(-21.0857646400936,17.7107520667789,-11.2922755723032));
#41574=CARTESIAN_POINT('Ctrl Pts',(-21.2926072565653,18.8863578111491,-11.3506882210795));
#41575=CARTESIAN_POINT('Ctrl Pts',(-21.2907952889915,19.209402892007,-11.3667089342955));
#41576=CARTESIAN_POINT('Origin',(-18.734,19.211,1.76670989022852));
#41577=CARTESIAN_POINT('',(-17.1744642439897,21.2411350264762,-10.0501312698105));
#41578=CARTESIAN_POINT('',(-17.1744642439897,21.2411350264762,-10.1166694888401));
#41579=CARTESIAN_POINT('',(-17.1744642439897,21.2411350264762,1.76670989022852));
#41580=CARTESIAN_POINT('',(-21.2939995125392,19.2125798097912,-10.6332901097715));
#41581=CARTESIAN_POINT('Ctrl Pts',(-17.1744642439897,21.2411350264762,-10.1166694888401));
#41582=CARTESIAN_POINT('Ctrl Pts',(-17.107774487029,21.1899044141359,-10.1208396489562));
#41583=CARTESIAN_POINT('Ctrl Pts',(-17.0436266170067,21.1353956546449,-10.1250098090722));
#41584=CARTESIAN_POINT('Ctrl Pts',(-16.9823480872221,21.0778999910176,-10.1291799691882));
#41585=CARTESIAN_POINT('Ctrl Pts',(-16.9210022641563,21.0203411882798,-10.1333547087835));
#41586=CARTESIAN_POINT('Ctrl Pts',(-16.8625324062092,20.9597892501365,-10.1375294483788));
#41587=CARTESIAN_POINT('Ctrl Pts',(-16.8072292781277,20.8965724800006,-10.1417041879741));
#41588=CARTESIAN_POINT('Ctrl Pts',(-16.7518918721062,20.8333165268977,-10.1458815151531));
#41589=CARTESIAN_POINT('Ctrl Pts',(-16.6997253880396,20.7673928147154,-10.1500588423321));
#41590=CARTESIAN_POINT('Ctrl Pts',(-16.6509789452328,20.6991610414859,-10.1542361695111));
#41591=CARTESIAN_POINT('Ctrl Pts',(-16.6021520613839,20.6308166726572,-10.1584203900864));
#41592=CARTESIAN_POINT('Ctrl Pts',(-16.5567567322681,20.5601570268823,-10.1626046106618));
#41593=CARTESIAN_POINT('Ctrl Pts',(-16.5149973626627,20.4875685627846,-10.1667888312371));
#41594=CARTESIAN_POINT('Ctrl Pts',(-16.4954988829386,20.4536752183978,-10.1687425470336));
#41595=CARTESIAN_POINT('Ctrl Pts',(-16.4767924376755,20.4193616721457,-10.1706962628301));
#41596=CARTESIAN_POINT('Ctrl Pts',(-16.4588952312818,20.3846687315233,-10.1726499786266));
#41597=CARTESIAN_POINT('Ctrl Pts',(-16.4205614748832,20.310360445341,-10.1768346130197));
#41598=CARTESIAN_POINT('Ctrl Pts',(-16.3858007370466,20.2340338438633,-10.1810192474127));
#41599=CARTESIAN_POINT('Ctrl Pts',(-16.3548302568732,20.1560668406995,-10.1852038818058));
#41600=CARTESIAN_POINT('Ctrl Pts',(-16.3239038593449,20.0782108139144,-10.1893825598897));
#41601=CARTESIAN_POINT('Ctrl Pts',(-16.2967571717625,19.9987194471875,-10.1935612379736));
#41602=CARTESIAN_POINT('Ctrl Pts',(-16.2735613224931,19.9179947059407,-10.1977399160576));
#41603=CARTESIAN_POINT('Ctrl Pts',(-16.2499497042962,19.8358230317228,-10.201993493943));
#41604=CARTESIAN_POINT('Ctrl Pts',(-16.2304321761497,19.7523737600805,-10.2062470718285));
#41605=CARTESIAN_POINT('Ctrl Pts',(-16.2151377103691,19.6680916383785,-10.2105006497139));
#41606=CARTESIAN_POINT('Ctrl Pts',(-16.2001397576524,19.5854434900687,-10.2146717636918));
#41607=CARTESIAN_POINT('Ctrl Pts',(-16.189202669843,19.5019949698567,-10.2188428776698));
#41608=CARTESIAN_POINT('Ctrl Pts',(-16.1823971528001,19.4181784500405,-10.2230139916478));
#41609=CARTESIAN_POINT('Ctrl Pts',(-16.1755939194142,19.3343900556671,-10.2271837059681));
#41610=CARTESIAN_POINT('Ctrl Pts',(-16.1729195406043,19.2502343650766,-10.2313534202885));
#41611=CARTESIAN_POINT('Ctrl Pts',(-16.1743929164357,19.1661493838669,-10.2355231346089));
#41612=CARTESIAN_POINT('Ctrl Pts',(-16.1758662398381,19.0820673947618,-10.2396927005529));
#41613=CARTESIAN_POINT('Ctrl Pts',(-16.1814870155133,18.9980565699821,-10.243862266497));
#41614=CARTESIAN_POINT('Ctrl Pts',(-16.1912220304803,18.9145540559813,-10.248031832441));
#41615=CARTESIAN_POINT('Ctrl Pts',(-16.2012993165641,18.8281156965995,-10.2523479951799));
#41616=CARTESIAN_POINT('Ctrl Pts',(-16.2157854771196,18.742222581345,-10.2566641579188));
#41617=CARTESIAN_POINT('Ctrl Pts',(-16.2345855425418,18.6573508603375,-10.2609803206578));
#41618=CARTESIAN_POINT('Ctrl Pts',(-16.2527731978103,18.575243826715,-10.2651558848494));
#41619=CARTESIAN_POINT('Ctrl Pts',(-16.2749978531258,18.4940931072454,-10.2693314490411));
#41620=CARTESIAN_POINT('Ctrl Pts',(-16.3011224991716,18.4143149518393,-10.2735070132328));
#41621=CARTESIAN_POINT('Ctrl Pts',(-16.3285666389837,18.3305073914581,-10.2778934752454));
#41622=CARTESIAN_POINT('Ctrl Pts',(-16.3603148903335,18.2482152402676,-10.2822799372579));
#41623=CARTESIAN_POINT('Ctrl Pts',(-16.396151895843,18.1678958623946,-10.2866663992705));
#41624=CARTESIAN_POINT('Ctrl Pts',(-16.4319889013525,18.0875764845217,-10.291052861283));
#41625=CARTESIAN_POINT('Ctrl Pts',(-16.4719143298048,18.0092303623903,-10.2954393232955));
#41626=CARTESIAN_POINT('Ctrl Pts',(-16.5156592733601,17.9332815566289,-10.2998257853081));
#41627=CARTESIAN_POINT('Ctrl Pts',(-16.5573914472168,17.8608272680038,-10.3040104197011));
#41628=CARTESIAN_POINT('Ctrl Pts',(-16.6027547120117,17.7902848467578,-10.3081950540942));
#41629=CARTESIAN_POINT('Ctrl Pts',(-16.6515488896105,17.7220415140652,-10.3123796884872));
#41630=CARTESIAN_POINT('Ctrl Pts',(-16.7002736147368,17.65389531731,-10.3165583665712));
#41631=CARTESIAN_POINT('Ctrl Pts',(-16.7524192872619,17.5880420799734,-10.3207370446551));
#41632=CARTESIAN_POINT('Ctrl Pts',(-16.8077405464177,17.5248432701896,-10.324915722739));
#41633=CARTESIAN_POINT('Ctrl Pts',(-16.8640533993853,17.4605116671605,-10.3291693006245));
#41634=CARTESIAN_POINT('Ctrl Pts',(-16.9236565628965,17.3989310067058,-10.3334228785099));
#41635=CARTESIAN_POINT('Ctrl Pts',(-16.9862458850684,17.3404504674456,-10.3376764563954));
#41636=CARTESIAN_POINT('Ctrl Pts',(-17.047621791097,17.2831036875543,-10.3418475703733));
#41637=CARTESIAN_POINT('Ctrl Pts',(-17.1118687523877,17.2287382262738,-10.3460186843513));
#41638=CARTESIAN_POINT('Ctrl Pts',(-17.1786614840028,17.1776475709667,-10.3501897983292));
#41639=CARTESIAN_POINT('Ctrl Pts',(-17.2454318026718,17.1265740596224,-10.3543595126496));
#41640=CARTESIAN_POINT('Ctrl Pts',(-17.3147458300055,17.0787734510952,-10.35852922697));
#41641=CARTESIAN_POINT('Ctrl Pts',(-17.3862455028589,17.0344987214716,-10.3626989412903));
#41642=CARTESIAN_POINT('Ctrl Pts',(-17.4577426314469,16.990225567333,-10.3668685072344));
#41643=CARTESIAN_POINT('Ctrl Pts',(-17.5314248593519,16.9494782841069,-10.3710380731784));
#41644=CARTESIAN_POINT('Ctrl Pts',(-17.6069066380297,16.9124655640164,-10.3752076391224));
#41645=CARTESIAN_POINT('Ctrl Pts',(-17.6850422629292,16.8741515223475,-10.3795238018614));
#41646=CARTESIAN_POINT('Ctrl Pts',(-17.7651058639349,16.8398397766947,-10.3838399646003));
#41647=CARTESIAN_POINT('Ctrl Pts',(-17.8466456689027,16.8097082036781,-10.3881561273392));
#41648=CARTESIAN_POINT('Ctrl Pts',(-17.9255293233002,16.7805581634832,-10.3923316915309));
#41649=CARTESIAN_POINT('Ctrl Pts',(-18.0057940203927,16.7553202361718,-10.3965072557226));
#41650=CARTESIAN_POINT('Ctrl Pts',(-18.087015599334,16.7341045267725,-10.4006828199142));
#41651=CARTESIAN_POINT('Ctrl Pts',(-18.1723394871415,16.711817262327,-10.4050692819268));
#41652=CARTESIAN_POINT('Ctrl Pts',(-18.2587188895798,16.6939693367971,-10.4094557439393));
#41653=CARTESIAN_POINT('Ctrl Pts',(-18.3456526669335,16.6806272312364,-10.4138422059519));
#41654=CARTESIAN_POINT('Ctrl Pts',(-18.4325864442873,16.6672851256758,-10.4182286679644));
#41655=CARTESIAN_POINT('Ctrl Pts',(-18.5200740116326,16.6584488227101,-10.422615129977));
#41656=CARTESIAN_POINT('Ctrl Pts',(-18.6076132463768,16.6541217493771,-10.4270015919895));
#41657=CARTESIAN_POINT('Ctrl Pts',(-18.6911246711663,16.6499937711024,-10.4311862263825));
#41658=CARTESIAN_POINT('Ctrl Pts',(-18.7749939587051,16.6499538232249,-10.4353708607756));
#41659=CARTESIAN_POINT('Ctrl Pts',(-18.8587871646375,16.6540431830902,-10.4395554951686));
#41660=CARTESIAN_POINT('Ctrl Pts',(-18.9424611013126,16.6581267222578,-10.4437341732526));
#41661=CARTESIAN_POINT('Ctrl Pts',(-19.0260587159288,16.6663278722549,-10.4479128513365));
#41662=CARTESIAN_POINT('Ctrl Pts',(-19.1091432618588,16.6786359793502,-10.4520915294204));
#41663=CARTESIAN_POINT('Ctrl Pts',(-19.1937170385631,16.6911647004194,-10.4563451073059));
#41664=CARTESIAN_POINT('Ctrl Pts',(-19.2777586905999,16.7079490849926,-10.4605986851913));
#41665=CARTESIAN_POINT('Ctrl Pts',(-19.360809982363,16.7289223932338,-10.4648522630768));
#41666=CARTESIAN_POINT('Ctrl Pts',(-19.4422511627741,16.7494890929688,-10.4690233770547));
#41667=CARTESIAN_POINT('Ctrl Pts',(-19.5227395737969,16.7740836270436,-10.4731944910327));
#41668=CARTESIAN_POINT('Ctrl Pts',(-19.6018523684377,16.8025913414462,-10.4773656050106));
#41669=CARTESIAN_POINT('Ctrl Pts',(-19.6809386160161,16.8310894898098,-10.481535319331));
#41670=CARTESIAN_POINT('Ctrl Pts',(-19.7586497315284,16.8634980548293,-10.4857050336514));
#41671=CARTESIAN_POINT('Ctrl Pts',(-19.8345791893309,16.8996528932219,-10.4898747479717));
#41672=CARTESIAN_POINT('Ctrl Pts',(-19.9105059452373,16.93580644507,-10.4940443139158));
#41673=CARTESIAN_POINT('Ctrl Pts',(-19.984650754504,16.9757058066958,-10.4982138798598));
#41674=CARTESIAN_POINT('Ctrl Pts',(-20.0566294498833,17.0191397539302,-10.5023834458038));
#41675=CARTESIAN_POINT('Ctrl Pts',(-20.131138827397,17.0641007851678,-10.5066996085427));
#41676=CARTESIAN_POINT('Ctrl Pts',(-20.2033264842377,17.1128493061259,-10.5110157712817));
#41677=CARTESIAN_POINT('Ctrl Pts',(-20.2727983186242,17.1651017291666,-10.5153319340206));
#41678=CARTESIAN_POINT('Ctrl Pts',(-20.3400071153126,17.2156520350226,-10.5195074982123));
#41679=CARTESIAN_POINT('Ctrl Pts',(-20.4046739763887,17.2694811317351,-10.5236830624039));
#41680=CARTESIAN_POINT('Ctrl Pts',(-20.4664767307265,17.326291964921,-10.5278586265956));
#41681=CARTESIAN_POINT('Ctrl Pts',(-20.5314009952638,17.3859721782363,-10.5322450886082));
#41682=CARTESIAN_POINT('Ctrl Pts',(-20.593163808364,17.4489428422735,-10.5366315506207));
#41683=CARTESIAN_POINT('Ctrl Pts',(-20.6514380125587,17.5148185627725,-10.5410180126333));
#41684=CARTESIAN_POINT('Ctrl Pts',(-20.7097122167533,17.5806942832716,-10.5454044746458));
#41685=CARTESIAN_POINT('Ctrl Pts',(-20.7644975100434,17.6494745589998,-10.5497909366583));
#41686=CARTESIAN_POINT('Ctrl Pts',(-20.8155192213964,17.7207390393097,-10.5541773986709));
#41687=CARTESIAN_POINT('Ctrl Pts',(-20.8646271615162,17.789330463214,-10.5583993290636));
#41688=CARTESIAN_POINT('Ctrl Pts',(-20.91043082465,17.8604769154309,-10.5626212594563));
#41689=CARTESIAN_POINT('Ctrl Pts',(-20.9526566798058,17.9338302629825,-10.5668431898491));
#41690=CARTESIAN_POINT('Ctrl Pts',(-20.9948201353165,18.0070752119515,-10.5710588812454));
#41691=CARTESIAN_POINT('Ctrl Pts',(-21.0334160638336,18.0825201920568,-10.5752745726417));
#41692=CARTESIAN_POINT('Ctrl Pts',(-21.0682129788551,18.1597865253222,-10.5794902640381));
#41693=CARTESIAN_POINT('Ctrl Pts',(-21.1029682787106,18.2369604523702,-10.583700913703));
#41694=CARTESIAN_POINT('Ctrl Pts',(-21.1339334100817,18.3159509969196,-10.587911563368));
#41695=CARTESIAN_POINT('Ctrl Pts',(-21.1609223976387,18.3963542635971,-10.592122213033));
#41696=CARTESIAN_POINT('Ctrl Pts',(-21.1878844462894,18.4766772762055,-10.5963286598616));
#41697=CARTESIAN_POINT('Ctrl Pts',(-21.2108781024617,18.5584097818782,-10.6005351066903));
#41698=CARTESIAN_POINT('Ctrl Pts',(-21.2297657078559,18.6411284956323,-10.6047415535189));
#41699=CARTESIAN_POINT('Ctrl Pts',(-21.24864245849,18.7237996707081,-10.6089455828907));
#41700=CARTESIAN_POINT('Ctrl Pts',(-21.2634177498248,18.8074554899473,-10.6131496122625));
#41701=CARTESIAN_POINT('Ctrl Pts',(-21.2740042132099,18.8916591211951,-10.6173536416343));
#41702=CARTESIAN_POINT('Ctrl Pts',(-21.2845883389273,18.975844158876,-10.6215567426862));
#41703=CARTESIAN_POINT('Ctrl Pts',(-21.2909854180498,19.0605763228041,-10.6257598437382));
#41704=CARTESIAN_POINT('Ctrl Pts',(-21.2931596531403,19.1454113596826,-10.6299629447901));
#41705=CARTESIAN_POINT('Ctrl Pts',(-21.2937333596144,19.1677964320698,-10.6310719997839));
#41706=CARTESIAN_POINT('Ctrl Pts',(-21.2940133304248,19.1901886456573,-10.6321810547777));
#41707=CARTESIAN_POINT('Ctrl Pts',(-21.2939995125392,19.2125798097912,-10.6332901097715));
#41708=CARTESIAN_POINT('Ctrl Pts',(-21.2907953051338,19.2125971079063,-10.6332910656997));
#41709=CARTESIAN_POINT('Ctrl Pts',(-21.292607272731,19.5356421908361,-10.6493117789173));
#41710=CARTESIAN_POINT('Ctrl Pts',(-21.0857646549701,20.7112479426697,-10.7077244276952));
#41711=CARTESIAN_POINT('Ctrl Pts',(-19.4306371445278,22.0881475490561,-10.8021586269852));
#41712=CARTESIAN_POINT('Ctrl Pts',(-17.7502563260471,21.6776341328961,-10.8805721130576));
#41713=CARTESIAN_POINT('Ctrl Pts',(-17.173194974388,21.2428171613069,-10.9165936635695));
#41714=CARTESIAN_POINT('',(-21.2940196853139,19.2096989556262,-10.5667098967305));
#41715=CARTESIAN_POINT('Ctrl Pts',(-21.2974135715529,19.2097193143547,-10.5667109992077));
#41716=CARTESIAN_POINT('Ctrl Pts',(-21.292595768045,19.9846331911651,-10.6053965865519));
#41717=CARTESIAN_POINT('Ctrl Pts',(-20.5048168766745,21.6171665132323,-10.6864741094567));
#41718=CARTESIAN_POINT('Ctrl Pts',(-18.3777720364044,21.9601260692161,-10.7809759372829));
#41719=CARTESIAN_POINT('Ctrl Pts',(-17.3887251838872,21.4060795618296,-10.8367921777649));
#41720=CARTESIAN_POINT('Ctrl Pts',(-17.1757181329864,21.2395346319229,-10.8502164826864));
#41721=CARTESIAN_POINT('Ctrl Pts',(-17.1744642439897,21.2411350264762,-10.0501312698105));
#41722=CARTESIAN_POINT('Ctrl Pts',(-17.1081216278261,21.1901710853072,-10.0543142329175));
#41723=CARTESIAN_POINT('Ctrl Pts',(-17.0441628085899,21.1358618379643,-10.0584971960246));
#41724=CARTESIAN_POINT('Ctrl Pts',(-16.9829440292627,21.0784589653712,-10.0626801591317));
#41725=CARTESIAN_POINT('Ctrl Pts',(-16.9218071503208,21.0211328881247,-10.0668575261407));
#41726=CARTESIAN_POINT('Ctrl Pts',(-16.8634033625468,20.9607217193491,-10.0710348931497));
#41727=CARTESIAN_POINT('Ctrl Pts',(-16.8080571271221,20.8975183219908,-10.0752122601588));
#41728=CARTESIAN_POINT('Ctrl Pts',(-16.7527685070128,20.834380719237,-10.0793852785375));
#41729=CARTESIAN_POINT('Ctrl Pts',(-16.7005314148742,20.7684570095275,-10.0835582969162));
#41730=CARTESIAN_POINT('Ctrl Pts',(-16.6516336173591,20.700076978684,-10.0877313152949));
#41731=CARTESIAN_POINT('Ctrl Pts',(-16.6027633898385,20.6317355024826,-10.091901980805));
#41732=CARTESIAN_POINT('Ctrl Pts',(-16.5572289858127,20.5609408282047,-10.0960726463151));
#41733=CARTESIAN_POINT('Ctrl Pts',(-16.5152772819117,20.4880550106548,-10.1002433118252));
#41734=CARTESIAN_POINT('Ctrl Pts',(-16.4733366469514,20.4151884239997,-10.1044128769068));
#41735=CARTESIAN_POINT('Ctrl Pts',(-16.4349770638098,20.3402321885223,-10.1085824419884));
#41736=CARTESIAN_POINT('Ctrl Pts',(-16.4004007975782,20.2635753001359,-10.11275200707));
#41737=CARTESIAN_POINT('Ctrl Pts',(-16.365823282296,20.1869156425573,-10.1169217227751));
#41738=CARTESIAN_POINT('Ctrl Pts',(-16.3350295432698,20.1085556299752,-10.1210914384802));
#41739=CARTESIAN_POINT('Ctrl Pts',(-16.3081742243601,20.0289054384468,-10.1252611541852));
#41740=CARTESIAN_POINT('Ctrl Pts',(-16.2812914480234,19.9491738109349,-10.1294351330929));
#41741=CARTESIAN_POINT('Ctrl Pts',(-16.2583552817622,19.8681498067063,-10.1336091120005));
#41742=CARTESIAN_POINT('Ctrl Pts',(-16.2394706988067,19.786259563578,-10.1377830909082));
#41743=CARTESIAN_POINT('Ctrl Pts',(-16.2205765762285,19.7043279532655,-10.141959178318));
#41744=CARTESIAN_POINT('Ctrl Pts',(-16.2057381946938,19.6215296857435,-10.1461352657278));
#41745=CARTESIAN_POINT('Ctrl Pts',(-16.1950090508136,19.5382994957977,-10.1503113531375));
#41746=CARTESIAN_POINT('Ctrl Pts',(-16.1842607922711,19.4549210258973,-10.1544948805166));
#41747=CARTESIAN_POINT('Ctrl Pts',(-16.1776364344997,19.3711095556487,-10.1586784078956));
#41748=CARTESIAN_POINT('Ctrl Pts',(-16.1751373971613,19.2873032095876,-10.1628619352746));
#41749=CARTESIAN_POINT('Ctrl Pts',(-16.1729067664636,19.2124980014741,-10.1665961350213));
#41750=CARTESIAN_POINT('Ctrl Pts',(-16.1739621448211,19.1376971079801,-10.170330334768));
#41751=CARTESIAN_POINT('Ctrl Pts',(-16.1782696504243,19.0632083214198,-10.1740645345148));
#41752=CARTESIAN_POINT('Ctrl Pts',(-16.1830967452018,18.9797343887762,-10.1782491689078));
#41753=CARTESIAN_POINT('Ctrl Pts',(-16.1920266966377,18.8963418534062,-10.1824338033009));
#41754=CARTESIAN_POINT('Ctrl Pts',(-16.205054135763,18.8134665853562,-10.1866184376939));
#41755=CARTESIAN_POINT('Ctrl Pts',(-16.2180630319411,18.7307092799923,-10.1907971157779));
#41756=CARTESIAN_POINT('Ctrl Pts',(-16.2351577602661,18.648468230058,-10.1949757938618));
#41757=CARTESIAN_POINT('Ctrl Pts',(-16.2562810188397,18.567176537863,-10.1991544719458));
#41758=CARTESIAN_POINT('Ctrl Pts',(-16.2777828966423,18.4844277505086,-10.2034080498312));
#41759=CARTESIAN_POINT('Ctrl Pts',(-16.3034591202047,18.4026631714652,-10.2076616277166));
#41760=CARTESIAN_POINT('Ctrl Pts',(-16.3331943249929,18.322331270465,-10.2119152056021));
#41761=CARTESIAN_POINT('Ctrl Pts',(-16.3623530548127,18.2435567601205,-10.21608631958));
#41762=CARTESIAN_POINT('Ctrl Pts',(-16.3954146207213,18.1661603243175,-10.220257433558));
#41763=CARTESIAN_POINT('Ctrl Pts',(-16.4322198035646,18.0905501228088,-10.2244285475359));
#41764=CARTESIAN_POINT('Ctrl Pts',(-16.4690126360733,18.0149652930334,-10.2285982618563));
#41765=CARTESIAN_POINT('Ctrl Pts',(-16.5095463894924,17.9411659204443,-10.2327679761767));
#41766=CARTESIAN_POINT('Ctrl Pts',(-16.5536143847776,17.8695386442647,-10.236937690497));
#41767=CARTESIAN_POINT('Ctrl Pts',(-16.5976808119345,17.7979139168909,-10.2411072564411));
#41768=CARTESIAN_POINT('Ctrl Pts',(-16.6452809891205,17.7284615236186,-10.2452768223851));
#41769=CARTESIAN_POINT('Ctrl Pts',(-16.6961638176235,17.6615408382932,-10.2494463883292));
#41770=CARTESIAN_POINT('Ctrl Pts',(-16.7488356236059,17.5922673042274,-10.2537625510681));
#41771=CARTESIAN_POINT('Ctrl Pts',(-16.8050248926421,17.5257072400677,-10.258078713807));
#41772=CARTESIAN_POINT('Ctrl Pts',(-16.8644075151044,17.462222158071,-10.2623948765459));
#41773=CARTESIAN_POINT('Ctrl Pts',(-16.9218557548859,17.4008050959429,-10.2665704407376));
#41774=CARTESIAN_POINT('Ctrl Pts',(-16.9822921248588,17.3422660512049,-10.2707460049293));
#41775=CARTESIAN_POINT('Ctrl Pts',(-17.0453868187423,17.2868935777658,-10.274921569121));
#41776=CARTESIAN_POINT('Ctrl Pts',(-17.1116682756205,17.2287243723289,-10.2793080311335));
#41777=CARTESIAN_POINT('Ctrl Pts',(-17.1808831995726,17.1740503939332,-10.283694493146));
#41778=CARTESIAN_POINT('Ctrl Pts',(-17.2526134178259,17.1231557064392,-10.2880809551586));
#41779=CARTESIAN_POINT('Ctrl Pts',(-17.3243436360791,17.0722610189452,-10.2924674171711));
#41780=CARTESIAN_POINT('Ctrl Pts',(-17.3985886179775,17.0251458690142,-10.2968538791837));
#41781=CARTESIAN_POINT('Ctrl Pts',(-17.4749010481802,16.9820383965787,-10.3012403411962));
#41782=CARTESIAN_POINT('Ctrl Pts',(-17.5477022303472,16.9409143628506,-10.3054249755892));
#41783=CARTESIAN_POINT('Ctrl Pts',(-17.6226557687809,16.9032842410815,-10.3096096099823));
#41784=CARTESIAN_POINT('Ctrl Pts',(-17.6993922596291,16.8693794450073,-10.3137942443753));
#41785=CARTESIAN_POINT('Ctrl Pts',(-17.7760195255806,16.8355229082136,-10.3179729224593));
#41786=CARTESIAN_POINT('Ctrl Pts',(-17.8544242858621,16.8053813489309,-10.3221516005432));
#41787=CARTESIAN_POINT('Ctrl Pts',(-17.9342113535406,16.779141015397,-10.3263302786272));
#41788=CARTESIAN_POINT('Ctrl Pts',(-18.0154285470652,16.752430342743,-10.3305838565126));
#41789=CARTESIAN_POINT('Ctrl Pts',(-18.0980776713418,16.7297623675601,-10.334837434398));
#41790=CARTESIAN_POINT('Ctrl Pts',(-18.1817191896631,16.7112828346924,-10.3390910122835));
#41791=CARTESIAN_POINT('Ctrl Pts',(-18.2637391539388,16.6931615636291,-10.3432621262614));
#41792=CARTESIAN_POINT('Ctrl Pts',(-18.3467129067616,16.6790678856914,-10.3474332402394));
#41793=CARTESIAN_POINT('Ctrl Pts',(-18.4302110680642,16.6690888519004,-10.3516043542173));
#41794=CARTESIAN_POINT('Ctrl Pts',(-18.5136812107523,16.6591131666705,-10.3557740685377));
#41795=CARTESIAN_POINT('Ctrl Pts',(-18.5976749560381,16.6532494380237,-10.3599437828581));
#41796=CARTESIAN_POINT('Ctrl Pts',(-18.6817553300752,16.6515331620698,-10.3641134971784));
#41797=CARTESIAN_POINT('Ctrl Pts',(-18.7658327121718,16.6498169471884,-10.3682830631225));
#41798=CARTESIAN_POINT('Ctrl Pts',(-18.8499962569362,16.652247900101,-10.3724526290665));
#41799=CARTESIAN_POINT('Ctrl Pts',(-18.9338078728663,16.6588094087744,-10.3766221950106));
#41800=CARTESIAN_POINT('Ctrl Pts',(-19.0205662018197,16.6656016119982,-10.3809383577495));
#41801=CARTESIAN_POINT('Ctrl Pts',(-19.1069468680349,16.6768201947949,-10.3852545204884));
#41802=CARTESIAN_POINT('Ctrl Pts',(-19.1924704625205,16.6923883119869,-10.3895706832273));
#41803=CARTESIAN_POINT('Ctrl Pts',(-19.2752081349112,16.7074492993989,-10.393746247419));
#41804=CARTESIAN_POINT('Ctrl Pts',(-19.357143268331,16.7265806476473,-10.3979218116107));
#41805=CARTESIAN_POINT('Ctrl Pts',(-19.437854716723,16.749661230601,-10.4020973758024));
#41806=CARTESIAN_POINT('Ctrl Pts',(-19.5226427085001,16.7739075589308,-10.4064838378149));
#41807=CARTESIAN_POINT('Ctrl Pts',(-19.6060795975567,16.8025123689437,-10.4108702998274));
#41808=CARTESIAN_POINT('Ctrl Pts',(-19.6877001821495,16.8352778018952,-10.41525676184));
#41809=CARTESIAN_POINT('Ctrl Pts',(-19.7693207667423,16.8680432348467,-10.4196432238525));
#41810=CARTESIAN_POINT('Ctrl Pts',(-19.8491245522344,16.9049689780518,-10.4240296858651));
#41811=CARTESIAN_POINT('Ctrl Pts',(-19.9266775857362,16.945802397917,-10.4284161478776));
#41812=CARTESIAN_POINT('Ctrl Pts',(-20.0006622892055,16.9847570116046,-10.4326007822707));
#41813=CARTESIAN_POINT('Ctrl Pts',(-20.0728741952653,17.0274126045708,-10.4367854166637));
#41814=CARTESIAN_POINT('Ctrl Pts',(-20.1429187702869,17.0735838265015,-10.4409700510568));
#41815=CARTESIAN_POINT('Ctrl Pts',(-20.2128636455258,17.1196893294125,-10.4451487291407));
#41816=CARTESIAN_POINT('Ctrl Pts',(-20.2806469365539,17.1693002706272,-10.4493274072247));
#41817=CARTESIAN_POINT('Ctrl Pts',(-20.3458981308861,17.2221851731129,-10.4535060853086));
#41818=CARTESIAN_POINT('Ctrl Pts',(-20.4123189059815,17.276017999468,-10.457759663194));
#41819=CARTESIAN_POINT('Ctrl Pts',(-20.4761154892317,17.3332430884428,-10.4620132410795));
#41820=CARTESIAN_POINT('Ctrl Pts',(-20.5369274194045,17.3935697481445,-10.4662668189649));
#41821=CARTESIAN_POINT('Ctrl Pts',(-20.5965603916461,17.4527268578301,-10.4704379329429));
#41822=CARTESIAN_POINT('Ctrl Pts',(-20.6533230631002,17.5148660125131,-10.4746090469208));
#41823=CARTESIAN_POINT('Ctrl Pts',(-20.7069098223473,17.5796732905743,-10.4787801608988));
#41824=CARTESIAN_POINT('Ctrl Pts',(-20.7604786000398,17.6444588219275,-10.4829498752191));
#41825=CARTESIAN_POINT('Ctrl Pts',(-20.8108732891324,17.7119103443124,-10.4871195895395));
#41826=CARTESIAN_POINT('Ctrl Pts',(-20.857827517359,17.7816796452479,-10.4912893038599));
#41827=CARTESIAN_POINT('Ctrl Pts',(-20.9047800747525,17.8514464634921,-10.4954588698039));
#41828=CARTESIAN_POINT('Ctrl Pts',(-20.9482921585527,17.9235305141741,-10.499628435748));
#41829=CARTESIAN_POINT('Ctrl Pts',(-20.9881406062296,17.9975544398916,-10.503798001692));
#41830=CARTESIAN_POINT('Ctrl Pts',(-21.0293900761685,18.074180955519,-10.5081141644309));
#41831=CARTESIAN_POINT('Ctrl Pts',(-21.0667132396991,18.1528858318598,-10.5124303271698));
#41832=CARTESIAN_POINT('Ctrl Pts',(-21.0999152164604,18.2332243669833,-10.5167464899088));
#41833=CARTESIAN_POINT('Ctrl Pts',(-21.1320356423208,18.3109458827751,-10.5209220541004));
#41834=CARTESIAN_POINT('Ctrl Pts',(-21.1602991397429,18.3901957994174,-10.5250976182921));
#41835=CARTESIAN_POINT('Ctrl Pts',(-21.1845795982611,18.4705544364463,-10.5292731824838));
#41836=CARTESIAN_POINT('Ctrl Pts',(-21.2100864050179,18.5549717971972,-10.5336596444963));
#41837=CARTESIAN_POINT('Ctrl Pts',(-21.2311970921469,18.6406122578467,-10.5380461065089));
#41838=CARTESIAN_POINT('Ctrl Pts',(-21.2478262226602,18.7269775601629,-10.5424325685214));
#41839=CARTESIAN_POINT('Ctrl Pts',(-21.2644553531735,18.813342862479,-10.5468190305339));
#41840=CARTESIAN_POINT('Ctrl Pts',(-21.2766029222518,18.9004324212998,-10.5512054925465));
#41841=CARTESIAN_POINT('Ctrl Pts',(-21.2842464642989,18.9877446051473,-10.555591954559));
#41842=CARTESIAN_POINT('Ctrl Pts',(-21.2907042434478,19.0615118189368,-10.5592979331155));
#41843=CARTESIAN_POINT('Ctrl Pts',(-21.293961988618,19.1355632322755,-10.563003911672));
#41844=CARTESIAN_POINT('Ctrl Pts',(-21.2939996693303,19.2096988355573,-10.5667098902285));
#41845=CARTESIAN_POINT('Origin',(-18.734,19.211,1.76670989022852));
#41846=CARTESIAN_POINT('',(-17.1744642439897,21.2411350264762,-9.25004023969327));
#41847=CARTESIAN_POINT('',(-17.1750494706851,21.2403917593384,-9.31680760799386));
#41848=CARTESIAN_POINT('',(-17.1744642439897,21.2411350264762,1.76670989022852));
#41849=CARTESIAN_POINT('',(-21.2939992159918,19.2089964727374,-9.8332901097715));
#41850=CARTESIAN_POINT('Ctrl Pts',(-17.1750494706848,21.2403917593382,-9.31680760799388));
#41851=CARTESIAN_POINT('Ctrl Pts',(-16.6852502113565,20.8565255580946,-9.34773678484192));
#41852=CARTESIAN_POINT('Ctrl Pts',(-15.8397229750276,19.5224826623952,-9.42105789725044));
#41853=CARTESIAN_POINT('Ctrl Pts',(-16.6528318707067,17.0128118877737,-9.53677094521943));
#41854=CARTESIAN_POINT('Ctrl Pts',(-19.4558314956606,16.2712294220481,-9.66394675190088));
#41855=CARTESIAN_POINT('Ctrl Pts',(-21.1196060595483,17.7909993809188,-9.76278617061903));
#41856=CARTESIAN_POINT('Ctrl Pts',(-21.2937097337482,18.9257985538188,-9.81923365377672));
#41857=CARTESIAN_POINT('Ctrl Pts',(-21.2916489871171,19.2089800104295,-9.83328920137392));
#41858=CARTESIAN_POINT('Ctrl Pts',(-21.2939992159918,19.2089964727374,-9.8332901097715));
#41859=CARTESIAN_POINT('Ctrl Pts',(-21.2940649620946,19.2930033015151,-9.83745593779552));
#41860=CARTESIAN_POINT('Ctrl Pts',(-21.2899913508454,19.3770604200798,-9.84162176581953));
#41861=CARTESIAN_POINT('Ctrl Pts',(-21.281790209728,19.4607299485725,-9.84578759384355));
#41862=CARTESIAN_POINT('Ctrl Pts',(-21.2735905258927,19.544384609609,-9.84995268163075));
#41863=CARTESIAN_POINT('Ctrl Pts',(-21.2612648140692,19.6276513592372,-9.85411776941795));
#41864=CARTESIAN_POINT('Ctrl Pts',(-21.2448768408732,19.7100966739687,-9.85828285720515));
#41865=CARTESIAN_POINT('Ctrl Pts',(-21.2284868533627,19.7925521223993,-9.86244845694073));
#41866=CARTESIAN_POINT('Ctrl Pts',(-21.2080337038204,19.8741854840197,-9.86661405667632));
#41867=CARTESIAN_POINT('Ctrl Pts',(-21.183632148948,19.9545740278144,-9.8707796564119));
#41868=CARTESIAN_POINT('Ctrl Pts',(-21.159203008195,20.0350534506039,-9.87494996534483));
#41869=CARTESIAN_POINT('Ctrl Pts',(-21.1308166833999,20.114284804087,-9.87912027427776));
#41870=CARTESIAN_POINT('Ctrl Pts',(-21.0986375209739,20.1918615572049,-9.88329058321069));
#41871=CARTESIAN_POINT('Ctrl Pts',(-21.066439637101,20.2694834435379,-9.88746331837884));
#41872=CARTESIAN_POINT('Ctrl Pts',(-21.0304447198545,20.3454483968716,-9.89163605354698));
#41873=CARTESIAN_POINT('Ctrl Pts',(-20.9908638255709,20.4193731513193,-9.89580878871513));
#41874=CARTESIAN_POINT('Ctrl Pts',(-20.9512104382913,20.4934333000532,-9.89998916630974));
#41875=CARTESIAN_POINT('Ctrl Pts',(-20.907958193034,20.5654453913561,-9.90416954390436));
#41876=CARTESIAN_POINT('Ctrl Pts',(-20.8613622504221,20.6350540212643,-9.90834992149897));
#41877=CARTESIAN_POINT('Ctrl Pts',(-20.8243993123263,20.6902721225411,-9.91166606942056));
#41878=CARTESIAN_POINT('Ctrl Pts',(-20.7853331875374,20.7439783287845,-9.91498221734216));
#41879=CARTESIAN_POINT('Ctrl Pts',(-20.7443085775785,20.7960108589263,-9.91829836526375));
#41880=CARTESIAN_POINT('Ctrl Pts',(-20.6925397790042,20.8616705099241,-9.9224829996568));
#41881=CARTESIAN_POINT('Ctrl Pts',(-20.6374544461771,20.9249134154189,-9.92666763404984));
#41882=CARTESIAN_POINT('Ctrl Pts',(-20.5793066365797,20.9853853631595,-9.93085226844289));
#41883=CARTESIAN_POINT('Ctrl Pts',(-20.5212415931921,21.0457712365674,-9.93503094652683));
#41884=CARTESIAN_POINT('Ctrl Pts',(-20.4601230476226,21.1033936577093,-9.93920962461076));
#41885=CARTESIAN_POINT('Ctrl Pts',(-20.3962460420505,21.1579304290825,-9.9433883026947));
#41886=CARTESIAN_POINT('Ctrl Pts',(-20.3312240870609,21.2134447328878,-9.94764188058014));
#41887=CARTESIAN_POINT('Ctrl Pts',(-20.2633441071063,21.2657612997089,-9.95189545846558));
#41888=CARTESIAN_POINT('Ctrl Pts',(-20.1929575410587,21.3145785921586,-9.95614903635102));
#41889=CARTESIAN_POINT('Ctrl Pts',(-20.1239355559419,21.3624494661351,-9.96032015032897));
#41890=CARTESIAN_POINT('Ctrl Pts',(-20.0525037029722,21.4069552612257,-9.96449126430692));
#41891=CARTESIAN_POINT('Ctrl Pts',(-19.979026280494,21.4478526015094,-9.96866237828488));
#41892=CARTESIAN_POINT('Ctrl Pts',(-19.9055735140746,21.4887362182955,-9.97283209260525));
#41893=CARTESIAN_POINT('Ctrl Pts',(-19.8300769429976,21.5260135615003,-9.97700180692563));
#41894=CARTESIAN_POINT('Ctrl Pts',(-19.7529274425308,21.5594860797666,-9.981171521246));
#41895=CARTESIAN_POINT('Ctrl Pts',(-19.6757806873742,21.5929574069372,-9.98534108719005));
#41896=CARTESIAN_POINT('Ctrl Pts',(-19.5969815421365,21.6226239960434,-9.98951065313409));
#41897=CARTESIAN_POINT('Ctrl Pts',(-19.5169416763859,21.6483350880373,-9.99368021907814));
#41898=CARTESIAN_POINT('Ctrl Pts',(-19.4340877076953,21.6749501503077,-9.99799638181706));
#41899=CARTESIAN_POINT('Ctrl Pts',(-19.3499046498555,21.6973262283484,-10.002312544556));
#41900=CARTESIAN_POINT('Ctrl Pts',(-19.264865245119,21.7153526292287,-10.0066287072949));
#41901=CARTESIAN_POINT('Ctrl Pts',(-19.1825959900473,21.7327918219964,-10.0108042714866));
#41902=CARTESIAN_POINT('Ctrl Pts',(-19.0995257948678,21.7461603390116,-10.0149798356783));
#41903=CARTESIAN_POINT('Ctrl Pts',(-19.0160902825554,21.7554105550182,-10.0191553998699));
#41904=CARTESIAN_POINT('Ctrl Pts',(-18.9284406408651,21.7651279774449,-10.0235418618825));
#41905=CARTESIAN_POINT('Ctrl Pts',(-18.840388390719,21.7703001003684,-10.027928323895));
#41906=CARTESIAN_POINT('Ctrl Pts',(-18.7524390182804,21.7709335933975,-10.0323147859076));
#41907=CARTESIAN_POINT('Ctrl Pts',(-18.6644896458417,21.7715670864265,-10.0367012479201));
#41908=CARTESIAN_POINT('Ctrl Pts',(-18.576643727377,21.767662051318,-10.0410877099326));
#41909=CARTESIAN_POINT('Ctrl Pts',(-18.4893986055751,21.759287691342,-10.0454741719452));
#41910=CARTESIAN_POINT('Ctrl Pts',(-18.4061740830914,21.7512992549033,-10.0496584884874));
#41911=CARTESIAN_POINT('Ctrl Pts',(-18.3231864480374,21.7392146225049,-10.0538428050297));
#41912=CARTESIAN_POINT('Ctrl Pts',(-18.2408709541661,21.7230556809424,-10.058027121572));
#41913=CARTESIAN_POINT('Ctrl Pts',(-18.1586671961938,21.7069186736935,-10.0622057582799));
#41914=CARTESIAN_POINT('Ctrl Pts',(-18.0771342151523,21.6867184269545,-10.0663843949878));
#41915=CARTESIAN_POINT('Ctrl Pts',(-17.9967026166128,21.6625286187296,-10.0705630316957));
#41916=CARTESIAN_POINT('Ctrl Pts',(-17.9163646373026,21.6383669664937,-10.0747368046342));
#41917=CARTESIAN_POINT('Ctrl Pts',(-17.8371259304894,21.6102251148538,-10.0789105775727));
#41918=CARTESIAN_POINT('Ctrl Pts',(-17.75940588948,21.578227559771,-10.0830843505111));
#41919=CARTESIAN_POINT('Ctrl Pts',(-17.6817391959917,21.5462519680098,-10.0872552585458));
#41920=CARTESIAN_POINT('Ctrl Pts',(-17.6055895218583,21.5104261042808,-10.0914261665805));
#41921=CARTESIAN_POINT('Ctrl Pts',(-17.531359015293,21.4709235964746,-10.0955970746152));
#41922=CARTESIAN_POINT('Ctrl Pts',(-17.4571459112369,21.4314303495882,-10.0997670048274));
#41923=CARTESIAN_POINT('Ctrl Pts',(-17.3848514901506,21.3882623802804,-10.1039369350395));
#41924=CARTESIAN_POINT('Ctrl Pts',(-17.3148548334226,21.341640043785,-10.1081068652516));
#41925=CARTESIAN_POINT('Ctrl Pts',(-17.266943957738,21.3097282772467,-10.1109610731144));
#41926=CARTESIAN_POINT('Ctrl Pts',(-17.2201091169427,21.276199103752,-10.1138152809773));
#41927=CARTESIAN_POINT('Ctrl Pts',(-17.1744642439897,21.2411350264762,-10.1166694888401));
#41928=CARTESIAN_POINT('',(-21.2939989766127,19.2132890482675,-9.7667098901893));
#41929=CARTESIAN_POINT('Ctrl Pts',(-21.293998976612,19.2132890490549,-9.76670989022852));
#41930=CARTESIAN_POINT('Ctrl Pts',(-21.2938920610985,19.3328599270272,-9.77266511192853));
#41931=CARTESIAN_POINT('Ctrl Pts',(-21.2854044483393,19.4520702292311,-9.77862033362855));
#41932=CARTESIAN_POINT('Ctrl Pts',(-21.2687069780215,19.5699714968758,-9.78457555532857));
#41933=CARTESIAN_POINT('Ctrl Pts',(-21.2612660069347,19.6225123852221,-9.78722940837586));
#41934=CARTESIAN_POINT('Ctrl Pts',(-21.2521952261605,19.6747937484515,-9.78988326142315));
#41935=CARTESIAN_POINT('Ctrl Pts',(-21.2415125421986,19.7267333135613,-9.79253711447044));
#41936=CARTESIAN_POINT('Ctrl Pts',(-21.2246679295087,19.8086323813113,-9.79672174886349));
#41937=CARTESIAN_POINT('Ctrl Pts',(-21.2037753333228,19.8898577370366,-9.80090638325654));
#41938=CARTESIAN_POINT('Ctrl Pts',(-21.1789030820534,19.9699788662181,-9.80509101764959));
#41939=CARTESIAN_POINT('Ctrl Pts',(-21.154066233355,20.0499859528893,-9.80926969573354));
#41940=CARTESIAN_POINT('Ctrl Pts',(-21.125261116367,20.1288914993745,-9.81344837381749));
#41941=CARTESIAN_POINT('Ctrl Pts',(-21.0926070466711,20.2062752380087,-9.81762705190143));
#41942=CARTESIAN_POINT('Ctrl Pts',(-21.0593676762441,20.2850460245431,-9.82188062978687));
#41943=CARTESIAN_POINT('Ctrl Pts',(-21.022140108072,20.362239437543,-9.8261342076723));
#41944=CARTESIAN_POINT('Ctrl Pts',(-20.9811033321017,20.4374283977703,-9.83038778555774));
#41945=CARTESIAN_POINT('Ctrl Pts',(-20.9408621341102,20.5111596732845,-9.83455889953569));
#41946=CARTESIAN_POINT('Ctrl Pts',(-20.8969583386824,20.5829631005171,-9.83873001351364));
#41947=CARTESIAN_POINT('Ctrl Pts',(-20.8496085018329,20.6524578269836,-9.84290112749159));
#41948=CARTESIAN_POINT('Ctrl Pts',(-20.8022745536785,20.7219292338234,-9.84707084181197));
#41949=CARTESIAN_POINT('Ctrl Pts',(-20.7514971194517,20.7890930986179,-9.85124055613234));
#41950=CARTESIAN_POINT('Ctrl Pts',(-20.6975366051101,20.853596724821,-9.85541027045272));
#41951=CARTESIAN_POINT('Ctrl Pts',(-20.643578010915,20.9180980557084,-9.85957983639676));
#41952=CARTESIAN_POINT('Ctrl Pts',(-20.5864368576391,20.9799389839169,-9.86374940234081));
#41953=CARTESIAN_POINT('Ctrl Pts',(-20.5264135623405,21.0388002137919,-9.86791896828486));
#41954=CARTESIAN_POINT('Ctrl Pts',(-20.4642799220261,21.099730931896,-9.87223513102378));
#41955=CARTESIAN_POINT('Ctrl Pts',(-20.3990580731255,21.1574681514492,-9.87655129376269));
#41956=CARTESIAN_POINT('Ctrl Pts',(-20.3311209857105,21.2117010163947,-9.88086745650161));
#41957=CARTESIAN_POINT('Ctrl Pts',(-20.2653969417723,21.264167251469,-9.88504302069329));
#41958=CARTESIAN_POINT('Ctrl Pts',(-20.1971322502975,21.3133536974901,-9.88921858488498));
#41959=CARTESIAN_POINT('Ctrl Pts',(-20.1266949702183,21.3590225138319,-9.89339414907666));
#41960=CARTESIAN_POINT('Ctrl Pts',(-20.0527000705711,21.4069979535197,-9.89778061108919));
#41961=CARTESIAN_POINT('Ctrl Pts',(-19.9763078452047,21.4510907819034,-9.90216707310173));
#41962=CARTESIAN_POINT('Ctrl Pts',(-19.8979731420051,21.4910803768049,-9.90655353511427));
#41963=CARTESIAN_POINT('Ctrl Pts',(-19.8196384388055,21.5310699717064,-9.91093999712681));
#41964=CARTESIAN_POINT('Ctrl Pts',(-19.7393618185147,21.5669561657756,-9.91532645913934));
#41965=CARTESIAN_POINT('Ctrl Pts',(-19.6576188802167,21.5985778865007,-9.91971292115187));
#41966=CARTESIAN_POINT('Ctrl Pts',(-19.5796370556819,21.6287446449807,-9.92389755554492));
#41967=CARTESIAN_POINT('Ctrl Pts',(-19.5000306196521,21.6551430224068,-9.92808218993797));
#41968=CARTESIAN_POINT('Ctrl Pts',(-19.4191985515815,21.6775974428168,-9.93226682433101));
#41969=CARTESIAN_POINT('Ctrl Pts',(-19.3384815379547,21.7000199021387,-9.93644550241496));
#41970=CARTESIAN_POINT('Ctrl Pts',(-19.2565427969408,21.7185094330108,-9.9406241804989));
#41971=CARTESIAN_POINT('Ctrl Pts',(-19.1738002903986,21.7329388780391,-9.94480285858285));
#41972=CARTESIAN_POINT('Ctrl Pts',(-19.0895746838927,21.7476269604994,-9.94905643646829));
#41973=CARTESIAN_POINT('Ctrl Pts',(-19.0045166631074,21.758107797425,-9.95331001435372));
#41974=CARTESIAN_POINT('Ctrl Pts',(-18.9190822179584,21.7643007211442,-9.95756359223916));
#41975=CARTESIAN_POINT('Ctrl Pts',(-18.8353040862403,21.7703735829526,-9.96173470621711));
#41976=CARTESIAN_POINT('Ctrl Pts',(-18.7511644753126,21.7723232722254,-9.96590582019506));
#41977=CARTESIAN_POINT('Ctrl Pts',(-18.6671008395073,21.7701257300737,-9.97007693417301));
#41978=CARTESIAN_POINT('Ctrl Pts',(-18.5830654120668,21.7679289253285,-9.97424664849338));
#41979=CARTESIAN_POINT('Ctrl Pts',(-18.49910636861,21.7615876649968,-9.97841636281376));
#41980=CARTESIAN_POINT('Ctrl Pts',(-18.4156612239222,21.7511300013277,-9.98258607713413));
#41981=CARTESIAN_POINT('Ctrl Pts',(-18.3322190485709,21.7406727097873,-9.98675564307817));
#41982=CARTESIAN_POINT('Ctrl Pts',(-18.2492911919861,21.7260993641991,-9.99092520902222));
#41983=CARTESIAN_POINT('Ctrl Pts',(-18.1673087413396,21.7074897390852,-9.99509477496626));
#41984=CARTESIAN_POINT('Ctrl Pts',(-18.0824438888646,21.6882258225098,-9.99941093770518));
#41985=CARTESIAN_POINT('Ctrl Pts',(-17.9985926745537,21.664636631037,-10.0037271004441));
#41986=CARTESIAN_POINT('Ctrl Pts',(-17.9162183607825,21.6368675129855,-10.008043263183));
#41987=CARTESIAN_POINT('Ctrl Pts',(-17.8365273816181,21.6100029710338,-10.0122188273747));
#41988=CARTESIAN_POINT('Ctrl Pts',(-17.7582189816852,21.5792268589617,-10.0163943915664));
#41989=CARTESIAN_POINT('Ctrl Pts',(-17.6816923706305,21.5447199174645,-10.0205699557581));
#41990=CARTESIAN_POINT('Ctrl Pts',(-17.6013005823761,21.5084701123848,-10.0249564177706));
#41991=CARTESIAN_POINT('Ctrl Pts',(-17.522875828849,21.4681029519009,-10.0293428797831));
#41992=CARTESIAN_POINT('Ctrl Pts',(-17.4468498189206,21.423881472503,-10.0337293417957));
#41993=CARTESIAN_POINT('Ctrl Pts',(-17.3708238089921,21.3796599931052,-10.0381158038082));
#41994=CARTESIAN_POINT('Ctrl Pts',(-17.2971969868963,21.3315845757053,-10.0425022658208));
#41995=CARTESIAN_POINT('Ctrl Pts',(-17.2263622218889,21.2799679383722,-10.0468887278333));
#41996=CARTESIAN_POINT('Ctrl Pts',(-17.2089081629896,21.2672493272763,-10.047969575159));
#41997=CARTESIAN_POINT('Ctrl Pts',(-17.19160669479,21.2543037392071,-10.0490504224848));
#41998=CARTESIAN_POINT('Ctrl Pts',(-17.1744642439897,21.2411350264762,-10.0501312698105));
#41999=CARTESIAN_POINT('Ctrl Pts',(-17.1744642439897,21.2411350264762,-9.25004023969326));
#42000=CARTESIAN_POINT('Ctrl Pts',(-17.1077984582143,21.1899228286354,-9.25421687978312));
#42001=CARTESIAN_POINT('Ctrl Pts',(-17.0437157308937,21.1354678945878,-9.25839351987297));
#42002=CARTESIAN_POINT('Ctrl Pts',(-16.9825323856757,21.0780728951953,-9.26257015996283));
#42003=CARTESIAN_POINT('Ctrl Pts',(-16.9212438722431,21.020579239386,-9.26675397929042));
#42004=CARTESIAN_POINT('Ctrl Pts',(-16.8628650136832,20.9601357565965,-9.27093779861802));
#42005=CARTESIAN_POINT('Ctrl Pts',(-16.8076738254214,20.8970805049384,-9.27512161794562));
#42006=CARTESIAN_POINT('Ctrl Pts',(-16.7693642901206,20.8533123335079,-9.27802570787865));
#42007=CARTESIAN_POINT('Ctrl Pts',(-16.7325897638593,20.8082865027903,-9.28092979781168));
#42008=CARTESIAN_POINT('Ctrl Pts',(-16.6974308899393,20.7621241923026,-9.28383388774471));
#42009=CARTESIAN_POINT('Ctrl Pts',(-16.6467688800087,20.6956068334797,-9.28801852213775));
#42010=CARTESIAN_POINT('Ctrl Pts',(-16.5992748500802,20.6264810343216,-9.2922031565308));
#42011=CARTESIAN_POINT('Ctrl Pts',(-16.5552283987658,20.5550812139358,-9.29638779092385));
#42012=CARTESIAN_POINT('Ctrl Pts',(-16.5112446421229,20.4837830223567,-9.30056646900779));
#42013=CARTESIAN_POINT('Ctrl Pts',(-16.470698956314,20.4102176270062,-9.30474514709174));
#42014=CARTESIAN_POINT('Ctrl Pts',(-16.4338297096936,20.3347511448678,-9.30892382517568));
#42015=CARTESIAN_POINT('Ctrl Pts',(-16.396299608325,20.2579319802739,-9.31317740306111));
#42016=CARTESIAN_POINT('Ctrl Pts',(-16.3625793350039,20.1791432881301,-9.31743098094655));
#42017=CARTESIAN_POINT('Ctrl Pts',(-16.3328731767862,20.0988006413847,-9.32168455883199));
#42018=CARTESIAN_POINT('Ctrl Pts',(-16.3037429304124,20.0200155936223,-9.32585567280994));
#42019=CARTESIAN_POINT('Ctrl Pts',(-16.2784727120492,19.9397367578111,-9.33002678678789));
#42020=CARTESIAN_POINT('Ctrl Pts',(-16.2572072783656,19.8583776440834,-9.33419790076584));
#42021=CARTESIAN_POINT('Ctrl Pts',(-16.2359489805037,19.777045831192,-9.33836761508621));
#42022=CARTESIAN_POINT('Ctrl Pts',(-16.2186929146628,19.6946349050203,-9.34253732940659));
#42023=CARTESIAN_POINT('Ctrl Pts',(-16.2055337985359,19.6115729247638,-9.34670704372696));
#42024=CARTESIAN_POINT('Ctrl Pts',(-16.1923751506669,19.528513900209,-9.350876609671));
#42025=CARTESIAN_POINT('Ctrl Pts',(-16.1833132337911,19.4448043221316,-9.35504617561504));
#42026=CARTESIAN_POINT('Ctrl Pts',(-16.1783912959603,19.3608804584879,-9.35921574155909));
#42027=CARTESIAN_POINT('Ctrl Pts',(-16.1732963088673,19.2740059353298,-9.36353190429801));
#42028=CARTESIAN_POINT('Ctrl Pts',(-16.1726378716504,19.1869023041989,-9.36784806703693));
#42029=CARTESIAN_POINT('Ctrl Pts',(-16.1764051921425,19.1000549738833,-9.37216422977585));
#42030=CARTESIAN_POINT('Ctrl Pts',(-16.1800497925657,19.016036686218,-9.37633979396753));
#42031=CARTESIAN_POINT('Ctrl Pts',(-16.1878361499306,18.9322587224488,-9.38051535815921));
#42032=CARTESIAN_POINT('Ctrl Pts',(-16.1997016639331,18.8491548068463,-9.38469092235089));
#42033=CARTESIAN_POINT('Ctrl Pts',(-16.2121664768403,18.7618535100274,-9.38907738436343));
#42034=CARTESIAN_POINT('Ctrl Pts',(-16.2291332400404,18.6752967161991,-9.39346384637597));
#42035=CARTESIAN_POINT('Ctrl Pts',(-16.2504693406595,18.5899722517347,-9.39785030838851));
#42036=CARTESIAN_POINT('Ctrl Pts',(-16.2718054412786,18.5046477872702,-9.40223677040106));
#42037=CARTESIAN_POINT('Ctrl Pts',(-16.2975106369606,18.4205561848056,-9.4066232324136));
#42038=CARTESIAN_POINT('Ctrl Pts',(-16.3273937923111,18.3381617783842,-9.41100969442614));
#42039=CARTESIAN_POINT('Ctrl Pts',(-16.3559019793865,18.2595584607401,-9.41519432881919));
#42040=CARTESIAN_POINT('Ctrl Pts',(-16.3883182194788,18.1822070136537,-9.41937896321224));
#42041=CARTESIAN_POINT('Ctrl Pts',(-16.4245126604673,18.1065235500301,-9.42356359760528));
#42042=CARTESIAN_POINT('Ctrl Pts',(-16.460655583149,18.0309478124493,-9.42774227568923));
#42043=CARTESIAN_POINT('Ctrl Pts',(-16.500565827944,17.9570357539527,-9.43192095377317));
#42044=CARTESIAN_POINT('Ctrl Pts',(-16.5440645726776,17.8851859767833,-9.43609963185711));
#42045=CARTESIAN_POINT('Ctrl Pts',(-16.5883430011486,17.8120483439956,-9.44035320974255));
#42046=CARTESIAN_POINT('Ctrl Pts',(-16.6363396782675,17.7410481057698,-9.44460678762798));
#42047=CARTESIAN_POINT('Ctrl Pts',(-16.6878157496594,17.6725819769457,-9.44886036551342));
#42048=CARTESIAN_POINT('Ctrl Pts',(-16.7382938569602,17.6054431976296,-9.45303147949137));
#42049=CARTESIAN_POINT('Ctrl Pts',(-16.7921173635638,17.5407415318688,-9.45720259346933));
#42050=CARTESIAN_POINT('Ctrl Pts',(-16.8490169269279,17.4788225223056,-9.46137370744728));
#42051=CARTESIAN_POINT('Ctrl Pts',(-16.905897397094,17.416924290264,-9.46554342176765));
#42052=CARTESIAN_POINT('Ctrl Pts',(-16.9658515630401,17.3578071984336,-9.46971313608802));
#42053=CARTESIAN_POINT('Ctrl Pts',(-17.0285707636154,17.3017825897283,-9.4738828504084));
#42054=CARTESIAN_POINT('Ctrl Pts',(-17.0912877323723,17.2457599746191,-9.47805241635244));
#42055=CARTESIAN_POINT('Ctrl Pts',(-17.1567691964755,17.1928299296704,-9.48222198229649));
#42056=CARTESIAN_POINT('Ctrl Pts',(-17.2246717329646,17.1432649632199,-9.48639154824053));
#42057=CARTESIAN_POINT('Ctrl Pts',(-17.2949616388698,17.0919573536941,-9.49070771097945));
#42058=CARTESIAN_POINT('Ctrl Pts',(-17.3678456086251,17.0442561687145,-9.49502387371837));
#42059=CARTESIAN_POINT('Ctrl Pts',(-17.442909648662,17.000415076347,-9.49934003645729));
#42060=CARTESIAN_POINT('Ctrl Pts',(-17.51552848549,16.9580021029521,-9.50351560064897));
#42061=CARTESIAN_POINT('Ctrl Pts',(-17.5901871024314,16.9192017744647,-9.50769116484065));
#42062=CARTESIAN_POINT('Ctrl Pts',(-17.6664869216557,16.8841962206572,-9.51186672903233));
#42063=CARTESIAN_POINT('Ctrl Pts',(-17.7466404633633,16.8474226195448,-9.51625319104487));
#42064=CARTESIAN_POINT('Ctrl Pts',(-17.8286048161833,16.8148374315278,-9.52063965305741));
#42065=CARTESIAN_POINT('Ctrl Pts',(-17.9118980145026,16.7865932013292,-9.52502611506995));
#42066=CARTESIAN_POINT('Ctrl Pts',(-17.9951912128219,16.7583489711306,-9.52941257708249));
#42067=CARTESIAN_POINT('Ctrl Pts',(-18.0798126775951,16.7344457832731,-9.53379903909503));
#42068=CARTESIAN_POINT('Ctrl Pts',(-18.1652685194102,16.7149742583487,-9.53818550110756));
#42069=CARTESIAN_POINT('Ctrl Pts',(-18.2467924112676,16.6963986471497,-9.54237013550061));
#42070=CARTESIAN_POINT('Ctrl Pts',(-18.3293790330748,16.6817867038644,-9.54655476989366));
#42071=CARTESIAN_POINT('Ctrl Pts',(-18.4126082132396,16.6712544774323,-9.55073940428671));
#42072=CARTESIAN_POINT('Ctrl Pts',(-18.4957189269681,16.6607372423208,-9.55491808237065));
#42073=CARTESIAN_POINT('Ctrl Pts',(-18.5794699298767,16.654288246849,-9.5590967604546));
#42074=CARTESIAN_POINT('Ctrl Pts',(-18.6634292675078,16.6519728857014,-9.56327543853854));
#42075=CARTESIAN_POINT('Ctrl Pts',(-18.7488935159254,16.6496160233692,-9.56752901642397));
#42076=CARTESIAN_POINT('Ctrl Pts',(-18.8345731712375,16.6515425508617,-9.57178259430941));
#42077=CARTESIAN_POINT('Ctrl Pts',(-18.9200053717024,16.6577663636679,-9.57603617219484));
#42078=CARTESIAN_POINT('Ctrl Pts',(-19.0037813022539,16.663869515718,-9.5802072861728));
#42079=CARTESIAN_POINT('Ctrl Pts',(-19.0873188071791,16.6741047825048,-9.58437840015075));
#42080=CARTESIAN_POINT('Ctrl Pts',(-19.1701815497895,16.6884327252533,-9.5885495141287));
#42081=CARTESIAN_POINT('Ctrl Pts',(-19.2530164870063,16.7027558601221,-9.59271922844908));
#42082=CARTESIAN_POINT('Ctrl Pts',(-19.335176658659,16.7211688651668,-9.59688894276945));
#42083=CARTESIAN_POINT('Ctrl Pts',(-19.4162332022013,16.7435807292205,-9.60105865708982));
#42084=CARTESIAN_POINT('Ctrl Pts',(-19.4972868614039,16.7659917957639,-9.60522822303387));
#42085=CARTESIAN_POINT('Ctrl Pts',(-19.5772365274094,16.7924013149753,-9.60939778897791));
#42086=CARTESIAN_POINT('Ctrl Pts',(-19.6556671754964,16.8226680260876,-9.61356735492195));
#42087=CARTESIAN_POINT('Ctrl Pts',(-19.7368553484154,16.8539988774245,-9.61788351766088));
#42088=CARTESIAN_POINT('Ctrl Pts',(-19.8164152065818,16.8894630151455,-9.6221996803998));
#42089=CARTESIAN_POINT('Ctrl Pts',(-19.8939093684294,16.9288496418882,-9.62651584313872));
#42090=CARTESIAN_POINT('Ctrl Pts',(-19.9688791661058,16.9669532534075,-9.6306914073304));
#42091=CARTESIAN_POINT('Ctrl Pts',(-20.0419153954163,17.0087274533691,-9.63486697152208));
#42092=CARTESIAN_POINT('Ctrl Pts',(-20.1126491714249,17.0539356842854,-9.63904253571376));
#42093=CARTESIAN_POINT('Ctrl Pts',(-20.1869555423062,17.1014272754729,-9.6434289977263));
#42094=CARTESIAN_POINT('Ctrl Pts',(-20.2587202783153,17.1527085808079,-9.64781545973884));
#42095=CARTESIAN_POINT('Ctrl Pts',(-20.3275542346358,17.2074569130477,-9.65220192175138));
#42096=CARTESIAN_POINT('Ctrl Pts',(-20.3963881909563,17.2622052452875,-9.65658838376392));
#42097=CARTESIAN_POINT('Ctrl Pts',(-20.4622909830917,17.3204201632972,-9.66097484577647));
#42098=CARTESIAN_POINT('Ctrl Pts',(-20.5249190804939,17.3817354354487,-9.66536130778901));
#42099=CARTESIAN_POINT('Ctrl Pts',(-20.5852113014986,17.440763796406,-9.66958416538902));
#42100=CARTESIAN_POINT('Ctrl Pts',(-20.6427127908696,17.5029045422552,-9.67380702298903));
#42101=CARTESIAN_POINT('Ctrl Pts',(-20.6970796830689,17.5678572314245,-9.67802988058905));
#42102=CARTESIAN_POINT('Ctrl Pts',(-20.7500936846377,17.6311936081461,-9.68214765466765));
#42103=CARTESIAN_POINT('Ctrl Pts',(-20.8001269202378,17.697203245602,-9.68626542874624));
#42104=CARTESIAN_POINT('Ctrl Pts',(-20.8468954124061,17.7655682388181,-9.69038320282484));
#42105=CARTESIAN_POINT('Ctrl Pts',(-20.89361966769,17.8338685676809,-9.69449708202705));
#42106=CARTESIAN_POINT('Ctrl Pts',(-20.9370850392269,17.9045194435154,-9.69861096122926));
#42107=CARTESIAN_POINT('Ctrl Pts',(-20.9770478427322,17.9771700379653,-9.70272484043147));
#42108=CARTESIAN_POINT('Ctrl Pts',(-21.016985643432,18.0497751784301,-9.70683614577719));
#42109=CARTESIAN_POINT('Ctrl Pts',(-21.0534249974544,18.1243771397533,-9.71094745112291));
#42110=CARTESIAN_POINT('Ctrl Pts',(-21.0861664418209,18.2005975900803,-9.71505875646863));
#42111=CARTESIAN_POINT('Ctrl Pts',(-21.1204445396303,18.2803952930204,-9.71936301761202));
#42112=CARTESIAN_POINT('Ctrl Pts',(-21.1506688210159,18.3619666588744,-9.72366727875541));
#42113=CARTESIAN_POINT('Ctrl Pts',(-21.1766659614561,18.4448518415192,-9.7279715398988));
#42114=CARTESIAN_POINT('Ctrl Pts',(-21.2014998963996,18.5240284432037,-9.73208321292915));
#42115=CARTESIAN_POINT('Ctrl Pts',(-21.2224767553181,18.6044033134951,-9.7361948859595));
#42116=CARTESIAN_POINT('Ctrl Pts',(-21.2394965458158,18.6855601281733,-9.74030655898986));
#42117=CARTESIAN_POINT('Ctrl Pts',(-21.2565208804897,18.7667386112071,-9.74441932981087));
#42118=CARTESIAN_POINT('Ctrl Pts',(-21.2695859645565,18.8486989864203,-9.74853210063189));
#42119=CARTESIAN_POINT('Ctrl Pts',(-21.2786432445869,18.9310165044542,-9.7526448714529));
#42120=CARTESIAN_POINT('Ctrl Pts',(-21.2877094512627,19.0134151527261,-9.75676169572553));
#42121=CARTESIAN_POINT('Ctrl Pts',(-21.2927599450141,19.0961711731438,-9.76087851999816));
#42122=CARTESIAN_POINT('Ctrl Pts',(-21.2937982075177,19.1788575547119,-9.76499534427079));
#42123=CARTESIAN_POINT('Ctrl Pts',(-21.2939423435977,19.1903364349236,-9.76556685957696));
#42124=CARTESIAN_POINT('Ctrl Pts',(-21.2940092371596,19.2018139780893,-9.76613837488313));
#42125=CARTESIAN_POINT('Ctrl Pts',(-21.2939989766127,19.2132890482674,-9.7667098901893));
#42126=CARTESIAN_POINT('Origin',(-18.734,19.211,1.76670989022852));
#42127=CARTESIAN_POINT('',(-17.1744642439897,21.2411350264762,-8.45013429617857));
#42128=CARTESIAN_POINT('',(-17.1744642439897,21.2411350264762,-8.51667714376075));
#42129=CARTESIAN_POINT('',(-17.1744642439897,21.2411350264762,1.76670989022852));
#42130=CARTESIAN_POINT('',(-21.2943302600992,19.210357489227,-9.03329016591285));
#42131=CARTESIAN_POINT('Ctrl Pts',(-17.1744642439897,21.2411350264762,-8.51667714376075));
#42132=CARTESIAN_POINT('Ctrl Pts',(-17.1602591749695,21.2302227902137,-8.51757292642982));
#42133=CARTESIAN_POINT('Ctrl Pts',(-17.1461740411721,21.2191656025168,-8.51846870909889));
#42134=CARTESIAN_POINT('Ctrl Pts',(-17.1322119090443,21.2079664272772,-8.51936449176795));
#42135=CARTESIAN_POINT('Ctrl Pts',(-17.0669880324057,21.1556496594946,-8.523549126161));
#42136=CARTESIAN_POINT('Ctrl Pts',(-17.0042085866861,21.1000367097147,-8.52773376055405));
#42137=CARTESIAN_POINT('Ctrl Pts',(-16.9442256444347,21.0413845924179,-8.5319183949471));
#42138=CARTESIAN_POINT('Ctrl Pts',(-16.8843280804773,20.9828159591504,-8.53609707303104));
#42139=CARTESIAN_POINT('Ctrl Pts',(-16.8272194396167,20.9212170697946,-8.54027575111498));
#42140=CARTESIAN_POINT('Ctrl Pts',(-16.7732194376018,20.8568856540237,-8.54445442919893));
#42141=CARTESIAN_POINT('Ctrl Pts',(-16.7182515243598,20.7914011438593,-8.54870800708436));
#42142=CARTESIAN_POINT('Ctrl Pts',(-16.6665051669309,20.723085484341,-8.5529615849698));
#42143=CARTESIAN_POINT('Ctrl Pts',(-16.6182789494494,20.6522926268656,-8.55721516285523));
#42144=CARTESIAN_POINT('Ctrl Pts',(-16.5709876912995,20.5828722270733,-8.56138627683319));
#42145=CARTESIAN_POINT('Ctrl Pts',(-16.527081572471,20.5110702205224,-8.56555739081114));
#42146=CARTESIAN_POINT('Ctrl Pts',(-16.4868009099954,20.4372529306315,-8.56972850478909));
#42147=CARTESIAN_POINT('Ctrl Pts',(-16.446533764085,20.3634604108451,-8.57389821910947));
#42148=CARTESIAN_POINT('Ctrl Pts',(-16.4098898786011,20.2876543542439,-8.57806793342984));
#42149=CARTESIAN_POINT('Ctrl Pts',(-16.3770645250476,20.2102272849111,-8.58223764775021));
#42150=CARTESIAN_POINT('Ctrl Pts',(-16.3442403395611,20.1328029707657,-8.58640721369426));
#42151=CARTESIAN_POINT('Ctrl Pts',(-16.3152345946181,20.0537581824513,-8.5905767796383));
#42152=CARTESIAN_POINT('Ctrl Pts',(-16.2901945969737,19.973505837446,-8.59474634558234));
#42153=CARTESIAN_POINT('Ctrl Pts',(-16.2642742239022,19.8904319189923,-8.59906250832126));
#42154=CARTESIAN_POINT('Ctrl Pts',(-16.2426038152404,19.8060644520148,-8.60337867106018));
#42155=CARTESIAN_POINT('Ctrl Pts',(-16.225290101654,19.7208770890525,-8.6076948337991));
#42156=CARTESIAN_POINT('Ctrl Pts',(-16.2085403804666,19.6384646954785,-8.61187039799078));
#42157=CARTESIAN_POINT('Ctrl Pts',(-16.1958678987932,19.5552854746203,-8.61604596218246));
#42158=CARTESIAN_POINT('Ctrl Pts',(-16.1873166326445,19.471775432959,-8.62022152637414));
#42159=CARTESIAN_POINT('Ctrl Pts',(-16.1783334623714,19.3840474976197,-8.62460798838669));
#42160=CARTESIAN_POINT('Ctrl Pts',(-16.173898803398,19.2959550268228,-8.62899445039922));
#42161=CARTESIAN_POINT('Ctrl Pts',(-16.1740017537922,19.2080034331647,-8.63338091241176));
#42162=CARTESIAN_POINT('Ctrl Pts',(-16.1741047041864,19.1200518395067,-8.63776737442431));
#42163=CARTESIAN_POINT('Ctrl Pts',(-16.1787451573697,19.0322416983818,-8.64215383643685));
#42164=CARTESIAN_POINT('Ctrl Pts',(-16.1878497481281,18.9450697555886,-8.64654029844939));
#42165=CARTESIAN_POINT('Ctrl Pts',(-16.1965354231695,18.8619087231031,-8.65072493284244));
#42166=CARTESIAN_POINT('Ctrl Pts',(-16.2093157897326,18.7790189093826,-8.65490956723549));
#42167=CARTESIAN_POINT('Ctrl Pts',(-16.2261653095063,18.6968354687883,-8.65909420162853));
#42168=CARTESIAN_POINT('Ctrl Pts',(-16.2429908460741,18.6147690061494,-8.66327287971248));
#42169=CARTESIAN_POINT('Ctrl Pts',(-16.2638739396399,18.5334073663311,-8.66745155779642));
#42170=CARTESIAN_POINT('Ctrl Pts',(-16.2887373027363,18.4531805351071,-8.67163023588037));
#42171=CARTESIAN_POINT('Ctrl Pts',(-16.3140463237472,18.3715156955915,-8.6758838137658));
#42172=CARTESIAN_POINT('Ctrl Pts',(-16.3434796603857,18.2910272272441,-8.68013739165124));
#42173=CARTESIAN_POINT('Ctrl Pts',(-16.3769013134697,18.2121577792479,-8.68439096953667));
#42174=CARTESIAN_POINT('Ctrl Pts',(-16.4096750225917,18.1348173694021,-8.68856208351463));
#42175=CARTESIAN_POINT('Ctrl Pts',(-16.4462835978107,18.0590342074479,-8.69273319749258));
#42176=CARTESIAN_POINT('Ctrl Pts',(-16.4865490981547,17.9852086458966,-8.69690431147053));
#42177=CARTESIAN_POINT('Ctrl Pts',(-16.5268010870212,17.9114078572255,-8.70107402579091));
#42178=CARTESIAN_POINT('Ctrl Pts',(-16.570707343848,17.8395637678914,-8.70524374011128));
#42179=CARTESIAN_POINT('Ctrl Pts',(-16.6180435147611,17.7700530361685,-8.70941345443165));
#42180=CARTESIAN_POINT('Ctrl Pts',(-16.6653780012501,17.7005447779356,-8.71358302037569));
#42181=CARTESIAN_POINT('Ctrl Pts',(-16.7161418995134,17.6333700919857,-8.71775258631974));
#42182=CARTESIAN_POINT('Ctrl Pts',(-16.7700677456501,17.5688763443869,-8.72192215226378));
#42183=CARTESIAN_POINT('Ctrl Pts',(-16.8258895580122,17.5021150761843,-8.72623831500271));
#42184=CARTESIAN_POINT('Ctrl Pts',(-16.8850994651023,17.4382271821969,-8.73055447774162));
#42185=CARTESIAN_POINT('Ctrl Pts',(-16.9473569713774,17.3775587851599,-8.73487064048054));
#42186=CARTESIAN_POINT('Ctrl Pts',(-17.007586445934,17.3188666547752,-8.73904620467222));
#42187=CARTESIAN_POINT('Ctrl Pts',(-17.0706676333014,17.2631877685198,-8.7432217688639));
#42188=CARTESIAN_POINT('Ctrl Pts',(-17.1362577244093,17.2107951052979,-8.74739733305558));
#42189=CARTESIAN_POINT('Ctrl Pts',(-17.2051606150934,17.1557562132084,-8.75178379506812));
#42190=CARTESIAN_POINT('Ctrl Pts',(-17.2768320453054,17.1043445831753,-8.75617025708067));
#42191=CARTESIAN_POINT('Ctrl Pts',(-17.3508411420262,17.0568246186514,-8.76055671909321));
#42192=CARTESIAN_POINT('Ctrl Pts',(-17.4248502387469,17.0093046541275,-8.76494318110575));
#42193=CARTESIAN_POINT('Ctrl Pts',(-17.5011964604717,16.9656765769471,-8.76932964311829));
#42194=CARTESIAN_POINT('Ctrl Pts',(-17.5794224113971,16.926147577655,-8.77371610513083));
#42195=CARTESIAN_POINT('Ctrl Pts',(-17.6540490703618,16.8884373662163,-8.77790073952388));
#42196=CARTESIAN_POINT('Ctrl Pts',(-17.730664056125,16.8543169479217,-8.78208537391692));
#42197=CARTESIAN_POINT('Ctrl Pts',(-17.8088876493305,16.8240003898956,-8.78627000830997));
#42198=CARTESIAN_POINT('Ctrl Pts',(-17.8869999009331,16.7937269837374,-8.79044868639391));
#42199=CARTESIAN_POINT('Ctrl Pts',(-17.9667157867297,16.7672468481169,-8.79462736447786));
#42200=CARTESIAN_POINT('Ctrl Pts',(-18.0476319224908,16.7447277396491,-8.7988060425618));
#42201=CARTESIAN_POINT('Ctrl Pts',(-18.1299984218321,16.7218049923463,-8.80305962044724));
#42202=CARTESIAN_POINT('Ctrl Pts',(-18.213608193011,16.7029868892008,-8.80731319833267));
#42203=CARTESIAN_POINT('Ctrl Pts',(-18.2980154243377,16.6883986740302,-8.81156677621811));
#42204=CARTESIAN_POINT('Ctrl Pts',(-18.380786256778,16.6740932798773,-8.81573789019606));
#42205=CARTESIAN_POINT('Ctrl Pts',(-18.4643234304655,16.6638553099794,-8.81990900417401));
#42206=CARTESIAN_POINT('Ctrl Pts',(-18.5481939962223,16.6577518473599,-8.82408011815197));
#42207=CARTESIAN_POINT('Ctrl Pts',(-18.6320364184008,16.6516504328163,-8.82824983247234));
#42208=CARTESIAN_POINT('Ctrl Pts',(-18.7162115520294,16.6496808035662,-8.83241954679271));
#42209=CARTESIAN_POINT('Ctrl Pts',(-18.8002812486104,16.6518581914863,-8.83658926111308));
#42210=CARTESIAN_POINT('Ctrl Pts',(-18.8843479536308,16.6540355019256,-8.84075882705713));
#42211=CARTESIAN_POINT('Ctrl Pts',(-18.9683087692067,16.660359523368,-8.84492839300117));
#42212=CARTESIAN_POINT('Ctrl Pts',(-19.0517268423097,16.6707933836643,-8.84909795894522));
#42213=CARTESIAN_POINT('Ctrl Pts',(-19.1380777919556,16.681594085617,-8.85341412168414));
#42214=CARTESIAN_POINT('Ctrl Pts',(-19.2238466000237,16.6967989420232,-8.85773028442306));
#42215=CARTESIAN_POINT('Ctrl Pts',(-19.3085579282895,16.7163089996876,-8.86204644716198));
#42216=CARTESIAN_POINT('Ctrl Pts',(-19.3905097939472,16.7351835192757,-8.86622201135366));
#42217=CARTESIAN_POINT('Ctrl Pts',(-19.4714715762059,16.758086889941,-8.87039757554534));
#42218=CARTESIAN_POINT('Ctrl Pts',(-19.551028186959,16.7848786218092,-8.87457313973702));
#42219=CARTESIAN_POINT('Ctrl Pts',(-19.6346030129933,16.8130235403628,-8.87895960174956));
#42220=CARTESIAN_POINT('Ctrl Pts',(-19.716626443602,16.8454597306831,-8.8833460637621));
#42221=CARTESIAN_POINT('Ctrl Pts',(-19.7966429339306,16.8819680133224,-8.88773252577464));
#42222=CARTESIAN_POINT('Ctrl Pts',(-19.8766594242591,16.9184762959617,-8.89211898778718));
#42223=CARTESIAN_POINT('Ctrl Pts',(-19.9546684946739,16.959056335675,-8.89650544979972));
#42224=CARTESIAN_POINT('Ctrl Pts',(-20.0302483510423,17.003435683288,-8.90089191181226));
#42225=CARTESIAN_POINT('Ctrl Pts',(-20.102350666183,17.0457730713314,-8.90507654620531));
#42226=CARTESIAN_POINT('Ctrl Pts',(-20.1725107769709,17.0917254144961,-8.90926118059836));
#42227=CARTESIAN_POINT('Ctrl Pts',(-20.240343151946,17.1410892993693,-8.91344581499141));
#42228=CARTESIAN_POINT('Ctrl Pts',(-20.3080789759311,17.1903829208624,-8.91762449307535));
#42229=CARTESIAN_POINT('Ctrl Pts',(-20.373493276466,17.243078170329,-8.9218031711593));
#42230=CARTESIAN_POINT('Ctrl Pts',(-20.4362266525528,17.2989266689431,-8.92598184924324));
#42231=CARTESIAN_POINT('Ctrl Pts',(-20.5000844793203,17.3557762117573,-8.93023542712868));
#42232=CARTESIAN_POINT('Ctrl Pts',(-20.5611639093906,17.4158929154665,-8.93448900501411));
#42233=CARTESIAN_POINT('Ctrl Pts',(-20.6191183231213,17.4789697150938,-8.93874258289955));
#42234=CARTESIAN_POINT('Ctrl Pts',(-20.6759491774531,17.5408236478761,-8.9429136968775));
#42235=CARTESIAN_POINT('Ctrl Pts',(-20.7297747776526,17.6055235719756,-8.94708481085545));
#42236=CARTESIAN_POINT('Ctrl Pts',(-20.7803043703348,17.6727417564177,-8.9512559248334));
#42237=CARTESIAN_POINT('Ctrl Pts',(-20.8308170073241,17.7399373851488,-8.95542563915377));
#42238=CARTESIAN_POINT('Ctrl Pts',(-20.8780355571482,17.8096492285708,-8.95959535347414));
#42239=CARTESIAN_POINT('Ctrl Pts',(-20.9217100507379,17.8815171178612,-8.96376506779451));
#42240=CARTESIAN_POINT('Ctrl Pts',(-20.9653829902017,17.9533824497836,-8.96793463373855));
#42241=CARTESIAN_POINT('Ctrl Pts',(-21.0055118859952,18.0274032814579,-8.9721041996826));
#42242=CARTESIAN_POINT('Ctrl Pts',(-21.0418912815019,18.1031923304257,-8.97627376562664));
#42243=CARTESIAN_POINT('Ctrl Pts',(-21.0795497316758,18.1816460288594,-8.98058992836556));
#42244=CARTESIAN_POINT('Ctrl Pts',(-21.1131898827321,18.2619941236263,-8.98490609110448));
#42245=CARTESIAN_POINT('Ctrl Pts',(-21.1426376470828,18.3437833690158,-8.9892222538434));
#42246=CARTESIAN_POINT('Ctrl Pts',(-21.171126153607,18.4229083383394,-8.99339781803508));
#42247=CARTESIAN_POINT('Ctrl Pts',(-21.1956911205896,18.5033815448835,-8.99757338222676));
#42248=CARTESIAN_POINT('Ctrl Pts',(-21.2162259984621,18.5847779207351,-9.00174894641844));
#42249=CARTESIAN_POINT('Ctrl Pts',(-21.2377980441989,18.6702854340294,-9.00613540843098));
#42250=CARTESIAN_POINT('Ctrl Pts',(-21.254922068569,18.7568112533014,-9.01052187044352));
#42251=CARTESIAN_POINT('Ctrl Pts',(-21.2675357890124,18.8438536997419,-9.01490833245606));
#42252=CARTESIAN_POINT('Ctrl Pts',(-21.2801495094559,18.9308961461825,-9.01929479446861));
#42253=CARTESIAN_POINT('Ctrl Pts',(-21.288252948244,19.0184546350337,-9.02368125648114));
#42254=CARTESIAN_POINT('Ctrl Pts',(-21.2918468828523,19.10602703261,-9.02806771849369));
#42255=CARTESIAN_POINT('Ctrl Pts',(-21.2932731600888,19.1407807303868,-9.02980851558629));
#42256=CARTESIAN_POINT('Ctrl Pts',(-21.2939911726516,19.1755636940745,-9.0315493126789));
#42257=CARTESIAN_POINT('Ctrl Pts',(-21.2939999191096,19.2103564484228,-9.0332901097715));
#42258=CARTESIAN_POINT('Ctrl Pts',(-21.2980344970333,19.2103691601534,-9.03329079544681));
#42259=CARTESIAN_POINT('Ctrl Pts',(-21.2952860334465,20.0241271385548,-9.07394170535625));
#42260=CARTESIAN_POINT('Ctrl Pts',(-20.4360629396139,21.691476034616,-9.15698455082618));
#42261=CARTESIAN_POINT('Ctrl Pts',(-18.2953377909523,21.9356233336023,-9.25149015500852));
#42262=CARTESIAN_POINT('Ctrl Pts',(-17.3565755020692,21.3826576096171,-9.30534484928144));
#42263=CARTESIAN_POINT('Ctrl Pts',(-17.1750494706848,21.2403917593382,-9.31680760799388));
#42264=CARTESIAN_POINT('',(-21.293999998394,19.2110906788005,-8.96670989026365));
#42265=CARTESIAN_POINT('Ctrl Pts',(-21.293999998394,19.2110906788005,-8.96670989026365));
#42266=CARTESIAN_POINT('Ctrl Pts',(-21.2939968622716,19.2996281672638,-8.97108917708311));
#42267=CARTESIAN_POINT('Ctrl Pts',(-21.2893963356695,19.3880718027693,-8.97546846390256));
#42268=CARTESIAN_POINT('Ctrl Pts',(-21.2802532223815,19.4759424985004,-8.97984775072202));
#42269=CARTESIAN_POINT('Ctrl Pts',(-21.2710840473103,19.5640636632957,-8.98423952038189));
#42270=CARTESIAN_POINT('Ctrl Pts',(-21.2573464424813,19.6516082364874,-8.98863129004176));
#42271=CARTESIAN_POINT('Ctrl Pts',(-21.2391468026208,19.7381048257401,-8.99302305970162));
#42272=CARTESIAN_POINT('Ctrl Pts',(-21.2209205771356,19.824727767266,-8.99742124475988));
#42273=CARTESIAN_POINT('Ctrl Pts',(-21.1982194166657,19.9102992971048,-9.00181942981815));
#42274=CARTESIAN_POINT('Ctrl Pts',(-21.1711995861977,19.9943633748381,-9.00621761487641));
#42275=CARTESIAN_POINT('Ctrl Pts',(-21.1441046030879,20.0786612674182,-9.01062803299537));
#42276=CARTESIAN_POINT('Ctrl Pts',(-21.1126670698914,20.1614429605725,-9.01503845111432));
#42277=CARTESIAN_POINT('Ctrl Pts',(-21.0770917883153,20.2422714829421,-9.01944886923327));
#42278=CARTESIAN_POINT('Ctrl Pts',(-21.0501146625114,20.3035646370618,-9.02279333761612));
#42279=CARTESIAN_POINT('Ctrl Pts',(-21.0207591774505,20.3637350853212,-9.02613780599898));
#42280=CARTESIAN_POINT('Ctrl Pts',(-20.989131617054,20.4226028184861,-9.02948227438183));
#42281=CARTESIAN_POINT('Ctrl Pts',(-20.9495588772781,20.4962587519987,-9.03366690877488));
#42282=CARTESIAN_POINT('Ctrl Pts',(-20.9063001320242,20.5681109610611,-9.03785154316793));
#42283=CARTESIAN_POINT('Ctrl Pts',(-20.8595440286337,20.6377664778581,-9.04203617756098));
#42284=CARTESIAN_POINT('Ctrl Pts',(-20.8128544767691,20.7073228486487,-9.04621485564492));
#42285=CARTESIAN_POINT('Ctrl Pts',(-20.7626777089519,20.7746883591287,-9.05039353372887));
#42286=CARTESIAN_POINT('Ctrl Pts',(-20.7092482964899,20.8394944480144,-9.05457221181281));
#42287=CARTESIAN_POINT('Ctrl Pts',(-20.6548612002085,20.9054621394682,-9.05882578969825));
#42288=CARTESIAN_POINT('Ctrl Pts',(-20.5971039332158,20.9687773268414,-9.06307936758368));
#42289=CARTESIAN_POINT('Ctrl Pts',(-20.5362701954423,21.0290819955712,-9.06733294546912));
#42290=CARTESIAN_POINT('Ctrl Pts',(-20.4766158383829,21.0882175406228,-9.07150405944707));
#42291=CARTESIAN_POINT('Ctrl Pts',(-20.4140035745829,21.1444579161298,-9.07567517342502));
#42292=CARTESIAN_POINT('Ctrl Pts',(-20.3487498736145,21.1975001499275,-9.07984628740297));
#42293=CARTESIAN_POINT('Ctrl Pts',(-20.2835180691557,21.2505245848913,-9.08401600172335));
#42294=CARTESIAN_POINT('Ctrl Pts',(-20.2156469445307,21.3003527195436,-9.08818571604372));
#42295=CARTESIAN_POINT('Ctrl Pts',(-20.1454869304126,21.3467211066228,-9.09235543036409));
#42296=CARTESIAN_POINT('Ctrl Pts',(-20.0753294128889,21.3930878437159,-9.09652499630814));
#42297=CARTESIAN_POINT('Ctrl Pts',(-20.0028835520724,21.4359948250818,-9.10069456225219));
#42298=CARTESIAN_POINT('Ctrl Pts',(-19.9285285607301,21.475222055718,-9.10486412819624));
#42299=CARTESIAN_POINT('Ctrl Pts',(-19.8515593396191,21.5158284673914,-9.10918029093516));
#42300=CARTESIAN_POINT('Ctrl Pts',(-19.7725447065604,21.5524913076845,-9.11349645367408));
#42301=CARTESIAN_POINT('Ctrl Pts',(-19.6919309796755,21.585019426664,-9.11781261641299));
#42302=CARTESIAN_POINT('Ctrl Pts',(-19.6139432364647,21.6164879455891,-9.12198818060467));
#42303=CARTESIAN_POINT('Ctrl Pts',(-19.5344594409715,21.6440868736177,-9.12616374479635));
#42304=CARTESIAN_POINT('Ctrl Pts',(-19.4539003149003,21.6676936187906,-9.13033930898803));
#42305=CARTESIAN_POINT('Ctrl Pts',(-19.3692723388824,21.6924926845425,-9.13472577100057));
#42306=CARTESIAN_POINT('Ctrl Pts',(-19.2834581156084,21.7128855434687,-9.13911223301311));
#42307=CARTESIAN_POINT('Ctrl Pts',(-19.1969566012277,21.7287909336122,-9.14349869502565));
#42308=CARTESIAN_POINT('Ctrl Pts',(-19.110455086847,21.7446963237556,-9.14788515703818));
#42309=CARTESIAN_POINT('Ctrl Pts',(-19.0232668665414,21.756114245197,-9.15227161905073));
#42310=CARTESIAN_POINT('Ctrl Pts',(-18.9358937423135,21.7630264334083,-9.15665808106326));
#42311=CARTESIAN_POINT('Ctrl Pts',(-18.8525619577015,21.7696189066009,-9.16084165250892));
#42312=CARTESIAN_POINT('Ctrl Pts',(-18.7687518984978,21.7721377831229,-9.16502522395457));
#42313=CARTESIAN_POINT('Ctrl Pts',(-18.6848957690166,21.7705290141937,-9.16920879540023));
#42314=CARTESIAN_POINT('Ctrl Pts',(-18.6011496143914,21.7689223551178,-9.17338688021455));
#42315=CARTESIAN_POINT('Ctrl Pts',(-18.5173579649434,21.7631988058255,-9.17756496502888));
#42316=CARTESIAN_POINT('Ctrl Pts',(-18.4339575044883,21.7533560924636,-9.18174304984321));
#42317=CARTESIAN_POINT('Ctrl Pts',(-18.3506413936366,21.7435233338307,-9.18591690902382));
#42318=CARTESIAN_POINT('Ctrl Pts',(-18.267716140326,21.7295797379285,-9.19009076820444));
#42319=CARTESIAN_POINT('Ctrl Pts',(-18.1856164183454,21.711575023344,-9.19426462738505));
#42320=CARTESIAN_POINT('Ctrl Pts',(-18.1035750976559,21.6935831163372,-9.19843551750853));
#42321=CARTESIAN_POINT('Ctrl Pts',(-18.0223585895858,21.6715359284619,-9.20260640763201));
#42322=CARTESIAN_POINT('Ctrl Pts',(-17.9423930915371,21.645534555613,-9.2067772977555));
#42323=CARTESIAN_POINT('Ctrl Pts',(-17.8624446940832,21.6195387431489,-9.21094729593553));
#42324=CARTESIAN_POINT('Ctrl Pts',(-17.7837472149607,21.5895905593654,-9.21511729411556));
#42325=CARTESIAN_POINT('Ctrl Pts',(-17.7067122821135,21.5558411342092,-9.21928729229559));
#42326=CARTESIAN_POINT('Ctrl Pts',(-17.6296873849862,21.5220961057568,-9.22345674722944));
#42327=CARTESIAN_POINT('Ctrl Pts',(-17.5543250225427,21.4845510104642,-9.22762620216328));
#42328=CARTESIAN_POINT('Ctrl Pts',(-17.4810158732245,21.4434047074956,-9.23179565709713));
#42329=CARTESIAN_POINT('Ctrl Pts',(-17.407668031838,21.4022366877893,-9.23596731264082));
#42330=CARTESIAN_POINT('Ctrl Pts',(-17.3363759656959,21.357463895993,-9.24013896818451));
#42331=CARTESIAN_POINT('Ctrl Pts',(-17.2675040274966,21.3093301843683,-9.2443106237282));
#42332=CARTESIAN_POINT('Ctrl Pts',(-17.2359730000249,21.28729355489,-9.24622049571655));
#42333=CARTESIAN_POINT('Ctrl Pts',(-17.204948823483,21.264553070649,-9.24813036770491));
#42334=CARTESIAN_POINT('Ctrl Pts',(-17.1744642439897,21.2411350264762,-9.25004023969326));
#42335=CARTESIAN_POINT('Ctrl Pts',(-17.1744642439897,21.2411350264762,-8.45013429617857));
#42336=CARTESIAN_POINT('Ctrl Pts',(-17.1077840465769,21.1899117577148,-8.45430378103253));
#42337=CARTESIAN_POINT('Ctrl Pts',(-17.0436167203881,21.1353895379119,-8.4584732658865));
#42338=CARTESIAN_POINT('Ctrl Pts',(-16.9822967584395,21.0778518295533,-8.46264275074046));
#42339=CARTESIAN_POINT('Ctrl Pts',(-16.9209699105371,21.0203076599707,-8.46681270380869));
#42340=CARTESIAN_POINT('Ctrl Pts',(-16.8624913963391,20.9597476451823,-8.47098265687691));
#42341=CARTESIAN_POINT('Ctrl Pts',(-16.807159597991,20.8964928256109,-8.47515260994513));
#42342=CARTESIAN_POINT('Ctrl Pts',(-16.7517686933345,20.8331704362336,-8.47932701742364));
#42343=CARTESIAN_POINT('Ctrl Pts',(-16.6995315186948,20.7671478420157,-8.48350142490214));
#42344=CARTESIAN_POINT('Ctrl Pts',(-16.6507064613291,20.6987795642272,-8.48767583238065));
#42345=CARTESIAN_POINT('Ctrl Pts',(-16.6018534047597,20.6303720799852,-8.49185263371371));
#42346=CARTESIAN_POINT('Ctrl Pts',(-16.5564166096692,20.5596166212149,-8.49602943504676));
#42347=CARTESIAN_POINT('Ctrl Pts',(-16.5146100453367,20.4868950697998,-8.50020623637982));
#42348=CARTESIAN_POINT('Ctrl Pts',(-16.4727323283785,20.4140497500386,-8.50439014641426));
#42349=CARTESIAN_POINT('Ctrl Pts',(-16.4344973889752,20.3392320654702,-8.50857405644871));
#42350=CARTESIAN_POINT('Ctrl Pts',(-16.4000721978852,20.2628464785868,-8.51275796648315));
#42351=CARTESIAN_POINT('Ctrl Pts',(-16.3780730591327,20.2140328897197,-8.51543166020746));
#42352=CARTESIAN_POINT('Ctrl Pts',(-16.3576287426084,20.1645794072701,-8.51810535393178));
#42353=CARTESIAN_POINT('Ctrl Pts',(-16.3387721302028,20.1145947386671,-8.52077904765609));
#42354=CARTESIAN_POINT('Ctrl Pts',(-16.3092593897977,20.0363630543649,-8.52496368204914));
#42355=CARTESIAN_POINT('Ctrl Pts',(-16.2835285016034,19.95653836908,-8.52914831644219));
#42356=CARTESIAN_POINT('Ctrl Pts',(-16.2617516946766,19.8755211184194,-8.53333295083524));
#42357=CARTESIAN_POINT('Ctrl Pts',(-16.2400058843389,19.7946191857871,-8.53751162891919));
#42358=CARTESIAN_POINT('Ctrl Pts',(-16.2222030943945,19.7125284999512,-8.54169030700313));
#42359=CARTESIAN_POINT('Ctrl Pts',(-16.2084669780844,19.6296680728378,-8.54586898508708));
#42360=CARTESIAN_POINT('Ctrl Pts',(-16.1944846517614,19.5453224321191,-8.55012256297252));
#42361=CARTESIAN_POINT('Ctrl Pts',(-16.1847163934876,19.4601796345795,-8.55437614085795));
#42362=CARTESIAN_POINT('Ctrl Pts',(-16.179239049994,19.3746963295992,-8.55862971874339));
#42363=CARTESIAN_POINT('Ctrl Pts',(-16.1738678954921,19.2908702852928,-8.56280083272134));
#42364=CARTESIAN_POINT('Ctrl Pts',(-16.1726227957354,19.2067172987628,-8.5669719466993));
#42365=CARTESIAN_POINT('Ctrl Pts',(-16.1755241458591,19.1226750104564,-8.57114306067725));
#42366=CARTESIAN_POINT('Ctrl Pts',(-16.1784245224067,19.0386609233514,-8.57531277499763));
#42367=CARTESIAN_POINT('Ctrl Pts',(-16.1854685696706,18.9547579200742,-8.579482489318));
#42368=CARTESIAN_POINT('Ctrl Pts',(-16.1966245729686,18.8714032651844,-8.58365220363838));
#42369=CARTESIAN_POINT('Ctrl Pts',(-16.2077801792882,18.7880515764109,-8.58782176958242));
#42370=CARTESIAN_POINT('Ctrl Pts',(-16.2230473888477,18.705248653083,-8.59199133552647));
#42371=CARTESIAN_POINT('Ctrl Pts',(-16.2423428203254,18.6234248992887,-8.59616090147052));
#42372=CARTESIAN_POINT('Ctrl Pts',(-16.2623166553703,18.5387243232516,-8.60047706420944));
#42373=CARTESIAN_POINT('Ctrl Pts',(-16.2866071262492,18.4550735664097,-8.60479322694835));
#42374=CARTESIAN_POINT('Ctrl Pts',(-16.3150650107316,18.372934657862,-8.60910938968727));
#42375=CARTESIAN_POINT('Ctrl Pts',(-16.3425958826202,18.2934714156207,-8.61328495387895));
#42376=CARTESIAN_POINT('Ctrl Pts',(-16.3740266108365,18.2154234566588,-8.61746051807063));
#42377=CARTESIAN_POINT('Ctrl Pts',(-16.4091731183431,18.1391884632431,-8.62163608226231));
#42378=CARTESIAN_POINT('Ctrl Pts',(-16.4460947923909,18.0591030215414,-8.62602254427484));
#42379=CARTESIAN_POINT('Ctrl Pts',(-16.48711720705,17.9810190212158,-8.63040900628739));
#42380=CARTESIAN_POINT('Ctrl Pts',(-16.5319737202491,17.9053659535359,-8.63479546829992));
#42381=CARTESIAN_POINT('Ctrl Pts',(-16.5768302334482,17.829712885856,-8.63918193031246));
#42382=CARTESIAN_POINT('Ctrl Pts',(-16.625520460569,17.7564911918506,-8.643568392325));
#42383=CARTESIAN_POINT('Ctrl Pts',(-16.677728404917,17.6860911085397,-8.64795485433754));
#42384=CARTESIAN_POINT('Ctrl Pts',(-16.7275341843548,17.6189302374198,-8.65213948873059));
#42385=CARTESIAN_POINT('Ctrl Pts',(-16.7807264703944,17.5540870443,-8.65632412312364));
#42386=CARTESIAN_POINT('Ctrl Pts',(-16.8370617843824,17.49192309476,-8.66050875751669));
#42387=CARTESIAN_POINT('Ctrl Pts',(-16.8933169120239,17.4298476279078,-8.66468743560064));
#42388=CARTESIAN_POINT('Ctrl Pts',(-16.952705875139,17.3704441676471,-8.66886611368458));
#42389=CARTESIAN_POINT('Ctrl Pts',(-17.014943282162,17.3140434899935,-8.67304479176854));
#42390=CARTESIAN_POINT('Ctrl Pts',(-17.0782962499765,17.2566318707276,-8.67729836965397));
#42391=CARTESIAN_POINT('Ctrl Pts',(-17.1446004956336,17.2023321299324,-8.68155194753941));
#42392=CARTESIAN_POINT('Ctrl Pts',(-17.2135136449486,17.151456059196,-8.68580552542484));
#42393=CARTESIAN_POINT('Ctrl Pts',(-17.2810907783913,17.1015663203672,-8.6899766394028));
#42394=CARTESIAN_POINT('Ctrl Pts',(-17.3511761736811,17.054968972992,-8.69414775338075));
#42395=CARTESIAN_POINT('Ctrl Pts',(-17.4234128839599,17.0119180526253,-8.6983188673587));
#42396=CARTESIAN_POINT('Ctrl Pts',(-17.4956253545128,16.9688815784106,-8.70248858167908));
#42397=CARTESIAN_POINT('Ctrl Pts',(-17.5699873115138,16.9293894030873,-8.70665829599945));
#42398=CARTESIAN_POINT('Ctrl Pts',(-17.6461139181108,16.8936515426394,-8.71082801031982));
#42399=CARTESIAN_POINT('Ctrl Pts',(-17.7222378157965,16.8579149538979,-8.71499757626387));
#42400=CARTESIAN_POINT('Ctrl Pts',(-17.8001258214376,16.8259326091334,-8.71916714220791));
#42401=CARTESIAN_POINT('Ctrl Pts',(-17.8793709005808,16.7978673674193,-8.72333670815196));
#42402=CARTESIAN_POINT('Ctrl Pts',(-17.9614021389473,16.7688153864287,-8.72765287089087));
#42403=CARTESIAN_POINT('Ctrl Pts',(-18.0448871586136,16.7439612602711,-8.73196903362979));
#42404=CARTESIAN_POINT('Ctrl Pts',(-18.129356695062,16.7234296042537,-8.73628519636871));
#42405=CARTESIAN_POINT('Ctrl Pts',(-18.2110746452452,16.7035667647714,-8.74046076056039));
#42406=CARTESIAN_POINT('Ctrl Pts',(-18.2937134844275,16.6877491532913,-8.74463632475206));
#42407=CARTESIAN_POINT('Ctrl Pts',(-18.3768391873479,16.676037248024,-8.74881188894374));
#42408=CARTESIAN_POINT('Ctrl Pts',(-18.4641633719102,16.6637338022641,-8.75319835095628));
#42409=CARTESIAN_POINT('Ctrl Pts',(-18.5520243141264,16.6559617726585,-8.75758481296882));
#42410=CARTESIAN_POINT('Ctrl Pts',(-18.6399165515113,16.6527294309005,-8.76197127498136));
#42411=CARTESIAN_POINT('Ctrl Pts',(-18.7278087888962,16.6494970891426,-8.76635773699389));
#42412=CARTESIAN_POINT('Ctrl Pts',(-18.8157317424278,16.65080435055,-8.77074419900643));
#42413=CARTESIAN_POINT('Ctrl Pts',(-18.903186241511,16.6565967398073,-8.77513066101897));
#42414=CARTESIAN_POINT('Ctrl Pts',(-18.9866168294529,16.6621226126484,-8.77931529541202));
#42415=CARTESIAN_POINT('Ctrl Pts',(-19.0699316687706,16.6717505167586,-8.78349992980506));
#42416=CARTESIAN_POINT('Ctrl Pts',(-19.1526949496533,16.6854714337124,-8.78768456419811));
#42417=CARTESIAN_POINT('Ctrl Pts',(-19.2353404272495,16.6991728206391,-8.79186324228204));
#42418=CARTESIAN_POINT('Ctrl Pts',(-19.3174354558604,16.7169555737482,-8.79604192036597));
#42419=CARTESIAN_POINT('Ctrl Pts',(-19.3985474281617,16.7387587666808,-8.8002205984499));
#42420=CARTESIAN_POINT('Ctrl Pts',(-19.4811132742726,16.7609527661771,-8.80447417633534));
#42421=CARTESIAN_POINT('Ctrl Pts',(-19.5626599937758,16.7873127240839,-8.80872775422078));
#42422=CARTESIAN_POINT('Ctrl Pts',(-19.6427400986355,16.8177195247669,-8.81298133210622));
#42423=CARTESIAN_POINT('Ctrl Pts',(-19.721267694399,16.8475368302847,-8.81715244608417));
#42424=CARTESIAN_POINT('Ctrl Pts',(-19.7983845845472,16.8812452961235,-8.82132356006213));
#42425=CARTESIAN_POINT('Ctrl Pts',(-19.8736839568162,16.9186822910915,-8.82549467404008));
#42426=CARTESIAN_POINT('Ctrl Pts',(-19.9489580616535,16.9561067237141,-8.82966438836045));
#42427=CARTESIAN_POINT('Ctrl Pts',(-20.0224154482667,16.9972569960429,-8.83383410268082));
#42428=CARTESIAN_POINT('Ctrl Pts',(-20.0936712215601,17.0419231988559,-8.83800381700119));
#42429=CARTESIAN_POINT('Ctrl Pts',(-20.1649244592672,17.0865878122538,-8.84217338294524));
#42430=CARTESIAN_POINT('Ctrl Pts',(-20.2339758500889,17.1347678623259,-8.84634294888928));
#42431=CARTESIAN_POINT('Ctrl Pts',(-20.3004681352881,17.1862092500392,-8.85051251483332));
#42432=CARTESIAN_POINT('Ctrl Pts',(-20.3692982072079,17.2394592534847,-8.85482867757224));
#42433=CARTESIAN_POINT('Ctrl Pts',(-20.4353854517826,17.29620387614,-8.85914484031116));
#42434=CARTESIAN_POINT('Ctrl Pts',(-20.4983710832764,17.3561159927106,-8.86346100305009));
#42435=CARTESIAN_POINT('Ctrl Pts',(-20.5593049644492,17.4140764783855,-8.86763656724176));
#42436=CARTESIAN_POINT('Ctrl Pts',(-20.6173359087924,17.4750008911684,-8.87181213143344));
#42437=CARTESIAN_POINT('Ctrl Pts',(-20.6721781340603,17.5385570202095,-8.87598769562512));
#42438=CARTESIAN_POINT('Ctrl Pts',(-20.7297903097515,17.6053232182381,-8.88037415763766));
#42439=CARTESIAN_POINT('Ctrl Pts',(-20.7838828183066,17.6749935141292,-8.88476061965021));
#42440=CARTESIAN_POINT('Ctrl Pts',(-20.8341751072843,17.7471473712345,-8.88914708166276));
#42441=CARTESIAN_POINT('Ctrl Pts',(-20.8844673962619,17.8193012283399,-8.8935335436753));
#42442=CARTESIAN_POINT('Ctrl Pts',(-20.930959223453,17.8939381139566,-8.89792000568785));
#42443=CARTESIAN_POINT('Ctrl Pts',(-20.9734262024012,17.9706088181549,-8.9023064677004));
#42444=CARTESIAN_POINT('Ctrl Pts',(-21.0159038253685,18.047298739271,-8.90669402914565));
#42445=CARTESIAN_POINT('Ctrl Pts',(-21.054500797719,18.1262856298352,-8.91108159059091));
#42446=CARTESIAN_POINT('Ctrl Pts',(-21.0889748257326,18.2071605854691,-8.91546915203617));
#42447=CARTESIAN_POINT('Ctrl Pts',(-21.1233545067053,18.2878142059939,-8.91984470579149));
#42448=CARTESIAN_POINT('Ctrl Pts',(-21.1536335666927,18.3703452363822,-8.92422025954681));
#42449=CARTESIAN_POINT('Ctrl Pts',(-21.1796158858341,18.4543211123894,-8.92859581330213));
#42450=CARTESIAN_POINT('Ctrl Pts',(-21.2055560013422,18.5381605845955,-8.93296425975244));
#42451=CARTESIAN_POINT('Ctrl Pts',(-21.2272131436812,18.6234398583861,-8.93733270620275));
#42452=CARTESIAN_POINT('Ctrl Pts',(-21.2444392039475,18.7097066694204,-8.94170115265306));
#42453=CARTESIAN_POINT('Ctrl Pts',(-21.2616295048393,18.7957944002037,-8.94606053069714));
#42454=CARTESIAN_POINT('Ctrl Pts',(-21.274406969619,18.8828651985172,-8.95041990874123));
#42455=CARTESIAN_POINT('Ctrl Pts',(-21.2826736357252,18.9704533339265,-8.95477928678531));
#42456=CARTESIAN_POINT('Ctrl Pts',(-21.2902149496553,19.0503561166423,-8.95875615459971));
#42457=CARTESIAN_POINT('Ctrl Pts',(-21.2940028463113,19.1306890276033,-8.96273302241411));
#42458=CARTESIAN_POINT('Ctrl Pts',(-21.293999998394,19.2110906780901,-8.96670989022851));
#42459=CARTESIAN_POINT('Origin',(-18.734,19.211,1.76670989022852));
#42460=CARTESIAN_POINT('',(-17.1732300852521,21.2427130357989,-7.65021347737831));
#42461=CARTESIAN_POINT('',(-17.1756294998725,21.2395871765567,-7.71658756787471));
#42462=CARTESIAN_POINT('',(-17.1744642439897,21.2411350264762,1.76670989022852));
#42463=CARTESIAN_POINT('',(-21.2939989173812,19.2133543591349,-8.2332901225083));
#42464=CARTESIAN_POINT('Ctrl Pts',(-17.1756294998728,21.2395871765569,-7.7165875678747));
#42465=CARTESIAN_POINT('Ctrl Pts',(-16.9627571463261,21.0789787236254,-7.72982826247625));
#42466=CARTESIAN_POINT('Ctrl Pts',(-16.1737485052776,20.2707708752208,-7.78546089263828));
#42467=CARTESIAN_POINT('Ctrl Pts',(-15.9391113864609,18.0482922133962,-7.88348545836079));
#42468=CARTESIAN_POINT('Ctrl Pts',(-18.1988330487837,16.2315893043347,-8.01066126504222));
#42469=CARTESIAN_POINT('Ctrl Pts',(-20.7208250384235,17.0720883649514,-8.12726281551246));
#42470=CARTESIAN_POINT('Ctrl Pts',(-21.28776986438,18.5735386239974,-8.20147243042222));
#42471=CARTESIAN_POINT('Ctrl Pts',(-21.2935817164968,19.2133537193276,-8.23329010977151));
#42472=CARTESIAN_POINT('Ctrl Pts',(-21.2939989173812,19.2133543591349,-8.2332901225083));
#42473=CARTESIAN_POINT('Ctrl Pts',(-21.2938985191577,19.3225217922602,-8.2387181286671));
#42474=CARTESIAN_POINT('Ctrl Pts',(-21.2868114603045,19.4313771443117,-8.2441461348259));
#42475=CARTESIAN_POINT('Ctrl Pts',(-21.2728791636074,19.5391654957492,-8.2495741409847));
#42476=CARTESIAN_POINT('Ctrl Pts',(-21.2596700733155,19.6413587017587,-8.2547203867915));
#42477=CARTESIAN_POINT('Ctrl Pts',(-21.2403084403105,19.7425933354651,-8.2598666325983));
#42478=CARTESIAN_POINT('Ctrl Pts',(-21.2149532278239,19.84224565848,-8.26501287840509));
#42479=CARTESIAN_POINT('Ctrl Pts',(-21.1943358111288,19.9232772597465,-8.26919751279814));
#42480=CARTESIAN_POINT('Ctrl Pts',(-21.1697059337058,20.0034485022604,-8.27338214719119));
#42481=CARTESIAN_POINT('Ctrl Pts',(-21.1411517779373,20.0823324956486,-8.27756678158424));
#42482=CARTESIAN_POINT('Ctrl Pts',(-21.1126382654752,20.1611042074361,-8.28174545966818));
#42483=CARTESIAN_POINT('Ctrl Pts',(-21.0802117249137,20.2385918806366,-8.28592413775212));
#42484=CARTESIAN_POINT('Ctrl Pts',(-21.04401079686,20.3143812207891,-8.29010281583607));
#42485=CARTESIAN_POINT('Ctrl Pts',(-21.0071609931882,20.391529030395,-8.2943563937215));
#42486=CARTESIAN_POINT('Ctrl Pts',(-20.9664002781982,20.466916555597,-8.29860997160694));
#42487=CARTESIAN_POINT('Ctrl Pts',(-20.9219272181894,20.5401254598066,-8.30286354949238));
#42488=CARTESIAN_POINT('Ctrl Pts',(-20.8783163552309,20.6119150665525,-8.30703466347033));
#42489=CARTESIAN_POINT('Ctrl Pts',(-20.8311360546877,20.6816093608382,-8.31120577744828));
#42490=CARTESIAN_POINT('Ctrl Pts',(-20.7806202689677,20.7488379221006,-8.31537689142623));
#42491=CARTESIAN_POINT('Ctrl Pts',(-20.7301214343074,20.8160439241699,-8.3195466057466));
#42492=CARTESIAN_POINT('Ctrl Pts',(-20.6762896134471,20.8807854689741,-8.32371632006697));
#42493=CARTESIAN_POINT('Ctrl Pts',(-20.6194012584855,20.9427222913912,-8.32788603438735));
#42494=CARTESIAN_POINT('Ctrl Pts',(-20.5625149278557,21.0046569098305,-8.33205560033139));
#42495=CARTESIAN_POINT('Ctrl Pts',(-20.5025725911954,21.0637866660879,-8.33622516627543));
#42496=CARTESIAN_POINT('Ctrl Pts',(-20.4398891227941,21.1198065121255,-8.34039473221948));
#42497=CARTESIAN_POINT('Ctrl Pts',(-20.3750017809722,21.1777959468418,-8.3447108949584));
#42498=CARTESIAN_POINT('Ctrl Pts',(-20.3071773578719,21.2324523620817,-8.34902705769732));
#42499=CARTESIAN_POINT('Ctrl Pts',(-20.2368028123897,21.2834824986169,-8.35334322043624));
#42500=CARTESIAN_POINT('Ctrl Pts',(-20.1687207103245,21.3328503338219,-8.35751878462792));
#42501=CARTESIAN_POINT('Ctrl Pts',(-20.0982524952705,21.3788242964685,-8.36169434881959));
#42502=CARTESIAN_POINT('Ctrl Pts',(-20.0257768405866,21.4211838371783,-8.36586991301127));
#42503=CARTESIAN_POINT('Ctrl Pts',(-19.949640612879,21.4656828575891,-8.37025637502381));
#42504=CARTESIAN_POINT('Ctrl Pts',(-19.8712893431908,21.5061924632349,-8.37464283703635));
#42505=CARTESIAN_POINT('Ctrl Pts',(-19.7911876038235,21.5425133219267,-8.3790292990489));
#42506=CARTESIAN_POINT('Ctrl Pts',(-19.7110858644562,21.5788341806186,-8.38341576106144));
#42507=CARTESIAN_POINT('Ctrl Pts',(-19.6292342232968,21.6109661511407,-8.38780222307398));
#42508=CARTESIAN_POINT('Ctrl Pts',(-19.5461152252309,21.638770347654,-8.39218868508653));
#42509=CARTESIAN_POINT('Ctrl Pts',(-19.4668195289777,21.6652956086964,-8.39637337892868));
#42510=CARTESIAN_POINT('Ctrl Pts',(-19.3860753481862,21.6879812201708,-8.40055807277084));
#42511=CARTESIAN_POINT('Ctrl Pts',(-19.3042893790366,21.7066702554941,-8.404742766613));
#42512=CARTESIAN_POINT('Ctrl Pts',(-19.2226201401935,21.7253326165988,-8.40892148778527));
#42513=CARTESIAN_POINT('Ctrl Pts',(-19.139912511179,21.7400096304283,-8.41310020895756));
#42514=CARTESIAN_POINT('Ctrl Pts',(-19.0565899049923,21.7505936196953,-8.41727893012983));
#42515=CARTESIAN_POINT('Ctrl Pts',(-18.9733652538744,21.7611651662959,-8.4214527387467));
#42516=CARTESIAN_POINT('Ctrl Pts',(-18.8895275166771,21.7676531957154,-8.42562654736356));
#42517=CARTESIAN_POINT('Ctrl Pts',(-18.8055104987545,21.7700010255113,-8.42980035598042));
#42518=CARTESIAN_POINT('Ctrl Pts',(-18.7215478255154,21.7723473366617,-8.43397146485485));
#42519=CARTESIAN_POINT('Ctrl Pts',(-18.6374065603104,21.7705587522904,-8.43814257372929));
#42520=CARTESIAN_POINT('Ctrl Pts',(-18.553524769967,21.7646304923274,-8.44231368260372));
#42521=CARTESIAN_POINT('Ctrl Pts',(-18.4696720738751,21.758704288571,-8.44648334473636));
#42522=CARTESIAN_POINT('Ctrl Pts',(-18.3860791323485,21.748641293549,-8.45065300686901));
#42523=CARTESIAN_POINT('Ctrl Pts',(-18.3031817775257,21.7344887872119,-8.45482266900166));
#42524=CARTESIAN_POINT('Ctrl Pts',(-18.22028830845,21.7203369442622,-8.45899213568473));
#42525=CARTESIAN_POINT('Ctrl Pts',(-18.1380908144902,21.7020960496259,-8.46316160236781));
#42526=CARTESIAN_POINT('Ctrl Pts',(-18.0570164290657,21.6798647684077,-8.46733106905089));
#42527=CARTESIAN_POINT('Ctrl Pts',(-17.9758686662976,21.6576133665023,-8.47150430935972));
#42528=CARTESIAN_POINT('Ctrl Pts',(-17.8958464874927,21.6313644844824,-8.47567754966855));
#42529=CARTESIAN_POINT('Ctrl Pts',(-17.8173628033701,21.6012669829445,-8.47985078997738));
#42530=CARTESIAN_POINT('Ctrl Pts',(-17.7388450977354,21.5711564345863,-8.48402583932395));
#42531=CARTESIAN_POINT('Ctrl Pts',(-17.6618676373455,21.5371941278435,-8.48820088867052));
#42532=CARTESIAN_POINT('Ctrl Pts',(-17.586822033013,21.4995765689746,-8.49237593801708));
#42533=CARTESIAN_POINT('Ctrl Pts',(-17.5116490489329,21.4618951593952,-8.49655807394435));
#42534=CARTESIAN_POINT('Ctrl Pts',(-17.4384148752304,21.4205463260528,-8.50074020987163));
#42535=CARTESIAN_POINT('Ctrl Pts',(-17.3674851353028,21.3757718412252,-8.50492234579891));
#42536=CARTESIAN_POINT('Ctrl Pts',(-17.3010306746449,21.3338223818942,-8.50884061178619));
#42537=CARTESIAN_POINT('Ctrl Pts',(-17.2365990013488,21.2888665194699,-8.51275887777347));
#42538=CARTESIAN_POINT('Ctrl Pts',(-17.1744642439897,21.2411350264762,-8.51667714376075));
#42539=CARTESIAN_POINT('',(-21.2939989424941,19.2086731074563,-8.16670989022852));
#42540=CARTESIAN_POINT('Ctrl Pts',(-21.2939989424941,19.2086731074563,-8.16670989022852));
#42541=CARTESIAN_POINT('Ctrl Pts',(-21.294074804776,19.2921352174732,-8.17086478789788));
#42542=CARTESIAN_POINT('Ctrl Pts',(-21.2900646933588,19.3757219830021,-8.17501968556724));
#42543=CARTESIAN_POINT('Ctrl Pts',(-21.2819596922617,19.458994771335,-8.17917458323661));
#42544=CARTESIAN_POINT('Ctrl Pts',(-21.2739328413916,19.5414646248839,-8.18328941845664));
#42545=CARTESIAN_POINT('Ctrl Pts',(-21.2618897634889,19.6236260477268,-8.18740425367667));
#42546=CARTESIAN_POINT('Ctrl Pts',(-21.2458740550218,19.7050533692914,-8.1915190888967));
#42547=CARTESIAN_POINT('Ctrl Pts',(-21.229865310909,19.7864452825742,-8.19563213480029));
#42548=CARTESIAN_POINT('Ctrl Pts',(-21.2098874553345,19.867103263636,-8.19974518070388));
#42549=CARTESIAN_POINT('Ctrl Pts',(-21.1860355605652,19.9466096857189,-8.20385822660747));
#42550=CARTESIAN_POINT('Ctrl Pts',(-21.1621864189586,20.0261069305809,-8.2079707977528));
#42551=CARTESIAN_POINT('Ctrl Pts',(-21.1344642632168,20.1044524267967,-8.21208336889812));
#42552=CARTESIAN_POINT('Ctrl Pts',(-21.1030141994638,20.1812431255818,-8.21619594004345));
#42553=CARTESIAN_POINT('Ctrl Pts',(-21.0710029255604,20.2594041147406,-8.2203818978976));
#42554=CARTESIAN_POINT('Ctrl Pts',(-21.0351295718013,20.3359537977659,-8.22456785575175));
#42555=CARTESIAN_POINT('Ctrl Pts',(-20.9955977974884,20.4104896424712,-8.22875381360589));
#42556=CARTESIAN_POINT('Ctrl Pts',(-20.9567081892514,20.4838147044139,-8.23287177349699));
#42557=CARTESIAN_POINT('Ctrl Pts',(-20.9142784405329,20.5551904907364,-8.23698973338808));
#42558=CARTESIAN_POINT('Ctrl Pts',(-20.8685472200438,20.624261534679,-8.24110769327918));
#42559=CARTESIAN_POINT('Ctrl Pts',(-20.8216832918827,20.6950433858241,-8.24532765011485));
#42560=CARTESIAN_POINT('Ctrl Pts',(-20.7713524862058,20.7634043768936,-8.24954760695052));
#42561=CARTESIAN_POINT('Ctrl Pts',(-20.7178552814756,20.8289982145112,-8.2537675637862));
#42562=CARTESIAN_POINT('Ctrl Pts',(-20.6643580767454,20.8945920521287,-8.25798752062187));
#42563=CARTESIAN_POINT('Ctrl Pts',(-20.6076948817588,20.9574183953714,-8.26220747745755));
#42564=CARTESIAN_POINT('Ctrl Pts',(-20.5482046419776,21.0171731691692,-8.26642743429322));
#42565=CARTESIAN_POINT('Ctrl Pts',(-20.4892123552949,21.0764277756309,-8.27061206868627));
#42566=CARTESIAN_POINT('Ctrl Pts',(-20.4272042190729,21.1328994502154,-8.27479670307932));
#42567=CARTESIAN_POINT('Ctrl Pts',(-20.3624734272384,21.1862656268913,-8.27898133747237));
#42568=CARTESIAN_POINT('Ctrl Pts',(-20.2978347716739,21.2395558434202,-8.28316001555632));
#42569=CARTESIAN_POINT('Ctrl Pts',(-20.2304815101078,21.2897490519969,-8.28733869364027));
#42570=CARTESIAN_POINT('Ctrl Pts',(-20.1607438576392,21.3365592122283,-8.29151737172421));
#42571=CARTESIAN_POINT('Ctrl Pts',(-20.0897562078698,21.3842084109399,-8.29577094960965));
#42572=CARTESIAN_POINT('Ctrl Pts',(-20.0162981861695,21.4283517444169,-8.30002452749509));
#42573=CARTESIAN_POINT('Ctrl Pts',(-19.9407536469185,21.4687301954948,-8.30427810538052));
#42574=CARTESIAN_POINT('Ctrl Pts',(-19.8666736859739,21.5083258315065,-8.30844921935847));
#42575=CARTESIAN_POINT('Ctrl Pts',(-19.7905878123472,21.5443010347693,-8.31262033333643));
#42576=CARTESIAN_POINT('Ctrl Pts',(-19.7128859499196,21.5764560442016,-8.31679144731438));
#42577=CARTESIAN_POINT('Ctrl Pts',(-19.6352101611023,21.60860026371,-8.32096116163475));
#42578=CARTESIAN_POINT('Ctrl Pts',(-19.5559198851418,21.6369266595076,-8.32513087595513));
#42579=CARTESIAN_POINT('Ctrl Pts',(-19.4754262787736,21.6612830598002,-8.3293005902755));
#42580=CARTESIAN_POINT('Ctrl Pts',(-19.3949355367132,21.6856385933876,-8.33347015621955));
#42581=CARTESIAN_POINT('Ctrl Pts',(-19.3132419899452,21.706024279931,-8.33763972216359));
#42582=CARTESIAN_POINT('Ctrl Pts',(-19.2307719418916,21.722337818325,-8.34180928810764));
#42583=CARTESIAN_POINT('Ctrl Pts',(-19.1454023486863,21.7392249206039,-8.34612545084656));
#42584=CARTESIAN_POINT('Ctrl Pts',(-19.0592011520722,21.7517480910506,-8.35044161358548));
#42585=CARTESIAN_POINT('Ctrl Pts',(-18.9726507026513,21.7598518674344,-8.35475777632439));
#42586=CARTESIAN_POINT('Ctrl Pts',(-18.8889196250168,21.7676916641549,-8.35893334051607));
#42587=CARTESIAN_POINT('Ctrl Pts',(-18.8048621716337,21.7713955951849,-8.36310890470776));
#42588=CARTESIAN_POINT('Ctrl Pts',(-18.7209165514638,21.770966566847,-8.36728446889944));
#42589=CARTESIAN_POINT('Ctrl Pts',(-18.632731037581,21.7705158693076,-8.37167093091198));
#42590=CARTESIAN_POINT('Ctrl Pts',(-18.5446695341427,21.7655037616187,-8.37605739292451));
#42591=CARTESIAN_POINT('Ctrl Pts',(-18.4572333890561,21.7559951361577,-8.38044385493705));
#42592=CARTESIAN_POINT('Ctrl Pts',(-18.3697972439695,21.7464865106968,-8.38483031694959));
#42593=CARTESIAN_POINT('Ctrl Pts',(-18.2829870179304,21.7324815349687,-8.38921677896213));
#42594=CARTESIAN_POINT('Ctrl Pts',(-18.1972887614195,21.7141062794818,-8.39360324097466));
#42595=CARTESIAN_POINT('Ctrl Pts',(-18.115527292268,21.6965751423758,-8.39778819867538));
#42596=CARTESIAN_POINT('Ctrl Pts',(-18.034473515681,21.6750011795361,-8.40197315637608));
#42597=CARTESIAN_POINT('Ctrl Pts',(-17.9545574583757,21.6494563404552,-8.40615811407679));
#42598=CARTESIAN_POINT('Ctrl Pts',(-17.8747749678507,21.6239541954464,-8.41033607729674));
#42599=CARTESIAN_POINT('Ctrl Pts',(-17.7961268504701,21.5944945081176,-8.41451404051668));
#42600=CARTESIAN_POINT('Ctrl Pts',(-17.719032145132,21.5612000454396,-8.41869200373662));
#42601=CARTESIAN_POINT('Ctrl Pts',(-17.6420120287322,21.5279377950727,-8.4228659247874));
#42602=CARTESIAN_POINT('Ctrl Pts',(-17.5665427606271,21.4908483161184,-8.42703984583817));
#42603=CARTESIAN_POINT('Ctrl Pts',(-17.4930266305614,21.4501036368029,-8.43121376688895));
#42604=CARTESIAN_POINT('Ctrl Pts',(-17.4195625033245,21.4093877788982,-8.43538473544887));
#42605=CARTESIAN_POINT('Ctrl Pts',(-17.3480491705109,21.3650220797705,-8.43955570400878));
#42606=CARTESIAN_POINT('Ctrl Pts',(-17.2788661013139,21.3172253765669,-8.4437266725687));
#42607=CARTESIAN_POINT('Ctrl Pts',(-17.2434387530277,21.2927495839925,-8.44586254710532));
#42608=CARTESIAN_POINT('Ctrl Pts',(-17.208622069414,21.267374832894,-8.44799842164195));
#42609=CARTESIAN_POINT('Ctrl Pts',(-17.1744642439897,21.2411350264762,-8.45013429617857));
#42610=CARTESIAN_POINT('Ctrl Pts',(-17.1732300852521,21.2427130357988,-7.65021347737832));
#42611=CARTESIAN_POINT('Ctrl Pts',(-16.6072658289841,20.7994054395201,-7.68605038744138));
#42612=CARTESIAN_POINT('Ctrl Pts',(-15.7765849789802,19.2885418340663,-7.76427923306491));
#42613=CARTESIAN_POINT('Ctrl Pts',(-16.9200888949879,16.787568930932,-7.88490001424893));
#42614=CARTESIAN_POINT('Ctrl Pts',(-19.7898863352068,16.3740305446598,-8.01207582093035));
#42615=CARTESIAN_POINT('Ctrl Pts',(-21.194097770004,17.9910561083639,-8.10601244625689));
#42616=CARTESIAN_POINT('Ctrl Pts',(-21.29615524784,19.0247813417565,-8.15755713602294));
#42617=CARTESIAN_POINT('Ctrl Pts',(-21.2944497293802,19.2086726977168,-8.16670989022852));
#42618=CARTESIAN_POINT('Origin',(-18.734,19.211,1.76670989022852));
#42619=CARTESIAN_POINT('',(-17.1744642439897,21.2411350264762,-6.8500446144235));
#42620=CARTESIAN_POINT('',(-17.1744642439897,21.2411350264762,-6.91673141505495));
#42621=CARTESIAN_POINT('',(-17.1744642439897,21.2411350264762,1.76670989022852));
#42622=CARTESIAN_POINT('',(-21.2936354886768,19.2104398261304,-7.43329008494697));
#42623=CARTESIAN_POINT('Ctrl Pts',(-17.1744642439897,21.2411350264762,-6.91673141505495));
#42624=CARTESIAN_POINT('Ctrl Pts',(-17.1077986986994,21.1899230133744,-6.92090111186911));
#42625=CARTESIAN_POINT('Ctrl Pts',(-17.0436335716999,21.1354047766269,-6.92507080868327));
#42626=CARTESIAN_POINT('Ctrl Pts',(-16.9823060367417,21.0778605355206,-6.92924050549743));
#42627=CARTESIAN_POINT('Ctrl Pts',(-16.9209802599973,21.020317944164,-6.93341008276956));
#42628=CARTESIAN_POINT('Ctrl Pts',(-16.8624922483838,20.9597498363999,-6.93757966004168));
#42629=CARTESIAN_POINT('Ctrl Pts',(-16.8071435285937,20.8964744550421,-6.94174923731381));
#42630=CARTESIAN_POINT('Ctrl Pts',(-16.7501679766327,20.8313392578402,-6.94604136850355));
#42631=CARTESIAN_POINT('Ctrl Pts',(-16.696519501211,20.7633355257695,-6.9503334996933));
#42632=CARTESIAN_POINT('Ctrl Pts',(-16.6464823621678,20.6928468583964,-6.95462563088304));
#42633=CARTESIAN_POINT('Ctrl Pts',(-16.5978036535748,20.6242718486381,-6.958801237391));
#42634=CARTESIAN_POINT('Ctrl Pts',(-16.5525428916109,20.5533455411254,-6.96297684389896));
#42635=CARTESIAN_POINT('Ctrl Pts',(-16.5109166558157,20.4804488744373,-6.96715245040692));
#42636=CARTESIAN_POINT('Ctrl Pts',(-16.4675479843273,20.4045008207689,-6.97150284393756));
#42637=CARTESIAN_POINT('Ctrl Pts',(-16.4281250493287,20.3264143312566,-6.9758532374682));
#42638=CARTESIAN_POINT('Ctrl Pts',(-16.392837789966,20.2466444883784,-6.98020363099883));
#42639=CARTESIAN_POINT('Ctrl Pts',(-16.3575505306033,20.1668746455003,-6.98455402452947));
#42640=CARTESIAN_POINT('Ctrl Pts',(-16.3263990771312,20.0854219954345,-6.98890441806011));
#42641=CARTESIAN_POINT('Ctrl Pts',(-16.2995147249235,20.0027584514457,-6.99325481159075));
#42642=CARTESIAN_POINT('Ctrl Pts',(-16.2736547230431,19.9232445622331,-6.9974394459838));
#42643=CARTESIAN_POINT('Ctrl Pts',(-16.251646255088,19.8423144298573,-7.00162408037684));
#42644=CARTESIAN_POINT('Ctrl Pts',(-16.233642830573,19.7603760326905,-7.00580871476989));
#42645=CARTESIAN_POINT('Ctrl Pts',(-16.2156650317043,19.6785542646903,-7.00998739285383));
#42646=CARTESIAN_POINT('Ctrl Pts',(-16.2016810508028,19.595727528011,-7.01416607093777));
#42647=CARTESIAN_POINT('Ctrl Pts',(-16.1917950137906,19.5123201090072,-7.01834474902171));
#42648=CARTESIAN_POINT('Ctrl Pts',(-16.1817317766699,19.4274176719615,-7.02259832690715));
#42649=CARTESIAN_POINT('Ctrl Pts',(-16.1759149888559,19.3419139888706,-7.02685190479258));
#42650=CARTESIAN_POINT('Ctrl Pts',(-16.1744002778054,19.256268776672,-7.03110548267802));
#42651=CARTESIAN_POINT('Ctrl Pts',(-16.1729149323844,19.1722839640348,-7.03527659665597));
#42652=CARTESIAN_POINT('Ctrl Pts',(-16.1755663524988,19.0881635420987,-7.03944771063393));
#42653=CARTESIAN_POINT('Ctrl Pts',(-16.1823546543812,19.00434562627,-7.04361882461188));
#42654=CARTESIAN_POINT('Ctrl Pts',(-16.1891406783834,18.9205558363523,-7.04778853893226));
#42655=CARTESIAN_POINT('Ctrl Pts',(-16.2000607901197,18.8370688090937,-7.05195825325263));
#42656=CARTESIAN_POINT('Ctrl Pts',(-16.2150630692561,18.7543198724111,-7.05612796757301));
#42657=CARTESIAN_POINT('Ctrl Pts',(-16.230064814547,18.671573880291,-7.06029753351705));
#42658=CARTESIAN_POINT('Ctrl Pts',(-16.2491483555176,18.5895663790282,-7.06446709946109));
#42659=CARTESIAN_POINT('Ctrl Pts',(-16.2722104781216,18.5087234519296,-7.06863666540513));
#42660=CARTESIAN_POINT('Ctrl Pts',(-16.2960834365062,18.4250381872446,-7.07295282814405));
#42661=CARTESIAN_POINT('Ctrl Pts',(-16.3242198111559,18.3426014204635,-7.07726899088297));
#42662=CARTESIAN_POINT('Ctrl Pts',(-16.3564491538596,18.2618677784329,-7.08158515362189));
#42663=CARTESIAN_POINT('Ctrl Pts',(-16.3876286291147,18.1837640262997,-7.08576071781358));
#42664=CARTESIAN_POINT('Ctrl Pts',(-16.4226382716204,18.1072545529911,-7.08993628200526));
#42665=CARTESIAN_POINT('Ctrl Pts',(-16.4612757941353,18.0327280941665,-7.09411184619694));
#42666=CARTESIAN_POINT('Ctrl Pts',(-16.5018648060604,17.9544374810765,-7.09849830820948));
#42667=CARTESIAN_POINT('Ctrl Pts',(-16.5464575227364,17.878335974976,-7.10288477022202));
#42668=CARTESIAN_POINT('Ctrl Pts',(-16.5947677080407,17.8048402647499,-7.10727123223456));
#42669=CARTESIAN_POINT('Ctrl Pts',(-16.643077893345,17.7313445545238,-7.11165769424711));
#42670=CARTESIAN_POINT('Ctrl Pts',(-16.6951051426578,17.6604550629257,-7.11604415625965));
#42671=CARTESIAN_POINT('Ctrl Pts',(-16.7505157350918,17.592546982189,-7.12043061827219));
#42672=CARTESIAN_POINT('Ctrl Pts',(-16.8033768040297,17.5277634529109,-7.12461525266524));
#42673=CARTESIAN_POINT('Ctrl Pts',(-16.8595134716063,17.4654518685826,-7.12879988705829));
#42674=CARTESIAN_POINT('Ctrl Pts',(-16.918665784363,17.4059621373673,-7.13298452145134));
#42675=CARTESIAN_POINT('Ctrl Pts',(-16.9777339011242,17.346557082421,-7.13716319953529));
#42676=CARTESIAN_POINT('Ctrl Pts',(-17.0398088154216,17.2899662258644,-7.14134187761924));
#42677=CARTESIAN_POINT('Ctrl Pts',(-17.1045901309627,17.2365067792763,-7.1455205557032));
#42678=CARTESIAN_POINT('Ctrl Pts',(-17.1705326050272,17.1820891105289,-7.14977413358863));
#42679=CARTESIAN_POINT('Ctrl Pts',(-17.2392791543357,17.1309165905525,-7.15402771147407));
#42680=CARTESIAN_POINT('Ctrl Pts',(-17.3104733397832,17.0832848292941,-7.1582812893595));
#42681=CARTESIAN_POINT('Ctrl Pts',(-17.3802872870217,17.0365765026735,-7.16245240333745));
#42682=CARTESIAN_POINT('Ctrl Pts',(-17.4524544129443,16.9932731384694,-7.1666235173154));
#42683=CARTESIAN_POINT('Ctrl Pts',(-17.5266063947422,16.9536119779749,-7.17079463129336));
#42684=CARTESIAN_POINT('Ctrl Pts',(-17.6007334941262,16.9139641261659,-7.17496434561372));
#42685=CARTESIAN_POINT('Ctrl Pts',(-17.6768437213085,16.8779562675928,-7.17913405993409));
#42686=CARTESIAN_POINT('Ctrl Pts',(-17.754542930911,16.8457803802159,-7.18330377425445));
#42687=CARTESIAN_POINT('Ctrl Pts',(-17.8322393756421,16.8136056377952,-7.18747334019848));
#42688=CARTESIAN_POINT('Ctrl Pts',(-17.9115242650151,16.7852627706774,-7.19164290614252));
#42689=CARTESIAN_POINT('Ctrl Pts',(-17.9919834625921,16.7608956229962,-7.19581247208655));
#42690=CARTESIAN_POINT('Ctrl Pts',(-18.075271506299,16.7356717564626,-7.20012863482547));
#42691=CARTESIAN_POINT('Ctrl Pts',(-18.1598174672101,16.7147085365435,-7.20444479756439));
#42692=CARTESIAN_POINT('Ctrl Pts',(-18.2451468157097,16.6981087241567,-7.20876096030332));
#42693=CARTESIAN_POINT('Ctrl Pts',(-18.3276965696568,16.6820496489125,-7.21293652449499));
#42694=CARTESIAN_POINT('Ctrl Pts',(-18.4109789843005,16.6700740910787,-7.21711208868666));
#42695=CARTESIAN_POINT('Ctrl Pts',(-18.4945577002227,16.6622223743376,-7.22128765287833));
#42696=CARTESIAN_POINT('Ctrl Pts',(-18.5823577783969,16.6539740860495,-7.22567411489088));
#42697=CARTESIAN_POINT('Ctrl Pts',(-18.6704842934721,16.6502772019506,-7.23006057690343));
#42698=CARTESIAN_POINT('Ctrl Pts',(-18.7584319418542,16.6511165885499,-7.23444703891598));
#42699=CARTESIAN_POINT('Ctrl Pts',(-18.8463795902362,16.6519559751493,-7.23883350092852));
#42700=CARTESIAN_POINT('Ctrl Pts',(-18.9341477974434,16.6573315210541,-7.24321996294107));
#42701=CARTESIAN_POINT('Ctrl Pts',(-19.0212404493958,16.6671657042506,-7.24760642495362));
#42702=CARTESIAN_POINT('Ctrl Pts',(-19.1043258393295,16.6765474021004,-7.25179105934667));
#42703=CARTESIAN_POINT('Ctrl Pts',(-19.1871057341706,16.6900213769478,-7.25597569373972));
#42704=CARTESIAN_POINT('Ctrl Pts',(-19.2691452086513,16.7075584477249,-7.26016032813276));
#42705=CARTESIAN_POINT('Ctrl Pts',(-19.3510679100948,16.7250705566525,-7.26433900621671));
#42706=CARTESIAN_POINT('Ctrl Pts',(-19.4322518385269,16.7466341786848,-7.26851768430066));
#42707=CARTESIAN_POINT('Ctrl Pts',(-19.5122676703941,16.7721684286898,-7.27269636238461));
#42708=CARTESIAN_POINT('Ctrl Pts',(-19.5937177285411,16.798160361775,-7.27694994027005));
#42709=CARTESIAN_POINT('Ctrl Pts',(-19.6739569228737,16.8282666158666,-7.28120351815548));
#42710=CARTESIAN_POINT('Ctrl Pts',(-19.7525437584805,16.8623474901424,-7.28545709604092));
#42711=CARTESIAN_POINT('Ctrl Pts',(-19.8296070349296,16.8957676401671,-7.28962821001887));
#42712=CARTESIAN_POINT('Ctrl Pts',(-19.9050810078235,16.9330094826423,-7.29379932399683));
#42713=CARTESIAN_POINT('Ctrl Pts',(-19.9785668286283,16.9738917305866,-7.29797043797478));
#42714=CARTESIAN_POINT('Ctrl Pts',(-20.0520279905562,17.0147602600976,-7.30214015229516));
#42715=CARTESIAN_POINT('Ctrl Pts',(-20.1235019236784,17.0592665455509,-7.30630986661553));
#42716=CARTESIAN_POINT('Ctrl Pts',(-20.1926138614937,17.1071830870871,-7.31047958093591));
#42717=CARTESIAN_POINT('Ctrl Pts',(-20.2617233400095,17.155097923547,-7.31464914687994));
#42718=CARTESIAN_POINT('Ctrl Pts',(-20.3284706127603,17.2064225119979,-7.31881871282398));
#42719=CARTESIAN_POINT('Ctrl Pts',(-20.3925105653945,17.2608864893358,-7.32298827876801));
#42720=CARTESIAN_POINT('Ctrl Pts',(-20.4588020837616,17.3172653529285,-7.32730444150693));
#42721=CARTESIAN_POINT('Ctrl Pts',(-20.5221919593123,17.3770081330231,-7.33162060424585));
#42722=CARTESIAN_POINT('Ctrl Pts',(-20.582336932496,17.4397714478444,-7.33593676698477));
#42723=CARTESIAN_POINT('Ctrl Pts',(-20.6405226895044,17.500490254287,-7.34011233117645));
#42724=CARTESIAN_POINT('Ctrl Pts',(-20.6956714299403,17.5640354429536,-7.34428789536813));
#42725=CARTESIAN_POINT('Ctrl Pts',(-20.7475130548915,17.6300619310734,-7.34846345955981));
#42726=CARTESIAN_POINT('Ctrl Pts',(-20.8019730770773,17.6994232601451,-7.35284992157235));
#42727=CARTESIAN_POINT('Ctrl Pts',(-20.8527827827185,17.771522659754,-7.35723638358489));
#42728=CARTESIAN_POINT('Ctrl Pts',(-20.8996813854342,17.8459270580721,-7.36162284559743));
#42729=CARTESIAN_POINT('Ctrl Pts',(-20.94657998815,17.9203314563902,-7.36600930760997));
#42730=CARTESIAN_POINT('Ctrl Pts',(-20.9895672706481,17.9970403100744,-7.37039576962251));
#42731=CARTESIAN_POINT('Ctrl Pts',(-21.0284398795321,18.0755945044995,-7.37478223163505));
#42732=CARTESIAN_POINT('Ctrl Pts',(-21.0682036058612,18.1559494788324,-7.37926924910127));
#42733=CARTESIAN_POINT('Ctrl Pts',(-21.103794382086,18.2385006465155,-7.38375626656748));
#42734=CARTESIAN_POINT('Ctrl Pts',(-21.1349820909848,18.3228080169409,-7.3882432840337));
#42735=CARTESIAN_POINT('Ctrl Pts',(-21.1660643193882,18.4068302499356,-7.39271512587973));
#42736=CARTESIAN_POINT('Ctrl Pts',(-21.1927730322953,18.4925965155768,-7.39718696772576));
#42737=CARTESIAN_POINT('Ctrl Pts',(-21.214925712994,18.5796462112212,-7.40165880957179));
#42738=CARTESIAN_POINT('Ctrl Pts',(-21.2370311427379,18.6665102326671,-7.40612111312312));
#42739=CARTESIAN_POINT('Ctrl Pts',(-21.2545997969947,18.7546518909174,-7.41058341667445));
#42740=CARTESIAN_POINT('Ctrl Pts',(-21.2674980351242,18.8435932689487,-7.41504572022578));
#42741=CARTESIAN_POINT('Ctrl Pts',(-21.2803582069864,18.9322721563795,-7.41949485428542));
#42742=CARTESIAN_POINT('Ctrl Pts',(-21.2885753721633,19.0217457093728,-7.42394398834505));
#42743=CARTESIAN_POINT('Ctrl Pts',(-21.292066600817,19.1115250494615,-7.42839312240469));
#42744=CARTESIAN_POINT('Ctrl Pts',(-21.2933474798424,19.1444637323838,-7.43002544244541));
#42745=CARTESIAN_POINT('Ctrl Pts',(-21.2939927168566,19.1774434535922,-7.43165776248613));
#42746=CARTESIAN_POINT('Ctrl Pts',(-21.2939999386838,19.2104396975212,-7.43329008252684));
#42747=CARTESIAN_POINT('Ctrl Pts',(-21.2898971261407,19.2104411453458,-7.4332901097715));
#42748=CARTESIAN_POINT('Ctrl Pts',(-21.2889976171803,19.6723917155128,-7.45617941928649));
#42749=CARTESIAN_POINT('Ctrl Pts',(-20.9482576239576,20.9911305382399,-7.52146066436197));
#42750=CARTESIAN_POINT('Ctrl Pts',(-19.0929372130342,22.083338204411,-7.61589315039638));
#42751=CARTESIAN_POINT('Ctrl Pts',(-17.6442977577302,21.5931891477782,-7.68743632691578));
#42752=CARTESIAN_POINT('Ctrl Pts',(-17.1756294998728,21.2395871765569,-7.7165875678747));
#42753=CARTESIAN_POINT('',(-21.2941234764334,19.2121301833364,-7.36670989022851));
#42754=CARTESIAN_POINT('Ctrl Pts',(-21.2976211331247,19.2121317273999,-7.36670989022851));
#42755=CARTESIAN_POINT('Ctrl Pts',(-21.2979709119767,19.2754624155768,-7.36987218932674));
#42756=CARTESIAN_POINT('Ctrl Pts',(-21.2671018166522,20.1874206516717,-7.41542642398545));
#42757=CARTESIAN_POINT('Ctrl Pts',(-20.178486706887,21.871216118483,-7.50337259420462));
#42758=CARTESIAN_POINT('Ctrl Pts',(-18.0960849586736,21.8671173941638,-7.594711490823));
#42759=CARTESIAN_POINT('Ctrl Pts',(-17.2767521278595,21.3237996192039,-7.6436584518809));
#42760=CARTESIAN_POINT('Ctrl Pts',(-17.1732300852521,21.2427130357988,-7.65021347737832));
#42761=CARTESIAN_POINT('Ctrl Pts',(-17.1744642439897,21.2411350264762,-6.8500446144235));
#42762=CARTESIAN_POINT('Ctrl Pts',(-17.1078662292582,21.189974889885,-6.85422898705064));
#42763=CARTESIAN_POINT('Ctrl Pts',(-17.0438781031357,21.1356032727387,-6.85841335967779));
#42764=CARTESIAN_POINT('Ctrl Pts',(-16.9828073053752,21.0783307543905,-6.86259773230493));
#42765=CARTESIAN_POINT('Ctrl Pts',(-16.9589891468458,21.0559939588775,-6.86422967513577));
#42766=CARTESIAN_POINT('Ctrl Pts',(-16.9356143137478,21.0332162880907,-6.86586161796661));
#42767=CARTESIAN_POINT('Ctrl Pts',(-16.9126993772538,21.0100175211999,-6.86749356079745));
#42768=CARTESIAN_POINT('Ctrl Pts',(-16.8539408046156,20.9505311495128,-6.8716781951905));
#42769=CARTESIAN_POINT('Ctrl Pts',(-16.7979903187279,20.8880523361676,-6.87586282958355));
#42770=CARTESIAN_POINT('Ctrl Pts',(-16.7451680193311,20.8228769657355,-6.88004746397659));
#42771=CARTESIAN_POINT('Ctrl Pts',(-16.6924209059395,20.7577943643761,-6.88422614206054));
#42772=CARTESIAN_POINT('Ctrl Pts',(-16.6427934219786,20.6900231841701,-6.88840482014448));
#42773=CARTESIAN_POINT('Ctrl Pts',(-16.5965688328439,20.6198960237255,-6.89258349822842));
#42774=CARTESIAN_POINT('Ctrl Pts',(-16.5495157011699,20.5485118843294,-6.89683707611386));
#42775=CARTESIAN_POINT('Ctrl Pts',(-16.5059889968458,20.4746868150557,-6.9010906539993));
#42776=CARTESIAN_POINT('Ctrl Pts',(-16.4662445138507,20.3988068256412,-6.90534423188473));
#42777=CARTESIAN_POINT('Ctrl Pts',(-16.4272705552135,20.324397917889,-6.90951534586268));
#42778=CARTESIAN_POINT('Ctrl Pts',(-16.3919336983952,20.2480134825273,-6.91368645984063));
#42779=CARTESIAN_POINT('Ctrl Pts',(-16.3604304325482,20.1700451024153,-6.91785757381858));
#42780=CARTESIAN_POINT('Ctrl Pts',(-16.3289377379264,20.0921028853463,-6.92202728813895));
#42781=CARTESIAN_POINT('Ctrl Pts',(-16.3012762516654,20.0125782052865,-6.92619700245933));
#42782=CARTESIAN_POINT('Ctrl Pts',(-16.2775946975111,19.9318834787289,-6.9303667167797));
#42783=CARTESIAN_POINT('Ctrl Pts',(-16.253913986048,19.8511916236359,-6.93453628272374));
#42784=CARTESIAN_POINT('Ctrl Pts',(-16.2342130538339,19.7693302464836,-6.93870584866779));
#42785=CARTESIAN_POINT('Ctrl Pts',(-16.2185906288469,19.6867264923413,-6.94287541461183));
#42786=CARTESIAN_POINT('Ctrl Pts',(-16.2024189386698,19.601218492106,-6.94719157735075));
#42787=CARTESIAN_POINT('Ctrl Pts',(-16.1906179905571,19.5149154578639,-6.95150774008967));
#42788=CARTESIAN_POINT('Ctrl Pts',(-16.1832392059578,19.4283001877063,-6.95582390282859));
#42789=CARTESIAN_POINT('Ctrl Pts',(-16.1761007844908,19.3445064008638,-6.95999946702027));
#42790=CARTESIAN_POINT('Ctrl Pts',(-16.1731008165489,19.2604208803107,-6.96417503121195));
#42791=CARTESIAN_POINT('Ctrl Pts',(-16.1742327266829,19.1764817953117,-6.96835059540363));
#42792=CARTESIAN_POINT('Ctrl Pts',(-16.1754218069069,19.0883031466757,-6.97273705741617));
#42793=CARTESIAN_POINT('Ctrl Pts',(-16.1811710990057,19.0002866979193,-6.97712351942871));
#42794=CARTESIAN_POINT('Ctrl Pts',(-16.1914115149699,18.9129332360151,-6.98150998144125));
#42795=CARTESIAN_POINT('Ctrl Pts',(-16.2016519309342,18.8255797741109,-6.9858964434538));
#42796=CARTESIAN_POINT('Ctrl Pts',(-16.2163832985703,18.7388898583324,-6.99028290546634));
#42797=CARTESIAN_POINT('Ctrl Pts',(-16.2354754819718,18.6533484665025,-6.99466936747888));
#42798=CARTESIAN_POINT('Ctrl Pts',(-16.2536892057137,18.5717429609135,-6.99885400187193));
#42799=CARTESIAN_POINT('Ctrl Pts',(-16.2759390634243,18.490878859979,-7.00303863626498));
#42800=CARTESIAN_POINT('Ctrl Pts',(-16.3021495269224,18.4111854736302,-7.00722327065803));
#42801=CARTESIAN_POINT('Ctrl Pts',(-16.3283226830699,18.3316055209528,-7.01140194874197));
#42802=CARTESIAN_POINT('Ctrl Pts',(-16.358445104793,18.2531934061978,-7.01558062682591));
#42803=CARTESIAN_POINT('Ctrl Pts',(-16.3923904554833,18.1763673400535,-7.01975930490986));
#42804=CARTESIAN_POINT('Ctrl Pts',(-16.4269442521885,18.0981642218874,-7.02401288279529));
#42805=CARTESIAN_POINT('Ctrl Pts',(-16.4654592728757,18.0216050420065,-7.02826646068073));
#42806=CARTESIAN_POINT('Ctrl Pts',(-16.5077494008732,17.9471138224161,-7.03252003856617));
#42807=CARTESIAN_POINT('Ctrl Pts',(-16.5492196522171,17.8740667604752,-7.03669115254412));
#42808=CARTESIAN_POINT('Ctrl Pts',(-16.5943197038781,17.8030086099539,-7.04086226652207));
#42809=CARTESIAN_POINT('Ctrl Pts',(-16.6428266524924,17.7343165435092,-7.04503338050002));
#42810=CARTESIAN_POINT('Ctrl Pts',(-16.6913173241316,17.6656475273508,-7.0492030948204));
#42811=CARTESIAN_POINT('Ctrl Pts',(-16.7432123571369,17.5993433939188,-7.05337280914077));
#42812=CARTESIAN_POINT('Ctrl Pts',(-16.798245475847,17.5357524295731,-7.05754252346114));
#42813=CARTESIAN_POINT('Ctrl Pts',(-16.8532766362426,17.4721637280668,-7.06171208940519));
#42814=CARTESIAN_POINT('Ctrl Pts',(-16.9114453586341,17.4112883509861,-7.06588165534924));
#42815=CARTESIAN_POINT('Ctrl Pts',(-16.9724459211976,17.3534405184612,-7.07005122129328));
#42816=CARTESIAN_POINT('Ctrl Pts',(-17.0355911882885,17.2935588275078,-7.0743673840322));
#42817=CARTESIAN_POINT('Ctrl Pts',(-17.1017707529441,17.2369219021168,-7.07868354677112));
#42818=CARTESIAN_POINT('Ctrl Pts',(-17.1706064918291,17.1838343090391,-7.08299970951004));
#42819=CARTESIAN_POINT('Ctrl Pts',(-17.2371999137602,17.132476038722,-7.08717527370172));
#42820=CARTESIAN_POINT('Ctrl Pts',(-17.3062787039752,17.0844396429708,-7.0913508378934));
#42821=CARTESIAN_POINT('Ctrl Pts',(-17.3774708722983,17.0399567655855,-7.09552640208508));
#42822=CARTESIAN_POINT('Ctrl Pts',(-17.4522587878001,16.9932271638116,-7.09991286409762));
#42823=CARTESIAN_POINT('Ctrl Pts',(-17.5293786750682,16.9504197742736,-7.10429932611016));
#42824=CARTESIAN_POINT('Ctrl Pts',(-17.6083720554812,16.9117475713793,-7.1086857881227));
#42825=CARTESIAN_POINT('Ctrl Pts',(-17.6873654358942,16.8730753684849,-7.11307225013524));
#42826=CARTESIAN_POINT('Ctrl Pts',(-17.7682317459862,16.8385385101709,-7.11745871214778));
#42827=CARTESIAN_POINT('Ctrl Pts',(-17.8504927560597,16.8082900820313,-7.12184517416032));
#42828=CARTESIAN_POINT('Ctrl Pts',(-17.9289688151197,16.7794334289094,-7.12602980855337));
#42829=CARTESIAN_POINT('Ctrl Pts',(-18.0090061529611,16.7543718340009,-7.13021444294642));
#42830=CARTESIAN_POINT('Ctrl Pts',(-18.0902029058994,16.733274167381,-7.13439907733947));
#42831=CARTESIAN_POINT('Ctrl Pts',(-18.17128408531,16.7122065306782,-7.13857775542341));
#42832=CARTESIAN_POINT('Ctrl Pts',(-18.2535209603945,16.6950917298573,-7.14275643350736));
#42833=CARTESIAN_POINT('Ctrl Pts',(-18.3364934985375,16.6820499053372,-7.1469351115913));
#42834=CARTESIAN_POINT('Ctrl Pts',(-18.4209532597953,16.6687743154856,-7.15118868947673));
#42835=CARTESIAN_POINT('Ctrl Pts',(-18.5061748645252,16.6597193207395,-7.15544226736217));
#42836=CARTESIAN_POINT('Ctrl Pts',(-18.5917010358989,16.654957941501,-7.1596958452476));
#42837=CARTESIAN_POINT('Ctrl Pts',(-18.67556911555,16.6502888708901,-7.16386695922556));
#42838=CARTESIAN_POINT('Ctrl Pts',(-18.7597295775162,16.6497484479464,-7.16803807320351));
#42839=CARTESIAN_POINT('Ctrl Pts',(-18.8437446259189,16.6533534026215,-7.17220918718146));
#42840=CARTESIAN_POINT('Ctrl Pts',(-18.9277314822607,16.6569571476192,-7.17637890150183));
#42841=CARTESIAN_POINT('Ctrl Pts',(-19.011572562719,16.6647034879404,-7.18054861582221));
#42842=CARTESIAN_POINT('Ctrl Pts',(-19.0948308836175,16.6765570486934,-7.18471833014258));
#42843=CARTESIAN_POINT('Ctrl Pts',(-19.1780862418278,16.6884101876458,-7.18888789608662));
#42844=CARTESIAN_POINT('Ctrl Pts',(-19.2607584263888,16.7043701907563,-7.19305746203067));
#42845=CARTESIAN_POINT('Ctrl Pts',(-19.3424177464726,16.7243500757491,-7.19722702797471));
#42846=CARTESIAN_POINT('Ctrl Pts',(-19.426948107513,16.7450324288504,-7.20154319071363));
#42847=CARTESIAN_POINT('Ctrl Pts',(-19.5103925419325,16.7700224760727,-7.20585935345255));
#42848=CARTESIAN_POINT('Ctrl Pts',(-19.5922902863025,16.799167131736,-7.21017551619147));
#42849=CARTESIAN_POINT('Ctrl Pts',(-19.6715202202639,16.8273624033065,-7.21435108038315));
#42850=CARTESIAN_POINT('Ctrl Pts',(-19.7493022661267,16.8594455439839,-7.21852664457483));
#42851=CARTESIAN_POINT('Ctrl Pts',(-19.8252402968867,16.8952291532946,-7.22270220876651));
#42852=CARTESIAN_POINT('Ctrl Pts',(-19.905013777055,16.9328201076442,-7.22708867077905));
#42853=CARTESIAN_POINT('Ctrl Pts',(-19.9827515495241,16.9744949002994,-7.23147513279159));
#42854=CARTESIAN_POINT('Ctrl Pts',(-20.058026370739,17.0199833023029,-7.23586159480413));
#42855=CARTESIAN_POINT('Ctrl Pts',(-20.1333011919539,17.0654717043064,-7.24024805681667));
#42856=CARTESIAN_POINT('Ctrl Pts',(-20.2061126241217,17.1147733273606,-7.24463451882921));
#42857=CARTESIAN_POINT('Ctrl Pts',(-20.2760730898188,17.1675689183003,-7.24902098084175));
#42858=CARTESIAN_POINT('Ctrl Pts',(-20.3421228419793,17.2174132934338,-7.25316224442401));
#42859=CARTESIAN_POINT('Ctrl Pts',(-20.4058887674611,17.270565700162,-7.25730350800627));
#42860=CARTESIAN_POINT('Ctrl Pts',(-20.4670153688585,17.3267872383141,-7.26144477158854));
#42861=CARTESIAN_POINT('Ctrl Pts',(-20.5280546973635,17.3829285067286,-7.26558012252323));
#42862=CARTESIAN_POINT('Ctrl Pts',(-20.5864618395734,17.4421298917808,-7.26971547345792));
#42863=CARTESIAN_POINT('Ctrl Pts',(-20.6419120481561,17.5041105435615,-7.27385082439261));
#42864=CARTESIAN_POINT('Ctrl Pts',(-20.6972986881793,17.5660201402308,-7.27798143452815));
#42865=CARTESIAN_POINT('Ctrl Pts',(-20.7497348173451,17.6307023247237,-7.28211204466368));
#42866=CARTESIAN_POINT('Ctrl Pts',(-20.7989315869956,17.6978385608179,-7.28624265479922));
#42867=CARTESIAN_POINT('Ctrl Pts',(-20.8480980593209,17.7649334517507,-7.29037072114094));
#42868=CARTESIAN_POINT('Ctrl Pts',(-20.8940288533085,17.8344790168689,-7.29449878748265));
#42869=CARTESIAN_POINT('Ctrl Pts',(-20.9364753744698,17.9061236744987,-7.29862685382437));
#42870=CARTESIAN_POINT('Ctrl Pts',(-20.9789091334294,17.9777467910562,-7.30275367899922));
#42871=CARTESIAN_POINT('Ctrl Pts',(-21.0178604599825,18.0514673424199,-7.30688050417407));
#42872=CARTESIAN_POINT('Ctrl Pts',(-21.0531249145872,18.1269060785426,-7.31100732934892));
#42873=CARTESIAN_POINT('Ctrl Pts',(-21.0883898804923,18.2023459084539,-7.31513421435873));
#42874=CARTESIAN_POINT('Ctrl Pts',(-21.1199676712092,18.2795035453347,-7.31926109936855));
#42875=CARTESIAN_POINT('Ctrl Pts',(-21.147701166054,18.3579779129534,-7.32338798437837));
#42876=CARTESIAN_POINT('Ctrl Pts',(-21.175460263615,18.4365247257135,-7.32751867920249));
#42877=CARTESIAN_POINT('Ctrl Pts',(-21.1993678247307,18.5163902510463,-7.33164937402661));
#42878=CARTESIAN_POINT('Ctrl Pts',(-21.2193162430201,18.5971570459961,-7.33578006885072));
#42879=CARTESIAN_POINT('Ctrl Pts',(-21.2392749611598,18.6779655427927,-7.33991289645234));
#42880=CARTESIAN_POINT('Ctrl Pts',(-21.2552703785523,18.7596757735081,-7.34404572405396));
#42881=CARTESIAN_POINT('Ctrl Pts',(-21.267246258349,18.8418612800574,-7.34817855165558));
#42882=CARTESIAN_POINT('Ctrl Pts',(-21.2792406903518,18.9241741027191,-7.35231778154839));
#42883=CARTESIAN_POINT('Ctrl Pts',(-21.2872031132021,19.0069632027568,-7.35645701144119));
#42884=CARTESIAN_POINT('Ctrl Pts',(-21.291129302603,19.0897988045891,-7.360596241334));
#42885=CARTESIAN_POINT('Ctrl Pts',(-21.2930622985235,19.1305815748695,-7.36263412429883));
#42886=CARTESIAN_POINT('Ctrl Pts',(-21.2940177418851,19.1713756409973,-7.36467200726367));
#42887=CARTESIAN_POINT('Ctrl Pts',(-21.2939997505486,19.2121301287168,-7.36670989022851));
#42888=CARTESIAN_POINT('Origin',(-18.734,19.211,1.76670989022852));
#42889=CARTESIAN_POINT('',(-17.1744642439897,21.2411350264762,-6.05008447538599));
#42890=CARTESIAN_POINT('',(-17.1725993531626,21.24352550386,-6.11677129344295));
#42891=CARTESIAN_POINT('',(-17.1744642439897,21.2411350264762,1.76670989022852));
#42892=CARTESIAN_POINT('',(-21.2939991231355,19.208881145288,-6.6332901097715));
#42893=CARTESIAN_POINT('Ctrl Pts',(-17.1725993531626,21.24352550386,-6.11677129344295));
#42894=CARTESIAN_POINT('Ctrl Pts',(-16.5753465248139,20.7772931197068,-6.15458085279602));
#42895=CARTESIAN_POINT('Ctrl Pts',(-15.7555914125513,19.1915608045691,-6.23478234770956));
#42896=CARTESIAN_POINT('Ctrl Pts',(-17.0342063027576,16.7062059673629,-6.35737577818358));
#42897=CARTESIAN_POINT('Ctrl Pts',(-19.9200693000182,16.4259449961135,-6.48455158486501));
#42898=CARTESIAN_POINT('Ctrl Pts',(-21.2201493011995,18.0710819511262,-6.57652302872765));
#42899=CARTESIAN_POINT('Ctrl Pts',(-21.2969229188781,19.0646440605456,-6.62610253702981));
#42900=CARTESIAN_POINT('Ctrl Pts',(-21.2956375040978,19.2088797892363,-6.6332901097715));
#42901=CARTESIAN_POINT('Ctrl Pts',(-21.2939991231355,19.208881145288,-6.6332901097715));
#42902=CARTESIAN_POINT('Ctrl Pts',(-21.2940674480299,19.2914312459012,-6.63740642252224));
#42903=CARTESIAN_POINT('Ctrl Pts',(-21.2901386830331,19.374124140816,-6.64152273527298));
#42904=CARTESIAN_POINT('Ctrl Pts',(-21.2821979940262,19.4565340775554,-6.64563904802373));
#42905=CARTESIAN_POINT('Ctrl Pts',(-21.2742662779566,19.5388508914942,-6.64975070936244));
#42906=CARTESIAN_POINT('Ctrl Pts',(-21.2623316869624,19.6208849121509,-6.65386237070115));
#42907=CARTESIAN_POINT('Ctrl Pts',(-21.2464314307688,19.7022110602224,-6.65797403203986));
#42908=CARTESIAN_POINT('Ctrl Pts',(-21.2305407999847,19.7834879765415,-6.66208320433541));
#42909=CARTESIAN_POINT('Ctrl Pts',(-21.2106893569246,19.864057405363,-6.66619237663095));
#42910=CARTESIAN_POINT('Ctrl Pts',(-21.1869659077107,19.9435013690152,-6.6703015489265));
#42911=CARTESIAN_POINT('Ctrl Pts',(-21.1632492097461,20.0229227244029,-6.67440955182855));
#42912=CARTESIAN_POINT('Ctrl Pts',(-21.1356628286736,20.1012187954781,-6.6785175547306));
#42913=CARTESIAN_POINT('Ctrl Pts',(-21.1043458531985,20.1779852823206,-6.68262555763265));
#42914=CARTESIAN_POINT('Ctrl Pts',(-21.0730277445931,20.2547545467759,-6.68673370917301));
#42915=CARTESIAN_POINT('Ctrl Pts',(-21.0379789552761,20.3299936782021,-6.69084186071338));
#42916=CARTESIAN_POINT('Ctrl Pts',(-20.9993866849092,20.4033184003596,-6.69495001225374));
#42917=CARTESIAN_POINT('Ctrl Pts',(-20.960756173379,20.4767157801412,-6.69906223457026));
#42918=CARTESIAN_POINT('Ctrl Pts',(-20.9185753946449,20.5481945435132,-6.70317445688679));
#42919=CARTESIAN_POINT('Ctrl Pts',(-20.8730771242595,20.6173957680787,-6.70728667920331));
#42920=CARTESIAN_POINT('Ctrl Pts',(-20.8275541489316,20.6866345679687,-6.71140113440066));
#42921=CARTESIAN_POINT('Ctrl Pts',(-20.7787103793541,20.7535929860942,-6.71551558959801));
#42922=CARTESIAN_POINT('Ctrl Pts',(-20.7268199445205,20.8179438909686,-6.71963004479536));
#42923=CARTESIAN_POINT('Ctrl Pts',(-20.6748438133911,20.8824010704232,-6.72375129495542));
#42924=CARTESIAN_POINT('Ctrl Pts',(-20.6198112918951,20.9442417891335,-6.72787254511548));
#42925=CARTESIAN_POINT('Ctrl Pts',(-20.5620341095488,21.003175017772,-6.73199379527554));
#42926=CARTESIAN_POINT('Ctrl Pts',(-20.5297457003867,21.0361094760174,-6.73429692959298));
#42927=CARTESIAN_POINT('Ctrl Pts',(-20.4966007367166,21.0681366118251,-6.73660006391043));
#42928=CARTESIAN_POINT('Ctrl Pts',(-20.4626578964191,21.0992112903878,-6.73890319822788));
#42929=CARTESIAN_POINT('Ctrl Pts',(-20.400986123379,21.1556718136325,-6.74308783262093));
#42930=CARTESIAN_POINT('Ctrl Pts',(-20.3364305466715,21.2092127933027,-6.74727246701397));
#42931=CARTESIAN_POINT('Ctrl Pts',(-20.2692989765722,21.2595255801518,-6.75145710140702));
#42932=CARTESIAN_POINT('Ctrl Pts',(-20.2022629599537,21.3097667529763,-6.75563577949096));
#42933=CARTESIAN_POINT('Ctrl Pts',(-20.1326585979524,21.3567885864284,-6.75981445757491));
#42934=CARTESIAN_POINT('Ctrl Pts',(-20.0608289916762,21.4003206313483,-6.76399313565885));
#42935=CARTESIAN_POINT('Ctrl Pts',(-19.9877118913305,21.4446329568875,-6.76824671354429));
#42936=CARTESIAN_POINT('Ctrl Pts',(-19.9122893426569,21.4853288288423,-6.77250029142972));
#42937=CARTESIAN_POINT('Ctrl Pts',(-19.8349567777299,21.5221672751167,-6.77675386931516));
#42938=CARTESIAN_POINT('Ctrl Pts',(-19.7591234554761,21.5582915362258,-6.78092498329311));
#42939=CARTESIAN_POINT('Ctrl Pts',(-19.6814539493099,21.5907063974351,-6.78509609727106));
#42940=CARTESIAN_POINT('Ctrl Pts',(-19.6023470115176,21.6192303601583,-6.78926721124902));
#42941=CARTESIAN_POINT('Ctrl Pts',(-19.5232666188222,21.6477447513905,-6.79343692556939));
#42942=CARTESIAN_POINT('Ctrl Pts',(-19.4427501848434,21.6723706812233,-6.79760663988977));
#42943=CARTESIAN_POINT('Ctrl Pts',(-19.3612154692014,21.6929751721551,-6.80177635421015));
#42944=CARTESIAN_POINT('Ctrl Pts',(-19.2796836549145,21.7135789298907,-6.80594592015419));
#42945=CARTESIAN_POINT('Ctrl Pts',(-19.1971340772291,21.7301614213603,-6.81011548609823));
#42946=CARTESIAN_POINT('Ctrl Pts',(-19.1139973178552,21.7426401873929,-6.81428505204228));
#42947=CARTESIAN_POINT('Ctrl Pts',(-19.027937572582,21.755557691445,-6.8186012147812));
#42948=CARTESIAN_POINT('Ctrl Pts',(-18.941249108334,21.7640774486062,-6.82291737752012));
#42949=CARTESIAN_POINT('Ctrl Pts',(-18.8544163259003,21.7681663826307,-6.82723354025904));
#42950=CARTESIAN_POINT('Ctrl Pts',(-18.7704121122212,21.7721221200595,-6.83140910445072));
#42951=CARTESIAN_POINT('Ctrl Pts',(-18.6862733092299,21.7719313177434,-6.8355846686424));
#42952=CARTESIAN_POINT('Ctrl Pts',(-18.6024375216844,21.7676171622477,-6.83976023283408));
#42953=CARTESIAN_POINT('Ctrl Pts',(-18.5143673878106,21.7630851090138,-6.84414669484662));
#42954=CARTESIAN_POINT('Ctrl Pts',(-18.4266322652435,21.7540022746856,-6.84853315685916));
#42955=CARTESIAN_POINT('Ctrl Pts',(-18.3397299608672,21.7404566879554,-6.8529196188717));
#42956=CARTESIAN_POINT('Ctrl Pts',(-18.252827656491,21.7269111012251,-6.85730608088424));
#42957=CARTESIAN_POINT('Ctrl Pts',(-18.1667587226472,21.7089029553708,-6.86169254289678));
#42958=CARTESIAN_POINT('Ctrl Pts',(-18.0820028534405,21.6865806835727,-6.86607900490932));
#42959=CARTESIAN_POINT('Ctrl Pts',(-18.0004434053584,21.6651002576761,-6.87030003908812));
#42960=CARTESIAN_POINT('Ctrl Pts',(-17.9197935149738,21.6395446599541,-6.87452107326693));
#42961=CARTESIAN_POINT('Ctrl Pts',(-17.8404904983898,21.610008288967,-6.87874210744573));
#42962=CARTESIAN_POINT('Ctrl Pts',(-17.7619934286695,21.5807720925077,-6.88292024377014));
#42963=CARTESIAN_POINT('Ctrl Pts',(-17.6848164352552,21.5476357908569,-6.88709838009456));
#42964=CARTESIAN_POINT('Ctrl Pts',(-17.6093723503702,21.5107418658815,-6.89127651641897));
#42965=CARTESIAN_POINT('Ctrl Pts',(-17.5327663637006,21.4732797437129,-6.89551899952497));
#42966=CARTESIAN_POINT('Ctrl Pts',(-17.457947583422,21.4319433870403,-6.89976148263096));
#42967=CARTESIAN_POINT('Ctrl Pts',(-17.385329256641,21.3869336446701,-6.90400396573696));
#42968=CARTESIAN_POINT('Ctrl Pts',(-17.3127109298599,21.3419239022999,-6.90824644884295));
#42969=CARTESIAN_POINT('Ctrl Pts',(-17.2422935040658,21.2932409972677,-6.91248893194895));
#42970=CARTESIAN_POINT('Ctrl Pts',(-17.1744642439897,21.2411350264762,-6.91673141505495));
#42971=CARTESIAN_POINT('',(-21.293999428374,19.2127107672549,-6.5667098902584));
#42972=CARTESIAN_POINT('Ctrl Pts',(-21.293999428374,19.2127107672549,-6.5667098902584));
#42973=CARTESIAN_POINT('Ctrl Pts',(-21.2939356382109,19.308166639887,-6.57143929947813));
#42974=CARTESIAN_POINT('Ctrl Pts',(-21.2885288437516,19.4034153336882,-6.57616870869786));
#42975=CARTESIAN_POINT('Ctrl Pts',(-21.2778724975471,19.4979019278834,-6.5808981179176));
#42976=CARTESIAN_POINT('Ctrl Pts',(-21.2671635859907,19.5928546031339,-6.58565085624617));
#42977=CARTESIAN_POINT('Ctrl Pts',(-21.2511533349013,19.6870374428281,-6.59040359457474));
#42978=CARTESIAN_POINT('Ctrl Pts',(-21.2299860493109,19.7799056526747,-6.59515633290331));
#42979=CARTESIAN_POINT('Ctrl Pts',(-21.2086961910765,19.8733116311444,-6.59993659274384));
#42980=CARTESIAN_POINT('Ctrl Pts',(-21.1821895164634,19.965387517667,-6.60471685258437));
#42981=CARTESIAN_POINT('Ctrl Pts',(-21.15066091743,20.055600503295,-6.60949711242489));
#42982=CARTESIAN_POINT('Ctrl Pts',(-21.1426476472037,20.0785289255507,-6.61071205742812));
#42983=CARTESIAN_POINT('Ctrl Pts',(-21.134310213157,20.1013371264666,-6.61192700243135));
#42984=CARTESIAN_POINT('Ctrl Pts',(-21.1256522921827,20.1240166007786,-6.61314194743458));
#42985=CARTESIAN_POINT('Ctrl Pts',(-21.0958318198279,20.2021315014283,-6.61732658182763));
#42986=CARTESIAN_POINT('Ctrl Pts',(-21.062124806143,20.2789292632222,-6.62151121622068));
#42987=CARTESIAN_POINT('Ctrl Pts',(-21.0246680532229,20.3539960060928,-6.62569585061373));
#42988=CARTESIAN_POINT('Ctrl Pts',(-20.9872646153543,20.4289559007464,-6.62987452869768));
#42989=CARTESIAN_POINT('Ctrl Pts',(-20.9461222434274,20.5021892624269,-6.63405320678162));
#42990=CARTESIAN_POINT('Ctrl Pts',(-20.9014264094923,20.5733005393213,-6.63823188486556));
#42991=CARTESIAN_POINT('Ctrl Pts',(-20.8559294348563,20.6456864347473,-6.642485462751));
#42992=CARTESIAN_POINT('Ctrl Pts',(-20.8067505255349,20.715872969927,-6.64673904063643));
#42993=CARTESIAN_POINT('Ctrl Pts',(-20.7541351457545,20.7834674854786,-6.65099261852187));
#42994=CARTESIAN_POINT('Ctrl Pts',(-20.7025398177816,20.8497515494465,-6.65516373249982));
#42995=CARTESIAN_POINT('Ctrl Pts',(-20.6476403712487,20.9135428198972,-6.65933484647777));
#42996=CARTESIAN_POINT('Ctrl Pts',(-20.5897118973506,20.9745003130228,-6.66350596045573));
#42997=CARTESIAN_POINT('Ctrl Pts',(-20.5318028619114,21.0354373512728,-6.6676756747761));
#42998=CARTESIAN_POINT('Ctrl Pts',(-20.4708671343699,21.0935421675084,-6.67184538909647));
#42999=CARTESIAN_POINT('Ctrl Pts',(-20.4072185463108,21.1485086312792,-6.67601510341685));
#43000=CARTESIAN_POINT('Ctrl Pts',(-20.3435722231416,21.2034731391074,-6.6801846693609));
#43001=CARTESIAN_POINT('Ctrl Pts',(-20.2772135801197,21.2552992164786,-6.68435423530495));
#43002=CARTESIAN_POINT('Ctrl Pts',(-20.2084905554454,21.3037201441909,-6.688523801249));
#43003=CARTESIAN_POINT('Ctrl Pts',(-20.1373513140027,21.3538434919878,-6.69283996398792));
#43004=CARTESIAN_POINT('Ctrl Pts',(-20.0636787652558,21.4003174810234,-6.69715612672683));
#43005=CARTESIAN_POINT('Ctrl Pts',(-19.9878910926204,21.4428954114938,-6.70147228946575));
#43006=CARTESIAN_POINT('Ctrl Pts',(-19.9145721954497,21.4840863703576,-6.70564785365743));
#43007=CARTESIAN_POINT('Ctrl Pts',(-19.8392743011541,21.5216310329473,-6.70982341784911));
#43008=CARTESIAN_POINT('Ctrl Pts',(-19.7623989816004,21.555353969571,-6.71399898204078));
#43009=CARTESIAN_POINT('Ctrl Pts',(-19.6816408724098,21.5907801715548,-6.71838544405332));
#43010=CARTESIAN_POINT('Ctrl Pts',(-19.5991423447412,21.6219882241026,-6.72277190606586));
#43011=CARTESIAN_POINT('Ctrl Pts',(-19.5153878511232,21.6488336748263,-6.7271583680784));
#43012=CARTESIAN_POINT('Ctrl Pts',(-19.4316333575052,21.67567912555,-6.73154483009094));
#43013=CARTESIAN_POINT('Ctrl Pts',(-19.3466234783173,21.6981618996353,-6.73593129210348));
#43014=CARTESIAN_POINT('Ctrl Pts',(-19.26085355124,21.7161996598167,-6.74031775411602));
#43015=CARTESIAN_POINT('Ctrl Pts',(-19.1790221317784,21.7334091360265,-6.7445027922189));
#43016=CARTESIAN_POINT('Ctrl Pts',(-19.0961943140709,21.746636934806,-6.74868783032178));
#43017=CARTESIAN_POINT('Ctrl Pts',(-19.0127922770448,21.7557740304907,-6.75287286842467));
#43018=CARTESIAN_POINT('Ctrl Pts',(-18.929533501023,21.764895431241,-6.75705071782109));
#43019=CARTESIAN_POINT('Ctrl Pts',(-18.8457029204263,21.7699400516436,-6.76122856721752));
#43020=CARTESIAN_POINT('Ctrl Pts',(-18.7617332667266,21.7708497740916,-6.76540641661395));
#43021=CARTESIAN_POINT('Ctrl Pts',(-18.6778456877578,21.7717586073466,-6.76958018244149));
#43022=CARTESIAN_POINT('Ctrl Pts',(-18.5938197628326,21.7685405617453,-6.77375394826903));
#43023=CARTESIAN_POINT('Ctrl Pts',(-18.5100929256421,21.7611893306287,-6.77792771409658));
#43024=CARTESIAN_POINT('Ctrl Pts',(-18.4264228070226,21.7538430794126,-6.78209865251488));
#43025=CARTESIAN_POINT('Ctrl Pts',(-18.3430518306229,21.7423692437081,-6.78626959093317));
#43026=CARTESIAN_POINT('Ctrl Pts',(-18.2604156415009,21.7268135573577,-6.79044052935147));
#43027=CARTESIAN_POINT('Ctrl Pts',(-18.1778106423785,21.7112637423073,-6.79460989350105));
#43028=CARTESIAN_POINT('Ctrl Pts',(-18.095940330876,21.6916352235908,-6.79877925765063));
#43029=CARTESIAN_POINT('Ctrl Pts',(-18.0152320947977,21.668025172531,-6.8029486218002));
#43030=CARTESIAN_POINT('Ctrl Pts',(-17.9344957178936,21.6444068892713,-6.80711943969671));
#43031=CARTESIAN_POINT('Ctrl Pts',(-17.8549226701451,21.6168044215289,-6.81129025759322));
#43032=CARTESIAN_POINT('Ctrl Pts',(-17.7769262677244,21.5853651511484,-6.81546107548973));
#43033=CARTESIAN_POINT('Ctrl Pts',(-17.6989179895601,21.5539210938201,-6.81963252843557));
#43034=CARTESIAN_POINT('Ctrl Pts',(-17.6224872571105,21.5186392540143,-6.82380398138141));
#43035=CARTESIAN_POINT('Ctrl Pts',(-17.5480265683683,21.4797148387278,-6.82797543432725));
#43036=CARTESIAN_POINT('Ctrl Pts',(-17.4734822892922,21.4407467264929,-6.83215157018901));
#43037=CARTESIAN_POINT('Ctrl Pts',(-17.4009128736038,21.3981280959147,-6.83632770605077));
#43038=CARTESIAN_POINT('Ctrl Pts',(-17.3306849632431,21.3520994623352,-6.84050384191253));
#43039=CARTESIAN_POINT('Ctrl Pts',(-17.2772042226053,21.3170472245321,-6.84368409941619));
#43040=CARTESIAN_POINT('Ctrl Pts',(-17.2250808728016,21.2800183723873,-6.84686435691984));
#43041=CARTESIAN_POINT('Ctrl Pts',(-17.1744642439897,21.2411350264762,-6.8500446144235));
#43042=CARTESIAN_POINT('Ctrl Pts',(-17.1744642439897,21.2411350264762,-6.05008447538598));
#43043=CARTESIAN_POINT('Ctrl Pts',(-17.1077758011212,21.1899054236124,-6.05425481627113));
#43044=CARTESIAN_POINT('Ctrl Pts',(-17.0436322849344,21.1354002166438,-6.05842515715628));
#43045=CARTESIAN_POINT('Ctrl Pts',(-16.9823603368735,21.0779114843939,-6.06259549804143));
#43046=CARTESIAN_POINT('Ctrl Pts',(-16.9210197564991,21.0203583575097,-6.06677051023461));
#43047=CARTESIAN_POINT('Ctrl Pts',(-16.8625574985143,20.9598153519561,-6.07094552242779));
#43048=CARTESIAN_POINT('Ctrl Pts',(-16.8072633791422,20.8966114599294,-6.07512053462096));
#43049=CARTESIAN_POINT('Ctrl Pts',(-16.7519330537637,20.8333661826606,-6.0792982805681));
#43050=CARTESIAN_POINT('Ctrl Pts',(-16.6997752805568,20.767456911828,-6.08347602651524));
#43051=CARTESIAN_POINT('Ctrl Pts',(-16.6510381296659,20.6992438801266,-6.08765377246238));
#43052=CARTESIAN_POINT('Ctrl Pts',(-16.6022223963696,20.6309208636598,-6.09183825448907));
#43053=CARTESIAN_POINT('Ctrl Pts',(-16.5568385388414,20.5602870604179,-6.09602273651575));
#43054=CARTESIAN_POINT('Ctrl Pts',(-16.5150897902318,20.4877292120832,-6.10020721854244));
#43055=CARTESIAN_POINT('Ctrl Pts',(-16.5010171667419,20.4632714902385,-6.10161771926458));
#43056=CARTESIAN_POINT('Ctrl Pts',(-16.4873571727183,20.4385953340331,-6.10302821998671));
#43057=CARTESIAN_POINT('Ctrl Pts',(-16.4741163568267,20.4137160593082,-6.10443872070885));
#43058=CARTESIAN_POINT('Ctrl Pts',(-16.4348338717473,20.3399049175952,-6.1086233551019));
#43059=CARTESIAN_POINT('Ctrl Pts',(-16.3990982578627,20.2640298565514,-6.11280798949495));
#43060=CARTESIAN_POINT('Ctrl Pts',(-16.3671315774457,20.1864659759906,-6.116992623888));
#43061=CARTESIAN_POINT('Ctrl Pts',(-16.3352103976415,20.1090124980131,-6.12117130197196));
#43062=CARTESIAN_POINT('Ctrl Pts',(-16.3070476692931,20.0298753969617,-6.12534998005591));
#43063=CARTESIAN_POINT('Ctrl Pts',(-16.2828196558214,19.949454413158,-6.12952865813987));
#43064=CARTESIAN_POINT('Ctrl Pts',(-16.2581573726207,19.8675919410174,-6.1337822360253));
#43065=CARTESIAN_POINT('Ctrl Pts',(-16.2375724777941,19.7843995318231,-6.13803581391074));
#43066=CARTESIAN_POINT('Ctrl Pts',(-16.2211996301976,19.7003202443399,-6.14228939179617));
#43067=CARTESIAN_POINT('Ctrl Pts',(-16.2051442022007,19.6178709979118,-6.14646050577412));
#43068=CARTESIAN_POINT('Ctrl Pts',(-16.1931390533221,19.5345694264037,-6.15063161975207));
#43069=CARTESIAN_POINT('Ctrl Pts',(-16.18526042222,19.4508469609104,-6.15480273373002));
#43070=CARTESIAN_POINT('Ctrl Pts',(-16.1773844348688,19.367152589299,-6.1589724480504));
#43071=CARTESIAN_POINT('Ctrl Pts',(-16.1736322583368,19.2830380618256,-6.16314216237078));
#43072=CARTESIAN_POINT('Ctrl Pts',(-16.1740284019004,19.1989411060445,-6.16731187669115));
#43073=CARTESIAN_POINT('Ctrl Pts',(-16.1744245313676,19.114847142794,-6.17148144263519));
#43074=CARTESIAN_POINT('Ctrl Pts',(-16.1789686844147,19.0307712100162,-6.17565100857924));
#43075=CARTESIAN_POINT('Ctrl Pts',(-16.187633250542,18.9471508437487,-6.17982057452328));
#43076=CARTESIAN_POINT('Ctrl Pts',(-16.1966024521254,18.8605904885601,-6.1841367372622));
#43077=CARTESIAN_POINT('Ctrl Pts',(-16.2099871509034,18.7745188559838,-6.18845290000111));
#43078=CARTESIAN_POINT('Ctrl Pts',(-16.2276984844483,18.6894132736129,-6.19276906274003));
#43079=CARTESIAN_POINT('Ctrl Pts',(-16.2448328731659,18.6070799966362,-6.19694462693171));
#43080=CARTESIAN_POINT('Ctrl Pts',(-16.2660161808879,18.5256512422045,-6.20112019112339));
#43081=CARTESIAN_POINT('Ctrl Pts',(-16.291116741615,18.4455449811371,-6.20529575531507));
#43082=CARTESIAN_POINT('Ctrl Pts',(-16.3174850719936,18.3613927432578,-6.20968221732761));
#43083=CARTESIAN_POINT('Ctrl Pts',(-16.3481765728437,18.2787006554449,-6.21406867934014));
#43084=CARTESIAN_POINT('Ctrl Pts',(-16.3829817631983,18.1979288029829,-6.21845514135268));
#43085=CARTESIAN_POINT('Ctrl Pts',(-16.4177869535528,18.117156950521,-6.22284160336521));
#43086=CARTESIAN_POINT('Ctrl Pts',(-16.4567055084016,18.0383058200372,-6.22722806537775));
#43087=CARTESIAN_POINT('Ctrl Pts',(-16.4994739740983,17.9618028820207,-6.23161452739028));
#43088=CARTESIAN_POINT('Ctrl Pts',(-16.5402745992903,17.8888199575868,-6.23579916178333));
#43089=CARTESIAN_POINT('Ctrl Pts',(-16.5847305081231,17.8177022301347,-6.23998379617638));
#43090=CARTESIAN_POINT('Ctrl Pts',(-16.6326464991108,17.7488394533087,-6.24416843056943));
#43091=CARTESIAN_POINT('Ctrl Pts',(-16.6804942876163,17.6800746941218,-6.24834710865338));
#43092=CARTESIAN_POINT('Ctrl Pts',(-16.7317921151762,17.6135588845839,-6.25252578673734));
#43093=CARTESIAN_POINT('Ctrl Pts',(-16.7862992714868,17.5496566061921,-6.2567044648213));
#43094=CARTESIAN_POINT('Ctrl Pts',(-16.8417834294006,17.4846089253861,-6.26095804270673));
#43095=CARTESIAN_POINT('Ctrl Pts',(-16.9005928669026,17.4222698132391,-6.26521162059216));
#43096=CARTESIAN_POINT('Ctrl Pts',(-16.9624279299719,17.3629923158449,-6.2694651984776));
#43097=CARTESIAN_POINT('Ctrl Pts',(-17.0230641996824,17.3048640284082,-6.27363631245555));
#43098=CARTESIAN_POINT('Ctrl Pts',(-17.0866094791688,17.2496800373392,-6.2778074264335));
#43099=CARTESIAN_POINT('Ctrl Pts',(-17.1527422696958,17.1977379727534,-6.28197854041145));
#43100=CARTESIAN_POINT('Ctrl Pts',(-17.2188528687262,17.145813337829,-6.28614825473182));
#43101=CARTESIAN_POINT('Ctrl Pts',(-17.2875488929276,17.0971287527973,-6.2903179690522));
#43102=CARTESIAN_POINT('Ctrl Pts',(-17.3584755491053,17.0519417597039,-6.29448768337257));
#43103=CARTESIAN_POINT('Ctrl Pts',(-17.429399681408,17.0067563745576,-6.29865724931661));
#43104=CARTESIAN_POINT('Ctrl Pts',(-17.5025538994269,16.965068580356,-6.30282681526065));
#43105=CARTESIAN_POINT('Ctrl Pts',(-17.5775553595561,16.9270919909969,-6.30699638120468));
#43106=CARTESIAN_POINT('Ctrl Pts',(-17.6551937784993,16.887780191605,-6.3113125439436));
#43107=CARTESIAN_POINT('Ctrl Pts',(-17.7348112839525,16.8524456628668,-6.31562870668252));
#43108=CARTESIAN_POINT('Ctrl Pts',(-17.8159584194019,16.8212720539164,-6.31994486942144));
#43109=CARTESIAN_POINT('Ctrl Pts',(-17.8944621954492,16.7911139219987,-6.32412043361312));
#43110=CARTESIAN_POINT('Ctrl Pts',(-17.9743970142431,16.7648498911064,-6.3282959978048));
#43111=CARTESIAN_POINT('Ctrl Pts',(-18.055340160162,16.7425954906477,-6.33247156199648));
#43112=CARTESIAN_POINT('Ctrl Pts',(-18.1403715519571,16.7192170733266,-6.33685802400902));
#43113=CARTESIAN_POINT('Ctrl Pts',(-18.2265152388011,16.7002641097526,-6.34124448602156));
#43114=CARTESIAN_POINT('Ctrl Pts',(-18.3132709737052,16.6858094950216,-6.3456309480341));
#43115=CARTESIAN_POINT('Ctrl Pts',(-18.4000267086093,16.6713548802907,-6.35001741004664));
#43116=CARTESIAN_POINT('Ctrl Pts',(-18.4873939064752,16.6613986045227,-6.35440387205918));
#43117=CARTESIAN_POINT('Ctrl Pts',(-18.5748705298082,16.6559505265619,-6.35879033407172));
#43118=CARTESIAN_POINT('Ctrl Pts',(-18.6583222240303,16.650753122744,-6.36297496846477));
#43119=CARTESIAN_POINT('Ctrl Pts',(-18.7421841184714,16.6496388297569,-6.36715960285782));
#43120=CARTESIAN_POINT('Ctrl Pts',(-18.8260228331344,16.6526544802975,-6.37134423725087));
#43121=CARTESIAN_POINT('Ctrl Pts',(-18.909742213764,16.6556658384328,-6.3755229153348));
#43122=CARTESIAN_POINT('Ctrl Pts',(-18.9934380243477,16.6627954472227,-6.37970159341873));
#43123=CARTESIAN_POINT('Ctrl Pts',(-19.0766734176208,16.6740382484444,-6.38388027150266));
#43124=CARTESIAN_POINT('Ctrl Pts',(-19.1614007454985,16.685482568798,-6.38813384938809));
#43125=CARTESIAN_POINT('Ctrl Pts',(-19.2456505065464,16.7011890198916,-6.39238742727353));
#43126=CARTESIAN_POINT('Ctrl Pts',(-19.3289636478323,16.7210967372691,-6.39664100515897));
#43127=CARTESIAN_POINT('Ctrl Pts',(-19.4106616013021,16.7406185046985,-6.40081211913691));
#43128=CARTESIAN_POINT('Ctrl Pts',(-19.4914584592896,16.7641799807696,-6.40498323311487));
#43129=CARTESIAN_POINT('Ctrl Pts',(-19.570929940801,16.7916719374606,-6.40915434709281));
#43130=CARTESIAN_POINT('Ctrl Pts',(-19.6503747548893,16.81915466896,-6.41332406141319));
#43131=CARTESIAN_POINT('Ctrl Pts',(-19.7284946413755,16.8505651114304,-6.41749377573357));
#43132=CARTESIAN_POINT('Ctrl Pts',(-19.804881005329,16.8857443425667,-6.42166349005394));
#43133=CARTESIAN_POINT('Ctrl Pts',(-19.8812646511277,16.920922321875,-6.42583305599798));
#43134=CARTESIAN_POINT('Ctrl Pts',(-19.9559144795488,16.959868629993,-6.43000262194201));
#43135=CARTESIAN_POINT('Ctrl Pts',(-20.028443649127,17.0023769811861,-6.43417218788604));
#43136=CARTESIAN_POINT('Ctrl Pts',(-20.1035228548334,17.0463798735676,-6.43848835062497));
#43137=CARTESIAN_POINT('Ctrl Pts',(-20.1763290473284,17.0941996856767,-6.44280451336389));
#43138=CARTESIAN_POINT('Ctrl Pts',(-20.2464645244668,17.1455579015065,-6.44712067610282));
#43139=CARTESIAN_POINT('Ctrl Pts',(-20.3143153458142,17.1952431288574,-6.45129624029449));
#43140=CARTESIAN_POINT('Ctrl Pts',(-20.379666440751,17.2482394397184,-6.45547180448617));
#43141=CARTESIAN_POINT('Ctrl Pts',(-20.4421918593792,17.3042539310253,-6.45964736867784));
#43142=CARTESIAN_POINT('Ctrl Pts',(-20.5078752882625,17.3630975811265,-6.46403383069039));
#43143=CARTESIAN_POINT('Ctrl Pts',(-20.5704396751013,17.4252719095171,-6.46842029270294));
#43144=CARTESIAN_POINT('Ctrl Pts',(-20.6295529524488,17.4903957443785,-6.47280675471549));
#43145=CARTESIAN_POINT('Ctrl Pts',(-20.6886662297962,17.5555195792399,-6.47719321672804));
#43146=CARTESIAN_POINT('Ctrl Pts',(-20.7443280892572,17.623592423249,-6.48157967874059));
#43147=CARTESIAN_POINT('Ctrl Pts',(-20.7962584977302,17.6941974787272,-6.48596614075314));
#43148=CARTESIAN_POINT('Ctrl Pts',(-20.8460908704134,17.7619500256716,-6.4901753857061));
#43149=CARTESIAN_POINT('Ctrl Pts',(-20.8926734978045,17.8322867639503,-6.49438463065905));
#43150=CARTESIAN_POINT('Ctrl Pts',(-20.9357293738867,17.9048653345981,-6.498593875612));
#43151=CARTESIAN_POINT('Ctrl Pts',(-20.9787228581407,17.9773387323842,-6.5027970209913));
#43152=CARTESIAN_POINT('Ctrl Pts',(-21.0181995127222,18.0520471246587,-6.50700016637059));
#43153=CARTESIAN_POINT('Ctrl Pts',(-21.0539239335172,18.1286170073888,-6.51120331174989));
#43154=CARTESIAN_POINT('Ctrl Pts',(-21.0896068791136,18.2050979943154,-6.51540157737787));
#43155=CARTESIAN_POINT('Ctrl Pts',(-21.1215460556625,18.283435770082,-6.51959984300585));
#43156=CARTESIAN_POINT('Ctrl Pts',(-21.1495512259746,18.3632310015738,-6.52379810863383));
#43157=CARTESIAN_POINT('Ctrl Pts',(-21.177530608527,18.4429527559101,-6.52799250840905));
#43158=CARTESIAN_POINT('Ctrl Pts',(-21.20158303815,18.5241288717761,-6.53218690818426));
#43159=CARTESIAN_POINT('Ctrl Pts',(-21.2215663308331,18.6063399717978,-6.53638130795947));
#43160=CARTESIAN_POINT('Ctrl Pts',(-21.2415389226779,18.6885070486596,-6.54057346167871));
#43161=CARTESIAN_POINT('Ctrl Pts',(-21.2574466025638,18.7717075687081,-6.54476561539795));
#43162=CARTESIAN_POINT('Ctrl Pts',(-21.2691973211302,18.8555080269057,-6.54895776911719));
#43163=CARTESIAN_POINT('Ctrl Pts',(-21.2809466969547,18.9392989093157,-6.55314944380356));
#43164=CARTESIAN_POINT('Ctrl Pts',(-21.288539988214,19.0236891460417,-6.55734111848993));
#43165=CARTESIAN_POINT('Ctrl Pts',(-21.2919366299884,19.1082371810269,-6.5615327931763));
#43166=CARTESIAN_POINT('Ctrl Pts',(-21.2933350165072,19.1430453357178,-6.56325849219371));
#43167=CARTESIAN_POINT('Ctrl Pts',(-21.294022704555,19.1778801783151,-6.56498419121111));
#43168=CARTESIAN_POINT('Ctrl Pts',(-21.2939994283744,19.2127107666517,-6.56670989022851));
#43169=CARTESIAN_POINT('Origin',(-18.734,19.211,1.76670989022852));
#43170=CARTESIAN_POINT('',(-17.1744642439897,21.2411350264762,-5.25018233500805));
#43171=CARTESIAN_POINT('',(-17.1744642439897,21.2411350264762,-5.31661774316889));
#43172=CARTESIAN_POINT('',(-17.1744642439897,21.2411350264762,1.76670989022852));
#43173=CARTESIAN_POINT('',(-21.2939994369002,19.2126979607666,-5.8332901097715));
#43174=CARTESIAN_POINT('Ctrl Pts',(-17.1744642439897,21.2411350264762,-5.31661774316889));
#43175=CARTESIAN_POINT('Ctrl Pts',(-17.1078004643465,21.1899243697324,-5.32080131395071));
#43176=CARTESIAN_POINT('Ctrl Pts',(-17.043740061828,21.1354869082706,-5.32498488473253));
#43177=CARTESIAN_POINT('Ctrl Pts',(-16.9825942508179,21.0781309278494,-5.32916845551436));
#43178=CARTESIAN_POINT('Ctrl Pts',(-16.9299734999191,21.0287716224703,-5.33276874525361));
#43179=CARTESIAN_POINT('Ctrl Pts',(-16.8795107939483,20.9772516236668,-5.33636903499286));
#43180=CARTESIAN_POINT('Ctrl Pts',(-16.8313804354228,20.923786849695,-5.3399693247321));
#43181=CARTESIAN_POINT('Ctrl Pts',(-16.7754382840342,20.8616444811128,-5.34415395912515));
#43182=CARTESIAN_POINT('Ctrl Pts',(-16.7224397206528,20.7966428559978,-5.3483385935182));
#43183=CARTESIAN_POINT('Ctrl Pts',(-16.6726908063355,20.7290923582293,-5.35252322791125));
#43184=CARTESIAN_POINT('Ctrl Pts',(-16.6230127034401,20.6616380102332,-5.35670190599519));
#43185=CARTESIAN_POINT('Ctrl Pts',(-16.5765753324319,20.5916423631924,-5.36088058407914));
#43186=CARTESIAN_POINT('Ctrl Pts',(-16.533646260122,20.5194507707227,-5.36505926216308));
#43187=CARTESIAN_POINT('Ctrl Pts',(-16.4899477150435,20.4459651958412,-5.36931284004852));
#43188=CARTESIAN_POINT('Ctrl Pts',(-16.4498848008428,20.3702045348863,-5.37356641793395));
#43189=CARTESIAN_POINT('Ctrl Pts',(-16.4136951701205,20.2925662237874,-5.37781999581939));
#43190=CARTESIAN_POINT('Ctrl Pts',(-16.378207146008,20.2164330828479,-5.38199110979734));
#43191=CARTESIAN_POINT('Ctrl Pts',(-16.3464437665668,20.1384948820616,-5.38616222377529));
#43192=CARTESIAN_POINT('Ctrl Pts',(-16.3185831851716,20.0591518794675,-5.39033333775325));
#43193=CARTESIAN_POINT('Ctrl Pts',(-16.2907319526636,19.9798355011843,-5.39450305207362));
#43194=CARTESIAN_POINT('Ctrl Pts',(-16.2667810695588,19.8991156909809,-5.39867276639399));
#43195=CARTESIAN_POINT('Ctrl Pts',(-16.2468600106956,19.8174113072849,-5.40284248071437));
#43196=CARTESIAN_POINT('Ctrl Pts',(-16.2269396607092,19.7357098309815,-5.40701204665841));
#43197=CARTESIAN_POINT('Ctrl Pts',(-16.2110489579958,19.6530242979866,-5.41118161260245));
#43198=CARTESIAN_POINT('Ctrl Pts',(-16.1992667534716,19.5697859653661,-5.4153511785465));
#43199=CARTESIAN_POINT('Ctrl Pts',(-16.1870703011714,19.4836210756563,-5.41966734128542));
#43200=CARTESIAN_POINT('Ctrl Pts',(-16.1792767060087,19.3968643124029,-5.42398350402434));
#43201=CARTESIAN_POINT('Ctrl Pts',(-16.1759149870658,19.3100003363692,-5.42829966676326));
#43202=CARTESIAN_POINT('Ctrl Pts',(-16.1726627757638,19.2259659452184,-5.43247523095494));
#43203=CARTESIAN_POINT('Ctrl Pts',(-16.1735580857934,19.1418316894465,-5.43665079514662));
#43204=CARTESIAN_POINT('Ctrl Pts',(-16.1785740672325,19.0580349643242,-5.4408263593383));
#43205=CARTESIAN_POINT('Ctrl Pts',(-16.1838433939698,18.9700058658238,-5.44521282135084));
#43206=CARTESIAN_POINT('Ctrl Pts',(-16.1936605371381,18.8823498716687,-5.44959928336338));
#43207=CARTESIAN_POINT('Ctrl Pts',(-16.2079333028748,18.7955640342066,-5.45398574537592));
#43208=CARTESIAN_POINT('Ctrl Pts',(-16.2222060686114,18.7087781967444,-5.45837220738847));
#43209=CARTESIAN_POINT('Ctrl Pts',(-16.2409342590202,18.6228630666792,-5.46275866940101));
#43210=CARTESIAN_POINT('Ctrl Pts',(-16.2639654295305,18.5382970784325,-5.46714513141355));
#43211=CARTESIAN_POINT('Ctrl Pts',(-16.2859369017452,18.4576220966618,-5.47132976580659));
#43212=CARTESIAN_POINT('Ctrl Pts',(-16.3119058645756,18.377874545241,-5.47551440019964));
#43213=CARTESIAN_POINT('Ctrl Pts',(-16.3417769993438,18.299479777991,-5.47969903459269));
#43214=CARTESIAN_POINT('Ctrl Pts',(-16.3716056162489,18.2211965959888,-5.48387771267663));
#43215=CARTESIAN_POINT('Ctrl Pts',(-16.4053252101866,18.1442627996736,-5.48805639076058));
#43216=CARTESIAN_POINT('Ctrl Pts',(-16.4427902222593,18.0690903037519,-5.49223506884452));
#43217=CARTESIAN_POINT('Ctrl Pts',(-16.4809267677478,17.9925703948664,-5.49648864672995));
#43218=CARTESIAN_POINT('Ctrl Pts',(-16.5229441986227,17.9178760152569,-5.50074222461539));
#43219=CARTESIAN_POINT('Ctrl Pts',(-16.5686369710084,17.8454221176819,-5.50499580250083));
#43220=CARTESIAN_POINT('Ctrl Pts',(-16.6134438998393,17.7743728802935,-5.50916691647878));
#43221=CARTESIAN_POINT('Ctrl Pts',(-16.6617846778615,17.7054784349765,-5.51333803045673));
#43222=CARTESIAN_POINT('Ctrl Pts',(-16.7134191824492,17.6391052326107,-5.51750914443468));
#43223=CARTESIAN_POINT('Ctrl Pts',(-16.7650363605803,17.572754302414,-5.52167885875505));
#43224=CARTESIAN_POINT('Ctrl Pts',(-16.8199447880143,17.5089232977414,-5.52584857307543));
#43225=CARTESIAN_POINT('Ctrl Pts',(-16.8778623533736,17.4479478065649,-5.5300182873958));
#43226=CARTESIAN_POINT('Ctrl Pts',(-16.9357778577775,17.386974485158,-5.53418785333984));
#43227=CARTESIAN_POINT('Ctrl Pts',(-16.9967019697692,17.3288568081793,-5.53835741928389));
#43228=CARTESIAN_POINT('Ctrl Pts',(-17.0603147509096,17.2738945080412,-5.54252698522793));
#43229=CARTESIAN_POINT('Ctrl Pts',(-17.12616407896,17.2169998012335,-5.54684314796685));
#43230=CARTESIAN_POINT('Ctrl Pts',(-17.1948942620563,17.1634868305881,-5.55115931070577));
#43231=CARTESIAN_POINT('Ctrl Pts',(-17.2661134846746,17.1136423342391,-5.55547547344469));
#43232=CARTESIAN_POINT('Ctrl Pts',(-17.3350127486071,17.0654215171161,-5.55965103763637));
#43233=CARTESIAN_POINT('Ctrl Pts',(-17.4062409575146,17.0206340542482,-5.56382660182805));
#43234=CARTESIAN_POINT('Ctrl Pts',(-17.4794157978406,16.9794941228641,-5.56800216601973));
#43235=CARTESIAN_POINT('Ctrl Pts',(-17.5562865253948,16.9362763113467,-5.57238862803227));
#43236=CARTESIAN_POINT('Ctrl Pts',(-17.6353051780176,16.897084448046,-5.57677509004481));
#43237=CARTESIAN_POINT('Ctrl Pts',(-17.7160039105555,16.8621100575217,-5.58116155205735));
#43238=CARTESIAN_POINT('Ctrl Pts',(-17.7967026430934,16.8271356669974,-5.58554801406989));
#43239=CARTESIAN_POINT('Ctrl Pts',(-17.8790808853742,16.7963788809358,-5.58993447608243));
#43240=CARTESIAN_POINT('Ctrl Pts',(-17.9626538344085,16.7699704850561,-5.59432093809497));
#43241=CARTESIAN_POINT('Ctrl Pts',(-18.0423814681728,16.7447771786174,-5.59850557248802));
#43242=CARTESIAN_POINT('Ctrl Pts',(-18.1234930456338,16.7234471296282,-5.60269020688106));
#43243=CARTESIAN_POINT('Ctrl Pts',(-18.2055793173493,16.7061304261206,-5.60687484127411));
#43244=CARTESIAN_POINT('Ctrl Pts',(-18.2875487494172,16.688838370797,-5.61105351935805));
#43245=CARTESIAN_POINT('Ctrl Pts',(-18.370489673737,16.6755484082766,-5.61523219744199));
#43246=CARTESIAN_POINT('Ctrl Pts',(-18.4539769469565,16.6663611081798,-5.61941087552594));
#43247=CARTESIAN_POINT('Ctrl Pts',(-18.5389606695472,16.6570091323315,-5.62366445341137));
#43248=CARTESIAN_POINT('Ctrl Pts',(-18.624510060566,16.6519084913031,-5.62791803129681));
#43249=CARTESIAN_POINT('Ctrl Pts',(-18.7101649534091,16.6511109612809,-5.63217160918225));
#43250=CARTESIAN_POINT('Ctrl Pts',(-18.7941592590127,16.6503288929346,-5.6363427231602));
#43251=CARTESIAN_POINT('Ctrl Pts',(-18.87825453103,16.6536845805936,-5.64051383713815));
#43252=CARTESIAN_POINT('Ctrl Pts',(-18.9620126684402,16.6611744720411,-5.6446849511161));
#43253=CARTESIAN_POINT('Ctrl Pts',(-19.0457426999984,16.6686618501832,-5.64885466543648));
#43254=CARTESIAN_POINT('Ctrl Pts',(-19.1291353638019,16.6802806360297,-5.65302437975685));
#43255=CARTESIAN_POINT('Ctrl Pts',(-19.2117557819362,16.6959752659613,-5.65719409407723));
#43256=CARTESIAN_POINT('Ctrl Pts',(-19.2943732600815,16.7116693374106,-5.66136366002127));
#43257=CARTESIAN_POINT('Ctrl Pts',(-19.3762180954027,16.7314388778862,-5.66553322596532));
#43258=CARTESIAN_POINT('Ctrl Pts',(-19.4568650837658,16.7551771092621,-5.66970279190936));
#43259=CARTESIAN_POINT('Ctrl Pts',(-19.5403475207509,16.7797499475689,-5.67401895464828));
#43260=CARTESIAN_POINT('Ctrl Pts',(-19.6225458049915,16.808575598709,-5.6783351173872));
#43261=CARTESIAN_POINT('Ctrl Pts',(-19.7030067527823,16.8414798137466,-5.68265128012612));
#43262=CARTESIAN_POINT('Ctrl Pts',(-19.7808466936618,16.8733121774403,-5.6868268443178));
#43263=CARTESIAN_POINT('Ctrl Pts',(-19.8570603406959,16.9089612248342,-5.69100240850948));
#43264=CARTESIAN_POINT('Ctrl Pts',(-19.9312606656524,16.9482214208011,-5.69517797270116));
#43265=CARTESIAN_POINT('Ctrl Pts',(-20.009208672628,16.989464555934,-5.6995644347137));
#43266=CARTESIAN_POINT('Ctrl Pts',(-20.0849341253746,17.0346929255447,-5.70395089672624));
#43267=CARTESIAN_POINT('Ctrl Pts',(-20.1580227463385,17.0836168145088,-5.70833735873878));
#43268=CARTESIAN_POINT('Ctrl Pts',(-20.2311113673024,17.1325407034729,-5.71272382075133));
#43269=CARTESIAN_POINT('Ctrl Pts',(-20.3015627371329,17.185159703645,-5.71711028276387));
#43270=CARTESIAN_POINT('Ctrl Pts',(-20.3690044710744,17.2411369642621,-5.72149674477641));
#43271=CARTESIAN_POINT('Ctrl Pts',(-20.4324580482224,17.2938040179914,-5.72562381401755));
#43272=CARTESIAN_POINT('Ctrl Pts',(-20.4934979978141,17.3496514870446,-5.72975088325869));
#43273=CARTESIAN_POINT('Ctrl Pts',(-20.5517814829092,17.4084267059583,-5.73387795249984));
#43274=CARTESIAN_POINT('Ctrl Pts',(-20.6102782700972,17.4674170265802,-5.73802012571949));
#43275=CARTESIAN_POINT('Ctrl Pts',(-20.6659979620834,17.5293563204315,-5.74216229893914));
#43276=CARTESIAN_POINT('Ctrl Pts',(-20.7186255971237,17.5939467419898,-5.74630447215879));
#43277=CARTESIAN_POINT('Ctrl Pts',(-20.7709257203662,17.658135205051,-5.75042086784547));
#43278=CARTESIAN_POINT('Ctrl Pts',(-20.8201718394843,17.7249415391099,-5.75453726353214));
#43279=CARTESIAN_POINT('Ctrl Pts',(-20.8660914253506,17.7940362905331,-5.75865365921881));
#43280=CARTESIAN_POINT('Ctrl Pts',(-20.9119829684087,17.8630888462171,-5.76276754104799));
#43281=CARTESIAN_POINT('Ctrl Pts',(-20.9545517475123,17.9344266527042,-5.76688142287717));
#43282=CARTESIAN_POINT('Ctrl Pts',(-20.9935669693931,18.0076891046668,-5.77099530470634));
#43283=CARTESIAN_POINT('Ctrl Pts',(-21.0325708263853,18.0809302157382,-5.77510798818763));
#43284=CARTESIAN_POINT('Ctrl Pts',(-21.0680229592547,18.1560944409463,-5.77922067166891));
#43285=CARTESIAN_POINT('Ctrl Pts',(-21.0997379788824,18.2327956168196,-5.7833333551502));
#43286=CARTESIAN_POINT('Ctrl Pts',(-21.1318415000295,18.3104363640289,-5.78749641803531));
#43287=CARTESIAN_POINT('Ctrl Pts',(-21.1601155043873,18.3896515290328,-5.79165948092042));
#43288=CARTESIAN_POINT('Ctrl Pts',(-21.1844181339266,18.4700202641611,-5.79582254380553));
#43289=CARTESIAN_POINT('Ctrl Pts',(-21.2084475698835,18.5494855487958,-5.79993880837768));
#43290=CARTESIAN_POINT('Ctrl Pts',(-21.2285944016388,18.6300781193823,-5.80405507294983));
#43291=CARTESIAN_POINT('Ctrl Pts',(-21.2447724368935,18.7113783730305,-5.80817133752198));
#43292=CARTESIAN_POINT('Ctrl Pts',(-21.2612263672264,18.7940650953984,-5.81235779956356));
#43293=CARTESIAN_POINT('Ctrl Pts',(-21.2735747867911,18.8774833595966,-5.81654426160515));
#43294=CARTESIAN_POINT('Ctrl Pts',(-21.281781944964,18.9611857471732,-5.82073072364674));
#43295=CARTESIAN_POINT('Ctrl Pts',(-21.2899891031369,19.0448881347499,-5.82491718568833));
#43296=CARTESIAN_POINT('Ctrl Pts',(-21.2940550344004,19.1288741338655,-5.82910364772991));
#43297=CARTESIAN_POINT('Ctrl Pts',(-21.2939994369002,19.2126979607666,-5.8332901097715));
#43298=CARTESIAN_POINT('Ctrl Pts',(-21.2967674808324,19.2126997967162,-5.8332901097715));
#43299=CARTESIAN_POINT('Ctrl Pts',(-21.2975540827487,19.3154768305114,-5.83841759033361));
#43300=CARTESIAN_POINT('Ctrl Pts',(-21.2452321516418,20.267165082075,-5.8859370064562));
#43301=CARTESIAN_POINT('Ctrl Pts',(-20.0538051929683,21.9352257637231,-5.97584835813928));
#43302=CARTESIAN_POINT('Ctrl Pts',(-18.0187465009573,21.8369135205367,-6.06521460546765));
#43303=CARTESIAN_POINT('Ctrl Pts',(-17.2449841467773,21.3000311130452,-6.11218891723554));
#43304=CARTESIAN_POINT('Ctrl Pts',(-17.1725993531626,21.24352550386,-6.11677129344295));
#43305=CARTESIAN_POINT('',(-21.2939992944986,19.2090994299067,-5.76670989019962));
#43306=CARTESIAN_POINT('Ctrl Pts',(-21.293999294499,19.2090994304895,-5.76670989022851));
#43307=CARTESIAN_POINT('Ctrl Pts',(-21.2940618231948,19.2933233519321,-5.77088500205647));
#43308=CARTESIAN_POINT('Ctrl Pts',(-21.2899635861128,19.3775880720651,-5.77506011388443));
#43309=CARTESIAN_POINT('Ctrl Pts',(-21.2817191504239,19.4614538491683,-5.77923522571239));
#43310=CARTESIAN_POINT('Ctrl Pts',(-21.2734754980237,19.5453116583388,-5.78340994087068));
#43311=CARTESIAN_POINT('Ctrl Pts',(-21.2610864747303,19.6287701442277,-5.78758465602897));
#43312=CARTESIAN_POINT('Ctrl Pts',(-21.2446185572459,19.7113943045362,-5.79175937118726));
#43313=CARTESIAN_POINT('Ctrl Pts',(-21.2281473245847,19.794035098017,-5.79593492676264));
#43314=CARTESIAN_POINT('Ctrl Pts',(-21.2075956572653,19.8758407835678,-5.80011048233803));
#43315=CARTESIAN_POINT('Ctrl Pts',(-21.1830809475491,19.956387491411,-5.80428603791341));
#43316=CARTESIAN_POINT('Ctrl Pts',(-21.1585369190256,20.0370305305357,-5.80846658731945));
#43317=CARTESIAN_POINT('Ctrl Pts',(-21.1300205198885,20.1164111473511,-5.8126471367255));
#43318=CARTESIAN_POINT('Ctrl Pts',(-21.0976986239764,20.1941219736187,-5.81682768613154));
#43319=CARTESIAN_POINT('Ctrl Pts',(-21.0653559283573,20.2718828081662,-5.82101092579446));
#43320=CARTESIAN_POINT('Ctrl Pts',(-21.0292030575738,20.347971299817,-5.82519416545738));
#43321=CARTESIAN_POINT('Ctrl Pts',(-20.9894534545796,20.4220035979404,-5.8293774051203));
#43322=CARTESIAN_POINT('Ctrl Pts',(-20.9496320042093,20.4961697093846,-5.83356820598562));
#43323=CARTESIAN_POINT('Ctrl Pts',(-20.906201076148,20.5682718138337,-5.83775900685095));
#43324=CARTESIAN_POINT('Ctrl Pts',(-20.8594180036074,20.6379542073737,-5.84194980771627));
#43325=CARTESIAN_POINT('Ctrl Pts',(-20.8291383592868,20.6830550948788,-5.84466224092617));
#43326=CARTESIAN_POINT('Ctrl Pts',(-20.7974553185202,20.7271429654288,-5.84737467413607));
#43327=CARTESIAN_POINT('Ctrl Pts',(-20.7644472985012,20.770129169764,-5.85008710734597));
#43328=CARTESIAN_POINT('Ctrl Pts',(-20.7135238341689,20.8364465811685,-5.85427174173902));
#43329=CARTESIAN_POINT('Ctrl Pts',(-20.6592531496868,20.9003899294851,-5.85845637613207));
#43330=CARTESIAN_POINT('Ctrl Pts',(-20.6018847443057,20.9616017771012,-5.86264101052512));
#43331=CARTESIAN_POINT('Ctrl Pts',(-20.5445979957491,21.0227264972285,-5.86681968860906));
#43332=CARTESIAN_POINT('Ctrl Pts',(-20.4842225962896,21.0811271065652,-5.87099836669299));
#43333=CARTESIAN_POINT('Ctrl Pts',(-20.4210494366145,21.1364776546142,-5.87517704477693));
#43334=CARTESIAN_POINT('Ctrl Pts',(-20.3567439434538,21.1928203214575,-5.87943062266237));
#43335=CARTESIAN_POINT('Ctrl Pts',(-20.28953969747,21.2460021244011,-5.8836842005478));
#43336=CARTESIAN_POINT('Ctrl Pts',(-20.2197842460679,21.2957170489389,-5.88793777843324));
#43337=CARTESIAN_POINT('Ctrl Pts',(-20.1513811402078,21.3444681526538,-5.89210889241119));
#43338=CARTESIAN_POINT('Ctrl Pts',(-20.0805252582505,21.3898853234968,-5.89628000638915));
#43339=CARTESIAN_POINT('Ctrl Pts',(-20.0075777510545,21.4317205389285,-5.9004511203671));
#43340=CARTESIAN_POINT('Ctrl Pts',(-19.9346547220992,21.4735417161496,-5.90462083468747));
#43341=CARTESIAN_POINT('Ctrl Pts',(-19.8596418605525,21.5117830963985,-5.90879054900784));
#43342=CARTESIAN_POINT('Ctrl Pts',(-19.7829274662089,21.5462411375771,-5.91296026332821));
#43343=CARTESIAN_POINT('Ctrl Pts',(-19.7062158016926,21.5806979525908,-5.91712982927226));
#43344=CARTESIAN_POINT('Ctrl Pts',(-19.6278031447569,21.6113715084927,-5.92129939521631));
#43345=CARTESIAN_POINT('Ctrl Pts',(-19.5480992000003,21.6381057852015,-5.92546896116036));
#43346=CARTESIAN_POINT('Ctrl Pts',(-19.4655929628716,21.6657800060991,-5.92978512389928));
#43347=CARTESIAN_POINT('Ctrl Pts',(-19.3817034451244,21.6892326159303,-5.9341012866382));
#43348=CARTESIAN_POINT('Ctrl Pts',(-19.2969019322697,21.7083468751151,-5.93841744937712));
#43349=CARTESIAN_POINT('Ctrl Pts',(-19.2148628197767,21.7268384893174,-5.9425930135688));
#43350=CARTESIAN_POINT('Ctrl Pts',(-19.1319706883699,21.7412700216399,-5.94676857776048));
#43351=CARTESIAN_POINT('Ctrl Pts',(-19.0486605152119,21.751588270493,-5.95094414195216));
#43352=CARTESIAN_POINT('Ctrl Pts',(-18.9611425432588,21.7624276695664,-5.9553306039647));
#43353=CARTESIAN_POINT('Ctrl Pts',(-18.8731637715282,21.7687272994046,-5.95971706597724));
#43354=CARTESIAN_POINT('Ctrl Pts',(-18.7852297301452,21.7704873538951,-5.96410352798978));
#43355=CARTESIAN_POINT('Ctrl Pts',(-18.6972956887621,21.7722474083857,-5.96848999000232));
#43356=CARTESIAN_POINT('Ctrl Pts',(-18.6094069552492,21.7694679818952,-5.97287645201486));
#43357=CARTESIAN_POINT('Ctrl Pts',(-18.5220617179689,21.7622119011579,-5.97726291402741));
#43358=CARTESIAN_POINT('Ctrl Pts',(-18.4387429644644,21.7552903148049,-5.98144716675325));
#43359=CARTESIAN_POINT('Ctrl Pts',(-18.3556086018994,21.7442699592594,-5.98563141947909));
#43360=CARTESIAN_POINT('Ctrl Pts',(-18.2730941087504,21.7291671428663,-5.98981567220493));
#43361=CARTESIAN_POINT('Ctrl Pts',(-18.190691343858,21.7140847763515,-5.99399425926836));
#43362=CARTESIAN_POINT('Ctrl Pts',(-18.1089072302507,21.6949310074154,-5.99817284633179));
#43363=CARTESIAN_POINT('Ctrl Pts',(-18.0281732667132,21.6717739885202,-6.00235143339522));
#43364=CARTESIAN_POINT('Ctrl Pts',(-17.9475320674686,21.6486435773176,-6.00652521921196));
#43365=CARTESIAN_POINT('Ctrl Pts',(-17.867939059854,21.6215191846037,-6.01069900502871));
#43366=CARTESIAN_POINT('Ctrl Pts',(-17.7898152017479,21.5905199235874,-6.01487279084546));
#43367=CARTESIAN_POINT('Ctrl Pts',(-17.711744863133,21.5595418989095,-6.01904371737058));
#43368=CARTESIAN_POINT('Ctrl Pts',(-17.6351421012572,21.5246944476472,-6.02321464389571));
#43369=CARTESIAN_POINT('Ctrl Pts',(-17.5604112612688,21.4861460331863,-6.02738557042083));
#43370=CARTESIAN_POINT('Ctrl Pts',(-17.4856945971112,21.4476049310452,-6.0315557057552));
#43371=CARTESIAN_POINT('Ctrl Pts',(-17.4128495626245,21.4053644619676,-6.03572584108958));
#43372=CARTESIAN_POINT('Ctrl Pts',(-17.3422580870172,21.3596401391687,-6.03989597642395));
#43373=CARTESIAN_POINT('Ctrl Pts',(-17.284768252093,21.3224021618192,-6.04329214274463));
#43374=CARTESIAN_POINT('Ctrl Pts',(-17.2287727645366,21.2828544582107,-6.04668830906531));
#43375=CARTESIAN_POINT('Ctrl Pts',(-17.1744642439897,21.2411350264762,-6.05008447538598));
#43376=CARTESIAN_POINT('Ctrl Pts',(-17.1744642439897,21.2411350264762,-5.25018233500805));
#43377=CARTESIAN_POINT('Ctrl Pts',(-17.1078623666769,21.1899719226766,-5.2543537667356));
#43378=CARTESIAN_POINT('Ctrl Pts',(-17.0437277229001,21.1354870746848,-5.25852519846314));
#43379=CARTESIAN_POINT('Ctrl Pts',(-16.9824038291382,21.0779522902908,-5.26269663019068));
#43380=CARTESIAN_POINT('Ctrl Pts',(-16.9211032708343,21.0204393994927,-5.26686647457169));
#43381=CARTESIAN_POINT('Ctrl Pts',(-16.8626116736662,20.9598791914874,-5.2710363189527));
#43382=CARTESIAN_POINT('Ctrl Pts',(-16.8072381052118,20.8965825701496,-5.27520616333371));
#43383=CARTESIAN_POINT('Ctrl Pts',(-16.7518689972008,20.8332910474717,-5.27937567182604));
#43384=CARTESIAN_POINT('Ctrl Pts',(-16.6996177211823,20.7672638961413,-5.28354518031838));
#43385=CARTESIAN_POINT('Ctrl Pts',(-16.6507542879591,20.6988465321609,-5.28771468881071));
#43386=CARTESIAN_POINT('Ctrl Pts',(-16.601880133168,20.6304141561077,-5.29188511217262));
#43387=CARTESIAN_POINT('Ctrl Pts',(-16.5563955634883,20.5595909010415,-5.29605553553454));
#43388=CARTESIAN_POINT('Ctrl Pts',(-16.5145275494684,20.4867515594077,-5.30022595889645));
#43389=CARTESIAN_POINT('Ctrl Pts',(-16.4726122570734,20.4138299658258,-5.30440109160139));
#43390=CARTESIAN_POINT('Ctrl Pts',(-16.4343218983041,20.3388881425673,-5.30857622430633));
#43391=CARTESIAN_POINT('Ctrl Pts',(-16.3998374264075,20.2623253920836,-5.31275135701127));
#43392=CARTESIAN_POINT('Ctrl Pts',(-16.3653298664573,20.1857113812853,-5.31692928505226));
#43393=CARTESIAN_POINT('Ctrl Pts',(-16.3346334319057,20.1074747112887,-5.32110721309324));
#43394=CARTESIAN_POINT('Ctrl Pts',(-16.3078800190985,20.0280323361228,-5.32528514113422));
#43395=CARTESIAN_POINT('Ctrl Pts',(-16.2810838876785,19.948463111045,-5.32946974029756));
#43396=CARTESIAN_POINT('Ctrl Pts',(-16.2582434643436,19.867684781143,-5.33365433946089));
#43397=CARTESIAN_POINT('Ctrl Pts',(-16.2394400132345,19.7861264838525,-5.33783893862422));
#43398=CARTESIAN_POINT('Ctrl Pts',(-16.2341302937206,19.7630960475706,-5.33902058595623));
#43399=CARTESIAN_POINT('Ctrl Pts',(-16.2291421595411,19.7400034568201,-5.34020223328824));
#43400=CARTESIAN_POINT('Ctrl Pts',(-16.2244766916358,19.7168584434174,-5.34138388062024));
#43401=CARTESIAN_POINT('Ctrl Pts',(-16.2079546068079,19.634893701071,-5.34556851501329));
#43402=CARTESIAN_POINT('Ctrl Pts',(-16.1954216323759,19.5519661209786,-5.34975314940634));
#43403=CARTESIAN_POINT('Ctrl Pts',(-16.1869832270606,19.4684986570165,-5.35393778379939));
#43404=CARTESIAN_POINT('Ctrl Pts',(-16.1785568327709,19.3851499986583,-5.35811646188333));
#43405=CARTESIAN_POINT('Ctrl Pts',(-16.1742134770096,19.3012634366145,-5.36229513996727));
#43406=CARTESIAN_POINT('Ctrl Pts',(-16.174007684269,19.2172724316078,-5.36647381805121));
#43407=CARTESIAN_POINT('Ctrl Pts',(-16.1737982028414,19.1317759481996,-5.37072739593664));
#43408=CARTESIAN_POINT('Ctrl Pts',(-16.177876170323,19.0461717133522,-5.37498097382208));
#43409=CARTESIAN_POINT('Ctrl Pts',(-16.1862438519479,18.960922791797,-5.37923455170752));
#43410=CARTESIAN_POINT('Ctrl Pts',(-16.1944493097363,18.8773265869357,-5.38340566568547));
#43411=CARTESIAN_POINT('Ctrl Pts',(-16.2067795899915,18.7940725203434,-5.38757677966342));
#43412=CARTESIAN_POINT('Ctrl Pts',(-16.2231843067498,18.7115958004499,-5.39174789364137));
#43413=CARTESIAN_POINT('Ctrl Pts',(-16.2395835187469,18.6291467564162,-5.39591760796175));
#43414=CARTESIAN_POINT('Ctrl Pts',(-16.260054362265,18.5474749918556,-5.40008732228212));
#43415=CARTESIAN_POINT('Ctrl Pts',(-16.2844950829502,18.4670069480508,-5.4042570366025));
#43416=CARTESIAN_POINT('Ctrl Pts',(-16.3089349339296,18.3865417676445,-5.40842660254653));
#43417=CARTESIAN_POINT('Ctrl Pts',(-16.3373442466934,18.3072806627592,-5.41259616849058));
#43418=CARTESIAN_POINT('Ctrl Pts',(-16.3695713807104,18.2296349790806,-5.41676573443461));
#43419=CARTESIAN_POINT('Ctrl Pts',(-16.402931581003,18.14925936895,-5.42108189717353));
#43420=CARTESIAN_POINT('Ctrl Pts',(-16.4403828646776,18.0706153771459,-5.42539805991245));
#43421=CARTESIAN_POINT('Ctrl Pts',(-16.4817035150008,17.9941349525687,-5.42971422265138));
#43422=CARTESIAN_POINT('Ctrl Pts',(-16.5216781494858,17.9201458697778,-5.43388978684306));
#43423=CARTESIAN_POINT('Ctrl Pts',(-16.5652736482194,17.8481819408654,-5.43806535103474));
#43424=CARTESIAN_POINT('Ctrl Pts',(-16.6122442629254,17.7786059926853,-5.44224091522642));
#43425=CARTESIAN_POINT('Ctrl Pts',(-16.6615872517182,17.7055159287637,-5.44662737723896));
#43426=CARTESIAN_POINT('Ctrl Pts',(-16.7146549198489,17.6350618855122,-5.45101383925151));
#43427=CARTESIAN_POINT('Ctrl Pts',(-16.7711149075846,17.5676247799199,-5.45540030126405));
#43428=CARTESIAN_POINT('Ctrl Pts',(-16.8275748953203,17.5001876743276,-5.45978676327659));
#43429=CARTESIAN_POINT('Ctrl Pts',(-16.8874267520075,17.4357678796896,-5.46417322528913));
#43430=CARTESIAN_POINT('Ctrl Pts',(-16.9502957329765,17.3746996193972,-5.46855968730167));
#43431=CARTESIAN_POINT('Ctrl Pts',(-17.010272018937,17.3164412002856,-5.47274432169473));
#43432=CARTESIAN_POINT('Ctrl Pts',(-17.0732171288673,17.2610158259163,-5.47692895608778));
#43433=CARTESIAN_POINT('Ctrl Pts',(-17.1388325082968,17.2087411072957,-5.48111359048083));
#43434=CARTESIAN_POINT('Ctrl Pts',(-17.2043544923552,17.1565407952668,-5.48529226856478));
#43435=CARTESIAN_POINT('Ctrl Pts',(-17.2725388396026,17.1074825154227,-5.48947094664872));
#43436=CARTESIAN_POINT('Ctrl Pts',(-17.3430505912413,17.0618467383004,-5.49364962473267));
#43437=CARTESIAN_POINT('Ctrl Pts',(-17.4148262153522,17.0153929726712,-5.49790320261811));
#43438=CARTESIAN_POINT('Ctrl Pts',(-17.4890131561479,16.9724859492607,-5.50215678050354));
#43439=CARTESIAN_POINT('Ctrl Pts',(-17.5652232755995,16.9333782209288,-5.50641035838897));
#43440=CARTESIAN_POINT('Ctrl Pts',(-17.6399559131736,16.895028672223,-5.51058147236693));
#43441=CARTESIAN_POINT('Ctrl Pts',(-17.716633554776,16.8603326394004,-5.51475258634488));
#43442=CARTESIAN_POINT('Ctrl Pts',(-17.7948629860237,16.8294833259077,-5.51892370032283));
#43443=CARTESIAN_POINT('Ctrl Pts',(-17.8730661666303,16.7986443642001,-5.5230934146432));
#43444=CARTESIAN_POINT('Ctrl Pts',(-17.9528196751248,16.7716497268885,-5.52726312896358));
#43445=CARTESIAN_POINT('Ctrl Pts',(-18.0337098641726,16.7486446792425,-5.53143284328395));
#43446=CARTESIAN_POINT('Ctrl Pts',(-18.1145971748004,16.7256404502148,-5.535602409228));
#43447=CARTESIAN_POINT('Ctrl Pts',(-18.1966206428412,16.7066256536092,-5.53977197517205));
#43448=CARTESIAN_POINT('Ctrl Pts',(-18.2793523115269,16.6916954373546,-5.5439415411161));
#43449=CARTESIAN_POINT('Ctrl Pts',(-18.3649927236227,16.676240293115,-5.54825770385502));
#43450=CARTESIAN_POINT('Ctrl Pts',(-18.4513915445816,16.6651623947289,-5.55257386659394));
#43451=CARTESIAN_POINT('Ctrl Pts',(-18.5380655626732,16.6585091192583,-5.55689002933285));
#43452=CARTESIAN_POINT('Ctrl Pts',(-18.6219161837418,16.6520725735364,-5.56106559352453));
#43453=CARTESIAN_POINT('Ctrl Pts',(-18.7060238760288,16.6497767790178,-5.5652411577162));
#43454=CARTESIAN_POINT('Ctrl Pts',(-18.7899505406878,16.651611491587,-5.56941672190788));
#43455=CARTESIAN_POINT('Ctrl Pts',(-18.8781161416622,16.6535388711264,-5.57380318392041));
#43456=CARTESIAN_POINT('Ctrl Pts',(-18.9660813646938,16.6600249445383,-5.57818964593295));
#43457=CARTESIAN_POINT('Ctrl Pts',(-19.0533460188564,16.670996433026,-5.58257610794549));
#43458=CARTESIAN_POINT('Ctrl Pts',(-19.1406106730191,16.6819679215137,-5.58696256995803));
#43459=CARTESIAN_POINT('Ctrl Pts',(-19.2271742005006,16.6974246482065,-5.59134903197057));
#43460=CARTESIAN_POINT('Ctrl Pts',(-19.3125527301388,16.7172324209243,-5.59573549398311));
#43461=CARTESIAN_POINT('Ctrl Pts',(-19.3940028670669,16.7361288086572,-5.59992012837615));
#43462=CARTESIAN_POINT('Ctrl Pts',(-19.4746778298125,16.7590549809083,-5.60410476276919));
#43463=CARTESIAN_POINT('Ctrl Pts',(-19.5541489559097,16.7859318174286,-5.60828939716224));
#43464=CARTESIAN_POINT('Ctrl Pts',(-19.6335069646957,16.8127703980989,-5.61246807524618));
#43465=CARTESIAN_POINT('Ctrl Pts',(-19.7116641083501,16.8435483273113,-5.61664675333013));
#43466=CARTESIAN_POINT('Ctrl Pts',(-19.7882032486925,16.8781357711075,-5.62082543141408));
#43467=CARTESIAN_POINT('Ctrl Pts',(-19.8661142981178,16.9133431699762,-5.62507900929951));
#43468=CARTESIAN_POINT('Ctrl Pts',(-19.9423482986085,16.9524978888715,-5.62933258718495));
#43469=CARTESIAN_POINT('Ctrl Pts',(-20.0164828014234,16.995410267208,-5.63358616507039));
#43470=CARTESIAN_POINT('Ctrl Pts',(-20.0891800622395,17.0374907053539,-5.63775727904834));
#43471=CARTESIAN_POINT('Ctrl Pts',(-20.15985808817,17.0831841629369,-5.64192839302629));
#43472=CARTESIAN_POINT('Ctrl Pts',(-20.2281415862035,17.1322645862503,-5.64609950700424));
#43473=CARTESIAN_POINT('Ctrl Pts',(-20.2964021710499,17.1813285401536,-5.65026922132462));
#43474=CARTESIAN_POINT('Ctrl Pts',(-20.3622694505382,17.2337769343483,-5.65443893564499));
#43475=CARTESIAN_POINT('Ctrl Pts',(-20.4253973801086,17.289340586222,-5.65860864996537));
#43476=CARTESIAN_POINT('Ctrl Pts',(-20.4885230633163,17.3449022609025,-5.66277821590942));
#43477=CARTESIAN_POINT('Ctrl Pts',(-20.5489092456572,17.4035786682711,-5.66694778185346));
#43478=CARTESIAN_POINT('Ctrl Pts',(-20.6062442778987,17.4650614661805,-5.67111734779751));
#43479=CARTESIAN_POINT('Ctrl Pts',(-20.6655951391432,17.5287059234172,-5.67543351053643));
#43480=CARTESIAN_POINT('Ctrl Pts',(-20.7216759416723,17.5953574026464,-5.67974967327535));
#43481=CARTESIAN_POINT('Ctrl Pts',(-20.7741852955296,17.6646352435778,-5.68406583601427));
#43482=CARTESIAN_POINT('Ctrl Pts',(-20.8249841627081,17.7316563661277,-5.68824140020596));
#43483=CARTESIAN_POINT('Ctrl Pts',(-20.8724404611874,17.8011349549806,-5.69241696439764));
#43484=CARTESIAN_POINT('Ctrl Pts',(-20.9163256700512,17.872697093392,-5.69659252858933));
#43485=CARTESIAN_POINT('Ctrl Pts',(-20.9624274164875,17.9478736652916,-5.70097899060187));
#43486=CARTESIAN_POINT('Ctrl Pts',(-21.004587562026,18.0253492855826,-5.7053654526144));
#43487=CARTESIAN_POINT('Ctrl Pts',(-21.0425969786767,18.1046637084301,-5.70975191462694));
#43488=CARTESIAN_POINT('Ctrl Pts',(-21.0806063953274,18.1839781312776,-5.71413837663948));
#43489=CARTESIAN_POINT('Ctrl Pts',(-21.1144649298774,18.2651307919131,-5.71852483865201));
#43490=CARTESIAN_POINT('Ctrl Pts',(-21.1440235064309,18.3476421955815,-5.72291130066455));
#43491=CARTESIAN_POINT('Ctrl Pts',(-21.1768030234133,18.4391447059575,-5.72777574688617));
#43492=CARTESIAN_POINT('Ctrl Pts',(-21.2043967060816,18.5325974942123,-5.73264019310779));
#43493=CARTESIAN_POINT('Ctrl Pts',(-21.2266026211952,18.6274486545204,-5.73750463932941));
#43494=CARTESIAN_POINT('Ctrl Pts',(-21.2488226674981,18.722360175309,-5.74237218114112));
#43495=CARTESIAN_POINT('Ctrl Pts',(-21.2656479288592,18.818671733481,-5.74723972295282));
#43496=CARTESIAN_POINT('Ctrl Pts',(-21.2769239065508,18.9158085274062,-5.75210726476452));
#43497=CARTESIAN_POINT('Ctrl Pts',(-21.2881998842425,19.0129453213313,-5.75697480657622));
#43498=CARTESIAN_POINT('Ctrl Pts',(-21.2939263955806,19.1109072194806,-5.76184234838792));
#43499=CARTESIAN_POINT('Ctrl Pts',(-21.2939992944986,19.2090994299067,-5.76670989019962));
#43500=CARTESIAN_POINT('Origin',(-18.734,19.211,1.76670989022852));
#43501=CARTESIAN_POINT('',(-17.1718943259277,21.2444859191102,-4.45010592489447));
#43502=CARTESIAN_POINT('',(-17.1769969560721,21.2378276429927,-4.51667469528573));
#43503=CARTESIAN_POINT('',(-17.1744642439897,21.2411350264762,1.76670989022852));
#43504=CARTESIAN_POINT('',(-21.2938494844892,19.2121967450766,-5.03329016024561));
#43505=CARTESIAN_POINT('Ctrl Pts',(-17.1769969560721,21.2378276429927,-4.51667469528573));
#43506=CARTESIAN_POINT('Ctrl Pts',(-16.8552506533971,20.9913954821563,-4.53675462507165));
#43507=CARTESIAN_POINT('Ctrl Pts',(-16.0276177501346,20.0000800476404,-4.59922649041805));
#43508=CARTESIAN_POINT('Ctrl Pts',(-16.1629699362253,17.6131589033056,-4.70409029132493));
#43509=CARTESIAN_POINT('Ctrl Pts',(-18.685881688405,16.1842895105068,-4.83126609800637));
#43510=CARTESIAN_POINT('Ctrl Pts',(-20.9008595855074,17.3473638996065,-4.94099937082188));
#43511=CARTESIAN_POINT('Ctrl Pts',(-21.288210327615,18.7088774717577,-5.00834070807693));
#43512=CARTESIAN_POINT('Ctrl Pts',(-21.2903253369841,19.2121940792196,-5.0332901097715));
#43513=CARTESIAN_POINT('Ctrl Pts',(-21.2939997202205,19.2121968587231,-5.03329016239734));
#43514=CARTESIAN_POINT('Ctrl Pts',(-21.293956476523,19.3046921979846,-5.03786858507676));
#43515=CARTESIAN_POINT('Ctrl Pts',(-21.2888961385951,19.397020737122,-5.04244700775617));
#43516=CARTESIAN_POINT('Ctrl Pts',(-21.2788976615039,19.4886614709891,-5.04702543043559));
#43517=CARTESIAN_POINT('Ctrl Pts',(-21.2688681118718,19.5805869992732,-5.0516180816045));
#43518=CARTESIAN_POINT('Ctrl Pts',(-21.2538698091613,19.6718201549447,-5.0562107327734));
#43519=CARTESIAN_POINT('Ctrl Pts',(-21.234032630531,19.7618510200409,-5.0608033839423));
#43520=CARTESIAN_POINT('Ctrl Pts',(-21.2141037578168,19.8522980379506,-5.06541726388317));
#43521=CARTESIAN_POINT('Ctrl Pts',(-21.1892913049467,19.9415313457699,-5.07003114382404));
#43522=CARTESIAN_POINT('Ctrl Pts',(-21.1597755903685,20.0290542678652,-5.07464502376491));
#43523=CARTESIAN_POINT('Ctrl Pts',(-21.1363775884239,20.0984363421481,-5.07830258629969));
#43524=CARTESIAN_POINT('Ctrl Pts',(-21.1100249393954,20.1667439285117,-5.08196014883446));
#43525=CARTESIAN_POINT('Ctrl Pts',(-21.0808281256645,20.233740313369,-5.08561771136923));
#43526=CARTESIAN_POINT('Ctrl Pts',(-21.0474239145965,20.3103911904541,-5.08980234576228));
#43527=CARTESIAN_POINT('Ctrl Pts',(-21.010198294198,20.3855464442561,-5.09398698015533));
#43528=CARTESIAN_POINT('Ctrl Pts',(-20.9693070771846,20.458798970463,-5.09817161454838));
#43529=CARTESIAN_POINT('Ctrl Pts',(-20.9284740637573,20.5319472307656,-5.10235029263232));
#43530=CARTESIAN_POINT('Ctrl Pts',(-20.8839860396698,20.6031977447538,-5.10652897071627));
#43531=CARTESIAN_POINT('Ctrl Pts',(-20.8360465870689,20.6721639695093,-5.11070764880021));
#43532=CARTESIAN_POINT('Ctrl Pts',(-20.7872478542335,20.7423663642784,-5.11496122668564));
#43533=CARTESIAN_POINT('Ctrl Pts',(-20.734872934752,20.8102013305707,-5.11921480457108));
#43534=CARTESIAN_POINT('Ctrl Pts',(-20.6791852047648,20.8752879916541,-5.12346838245652));
#43535=CARTESIAN_POINT('Ctrl Pts',(-20.6245770900892,20.9391128208061,-5.12763949643447));
#43536=CARTESIAN_POINT('Ctrl Pts',(-20.5667837820758,21.0002945906742,-5.13181061041242));
#43537=CARTESIAN_POINT('Ctrl Pts',(-20.506095860174,21.0585054160554,-5.13598172439037));
#43538=CARTESIAN_POINT('Ctrl Pts',(-20.4454283026906,21.1166967082319,-5.14015143871074));
#43539=CARTESIAN_POINT('Ctrl Pts',(-20.381868392088,21.1719187176573,-5.14432115303111));
#43540=CARTESIAN_POINT('Ctrl Pts',(-20.3157437934275,21.2238801683045,-5.14849086735148));
#43541=CARTESIAN_POINT('Ctrl Pts',(-20.249621547764,21.2758397699403,-5.15266043329553));
#43542=CARTESIAN_POINT('Ctrl Pts',(-20.1809351577379,21.324538759915,-5.15682999923957));
#43543=CARTESIAN_POINT('Ctrl Pts',(-20.1100445342431,21.3697268098997,-5.16099956518362));
#43544=CARTESIAN_POINT('Ctrl Pts',(-20.0366614838793,21.4165036159763,-5.16531572792254));
#43545=CARTESIAN_POINT('Ctrl Pts',(-19.9609167591476,21.4595177156539,-5.16963189066146));
#43546=CARTESIAN_POINT('Ctrl Pts',(-19.8832395142305,21.4985420299813,-5.17394805340038));
#43547=CARTESIAN_POINT('Ctrl Pts',(-19.8080925973964,21.5362951313742,-5.17812361759206));
#43548=CARTESIAN_POINT('Ctrl Pts',(-19.7311375805023,21.5703142429022,-5.18229918178374));
#43549=CARTESIAN_POINT('Ctrl Pts',(-19.6527837251098,21.6004427104397,-5.18647474597542));
#43550=CARTESIAN_POINT('Ctrl Pts',(-19.5704724027501,21.6320928952489,-5.19086120798796));
#43551=CARTESIAN_POINT('Ctrl Pts',(-19.4866177726056,21.6594488930308,-5.1952476700005));
#43552=CARTESIAN_POINT('Ctrl Pts',(-19.401710454222,21.6823888300554,-5.19963413201304));
#43553=CARTESIAN_POINT('Ctrl Pts',(-19.3168031358385,21.7053287670799,-5.20402059402559));
#43554=CARTESIAN_POINT('Ctrl Pts',(-19.2308437124363,21.723852595477,-5.20840705603813));
#43555=CARTESIAN_POINT('Ctrl Pts',(-19.1443308019265,21.7379009939035,-5.21279351805067));
#43556=CARTESIAN_POINT('Ctrl Pts',(-19.0590101810525,21.7517557823849,-5.2171195274306));
#43557=CARTESIAN_POINT('Ctrl Pts',(-18.9728228912871,21.7613111055906,-5.22144553681052));
#43558=CARTESIAN_POINT('Ctrl Pts',(-18.8862405443866,21.7664691969665,-5.22577154619045));
#43559=CARTESIAN_POINT('Ctrl Pts',(-18.8026253778788,21.7714505203506,-5.22994930306083));
#43560=CARTESIAN_POINT('Ctrl Pts',(-18.7186422980839,21.7723310237495,-5.2341270599312));
#43561=CARTESIAN_POINT('Ctrl Pts',(-18.6347264664641,21.7690744253323,-5.23830481680158));
#43562=CARTESIAN_POINT('Ctrl Pts',(-18.5508928335468,21.7658210168754,-5.24247848140252));
#43563=CARTESIAN_POINT('Ctrl Pts',(-18.4671267750382,21.7584385707795,-5.24665214600345));
#43564=CARTESIAN_POINT('Ctrl Pts',(-18.3838655165602,21.7469427918441,-5.25082581060438));
#43565=CARTESIAN_POINT('Ctrl Pts',(-18.3006608358562,21.735454824532,-5.25499663911255));
#43566=CARTESIAN_POINT('Ctrl Pts',(-18.217960728171,21.7198591392685,-5.25916746762072));
#43567=CARTESIAN_POINT('Ctrl Pts',(-18.1361979890339,21.7002233237869,-5.26333829612888));
#43568=CARTESIAN_POINT('Ctrl Pts',(-18.0544662814438,21.6805949607188,-5.26750754167564));
#43569=CARTESIAN_POINT('Ctrl Pts',(-17.9736716819021,21.6569296230204,-5.27167678722239));
#43570=CARTESIAN_POINT('Ctrl Pts',(-17.894236126945,21.6293458473741,-5.27584603276915));
#43571=CARTESIAN_POINT('Ctrl Pts',(-17.8147812397687,21.6017553586685,-5.28001629298458));
#43572=CARTESIAN_POINT('Ctrl Pts',(-17.7366864944959,21.5702446726599,-5.28418655320001));
#43573=CARTESIAN_POINT('Ctrl Pts',(-17.6603571013659,21.5349816966174,-5.28835681341544));
#43574=CARTESIAN_POINT('Ctrl Pts',(-17.5840157675873,21.4997132041835,-5.29252772600881));
#43575=CARTESIAN_POINT('Ctrl Pts',(-17.5094407480921,21.4606914573206,-5.29669863860218));
#43576=CARTESIAN_POINT('Ctrl Pts',(-17.4370140541151,21.418131046444,-5.30086955119554));
#43577=CARTESIAN_POINT('Ctrl Pts',(-17.3645257193928,21.3755344133502,-5.30504401355968));
#43578=CARTESIAN_POINT('Ctrl Pts',(-17.294189747792,21.3293933517496,-5.30921847592382));
#43579=CARTESIAN_POINT('Ctrl Pts',(-17.2263597646639,21.2799661478129,-5.31339293828795));
#43580=CARTESIAN_POINT('Ctrl Pts',(-17.2088933668714,21.2672385137208,-5.31446787324827));
#43581=CARTESIAN_POINT('Ctrl Pts',(-17.1915929675281,21.254293194019,-5.31554280820858));
#43582=CARTESIAN_POINT('Ctrl Pts',(-17.1744642439897,21.2411350264762,-5.31661774316889));
#43583=CARTESIAN_POINT('',(-21.2942631007509,19.2101644346482,-4.96670989022851));
#43584=CARTESIAN_POINT('Ctrl Pts',(-21.2939998636668,19.210164520558,-4.96670989022851));
#43585=CARTESIAN_POINT('Ctrl Pts',(-21.2940269378475,19.2931227545131,-4.97085977152528));
#43586=CARTESIAN_POINT('Ctrl Pts',(-21.2900172964774,19.3762448671897,-4.97500965282206));
#43587=CARTESIAN_POINT('Ctrl Pts',(-21.2819493183893,19.4591013319584,-4.97915953411883));
#43588=CARTESIAN_POINT('Ctrl Pts',(-21.273892503302,19.5418431550195,-4.98330367356457));
#43589=CARTESIAN_POINT('Ctrl Pts',(-21.2617885455564,19.6243195978693,-4.9874478130103));
#43590=CARTESIAN_POINT('Ctrl Pts',(-21.2456678375727,19.7061006702713,-4.99159195245604));
#43591=CARTESIAN_POINT('Ctrl Pts',(-21.2295645603718,19.787793315532,-4.99573161098226));
#43592=CARTESIAN_POINT('Ctrl Pts',(-21.2094532518121,19.8687916269892,-4.99987126950847));
#43593=CARTESIAN_POINT('Ctrl Pts',(-21.185415992005,19.9486717658566,-5.00401092803468));
#43594=CARTESIAN_POINT('Ctrl Pts',(-21.1613926712712,20.0285055826756,-5.00814818599593));
#43595=CARTESIAN_POINT('Ctrl Pts',(-21.1334480518402,20.1072220663071,-5.01228544395718));
#43596=CARTESIAN_POINT('Ctrl Pts',(-21.1017147974227,20.1844097996556,-5.01642270191842));
#43597=CARTESIAN_POINT('Ctrl Pts',(-21.0699900384709,20.2615768686961,-5.02055885227398));
#43598=CARTESIAN_POINT('Ctrl Pts',(-21.0344788364884,20.3372155671953,-5.02469500262954));
#43599=CARTESIAN_POINT('Ctrl Pts',(-20.9953624823965,20.4109332161455,-5.02883115298509));
#43600=CARTESIAN_POINT('Ctrl Pts',(-20.9562443890678,20.4846541428155,-5.03296748724698));
#43601=CARTESIAN_POINT('Ctrl Pts',(-20.9135210465748,20.5564534375451,-5.03710382150886));
#43602=CARTESIAN_POINT('Ctrl Pts',(-20.8674196102005,20.6259631680054,-5.04124015577075));
#43603=CARTESIAN_POINT('Ctrl Pts',(-20.8212714994521,20.6955432720466,-5.04538067777227));
#43604=CARTESIAN_POINT('Ctrl Pts',(-20.7717387262307,20.7628287929985,-5.0495211997738));
#43605=CARTESIAN_POINT('Ctrl Pts',(-20.7190913321275,20.8274814886389,-5.05366172177532));
#43606=CARTESIAN_POINT('Ctrl Pts',(-20.6664157771977,20.8921687666814,-5.05780445852126));
#43607=CARTESIAN_POINT('Ctrl Pts',(-20.6106225991445,20.9542200685987,-5.0619471952672));
#43608=CARTESIAN_POINT('Ctrl Pts',(-20.5520199344765,21.0133327988598,-5.06608993201314));
#43609=CARTESIAN_POINT('Ctrl Pts',(-20.4933173061603,21.0725463628324,-5.07023973538449));
#43610=CARTESIAN_POINT('Ctrl Pts',(-20.4317959684764,21.1288110311776,-5.07438953875584));
#43611=CARTESIAN_POINT('Ctrl Pts',(-20.3677981562815,21.181863664623,-5.07853934212718));
#43612=CARTESIAN_POINT('Ctrl Pts',(-20.3241391698325,21.218055905033,-5.08137031717058));
#43613=CARTESIAN_POINT('Ctrl Pts',(-20.2793283343472,21.252754156268,-5.08420129221397));
#43614=CARTESIAN_POINT('Ctrl Pts',(-20.2334815623284,21.2858867545572,-5.08703226725737));
#43615=CARTESIAN_POINT('Ctrl Pts',(-20.165712692572,21.3348620398235,-5.09121690165042));
#43616=CARTESIAN_POINT('Ctrl Pts',(-20.0954157767524,21.38060482739,-5.09540153604347));
#43617=CARTESIAN_POINT('Ctrl Pts',(-20.0229321512534,21.4228440065848,-5.09958617043652));
#43618=CARTESIAN_POINT('Ctrl Pts',(-19.9505516972235,21.4650230635363,-5.10376484852047));
#43619=CARTESIAN_POINT('Ctrl Pts',(-19.875991110009,21.5037081881332,-5.10794352660443));
#43620=CARTESIAN_POINT('Ctrl Pts',(-19.7996223782739,21.5386702831204,-5.11212220468838));
#43621=CARTESIAN_POINT('Ctrl Pts',(-19.7218847919078,21.5742590485334,-5.11637578257381));
#43622=CARTESIAN_POINT('Ctrl Pts',(-19.642273992229,21.6059897185087,-5.12062936045925));
#43623=CARTESIAN_POINT('Ctrl Pts',(-19.5612105522304,21.6336685085415,-5.12488293834468));
#43624=CARTESIAN_POINT('Ctrl Pts',(-19.4817186851983,21.6608106912188,-5.12905405232263));
#43625=CARTESIAN_POINT('Ctrl Pts',(-19.4008304551544,21.6840565436591,-5.13322516630058));
#43626=CARTESIAN_POINT('Ctrl Pts',(-19.3189628776791,21.7032717411505,-5.13739628027853));
#43627=CARTESIAN_POINT('Ctrl Pts',(-19.2371227716599,21.7224804907969,-5.14156599459891));
#43628=CARTESIAN_POINT('Ctrl Pts',(-19.1543044183623,21.7376611666004,-5.14573570891929));
#43629=CARTESIAN_POINT('Ctrl Pts',(-19.0709381209922,21.7487298324728,-5.14990542323966));
#43630=CARTESIAN_POINT('Ctrl Pts',(-18.9875747901529,21.7597981044745,-5.15407498918371));
#43631=CARTESIAN_POINT('Ctrl Pts',(-18.9036640101517,21.7667545977695,-5.15824455512775));
#43632=CARTESIAN_POINT('Ctrl Pts',(-18.819642997584,21.7695670358552,-5.16241412107179));
#43633=CARTESIAN_POINT('Ctrl Pts',(-18.7326679098656,21.7724783557944,-5.16673028381071));
#43634=CARTESIAN_POINT('Ctrl Pts',(-18.6455752209303,21.7709487709587,-5.17104644654963));
#43635=CARTESIAN_POINT('Ctrl Pts',(-18.5588499153533,21.7650012623036,-5.17536260928855));
#43636=CARTESIAN_POINT('Ctrl Pts',(-18.4749496774835,21.7592474931173,-5.17953817348023));
#43637=CARTESIAN_POINT('Ctrl Pts',(-18.3913937177404,21.749359309981,-5.18371373767191));
#43638=CARTESIAN_POINT('Ctrl Pts',(-18.3086140512033,21.7354101874629,-5.18788930186359));
#43639=CARTESIAN_POINT('Ctrl Pts',(-18.2216533804995,21.7207565279272,-5.19227576387613));
#43640=CARTESIAN_POINT('Ctrl Pts',(-18.1355500550633,21.701621038382,-5.19666222588866));
#43641=CARTESIAN_POINT('Ctrl Pts',(-18.0507884164764,21.6781485427795,-5.2010486879012));
#43642=CARTESIAN_POINT('Ctrl Pts',(-17.9660267778894,21.654676047177,-5.20543514991373));
#43643=CARTESIAN_POINT('Ctrl Pts',(-17.8826073525323,21.6268668011753,-5.20982161192627));
#43644=CARTESIAN_POINT('Ctrl Pts',(-17.8009895271363,21.5949235427183,-5.21420807393881));
#43645=CARTESIAN_POINT('Ctrl Pts',(-17.723133526371,21.5644525721575,-5.21839236074317));
#43646=CARTESIAN_POINT('Ctrl Pts',(-17.6466269368319,21.5301068697023,-5.22257664754754));
#43647=CARTESIAN_POINT('Ctrl Pts',(-17.5718823763611,21.4920266611392,-5.2267609343519));
#43648=CARTESIAN_POINT('Ctrl Pts',(-17.497252122809,21.4540046886708,-5.23093882212296));
#43649=CARTESIAN_POINT('Ctrl Pts',(-17.4243789496118,21.4122597663377,-5.23511670989402));
#43650=CARTESIAN_POINT('Ctrl Pts',(-17.3536566218709,21.3669805561403,-5.23929459766508));
#43651=CARTESIAN_POINT('Ctrl Pts',(-17.2922215801368,21.327647430987,-5.24292384344607));
#43652=CARTESIAN_POINT('Ctrl Pts',(-17.2324094767135,21.2856481554772,-5.24655308922706));
#43653=CARTESIAN_POINT('Ctrl Pts',(-17.1744642439897,21.2411350264762,-5.25018233500805));
#43654=CARTESIAN_POINT('Ctrl Pts',(-17.1718943259273,21.2444859191099,-4.45010592489449));
#43655=CARTESIAN_POINT('Ctrl Pts',(-17.1663500721053,21.2402338685243,-4.45045502787973));
#43656=CARTESIAN_POINT('Ctrl Pts',(-16.4898974816279,20.7166175504919,-4.49319606642544));
#43657=CARTESIAN_POINT('Ctrl Pts',(-15.7195027796251,18.9351410654681,-4.57832904053163));
#43658=CARTESIAN_POINT('Ctrl Pts',(-17.3342635373914,16.5269676830084,-4.70550484721307));
#43659=CARTESIAN_POINT('Ctrl Pts',(-20.2331956221585,16.5812273615557,-4.8326806538945));
#43660=CARTESIAN_POINT('Ctrl Pts',(-21.2762381336493,18.2701494254144,-4.91974900156631));
#43661=CARTESIAN_POINT('Ctrl Pts',(-21.2980949765117,19.1644257538227,-4.96442541367765));
#43662=CARTESIAN_POINT('Ctrl Pts',(-21.2979002687903,19.210163247625,-4.96670989022851));
#43663=CARTESIAN_POINT('Origin',(-18.734,19.211,1.76670989022852));
#43664=CARTESIAN_POINT('',(-17.1744642439897,21.2411350264762,-3.6500459524789));
#43665=CARTESIAN_POINT('',(-17.1744642439897,21.2411350264762,-3.71676814526475));
#43666=CARTESIAN_POINT('',(-17.1744642439897,21.2411350264762,1.76670989022852));
#43667=CARTESIAN_POINT('',(-21.2939990418858,19.2087851537695,-4.23329008725203));
#43668=CARTESIAN_POINT('Ctrl Pts',(-17.1744642439897,21.2411350264762,-3.71676814526475));
#43669=CARTESIAN_POINT('Ctrl Pts',(-17.1078988246138,21.1899999294128,-3.72094075707419));
#43670=CARTESIAN_POINT('Ctrl Pts',(-17.0437864698061,21.1355379119879,-3.72511336888363));
#43671=CARTESIAN_POINT('Ctrl Pts',(-16.9824731010997,21.0780172796277,-3.72928598069307));
#43672=CARTESIAN_POINT('Ctrl Pts',(-16.9211917165634,21.0205266529536,-3.73345641585606));
#43673=CARTESIAN_POINT('Ctrl Pts',(-16.8627067539701,20.9599808934146,-3.73762685101905));
#43674=CARTESIAN_POINT('Ctrl Pts',(-16.8073301828919,20.8966878168405,-3.74179728618204));
#43675=CARTESIAN_POINT('Ctrl Pts',(-16.7519658872628,20.8334087705851,-3.74596679687528));
#43676=CARTESIAN_POINT('Ctrl Pts',(-16.6997089170967,20.7673839632324,-3.75013630756853));
#43677=CARTESIAN_POINT('Ctrl Pts',(-16.6508326185409,20.6989562025896,-3.75430581826177));
#43678=CARTESIAN_POINT('Ctrl Pts',(-16.6019524929159,20.630523083976,-3.75847565543239));
#43679=CARTESIAN_POINT('Ctrl Pts',(-16.5564538308376,20.5596870135816,-3.76264549260301));
#43680=CARTESIAN_POINT('Ctrl Pts',(-16.5145672996359,20.4868207117594,-3.76681532977363));
#43681=CARTESIAN_POINT('Ctrl Pts',(-16.4726368702626,20.4138780441624,-3.77098953704179));
#43682=CARTESIAN_POINT('Ctrl Pts',(-16.4343263606549,20.3389012961015,-3.77516374430996));
#43683=CARTESIAN_POINT('Ctrl Pts',(-16.3998207425502,20.262288349641,-3.77933795157812));
#43684=CARTESIAN_POINT('Ctrl Pts',(-16.365296388734,20.1856338042138,-3.78351442533932));
#43685=CARTESIAN_POINT('Ctrl Pts',(-16.3345812083815,20.1073417197765,-3.78769089910052));
#43686=CARTESIAN_POINT('Ctrl Pts',(-16.3078113066412,20.0278282709468,-3.79186737286172));
#43687=CARTESIAN_POINT('Ctrl Pts',(-16.2809949059668,19.9481767084005,-3.79605110109774));
#43688=CARTESIAN_POINT('Ctrl Pts',(-16.2581375967678,19.8672999871918,-3.80023482933376));
#43689=CARTESIAN_POINT('Ctrl Pts',(-16.2393250174113,19.7856274717117,-3.80441855756978));
#43690=CARTESIAN_POINT('Ctrl Pts',(-16.2251740665448,19.7241928469432,-3.80756558656482));
#43691=CARTESIAN_POINT('Ctrl Pts',(-16.2133106294126,19.6623082203732,-3.81071261555985));
#43692=CARTESIAN_POINT('Ctrl Pts',(-16.2037517912764,19.6001580684646,-3.81385964455489));
#43693=CARTESIAN_POINT('Ctrl Pts',(-16.1910413132713,19.5175164202231,-3.81804427894799));
#43694=CARTESIAN_POINT('Ctrl Pts',(-16.182360236898,19.4340976099864,-3.8222289133411));
#43695=CARTESIAN_POINT('Ctrl Pts',(-16.1777943305988,19.3503290196653,-3.8264135477342));
#43696=CARTESIAN_POINT('Ctrl Pts',(-16.1732349233019,19.266679663564,-3.8305922258182));
#43697=CARTESIAN_POINT('Ctrl Pts',(-16.1727790761929,19.1826819717243,-3.8347709039022));
#43698=CARTESIAN_POINT('Ctrl Pts',(-16.1764611917473,19.0987714640513,-3.8389495819862));
#43699=CARTESIAN_POINT('Ctrl Pts',(-16.1802093065766,19.0133569208352,-3.84320315987162));
#43700=CARTESIAN_POINT('Ctrl Pts',(-16.1882452624471,18.9280331946169,-3.84745673775704));
#43701=CARTESIAN_POINT('Ctrl Pts',(-16.2005498883094,18.8432629586585,-3.85171031564246));
#43702=CARTESIAN_POINT('Ctrl Pts',(-16.212615964989,18.7601361591384,-3.85588142962047));
#43703=CARTESIAN_POINT('Ctrl Pts',(-16.2287866065491,18.6775420566428,-3.86005254359848));
#43704=CARTESIAN_POINT('Ctrl Pts',(-16.2489913365583,18.5959130609259,-3.86422365757649));
#43705=CARTESIAN_POINT('Ctrl Pts',(-16.2691892866751,18.5143114566068,-3.86839337189693));
#43706=CARTESIAN_POINT('Ctrl Pts',(-16.293418526377,18.4336747620786,-3.87256308621736));
#43707=CARTESIAN_POINT('Ctrl Pts',(-16.3215576717042,18.3544242516587,-3.87673280053779));
#43708=CARTESIAN_POINT('Ctrl Pts',(-16.3496958157198,18.275176561312,-3.8809023664819));
#43709=CARTESIAN_POINT('Ctrl Pts',(-16.3817434340021,18.1973153902317,-3.885071932426));
#43710=CARTESIAN_POINT('Ctrl Pts',(-16.4175300086123,18.1212446242388,-3.88924149837011));
#43711=CARTESIAN_POINT('Ctrl Pts',(-16.4545747950371,18.0424993039595,-3.89355766110896));
#43712=CARTESIAN_POINT('Ctrl Pts',(-16.4956261286209,17.9656731098166,-3.89787382384781));
#43713=CARTESIAN_POINT('Ctrl Pts',(-16.5404425366712,17.8911872651491,-3.90218998658667));
#43714=CARTESIAN_POINT('Ctrl Pts',(-16.5837990549445,17.8191277890349,-3.9063655507784));
#43715=CARTESIAN_POINT('Ctrl Pts',(-16.6306788183653,17.7492588949824,-3.91054111497015));
#43716=CARTESIAN_POINT('Ctrl Pts',(-16.6808195479048,17.681931646023,-3.91471667916188));
#43717=CARTESIAN_POINT('Ctrl Pts',(-16.7334927664927,17.6112038577771,-3.91910314117429));
#43718=CARTESIAN_POINT('Ctrl Pts',(-16.789764658884,17.5432816689319,-3.9234896031867));
#43719=CARTESIAN_POINT('Ctrl Pts',(-16.8492855900871,17.4785302042844,-3.92787606519911));
#43720=CARTESIAN_POINT('Ctrl Pts',(-16.9088065212903,17.413778739637,-3.93226252721152));
#43721=CARTESIAN_POINT('Ctrl Pts',(-16.9715760238564,17.3521983512228,-3.93664898922392));
#43722=CARTESIAN_POINT('Ctrl Pts',(-17.0372042845901,17.2941055584184,-3.94103545123633));
#43723=CARTESIAN_POINT('Ctrl Pts',(-17.0998128917648,17.2386857011235,-3.94522008562937));
#43724=CARTESIAN_POINT('Ctrl Pts',(-17.1652560078683,17.1862332698863,-3.9494047200224));
#43725=CARTESIAN_POINT('Ctrl Pts',(-17.2332206971797,17.1370517161158,-3.95358935441543));
#43726=CARTESIAN_POINT('Ctrl Pts',(-17.3010886471682,17.0879401661996,-3.95776803249936));
#43727=CARTESIAN_POINT('Ctrl Pts',(-17.3714706716869,17.0420905134701,-3.96194671058329));
#43728=CARTESIAN_POINT('Ctrl Pts',(-17.4440191888255,16.9997674236297,-3.96612538866722));
#43729=CARTESIAN_POINT('Ctrl Pts',(-17.5178680859944,16.9566857228207,-3.97037896655266));
#43730=CARTESIAN_POINT('Ctrl Pts',(-17.5939615474704,16.9172585752801,-3.9746325444381));
#43731=CARTESIAN_POINT('Ctrl Pts',(-17.6719001613345,16.881720297451,-3.97888612232354));
#43732=CARTESIAN_POINT('Ctrl Pts',(-17.7483277830838,16.846870998485,-3.98305723630147));
#43733=CARTESIAN_POINT('Ctrl Pts',(-17.8265292140571,16.815761327818,-3.98722835027941));
#43734=CARTESIAN_POINT('Ctrl Pts',(-17.9061027185259,16.7885660811226,-3.99139946425735));
#43735=CARTESIAN_POINT('Ctrl Pts',(-17.9856495213366,16.761379960055,-3.9955691785777));
#43736=CARTESIAN_POINT('Ctrl Pts',(-18.0665670483063,16.7381058029316,-3.99973889289804));
#43737=CARTESIAN_POINT('Ctrl Pts',(-18.1484353715671,16.7188695728497,-4.00390860721839));
#43738=CARTESIAN_POINT('Ctrl Pts',(-18.2303007816016,16.6996340272755,-4.00807817316241));
#43739=CARTESIAN_POINT('Ctrl Pts',(-18.313116472626,16.6844362274532,-4.01224773910643));
#43740=CARTESIAN_POINT('Ctrl Pts',(-18.3964505424551,16.6733514105158,-4.01641730505044));
#43741=CARTESIAN_POINT('Ctrl Pts',(-18.4827145353766,16.6618768650894,-4.02073346778938));
#43742=CARTESIAN_POINT('Ctrl Pts',(-18.5695335149127,16.6548099783526,-4.02504963052833));
#43743=CARTESIAN_POINT('Ctrl Pts',(-18.6564225943068,16.6521757101892,-4.02936579326727));
#43744=CARTESIAN_POINT('Ctrl Pts',(-18.7404812710779,16.6496272530341,-4.03354135745893));
#43745=CARTESIAN_POINT('Ctrl Pts',(-18.8246050807771,16.6512270080048,-4.03771692165059));
#43746=CARTESIAN_POINT('Ctrl Pts',(-18.9083568682879,16.6569444637047,-4.04189248584225));
#43747=CARTESIAN_POINT('Ctrl Pts',(-18.9963387594864,16.6629506945001,-4.04627894785483));
#43748=CARTESIAN_POINT('Ctrl Pts',(-19.08390947946,16.6735014582054,-4.05066540986742));
#43749=CARTESIAN_POINT('Ctrl Pts',(-19.1705727652473,16.6885004022509,-4.05505187188));
#43750=CARTESIAN_POINT('Ctrl Pts',(-19.2572360510346,16.7034993462965,-4.05943833389259));
#43751=CARTESIAN_POINT('Ctrl Pts',(-19.342991353608,16.7229462681819,-4.06382479590517));
#43752=CARTESIAN_POINT('Ctrl Pts',(-19.4273615317729,16.7466847226344,-4.06821125791776));
#43753=CARTESIAN_POINT('Ctrl Pts',(-19.5078497129729,16.7693309356085,-4.0723958923108));
#43754=CARTESIAN_POINT('Ctrl Pts',(-19.5873770243864,16.7959667334644,-4.07658052670384));
#43755=CARTESIAN_POINT('Ctrl Pts',(-19.6655189252299,16.826493239276,-4.08076516109689));
#43756=CARTESIAN_POINT('Ctrl Pts',(-19.7435496007498,16.8569762943851,-4.08494383918084));
#43757=CARTESIAN_POINT('Ctrl Pts',(-19.8201983578021,16.8913388913937,-4.08912251726478));
#43758=CARTESIAN_POINT('Ctrl Pts',(-19.8950545149197,16.9294320274459,-4.09330119534873));
#43759=CARTESIAN_POINT('Ctrl Pts',(-19.9712524148554,16.9682079555848,-4.09755477323417));
#43760=CARTESIAN_POINT('Ctrl Pts',(-20.0455923539259,17.0108493474662,-4.1018083511196));
#43761=CARTESIAN_POINT('Ctrl Pts',(-20.1176611149876,17.0571471919207,-4.10606192900504));
#43762=CARTESIAN_POINT('Ctrl Pts',(-20.1883326824854,17.1025474623176,-4.11023304298298));
#43763=CARTESIAN_POINT('Ctrl Pts',(-20.2568199436827,17.1514634154309,-4.11440415696093));
#43764=CARTESIAN_POINT('Ctrl Pts',(-20.3227584711506,17.2036518686717,-4.11857527093887));
#43765=CARTESIAN_POINT('Ctrl Pts',(-20.3886748723087,17.2558228095729,-4.12274498525924));
#43766=CARTESIAN_POINT('Ctrl Pts',(-20.4520438778608,17.3112637844568,-4.1269146995796));
#43767=CARTESIAN_POINT('Ctrl Pts',(-20.5125322737859,17.369689881877,-4.13108441389996));
#43768=CARTESIAN_POINT('Ctrl Pts',(-20.5730185172743,17.4281139002461,-4.135253979844));
#43769=CARTESIAN_POINT('Ctrl Pts',(-20.6306240246489,17.489522509736,-4.13942354578804));
#43770=CARTESIAN_POINT('Ctrl Pts',(-20.6850517529259,17.5535932733922,-4.14359311173208));
#43771=CARTESIAN_POINT('Ctrl Pts',(-20.7413930929854,17.6199166860588,-4.14790927447101));
#43772=CARTESIAN_POINT('Ctrl Pts',(-20.7943286933423,17.6890925366906,-4.15222543720993));
#43773=CARTESIAN_POINT('Ctrl Pts',(-20.8435751066798,17.7607266225719,-4.15654159994886));
#43774=CARTESIAN_POINT('Ctrl Pts',(-20.8912173232825,17.83002723564,-4.16071716414053));
#43775=CARTESIAN_POINT('Ctrl Pts',(-20.9354068051749,17.9016279637396,-4.16489272833221));
#43776=CARTESIAN_POINT('Ctrl Pts',(-20.9759325838396,17.9751447133591,-4.16906829252388));
#43777=CARTESIAN_POINT('Ctrl Pts',(-21.018505223244,18.0523746192327,-4.17345475453643));
#43778=CARTESIAN_POINT('Ctrl Pts',(-21.0570340704737,18.1317186646457,-4.17784121654899));
#43779=CARTESIAN_POINT('Ctrl Pts',(-21.0913315250629,18.2127074171643,-4.18222767856154));
#43780=CARTESIAN_POINT('Ctrl Pts',(-21.125628979652,18.2936961696829,-4.18661414057409));
#43781=CARTESIAN_POINT('Ctrl Pts',(-21.1556949146933,18.3763290580522,-4.19100060258664));
#43782=CARTESIAN_POINT('Ctrl Pts',(-21.1814026084241,18.4601202011779,-4.19538706459919));
#43783=CARTESIAN_POINT('Ctrl Pts',(-21.211365847261,18.557781782967,-4.20049964335899));
#43784=CARTESIAN_POINT('Ctrl Pts',(-21.2355013786602,18.6573099274653,-4.20561222211879));
#43785=CARTESIAN_POINT('Ctrl Pts',(-21.2536149670824,18.758075704279,-4.21072480087859));
#43786=CARTESIAN_POINT('Ctrl Pts',(-21.271481685507,18.8574681448711,-4.2157677003304));
#43787=CARTESIAN_POINT('Ctrl Pts',(-21.2834894543748,18.9580647258708,-4.22081059978222));
#43788=CARTESIAN_POINT('Ctrl Pts',(-21.289497836736,19.0592409592887,-4.22585349923404));
#43789=CARTESIAN_POINT('Ctrl Pts',(-21.2924512874047,19.1089746473736,-4.2283323619067));
#43790=CARTESIAN_POINT('Ctrl Pts',(-21.293955837589,19.1588480714825,-4.23081122457936));
#43791=CARTESIAN_POINT('Ctrl Pts',(-21.2939990418858,19.2087851537695,-4.23329008725203));
#43792=CARTESIAN_POINT('Ctrl Pts',(-21.2923873880696,19.2087870015046,-4.2332901097715));
#43793=CARTESIAN_POINT('Ctrl Pts',(-21.2874613882922,19.8078856368616,-4.26304769694121));
#43794=CARTESIAN_POINT('Ctrl Pts',(-20.7784814085672,21.2679844548948,-4.3351972196714));
#43795=CARTESIAN_POINT('Ctrl Pts',(-18.7708037338048,22.0472233474103,-4.42965874817614));
#43796=CARTESIAN_POINT('Ctrl Pts',(-17.5345084334408,21.5116530922966,-4.49436268951118));
#43797=CARTESIAN_POINT('Ctrl Pts',(-17.1769969560721,21.2378276429927,-4.51667469528573));
#43798=CARTESIAN_POINT('',(-21.2939989159607,19.2133559031925,-4.16670989022851));
#43799=CARTESIAN_POINT('Ctrl Pts',(-21.2939117877142,19.2133565885178,-4.16670992830965));
#43800=CARTESIAN_POINT('Ctrl Pts',(-21.2957664845097,19.4149927548523,-4.17674049236887));
#43801=CARTESIAN_POINT('Ctrl Pts',(-21.1817726734028,20.4667260333026,-4.22916299198858));
#43802=CARTESIAN_POINT('Ctrl Pts',(-19.7363287853609,22.0632999679849,-4.32362832418352));
#43803=CARTESIAN_POINT('Ctrl Pts',(-17.8395945320329,21.7565647566733,-4.40806309231925));
#43804=CARTESIAN_POINT('Ctrl Pts',(-17.1718943259273,21.2444859191099,-4.45010592489449));
#43805=CARTESIAN_POINT('Ctrl Pts',(-17.1744642439897,21.2411350264762,-3.6500459524789));
#43806=CARTESIAN_POINT('Ctrl Pts',(-17.1077769031899,21.189906270214,-3.65422167346473));
#43807=CARTESIAN_POINT('Ctrl Pts',(-17.0436659910486,21.1354262971526,-3.65839739445057));
#43808=CARTESIAN_POINT('Ctrl Pts',(-16.9824502029285,21.0779957976329,-3.66257311543641));
#43809=CARTESIAN_POINT('Ctrl Pts',(-16.9200837263783,21.0194857626965,-3.66682732849061));
#43810=CARTESIAN_POINT('Ctrl Pts',(-16.8607226752009,20.9579135054828,-3.6710815415448));
#43811=CARTESIAN_POINT('Ctrl Pts',(-16.8046620408575,20.8936333645247,-3.675335754599));
#43812=CARTESIAN_POINT('Ctrl Pts',(-16.748601406514,20.8293532235666,-3.6795899676532));
#43813=CARTESIAN_POINT('Ctrl Pts',(-16.6958414444482,20.7623656310848,-3.68384418070739));
#43814=CARTESIAN_POINT('Ctrl Pts',(-16.6466304638568,20.6930554711553,-3.68809839376159));
#43815=CARTESIAN_POINT('Ctrl Pts',(-16.5982243404927,20.6248788952851,-3.69228302815505));
#43816=CARTESIAN_POINT('Ctrl Pts',(-16.553071769447,20.5542014284547,-3.69646766254851));
#43817=CARTESIAN_POINT('Ctrl Pts',(-16.511440993796,20.4813666651567,-3.70065229694197));
#43818=CARTESIAN_POINT('Ctrl Pts',(-16.4698694744012,20.408635573129,-3.70483097502633));
#43819=CARTESIAN_POINT('Ctrl Pts',(-16.4318100196567,20.3337536798785,-3.70900965311069));
#43820=CARTESIAN_POINT('Ctrl Pts',(-16.3974886040357,20.2570948793148,-3.71318833119505));
#43821=CARTESIAN_POINT('Ctrl Pts',(-16.3625520017103,20.1790620248544,-3.71744190908038));
#43822=CARTESIAN_POINT('Ctrl Pts',(-16.3314890444374,20.0991883275089,-3.72169548696571));
#43823=CARTESIAN_POINT('Ctrl Pts',(-16.3044899883695,20.0178959681317,-3.72594906485105));
#43824=CARTESIAN_POINT('Ctrl Pts',(-16.2780143616845,19.9381796197598,-3.73012017882943));
#43825=CARTESIAN_POINT('Ctrl Pts',(-16.2554466207297,19.8570995822358,-3.73429129280781));
#43826=CARTESIAN_POINT('Ctrl Pts',(-16.2369175937363,19.7750739812545,-3.7384624067862));
#43827=CARTESIAN_POINT('Ctrl Pts',(-16.2183947843369,19.6930759047558,-3.74263212110701));
#43828=CARTESIAN_POINT('Ctrl Pts',(-16.2039080986716,19.6101333433017,-3.74680183542781));
#43829=CARTESIAN_POINT('Ctrl Pts',(-16.1935378668542,19.5266772878308,-3.75097154974862));
#43830=CARTESIAN_POINT('Ctrl Pts',(-16.1831680040541,19.4432242020846,-3.7551411156931));
#43831=CARTESIAN_POINT('Ctrl Pts',(-16.1769143597415,19.3592581152788,-3.75931068163757));
#43832=CARTESIAN_POINT('Ctrl Pts',(-16.174805548368,19.2752164989404,-3.76348024758204));
#43833=CARTESIAN_POINT('Ctrl Pts',(-16.1726225937887,19.1882200830672,-3.76779641032046));
#43834=CARTESIAN_POINT('Ctrl Pts',(-16.1748813730051,19.1011432548622,-3.77211257305887));
#43835=CARTESIAN_POINT('Ctrl Pts',(-16.1815548449752,19.0144707894735,-3.77642873579729));
#43836=CARTESIAN_POINT('Ctrl Pts',(-16.1880109292992,18.9306216705099,-3.78060429998941));
#43837=CARTESIAN_POINT('Ctrl Pts',(-16.1985983999137,18.8471514360449,-3.78477986418153));
#43838=CARTESIAN_POINT('Ctrl Pts',(-16.2132401674604,18.7644914707929,-3.78895542837364));
#43839=CARTESIAN_POINT('Ctrl Pts',(-16.2286214558733,18.6776565472299,-3.79334189038521));
#43840=CARTESIAN_POINT('Ctrl Pts',(-16.24847723842,18.5917164663179,-3.79772835239677));
#43841=CARTESIAN_POINT('Ctrl Pts',(-16.2726586407169,18.5071543400131,-3.80211481440834));
#43842=CARTESIAN_POINT('Ctrl Pts',(-16.2968400430138,18.4225922137084,-3.8065012764199));
#43843=CARTESIAN_POINT('Ctrl Pts',(-16.3253468050043,18.3394085662325,-3.81088773843146));
#43844=CARTESIAN_POINT('Ctrl Pts',(-16.3579723492966,18.2580610706385,-3.81527420044303));
#43845=CARTESIAN_POINT('Ctrl Pts',(-16.3890967439393,18.1804564938875,-3.81945883483596));
#43846=CARTESIAN_POINT('Ctrl Pts',(-16.4240850782656,18.1042339549061,-3.8236434692289));
#43847=CARTESIAN_POINT('Ctrl Pts',(-16.4627936385718,18.029804984853,-3.82782810362184));
#43848=CARTESIAN_POINT('Ctrl Pts',(-16.5014471020336,17.9554819552264,-3.83200678170567));
#43849=CARTESIAN_POINT('Ctrl Pts',(-16.5438100629349,17.8829478282646,-3.8361854597895));
#43850=CARTESIAN_POINT('Ctrl Pts',(-16.5896904513643,17.8125949944205,-3.84036413787333));
#43851=CARTESIAN_POINT('Ctrl Pts',(-16.6363932127842,17.740981136589,-3.84461771575879));
#43852=CARTESIAN_POINT('Ctrl Pts',(-16.6867405623486,17.6716279878895,-3.84887129364426));
#43853=CARTESIAN_POINT('Ctrl Pts',(-16.7404804948183,17.6049240421263,-3.85312487152972));
#43854=CARTESIAN_POINT('Ctrl Pts',(-16.7931785738305,17.5395132825159,-3.85729598550756));
#43855=CARTESIAN_POINT('Ctrl Pts',(-16.8491385640374,17.4766502972939,-3.86146709948541));
#43856=CARTESIAN_POINT('Ctrl Pts',(-16.9080797027397,17.4166714158068,-3.86563821346325));
#43857=CARTESIAN_POINT('Ctrl Pts',(-16.9670010631736,17.3567126608127,-3.8698079277835));
#43858=CARTESIAN_POINT('Ctrl Pts',(-17.0289012632126,17.299636415355,-3.87397764210376));
#43859=CARTESIAN_POINT('Ctrl Pts',(-17.0934613888502,17.2457435115673,-3.87814735642402));
#43860=CARTESIAN_POINT('Ctrl Pts',(-17.1580192171616,17.1918525255203,-3.88231692236795));
#43861=CARTESIAN_POINT('Ctrl Pts',(-17.2252364291767,17.1411449500709,-3.88648648831189));
#43862=CARTESIAN_POINT('Ctrl Pts',(-17.2947606690324,17.0938816404849,-3.89065605425582));
#43863=CARTESIAN_POINT('Ctrl Pts',(-17.3667292953982,17.0449566112366,-3.89497221699488));
#43864=CARTESIAN_POINT('Ctrl Pts',(-17.4411697620701,16.9997228515219,-3.89928837973393));
#43865=CARTESIAN_POINT('Ctrl Pts',(-17.5176598130624,16.9584200236971,-3.90360454247298));
#43866=CARTESIAN_POINT('Ctrl Pts',(-17.5916582086847,16.9184626311467,-3.90778010666456));
#43867=CARTESIAN_POINT('Ctrl Pts',(-17.6675742634443,16.8821841636526,-3.91195567085613));
#43868=CARTESIAN_POINT('Ctrl Pts',(-17.7450035240569,16.8497533016281,-3.9161312350477));
#43869=CARTESIAN_POINT('Ctrl Pts',(-17.8263435525593,16.815684433857,-3.92051769706049));
#43870=CARTESIAN_POINT('Ctrl Pts',(-17.9093531188143,16.7858622689057,-3.92490415907329));
#43871=CARTESIAN_POINT('Ctrl Pts',(-17.9935454192401,16.7604231263167,-3.92929062108608));
#43872=CARTESIAN_POINT('Ctrl Pts',(-18.077737719666,16.7349839837276,-3.93367708309888));
#43873=CARTESIAN_POINT('Ctrl Pts',(-18.1631121727116,16.7139279285856,-3.93806354511167));
#43874=CARTESIAN_POINT('Ctrl Pts',(-18.249172131343,16.6973289917387,-3.94245000712447));
#43875=CARTESIAN_POINT('Ctrl Pts',(-18.3312723437007,16.6814937965827,-3.94663464151747));
#43876=CARTESIAN_POINT('Ctrl Pts',(-18.4143019582716,16.6696556340513,-3.95081927591047));
#43877=CARTESIAN_POINT('Ctrl Pts',(-18.4978371529756,16.6619164176737,-3.95500391030348));
#43878=CARTESIAN_POINT('Ctrl Pts',(-18.5812534456693,16.6541882171128,-3.95918258838737));
#43879=CARTESIAN_POINT('Ctrl Pts',(-18.6651734349296,16.6505474159413,-3.96336126647126));
#43880=CARTESIAN_POINT('Ctrl Pts',(-18.7491632186827,16.651044907269,-3.96753994455515));
#43881=CARTESIAN_POINT('Ctrl Pts',(-18.8346584589486,16.6515513157714,-3.9717935224406));
#43882=CARTESIAN_POINT('Ctrl Pts',(-18.9202255470369,16.6563459251098,-3.97604710032605));
#43883=CARTESIAN_POINT('Ctrl Pts',(-19.0054014154824,16.6654271230872,-3.9803006782115));
#43884=CARTESIAN_POINT('Ctrl Pts',(-19.0889259835097,16.6743322643211,-3.98447179218939));
#43885=CARTESIAN_POINT('Ctrl Pts',(-19.172073887133,16.6873592186152,-3.98864290616729));
#43886=CARTESIAN_POINT('Ctrl Pts',(-19.2544103550733,16.7044539576675,-3.99281402014518));
#43887=CARTESIAN_POINT('Ctrl Pts',(-19.3367191942166,16.7215429604151,-3.9969837344655));
#43888=CARTESIAN_POINT('Ctrl Pts',(-19.4182166883869,16.7426969435999,-4.00115344878583));
#43889=CARTESIAN_POINT('Ctrl Pts',(-19.4984772632645,16.7678105857401,-4.00532316310615));
#43890=CARTESIAN_POINT('Ctrl Pts',(-19.5787349821264,16.7929233342292,-4.00949272905014));
#43891=CARTESIAN_POINT('Ctrl Pts',(-19.657755430421,16.8219953233348,-4.01366229499414));
#43892=CARTESIAN_POINT('Ctrl Pts',(-19.7351285466053,16.8548714735456,-4.01783186093814));
#43893=CARTESIAN_POINT('Ctrl Pts',(-19.8152220061065,16.8889035086417,-4.02214802367712));
#43894=CARTESIAN_POINT('Ctrl Pts',(-19.8935496523617,16.9270119844459,-4.02646418641609));
#43895=CARTESIAN_POINT('Ctrl Pts',(-19.9696814081002,16.9689715751857,-4.03078034915507));
#43896=CARTESIAN_POINT('Ctrl Pts',(-20.0433331799012,17.0095643366693,-4.0349559133467));
#43897=CARTESIAN_POINT('Ctrl Pts',(-20.114929550452,17.0537608783681,-4.03913147753832));
#43898=CARTESIAN_POINT('Ctrl Pts',(-20.1841097633275,17.1013124225843,-4.04330704172995));
#43899=CARTESIAN_POINT('Ctrl Pts',(-20.256784104298,17.1512656822579,-4.0476935037426));
#43900=CARTESIAN_POINT('Ctrl Pts',(-20.3267913293727,17.2049214186624,-4.05207996575526));
#43901=CARTESIAN_POINT('Ctrl Pts',(-20.3937533178436,17.2619440942068,-4.05646642776792));
#43902=CARTESIAN_POINT('Ctrl Pts',(-20.4607153063144,17.3189667697512,-4.06085288978058));
#43903=CARTESIAN_POINT('Ctrl Pts',(-20.524631688673,17.3793559306722,-4.06523935179324));
#43904=CARTESIAN_POINT('Ctrl Pts',(-20.5851713910718,17.4427340469043,-4.0696258138059));
#43905=CARTESIAN_POINT('Ctrl Pts',(-20.6421808499863,17.5024164036099,-4.07375648865202));
#43906=CARTESIAN_POINT('Ctrl Pts',(-20.6964202744402,17.5649836670307,-4.07788716349815));
#43907=CARTESIAN_POINT('Ctrl Pts',(-20.7475781317949,17.6301448177783,-4.08201783834428));
#43908=CARTESIAN_POINT('Ctrl Pts',(-20.7986699217384,17.6952218166719,-4.08614317866296));
#43909=CARTESIAN_POINT('Ctrl Pts',(-20.8466877493677,17.7628856907895,-4.09026851898165));
#43910=CARTESIAN_POINT('Ctrl Pts',(-20.8913569516644,17.8328088002366,-4.09439385930033));
#43911=CARTESIAN_POINT('Ctrl Pts',(-20.9359826817961,17.9026638603613,-4.09851518482883));
#43912=CARTESIAN_POINT('Ctrl Pts',(-20.977265999821,17.9747733973533,-4.10263651035733));
#43913=CARTESIAN_POINT('Ctrl Pts',(-21.0149735460515,18.0487781269426,-4.10675783588582));
#43914=CARTESIAN_POINT('Ctrl Pts',(-21.0526563884393,18.122734372836,-4.1108764613559));
#43915=CARTESIAN_POINT('Ctrl Pts',(-21.0867678956213,18.1985829265156,-4.11499508682597));
#43916=CARTESIAN_POINT('Ctrl Pts',(-21.117119754579,18.2759383788566,-4.11911371229604));
#43917=CARTESIAN_POINT('Ctrl Pts',(-21.1474714047475,18.3532932990728,-4.12323230943427));
#43918=CARTESIAN_POINT('Ctrl Pts',(-21.174063267692,18.4321546644581,-4.1273509065725));
#43919=CARTESIAN_POINT('Ctrl Pts',(-21.1967549321189,18.5121165016086,-4.13146950371073));
#43920=CARTESIAN_POINT('Ctrl Pts',(-21.2194452848828,18.5920737166658,-4.13558786277863));
#43921=CARTESIAN_POINT('Ctrl Pts',(-21.238235765403,18.6731308198826,-4.13970622184654));
#43922=CARTESIAN_POINT('Ctrl Pts',(-21.2530362470694,18.7548680169614,-4.14382458091445));
#43923=CARTESIAN_POINT('Ctrl Pts',(-21.2678499327185,18.8366781344066,-4.14794661410212));
#43924=CARTESIAN_POINT('Ctrl Pts',(-21.2786664327327,18.9191690901919,-4.1520686472898));
#43925=CARTESIAN_POINT('Ctrl Pts',(-21.2854471635996,19.001913005284,-4.15619068047748));
#43926=CARTESIAN_POINT('Ctrl Pts',(-21.2912151852698,19.0722990307271,-4.15969708372782));
#43927=CARTESIAN_POINT('Ctrl Pts',(-21.2940637843831,19.1428678239492,-4.16320348697816));
#43928=CARTESIAN_POINT('Ctrl Pts',(-21.2939989159607,19.2133559031925,-4.16670989022851));
#43929=CARTESIAN_POINT('Origin',(-18.734,19.211,1.76670989022852));
#43930=CARTESIAN_POINT('',(-17.1767158522682,21.2382341403344,-2.85017127940472));
#43931=CARTESIAN_POINT('',(-17.1744642439897,21.2411350264762,-2.91665630319145));
#43932=CARTESIAN_POINT('',(-17.1744642439897,21.2411350264762,1.76670989022852));
#43933=CARTESIAN_POINT('',(-21.2939999971965,19.2108801919503,-3.43329010980363));
#43934=CARTESIAN_POINT('Ctrl Pts',(-17.1744642439897,21.2411350264762,-2.91665630319145));
#43935=CARTESIAN_POINT('Ctrl Pts',(-17.1375641435127,21.2127886232351,-2.91898053472258));
#43936=CARTESIAN_POINT('Ctrl Pts',(-17.101470973183,21.1834618385403,-2.92130476625372));
#43937=CARTESIAN_POINT('Ctrl Pts',(-17.0662376770537,21.1532072068038,-2.92362899778485));
#43938=CARTESIAN_POINT('Ctrl Pts',(-17.002802317601,21.0987356230989,-2.92781363217408));
#43939=CARTESIAN_POINT('Ctrl Pts',(-16.9419203976439,21.0410515629429,-2.9319982665633));
#43940=CARTESIAN_POINT('Ctrl Pts',(-16.883935185605,20.9804236865537,-2.93618290095253));
#43941=CARTESIAN_POINT('Ctrl Pts',(-16.8260325083393,20.9198821064435,-2.94036157903258));
#43942=CARTESIAN_POINT('Ctrl Pts',(-16.7710186644539,20.8564053626863,-2.94454025711262));
#43943=CARTESIAN_POINT('Ctrl Pts',(-16.7192032202845,20.7903017243225,-2.94871893519267));
#43944=CARTESIAN_POINT('Ctrl Pts',(-16.6664590214564,20.7230132256709,-2.95297251307907));
#43945=CARTESIAN_POINT('Ctrl Pts',(-16.6170293785849,20.653003046041,-2.95722609096547));
#43946=CARTESIAN_POINT('Ctrl Pts',(-16.5712008555424,20.5806349370301,-2.96147966885187));
#43947=CARTESIAN_POINT('Ctrl Pts',(-16.5262608079,20.5096698251123,-2.96565078282577));
#43948=CARTESIAN_POINT('Ctrl Pts',(-16.4847837540961,20.4364378006271,-2.96982189679966));
#43949=CARTESIAN_POINT('Ctrl Pts',(-16.4469976092755,20.3613130290579,-2.97399301077356));
#43950=CARTESIAN_POINT('Ctrl Pts',(-16.4092241439612,20.2862134663323,-2.97816272508982));
#43951=CARTESIAN_POINT('Ctrl Pts',(-16.3751393344489,20.2092228285331,-2.98233243940609));
#43952=CARTESIAN_POINT('Ctrl Pts',(-16.3449251982357,20.1307399586702,-2.98650215372236));
#43953=CARTESIAN_POINT('Ctrl Pts',(-16.3147121371714,20.0522598815654,-2.99067171966225));
#43954=CARTESIAN_POINT('Ctrl Pts',(-16.2883696400355,19.9722881075971,-2.99484128560214));
#43955=CARTESIAN_POINT('Ctrl Pts',(-16.2660311035615,19.8912422555325,-2.99901085154203));
#43956=CARTESIAN_POINT('Ctrl Pts',(-16.2429071716539,19.8073469311139,-3.00332701428572));
#43957=CARTESIAN_POINT('Ctrl Pts',(-16.2240741377499,19.7223011025939,-3.00764317702941));
#43958=CARTESIAN_POINT('Ctrl Pts',(-16.2096228114109,19.6365817309648,-3.01195933977309));
#43959=CARTESIAN_POINT('Ctrl Pts',(-16.1956422355369,19.5536546590259,-3.01613490396055));
#43960=CARTESIAN_POINT('Ctrl Pts',(-16.1857622912647,19.4700977247645,-3.02031046814801));
#43961=CARTESIAN_POINT('Ctrl Pts',(-16.1800123293527,19.3863481627554,-3.02448603233547));
#43962=CARTESIAN_POINT('Ctrl Pts',(-16.173971950515,19.29836860919,-3.02887249435727));
#43963=CARTESIAN_POINT('Ctrl Pts',(-16.1724897391971,19.2101770410221,-3.03325895637908));
#43964=CARTESIAN_POINT('Ctrl Pts',(-16.175537874784,19.1222782223174,-3.03764541840088));
#43965=CARTESIAN_POINT('Ctrl Pts',(-16.1785860103709,19.0343794036126,-3.04203188042268));
#43966=CARTESIAN_POINT('Ctrl Pts',(-16.1861643670755,18.9467739058737,-3.04641834244449));
#43967=CARTESIAN_POINT('Ctrl Pts',(-16.1981829862585,18.8599557395154,-3.05080480446629));
#43968=CARTESIAN_POINT('Ctrl Pts',(-16.2096486109408,18.777132205804,-3.05498943886225));
#43969=CARTESIAN_POINT('Ctrl Pts',(-16.2251975483162,18.6947168580516,-3.0591740732582));
#43970=CARTESIAN_POINT('Ctrl Pts',(-16.244789702343,18.6131437513597,-3.06335870765416));
#43971=CARTESIAN_POINT('Ctrl Pts',(-16.2643539693637,18.5316867538876,-3.06753738574105));
#43972=CARTESIAN_POINT('Ctrl Pts',(-16.2879499152422,18.4510700597166,-3.07171606382794));
#43973=CARTESIAN_POINT('Ctrl Pts',(-16.3154858968848,18.3717208253311,-3.07589474191484));
#43974=CARTESIAN_POINT('Ctrl Pts',(-16.343515441184,18.2909493130174,-3.08014831979954));
#43975=CARTESIAN_POINT('Ctrl Pts',(-16.3756275947392,18.2114916234351,-3.08440189768424));
#43976=CARTESIAN_POINT('Ctrl Pts',(-16.4116716116104,18.1337856032898,-3.08865547556895));
#43977=CARTESIAN_POINT('Ctrl Pts',(-16.4470168449122,18.0575860659074,-3.09282658954992));
#43978=CARTESIAN_POINT('Ctrl Pts',(-16.4861426458307,17.9830713215449,-3.0969977035309));
#43979=CARTESIAN_POINT('Ctrl Pts',(-16.528857766551,17.9106355394507,-3.10116881751188));
#43980=CARTESIAN_POINT('Ctrl Pts',(-16.5715585538004,17.8382240638824,-3.1053385318353));
#43981=CARTESIAN_POINT('Ctrl Pts',(-16.6178460353512,17.7678905610413,-3.10950824615873));
#43982=CARTESIAN_POINT('Ctrl Pts',(-16.6674833699683,17.7000039649946,-3.11367796048215));
#43983=CARTESIAN_POINT('Ctrl Pts',(-16.7171189382761,17.632119784644,-3.11784752642926));
#43984=CARTESIAN_POINT('Ctrl Pts',(-16.7701038504313,17.5666827088182,-3.12201709237638));
#43985=CARTESIAN_POINT('Ctrl Pts',(-16.8261591602606,17.504030952178,-3.12618665832349));
#43986=CARTESIAN_POINT('Ctrl Pts',(-16.8841853055411,17.4391764371649,-3.13050282105884));
#43987=CARTESIAN_POINT('Ctrl Pts',(-16.9455014243886,17.3773071422649,-3.13481898379419));
#43988=CARTESIAN_POINT('Ctrl Pts',(-17.009755621585,17.3187575938839,-3.13913514652954));
#43989=CARTESIAN_POINT('Ctrl Pts',(-17.0719167451634,17.2621152907944,-3.14331071072431));
#43990=CARTESIAN_POINT('Ctrl Pts',(-17.1368270773952,17.2085800374251,-3.14748627491907));
#43991=CARTESIAN_POINT('Ctrl Pts',(-17.2041348602048,17.1584131799021,-3.15166183911384));
#43992=CARTESIAN_POINT('Ctrl Pts',(-17.2748421989517,17.1057125137878,-3.15604830111948));
#43993=CARTESIAN_POINT('Ctrl Pts',(-17.3481950580309,17.0567297857013,-3.16043476312513));
#43994=CARTESIAN_POINT('Ctrl Pts',(-17.4237539519783,17.0117148221198,-3.16482122513078));
#43995=CARTESIAN_POINT('Ctrl Pts',(-17.4993128459257,16.9666998585384,-3.16920768713642));
#43996=CARTESIAN_POINT('Ctrl Pts',(-17.5770772261119,16.9256528630385,-3.17359414914207));
#43997=CARTESIAN_POINT('Ctrl Pts',(-17.6565830150582,16.8887655931067,-3.17798061114772));
#43998=CARTESIAN_POINT('Ctrl Pts',(-17.7324306249075,16.8535755610943,-3.18216524554016));
#43999=CARTESIAN_POINT('Ctrl Pts',(-17.8101452346757,16.8220398921685,-3.18634987993261));
#44000=CARTESIAN_POINT('Ctrl Pts',(-17.8893401694872,16.7943598176977,-3.19053451432505));
#44001=CARTESIAN_POINT('Ctrl Pts',(-17.9684223801113,16.7667191423868,-3.19471319240839));
#44002=CARTESIAN_POINT('Ctrl Pts',(-18.0489802999387,16.7429233111999,-3.19889187049172));
#44003=CARTESIAN_POINT('Ctrl Pts',(-18.1306051532975,16.7231264785016,-3.20307054857506));
#44004=CARTESIAN_POINT('Ctrl Pts',(-18.213693073505,16.7029748018013,-3.20732412646065));
#44005=CARTESIAN_POINT('Ctrl Pts',(-18.2978861156729,16.6869671007255,-3.21157770434623));
#44006=CARTESIAN_POINT('Ctrl Pts',(-18.3827345240937,16.6752136199127,-3.21583128223182));
#44007=CARTESIAN_POINT('Ctrl Pts',(-18.4659379805341,16.6636880032625,-3.22000239620916));
#44008=CARTESIAN_POINT('Ctrl Pts',(-18.5497711422168,16.6562531921902,-3.22417351018651));
#44009=CARTESIAN_POINT('Ctrl Pts',(-18.6337990563682,16.6529617338876,-3.22834462416385));
#44010=CARTESIAN_POINT('Ctrl Pts',(-18.7177987741416,16.6496713800656,-3.23251433848362));
#44011=CARTESIAN_POINT('Ctrl Pts',(-18.8019926552976,16.6505216357632,-3.23668405280339));
#44012=CARTESIAN_POINT('Ctrl Pts',(-18.885942287003,16.6555130519957,-3.24085376712315));
#44013=CARTESIAN_POINT('Ctrl Pts',(-18.9698889314202,16.6605042906123,-3.24502333306659));
#44014=CARTESIAN_POINT('Ctrl Pts',(-19.0535908844962,16.669636368619,-3.24919289901003));
#44015=CARTESIAN_POINT('Ctrl Pts',(-19.1366127729526,16.6828578056099,-3.25336246495347));
#44016=CARTESIAN_POINT('Ctrl Pts',(-19.2225536086153,16.6965440920193,-3.25767862769311));
#44017=CARTESIAN_POINT('Ctrl Pts',(-19.3077651468771,16.7146125685867,-3.26199479043275));
#44018=CARTESIAN_POINT('Ctrl Pts',(-19.3917756297612,16.7369484199208,-3.26631095317239));
#44019=CARTESIAN_POINT('Ctrl Pts',(-19.4730494799765,16.7585566832404,-3.27048651736348));
#44020=CARTESIAN_POINT('Ctrl Pts',(-19.5531988875823,16.7841583830433,-3.27466208155456));
#44021=CARTESIAN_POINT('Ctrl Pts',(-19.6318137018712,16.8135992081564,-3.27883764574565));
#44022=CARTESIAN_POINT('Ctrl Pts',(-19.7143991635786,16.8445270193712,-3.28322410775957));
#44023=CARTESIAN_POINT('Ctrl Pts',(-19.7952903977548,16.8796917438777,-3.28761056977348));
#44024=CARTESIAN_POINT('Ctrl Pts',(-19.8740394547192,16.9188590702831,-3.2919970317874));
#44025=CARTESIAN_POINT('Ctrl Pts',(-19.9527885116835,16.9580263966884,-3.29638349380132));
#44026=CARTESIAN_POINT('Ctrl Pts',(-20.0293949232977,17.0011959738741,-3.30076995581524));
#44027=CARTESIAN_POINT('Ctrl Pts',(-20.1034462555219,17.0480813808104,-3.30515641782916));
#44028=CARTESIAN_POINT('Ctrl Pts',(-20.1740903761505,17.092809520654,-3.30934105222176));
#44029=CARTESIAN_POINT('Ctrl Pts',(-20.2426723273843,17.1410855493988,-3.31352568661436));
#44030=CARTESIAN_POINT('Ctrl Pts',(-20.3088136057117,17.19269325739,-3.31771032100697));
#44031=CARTESIAN_POINT('Ctrl Pts',(-20.374860740116,17.2442275081965,-3.32188899909046));
#44032=CARTESIAN_POINT('Ctrl Pts',(-20.4384737424745,17.2990837381083,-3.32606767717394));
#44033=CARTESIAN_POINT('Ctrl Pts',(-20.4993017308437,17.3570016723092,-3.33024635525743));
#44034=CARTESIAN_POINT('Ctrl Pts',(-20.5612200171964,17.4159577438638,-3.33449993314298));
#44035=CARTESIAN_POINT('Ctrl Pts',(-20.6202520574043,17.4780861035065,-3.33875351102853));
#44036=CARTESIAN_POINT('Ctrl Pts',(-20.6760617089389,17.5430682511945,-3.34300708891408));
#44037=CARTESIAN_POINT('Ctrl Pts',(-20.7307893814672,17.6067905931385,-3.34717820289156));
#44038=CARTESIAN_POINT('Ctrl Pts',(-20.7824181813928,17.6732566930095,-3.35134931686903));
#44039=CARTESIAN_POINT('Ctrl Pts',(-20.8306684931563,17.742129267156,-3.35552043084651));
#44040=CARTESIAN_POINT('Ctrl Pts',(-20.8789026140616,17.810978730445,-3.3596901451664));
#44041=CARTESIAN_POINT('Ctrl Pts',(-20.923760234583,17.8822326878121,-3.36385985948629));
#44042=CARTESIAN_POINT('Ctrl Pts',(-20.9650035868519,17.955522801699,-3.36802957380618));
#44043=CARTESIAN_POINT('Ctrl Pts',(-21.0062454715054,18.028810307609,-3.37219913974974));
#44044=CARTESIAN_POINT('Ctrl Pts',(-21.0438731187515,18.1041334246492,-3.37636870569329));
#44045=CARTESIAN_POINT('Ctrl Pts',(-21.0776941561666,18.1810982074244,-3.38053827163685));
#44046=CARTESIAN_POINT('Ctrl Pts',(-21.1127042995431,18.2607689770352,-3.38485443437633));
#44047=CARTESIAN_POINT('Ctrl Pts',(-21.1436349596428,18.3421985193634,-3.3891705971158));
#44048=CARTESIAN_POINT('Ctrl Pts',(-21.1703273243944,18.4249280132143,-3.39348675985528));
#44049=CARTESIAN_POINT('Ctrl Pts',(-21.1961501881654,18.5049626024847,-3.39766232404647));
#44050=CARTESIAN_POINT('Ctrl Pts',(-21.2180065643708,18.5862132848946,-3.40183788823765));
#44051=CARTESIAN_POINT('Ctrl Pts',(-21.2358041974883,18.6682516628954,-3.40601345242883));
#44052=CARTESIAN_POINT('Ctrl Pts',(-21.2545007467516,18.7544336043729,-3.41039991444246));
#44053=CARTESIAN_POINT('Ctrl Pts',(-21.2687176692139,18.8414843294195,-3.41478637645609));
#44054=CARTESIAN_POINT('Ctrl Pts',(-21.2784095170101,18.9289003549305,-3.41917283846971));
#44055=CARTESIAN_POINT('Ctrl Pts',(-21.2881013648063,19.0163163804415,-3.42355930048334));
#44056=CARTESIAN_POINT('Ctrl Pts',(-21.293268179777,19.1040971227328,-3.42794576249697));
#44057=CARTESIAN_POINT('Ctrl Pts',(-21.2939275539577,19.1917407557754,-3.43233222451059));
#44058=CARTESIAN_POINT('Ctrl Pts',(-21.2939755504833,19.1981204260763,-3.43265151959756));
#44059=CARTESIAN_POINT('Ctrl Pts',(-21.2939996986147,19.2045002760229,-3.43297081468453));
#44060=CARTESIAN_POINT('Ctrl Pts',(-21.2939999971965,19.2108801913083,-3.4332901097715));
#44061=CARTESIAN_POINT('Ctrl Pts',(-21.2939999971965,19.2108801919503,-3.43329010980363));
#44062=CARTESIAN_POINT('Ctrl Pts',(-21.294003905102,19.2943824116244,-3.43746913841141));
#44063=CARTESIAN_POINT('Ctrl Pts',(-21.2899179933662,19.3780422026729,-3.44164816701919));
#44064=CARTESIAN_POINT('Ctrl Pts',(-21.2817219740999,19.4614251239161,-3.44582719562696));
#44065=CARTESIAN_POINT('Ctrl Pts',(-21.2735376207105,19.5446893613373,-3.45000027597723));
#44066=CARTESIAN_POINT('Ctrl Pts',(-21.2612548239782,19.6276770564323,-3.45417335632749));
#44067=CARTESIAN_POINT('Ctrl Pts',(-21.2449053023278,19.7099534675119,-3.45834643667776));
#44068=CARTESIAN_POINT('Ctrl Pts',(-21.228391285294,19.7930576758855,-3.46256150311585));
#44069=CARTESIAN_POINT('Ctrl Pts',(-21.2077282378307,19.875435728573,-3.46677656955395));
#44070=CARTESIAN_POINT('Ctrl Pts',(-21.1830026840864,19.9566445891559,-3.47099163599204));
#44071=CARTESIAN_POINT('Ctrl Pts',(-21.1585674190593,20.0369000225192,-3.47515721572332));
#44072=CARTESIAN_POINT('Ctrl Pts',(-21.1301646741428,20.1160131199896,-3.47932279545459));
#44073=CARTESIAN_POINT('Ctrl Pts',(-21.0979289771719,20.1935679573886,-3.48348837518587));
#44074=CARTESIAN_POINT('Ctrl Pts',(-21.0657039544922,20.2710971138504,-3.48765257555778));
#44075=CARTESIAN_POINT('Ctrl Pts',(-21.0296486772609,20.347068609211,-3.49181677592968));
#44076=CARTESIAN_POINT('Ctrl Pts',(-20.9899463178963,20.4210852080619,-3.49598097630159));
#44077=CARTESIAN_POINT('Ctrl Pts',(-20.9502451090693,20.4950996619801,-3.50014505599882));
#44078=CARTESIAN_POINT('Ctrl Pts',(-20.9068972472216,20.5671589258642,-3.50430913569605));
#44079=CARTESIAN_POINT('Ctrl Pts',(-20.8601318431733,20.6368903833901,-3.50847321539329));
#44080=CARTESIAN_POINT('Ctrl Pts',(-20.8123689128483,20.7081092430375,-3.51272611670985));
#44081=CARTESIAN_POINT('Ctrl Pts',(-20.7610412266545,20.7768994173757,-3.51697901802641));
#44082=CARTESIAN_POINT('Ctrl Pts',(-20.7064383509255,20.8428967344162,-3.52123191934297));
#44083=CARTESIAN_POINT('Ctrl Pts',(-20.6528987388227,20.9076089076671,-3.52540200532764));
#44084=CARTESIAN_POINT('Ctrl Pts',(-20.5962107113947,20.969635714652,-3.5295720913123));
#44085=CARTESIAN_POINT('Ctrl Pts',(-20.5366855500212,21.0286701592271,-3.53374217729697));
#44086=CARTESIAN_POINT('Ctrl Pts',(-20.4753871892413,21.0894631852098,-3.53803648627948));
#44087=CARTESIAN_POINT('Ctrl Pts',(-20.411080380652,21.1470823903906,-3.54233079526199));
#44088=CARTESIAN_POINT('Ctrl Pts',(-20.3441412203941,21.2012374859267,-3.54662510424449));
#44089=CARTESIAN_POINT('Ctrl Pts',(-20.2772020601362,21.2553925814628,-3.550919413227));
#44090=CARTESIAN_POINT('Ctrl Pts',(-20.2076310154016,21.306083314333,-3.55521372220951));
#44091=CARTESIAN_POINT('Ctrl Pts',(-20.1358342086543,21.353069291934,-3.55950803119202));
#44092=CARTESIAN_POINT('Ctrl Pts',(-20.0658710578792,21.3988552702266,-3.56369266558496));
#44093=CARTESIAN_POINT('Ctrl Pts',(-19.9935321931099,21.4412951999105,-3.56787729997789));
#44094=CARTESIAN_POINT('Ctrl Pts',(-19.9191711337672,21.4801340603157,-3.57206193437083));
#44095=CARTESIAN_POINT('Ctrl Pts',(-19.8449159181885,21.5189176384104,-3.57624061245465));
#44096=CARTESIAN_POINT('Ctrl Pts',(-19.7686446296092,21.5541101172785,-3.58041929053848));
#44097=CARTESIAN_POINT('Ctrl Pts',(-19.690739462204,21.5854998634368,-3.58459796862231));
#44098=CARTESIAN_POINT('Ctrl Pts',(-19.6114379006597,21.6174522482367,-3.58885154650778));
#44099=CARTESIAN_POINT('Ctrl Pts',(-19.5304437130248,21.645463967428,-3.59310512439324));
#44100=CARTESIAN_POINT('Ctrl Pts',(-19.4481859912097,21.6693609112496,-3.5973587022787));
#44101=CARTESIAN_POINT('Ctrl Pts',(-19.3675229958474,21.6927945661833,-3.60152981625654));
#44102=CARTESIAN_POINT('Ctrl Pts',(-19.2856454833722,21.7122714336375,-3.60570093023438));
#44103=CARTESIAN_POINT('Ctrl Pts',(-19.2029762398825,21.7276766352524,-3.60987204421221));
#44104=CARTESIAN_POINT('Ctrl Pts',(-19.1203347368559,21.7430766675032,-3.61404175853247));
#44105=CARTESIAN_POINT('Ctrl Pts',(-19.0369024823169,21.754407663177,-3.61821147285273));
#44106=CARTESIAN_POINT('Ctrl Pts',(-18.9531132034118,21.7616056935737,-3.62238118717299));
#44107=CARTESIAN_POINT('Ctrl Pts',(-18.8693269060889,21.7688034678336,-3.62655075311692));
#44108=CARTESIAN_POINT('Ctrl Pts',(-18.7851840680773,21.7718685307012,-3.63072031906085));
#44109=CARTESIAN_POINT('Ctrl Pts',(-18.7011229313379,21.7707888776921,-3.63488988500478));
#44110=CARTESIAN_POINT('Ctrl Pts',(-18.6141063087263,21.769671265415,-3.63920604774384));
#44111=CARTESIAN_POINT('Ctrl Pts',(-18.5271777668963,21.7641120647909,-3.6435222104829));
#44112=CARTESIAN_POINT('Ctrl Pts',(-18.4408207068909,21.7541566806023,-3.64783837322195));
#44113=CARTESIAN_POINT('Ctrl Pts',(-18.3572767190368,21.744525592007,-3.65201393741352));
#44114=CARTESIAN_POINT('Ctrl Pts',(-18.2742680097319,21.7307804563761,-3.65618950160509));
#44115=CARTESIAN_POINT('Ctrl Pts',(-18.1922227301014,21.7130146661883,-3.66036506579665));
#44116=CARTESIAN_POINT('Ctrl Pts',(-18.1060335384334,21.6943515681706,-3.66475152780945));
#44117=CARTESIAN_POINT('Ctrl Pts',(-18.0209082233735,21.6712511277376,-3.66913798982225));
#44118=CARTESIAN_POINT('Ctrl Pts',(-17.937323903919,21.6438804323133,-3.67352445183506));
#44119=CARTESIAN_POINT('Ctrl Pts',(-17.8537395844645,21.616509736889,-3.67791091384786));
#44120=CARTESIAN_POINT('Ctrl Pts',(-17.7716967745983,21.584869066222,-3.68229737586066));
#44121=CARTESIAN_POINT('Ctrl Pts',(-17.6916449845522,21.5491822045706,-3.68668383787346));
#44122=CARTESIAN_POINT('Ctrl Pts',(-17.6152736995615,21.5151361016662,-3.69086862550016));
#44123=CARTESIAN_POINT('Ctrl Pts',(-17.5404300949785,21.4772809673625,-3.69505341312687));
#44124=CARTESIAN_POINT('Ctrl Pts',(-17.4675200004595,21.4357760360908,-3.69923820075358));
#44125=CARTESIAN_POINT('Ctrl Pts',(-17.3947226531712,21.39433528751,-3.70341651707862));
#44126=CARTESIAN_POINT('Ctrl Pts',(-17.3238532702767,21.3492561841251,-3.70759483340367));
#44127=CARTESIAN_POINT('Ctrl Pts',(-17.2552965767404,21.3007454835554,-3.71177314972872));
#44128=CARTESIAN_POINT('Ctrl Pts',(-17.227977727748,21.2814146722952,-3.71343814824073));
#44129=CARTESIAN_POINT('Ctrl Pts',(-17.2010258627729,21.2615394792291,-3.71510314675274));
#44130=CARTESIAN_POINT('Ctrl Pts',(-17.1744642439897,21.2411350264762,-3.71676814526475));
#44131=CARTESIAN_POINT('',(-21.2936055426903,19.2106176052578,-3.36670986511441));
#44132=CARTESIAN_POINT('Ctrl Pts',(-21.2939999715072,19.2106180532905,-3.36670989022851));
#44133=CARTESIAN_POINT('Ctrl Pts',(-21.2940130064034,19.2979845189442,-3.37103154303559));
#44134=CARTESIAN_POINT('Ctrl Pts',(-21.2895493128086,19.3852864628676,-3.37535319584268));
#44135=CARTESIAN_POINT('Ctrl Pts',(-21.2806546261691,19.4720559614555,-3.37967484864976));
#44136=CARTESIAN_POINT('Ctrl Pts',(-21.2713805337796,19.5625266412119,-3.38418084296218));
#44137=CARTESIAN_POINT('Ctrl Pts',(-21.2572890869444,19.6524179424097,-3.38868683727459));
#44138=CARTESIAN_POINT('Ctrl Pts',(-21.2384911684206,19.7412112666692,-3.393192831587));
#44139=CARTESIAN_POINT('Ctrl Pts',(-21.2204017935413,19.8266577339088,-3.3975289829656));
#44140=CARTESIAN_POINT('Ctrl Pts',(-21.1979545494935,19.911087135192,-3.40186513434419));
#44141=CARTESIAN_POINT('Ctrl Pts',(-21.1712990035409,19.9940540002698,-3.40620128572279));
#44142=CARTESIAN_POINT('Ctrl Pts',(-21.1446099328528,20.0771252129461,-3.41054289068797));
#44143=CARTESIAN_POINT('Ctrl Pts',(-21.1137021554183,20.1587298407179,-3.41488449565315));
#44144=CARTESIAN_POINT('Ctrl Pts',(-21.0787731611217,20.2384428562617,-3.41922610061834));
#44145=CARTESIAN_POINT('Ctrl Pts',(-21.0437703953367,20.3183242290092,-3.42357687523375));
#44146=CARTESIAN_POINT('Ctrl Pts',(-21.0047296348366,20.3963056454717,-3.42792764984916));
#44147=CARTESIAN_POINT('Ctrl Pts',(-20.9618940508659,20.4719869539834,-3.43227842446457));
#44148=CARTESIAN_POINT('Ctrl Pts',(-20.9570751477604,20.4805009243513,-3.43276787644263));
#44149=CARTESIAN_POINT('Ctrl Pts',(-20.9522082623986,20.4889858169837,-3.43325732842068));
#44150=CARTESIAN_POINT('Ctrl Pts',(-20.9472937739975,20.4974410868688,-3.43374678039873));
#44151=CARTESIAN_POINT('Ctrl Pts',(-20.9052767057113,20.5697305345463,-3.43793141479118));
#44152=CARTESIAN_POINT('Ctrl Pts',(-20.8596361007269,20.6400938357955,-3.44211604918362));
#44153=CARTESIAN_POINT('Ctrl Pts',(-20.8105736599315,20.7081445604478,-3.44630068357607));
#44154=CARTESIAN_POINT('Ctrl Pts',(-20.7615810534479,20.7760984233165,-3.45047936165941));
#44155=CARTESIAN_POINT('Ctrl Pts',(-20.7091765523538,20.8417458779045,-3.45465803974274));
#44156=CARTESIAN_POINT('Ctrl Pts',(-20.6536069384425,20.9047264247462,-3.45883671782608));
#44157=CARTESIAN_POINT('Ctrl Pts',(-20.5970412791288,20.9688358526382,-3.46309029571167));
#44158=CARTESIAN_POINT('Ctrl Pts',(-20.5371961639062,21.0301814068962,-3.46734387359725));
#44159=CARTESIAN_POINT('Ctrl Pts',(-20.4743771168498,21.0884151089052,-3.47159745148284));
#44160=CARTESIAN_POINT('Ctrl Pts',(-20.412775939613,21.1455198369568,-3.47576856546018));
#44161=CARTESIAN_POINT('Ctrl Pts',(-20.3483154653815,21.1996319675306,-3.47993967943753));
#44162=CARTESIAN_POINT('Ctrl Pts',(-20.2813221318913,21.250459296029,-3.48411079341487));
#44163=CARTESIAN_POINT('Ctrl Pts',(-20.2143512786613,21.3012695689265,-3.48828050773464));
#44164=CARTESIAN_POINT('Ctrl Pts',(-20.1448496203246,21.3487969510057,-3.4924502220544));
#44165=CARTESIAN_POINT('Ctrl Pts',(-20.0731762130974,21.3927898776633,-3.49661993637416));
#44166=CARTESIAN_POINT('Ctrl Pts',(-20.0015053563176,21.4367812388638,-3.50078950231759));
#44167=CARTESIAN_POINT('Ctrl Pts',(-19.9276632968144,21.4772381547836,-3.50495906826103));
#44168=CARTESIAN_POINT('Ctrl Pts',(-19.8520364016656,21.5139534525367,-3.50912863420446));
#44169=CARTESIAN_POINT('Ctrl Pts',(-19.7737505581546,21.5519596148775,-3.5134447969441));
#44170=CARTESIAN_POINT('Ctrl Pts',(-19.6935525085944,21.585955922694,-3.51776095968374));
#44171=CARTESIAN_POINT('Ctrl Pts',(-19.6118947218442,21.6157662791544,-3.52207712242338));
#44172=CARTESIAN_POINT('Ctrl Pts',(-19.5328969289329,21.6446055663797,-3.52625268661447));
#44173=CARTESIAN_POINT('Ctrl Pts',(-19.4525335041393,21.6695273345314,-3.53042825080555));
#44174=CARTESIAN_POINT('Ctrl Pts',(-19.3712290384541,21.690423149152,-3.53460381499664));
#44175=CARTESIAN_POINT('Ctrl Pts',(-19.2858180774511,21.712374361704,-3.53899027701056));
#44176=CARTESIAN_POINT('Ctrl Pts',(-19.1993690855429,21.7298821146793,-3.54337673902448));
#44177=CARTESIAN_POINT('Ctrl Pts',(-19.1123834602667,21.7428819002861,-3.5477632010384));
#44178=CARTESIAN_POINT('Ctrl Pts',(-19.0253978349904,21.755881685893,-3.55214966305232));
#44179=CARTESIAN_POINT('Ctrl Pts',(-18.9378761611969,21.7643735238079,-3.55653612506624));
#44180=CARTESIAN_POINT('Ctrl Pts',(-18.8503205710795,21.7683559636358,-3.56092258708016));
#44181=CARTESIAN_POINT('Ctrl Pts',(-18.7668123251272,21.7721543112249,-3.56510628052826));
#44182=CARTESIAN_POINT('Ctrl Pts',(-18.6829624657632,21.7718650921498,-3.56928997397637));
#44183=CARTESIAN_POINT('Ctrl Pts',(-18.599204802892,21.7674487585001,-3.57347366742447));
#44184=CARTESIAN_POINT('Ctrl Pts',(-18.5155577245013,21.7630382556955,-3.57765183718017));
#44185=CARTESIAN_POINT('Ctrl Pts',(-18.4320030559613,21.7545114802022,-3.58183000693587));
#44186=CARTESIAN_POINT('Ctrl Pts',(-18.3489773389754,21.7418807855167,-3.58600817669157));
#44187=CARTESIAN_POINT('Ctrl Pts',(-18.2660363238681,21.7292629765201,-3.59018208392669));
#44188=CARTESIAN_POINT('Ctrl Pts',(-18.183623640842,21.7125496319968,-3.59435599116181));
#44189=CARTESIAN_POINT('Ctrl Pts',(-18.1021720695873,21.6918050036934,-3.59852989839693));
#44190=CARTESIAN_POINT('Ctrl Pts',(-18.0183963786608,21.6704684531229,-3.60282290290376));
#44191=CARTESIAN_POINT('Ctrl Pts',(-17.9356379804305,21.6448670989516,-3.60711590741059));
#44192=CARTESIAN_POINT('Ctrl Pts',(-17.8543574465608,21.6151274879213,-3.61140891191742));
#44193=CARTESIAN_POINT('Ctrl Pts',(-17.775411049397,21.5862419106236,-3.61557863402291));
#44194=CARTESIAN_POINT('Ctrl Pts',(-17.6978592336747,21.5534527314071,-3.61974835612839));
#44195=CARTESIAN_POINT('Ctrl Pts',(-17.6221076884281,21.5169261669592,-3.62391807823388));
#44196=CARTESIAN_POINT('Ctrl Pts',(-17.5429966270672,21.4787796806806,-3.62827272394138));
#44197=CARTESIAN_POINT('Ctrl Pts',(-17.4658497272794,21.4365568045564,-3.63262736964889));
#44198=CARTESIAN_POINT('Ctrl Pts',(-17.3911027171311,21.3905015227485,-3.63698201535639));
#44199=CARTESIAN_POINT('Ctrl Pts',(-17.3163557069827,21.3444462409407,-3.64133666106389));
#44200=CARTESIAN_POINT('Ctrl Pts',(-17.244009058728,21.2945588745528,-3.64569130677139));
#44201=CARTESIAN_POINT('Ctrl Pts',(-17.1744642439897,21.2411350264762,-3.6500459524789));
#44202=CARTESIAN_POINT('Ctrl Pts',(-17.1767158522682,21.2382341403344,-2.85017127940472));
#44203=CARTESIAN_POINT('Ctrl Pts',(-16.7788810867994,20.9296544485643,-2.87512870416081));
#44204=CARTESIAN_POINT('Ctrl Pts',(-15.9356497699281,19.7924127402861,-2.94247806447738));
#44205=CARTESIAN_POINT('Ctrl Pts',(-16.3642904626609,17.3274479445074,-3.05221936035442));
#44206=CARTESIAN_POINT('Ctrl Pts',(-19.0350903727826,16.1989182890321,-3.17939516703585));
#44207=CARTESIAN_POINT('Ctrl Pts',(-21.0089154299348,17.5465283377359,-3.28422525530949));
#44208=CARTESIAN_POINT('Ctrl Pts',(-21.290373212379,18.8060182046973,-3.34666340802265));
#44209=CARTESIAN_POINT('Ctrl Pts',(-21.2898371856445,19.2106133247715,-3.36670962517532));
#44210=CARTESIAN_POINT('Origin',(-18.734,19.211,1.76670989022852));
#44211=CARTESIAN_POINT('',(-17.1744642439897,21.2411350264762,-2.05017636798559));
#44212=CARTESIAN_POINT('',(-17.1744642439897,21.2411350264762,-2.11663750951706));
#44213=CARTESIAN_POINT('',(-17.1744642439897,21.2411350264762,1.76670989022852));
#44214=CARTESIAN_POINT('',(-21.2939989850552,19.2132795868247,-2.63329010980608));
#44215=CARTESIAN_POINT('Ctrl Pts',(-17.1744642439897,21.2411350264762,-2.11663750951706));
#44216=CARTESIAN_POINT('Ctrl Pts',(-17.1077529033479,21.1898878337006,-2.1208121744548));
#44217=CARTESIAN_POINT('Ctrl Pts',(-17.0436084091249,21.135378288778,-2.12498683939254));
#44218=CARTESIAN_POINT('Ctrl Pts',(-16.9823526577971,21.0779042794298,-2.12916150433028));
#44219=CARTESIAN_POINT('Ctrl Pts',(-16.9210595534414,21.0203952231151,-2.13333871492899));
#44220=CARTESIAN_POINT('Ctrl Pts',(-16.8626590177325,20.9599184348882,-2.13751592552771));
#44221=CARTESIAN_POINT('Ctrl Pts',(-16.8074346248094,20.8968071820694,-2.14169313612642));
#44222=CARTESIAN_POINT('Ctrl Pts',(-16.7521184910976,20.8335910865205,-2.14587728606073));
#44223=CARTESIAN_POINT('Ctrl Pts',(-16.6999893181143,20.7677321503202,-2.15006143599504));
#44224=CARTESIAN_POINT('Ctrl Pts',(-16.6512888568846,20.6995947381148,-2.15424558592935));
#44225=CARTESIAN_POINT('Ctrl Pts',(-16.6267355331262,20.6652418819056,-2.15635510985165));
#44226=CARTESIAN_POINT('Ctrl Pts',(-16.6030530382591,20.6303102941139,-2.15846463377395));
#44227=CARTESIAN_POINT('Ctrl Pts',(-16.5802679097319,20.5948490103148,-2.16057415769624));
#44228=CARTESIAN_POINT('Ctrl Pts',(-16.5350693576789,20.5245049400697,-2.16475879184019));
#44229=CARTESIAN_POINT('Ctrl Pts',(-16.4932366287838,20.4518132565164,-2.16894342598413));
#44230=CARTESIAN_POINT('Ctrl Pts',(-16.455021774691,20.3771296019601,-2.17312806012807));
#44231=CARTESIAN_POINT('Ctrl Pts',(-16.4168613147564,20.3025522504267,-2.17730673795852));
#44232=CARTESIAN_POINT('Ctrl Pts',(-16.3823087086575,20.2259889657712,-2.18148541578897));
#44233=CARTESIAN_POINT('Ctrl Pts',(-16.3515723822767,20.1478237007618,-2.18566409361941));
#44234=CARTESIAN_POINT('Ctrl Pts',(-16.3202851269751,20.0682573735515,-2.18991767156768));
#44235=CARTESIAN_POINT('Ctrl Pts',(-16.2929525719374,19.9870314754769,-2.19417124951594));
#44236=CARTESIAN_POINT('Ctrl Pts',(-16.2697452279947,19.9045765413053,-2.1984248274642));
#44237=CARTESIAN_POINT('Ctrl Pts',(-16.2469878054675,19.823720163211,-2.20259594117975));
#44238=CARTESIAN_POINT('Ctrl Pts',(-16.2281972006316,19.7416824416901,-2.2067670548953));
#44239=CARTESIAN_POINT('Ctrl Pts',(-16.2134847477526,19.6588871098706,-2.21093816861086));
#44240=CARTESIAN_POINT('Ctrl Pts',(-16.1987772317893,19.5761195608808,-2.21510788266607));
#44241=CARTESIAN_POINT('Ctrl Pts',(-16.1881452304062,19.4925953590458,-2.21927759672128));
#44242=CARTESIAN_POINT('Ctrl Pts',(-16.1816490383842,19.4087487515486,-2.22344731077649));
#44243=CARTESIAN_POINT('Ctrl Pts',(-16.1751530775284,19.3249051277225,-2.22761687645295));
#44244=CARTESIAN_POINT('Ctrl Pts',(-16.1727926681034,19.2407395797693,-2.23178644212941));
#44245=CARTESIAN_POINT('Ctrl Pts',(-16.1745761446913,19.1566904347581,-2.23595600780587));
#44246=CARTESIAN_POINT('Ctrl Pts',(-16.1764223263664,19.0696862136873,-2.24027217085352));
#44247=CARTESIAN_POINT('Ctrl Pts',(-16.1827092038737,18.982807260651,-2.24458833390117));
#44248=CARTESIAN_POINT('Ctrl Pts',(-16.1933873263915,18.8965365797108,-2.24890449694883));
#44249=CARTESIAN_POINT('Ctrl Pts',(-16.2037176087823,18.8130761685129,-2.25308006086959));
#44250=CARTESIAN_POINT('Ctrl Pts',(-16.2181573115164,18.7301854648525,-2.25725562479036));
#44251=CARTESIAN_POINT('Ctrl Pts',(-16.236609460393,18.6482918228058,-2.26143118871113));
#44252=CARTESIAN_POINT('Ctrl Pts',(-16.2559935873462,18.5622619102622,-2.26581765132222));
#44253=CARTESIAN_POINT('Ctrl Pts',(-16.2798059943657,18.4773329921965,-2.27020411393331));
#44254=CARTESIAN_POINT('Ctrl Pts',(-16.3078756047626,18.3939807720539,-2.2745905765444));
#44255=CARTESIAN_POINT('Ctrl Pts',(-16.3359452151594,18.3106285519112,-2.2789770391555));
#44256=CARTESIAN_POINT('Ctrl Pts',(-16.3682717448907,18.2288535413147,-2.28336350176659));
#44257=CARTESIAN_POINT('Ctrl Pts',(-16.4046276535509,18.1491033611513,-2.28774996437768));
#44258=CARTESIAN_POINT('Ctrl Pts',(-16.4393107693519,18.0730226129128,-2.29193459890625));
#44259=CARTESIAN_POINT('Ctrl Pts',(-16.4777897133166,17.9985012713564,-2.29611923343482));
#44260=CARTESIAN_POINT('Ctrl Pts',(-16.5199018772185,17.9259437745003,-2.3003038679634));
#44261=CARTESIAN_POINT('Ctrl Pts',(-16.5619540996867,17.8534895542273,-2.30448254618457));
#44262=CARTESIAN_POINT('Ctrl Pts',(-16.6076290410406,17.7829940208021,-2.30866122440573));
#44263=CARTESIAN_POINT('Ctrl Pts',(-16.6567166746412,17.7148402537876,-2.3128399026269));
#44264=CARTESIAN_POINT('Ctrl Pts',(-16.7066841667541,17.6454648823148,-2.31709348047825));
#44265=CARTESIAN_POINT('Ctrl Pts',(-16.7601876992284,17.5785164938348,-2.32134705832959));
#44266=CARTESIAN_POINT('Ctrl Pts',(-16.8169575547354,17.5143715011666,-2.32560063618093));
#44267=CARTESIAN_POINT('Ctrl Pts',(-16.872626818136,17.4514700817286,-2.32977175029927));
#44268=CARTESIAN_POINT('Ctrl Pts',(-16.9314365679997,17.3912646900964,-2.33394286441762));
#44269=CARTESIAN_POINT('Ctrl Pts',(-16.9930907748647,17.3340782994918,-2.33811397853596));
#44270=CARTESIAN_POINT('Ctrl Pts',(-17.0547242930789,17.27691109832,-2.34228369299761));
#44271=CARTESIAN_POINT('Ctrl Pts',(-17.1192000356704,17.2227611988155,-2.34645340745925));
#44272=CARTESIAN_POINT('Ctrl Pts',(-17.1861855058205,17.1719143491242,-2.3506231219209));
#44273=CARTESIAN_POINT('Ctrl Pts',(-17.2531685923512,17.1210693087735,-2.35479268800691));
#44274=CARTESIAN_POINT('Ctrl Pts',(-17.3226608619368,17.0735273620081,-2.35896225409291));
#44275=CARTESIAN_POINT('Ctrl Pts',(-17.394298262154,17.0295327750314,-2.36313182017892));
#44276=CARTESIAN_POINT('Ctrl Pts',(-17.468454339619,16.9839913959473,-2.36744798275227));
#44277=CARTESIAN_POINT('Ctrl Pts',(-17.5449087501569,16.9422517437132,-2.37176414532562));
#44278=CARTESIAN_POINT('Ctrl Pts',(-17.6232285971903,16.9045336788281,-2.37608030789897));
#44279=CARTESIAN_POINT('Ctrl Pts',(-17.698997188932,16.8680442732967,-2.3802558722329));
#44280=CARTESIAN_POINT('Ctrl Pts',(-17.7765110982796,16.8353186125376,-2.38443143656682));
#44281=CARTESIAN_POINT('Ctrl Pts',(-17.855358497723,16.8065064752684,-2.38860700090075));
#44282=CARTESIAN_POINT('Ctrl Pts',(-17.938188283016,16.7762391086755,-2.39299346259381));
#44283=CARTESIAN_POINT('Ctrl Pts',(-18.022489249436,16.7502911703925,-2.39737992428687));
#44284=CARTESIAN_POINT('Ctrl Pts',(-18.1077688054804,16.7287763011746,-2.40176638597993));
#44285=CARTESIAN_POINT('Ctrl Pts',(-18.1930483615248,16.7072614319567,-2.40615284767299));
#44286=CARTESIAN_POINT('Ctrl Pts',(-18.2793059232537,16.6901796699007,-2.41053930936606));
#44287=CARTESIAN_POINT('Ctrl Pts',(-18.3660419494175,16.6775819782335,-2.41492577105912));
#44288=CARTESIAN_POINT('Ctrl Pts',(-18.4487871282915,16.6655639241848,-2.41911040544311));
#44289=CARTESIAN_POINT('Ctrl Pts',(-18.5322757027657,16.6575816378619,-2.42329503982711));
#44290=CARTESIAN_POINT('Ctrl Pts',(-18.6160795877536,16.6537173061283,-2.42747967421111));
#44291=CARTESIAN_POINT('Ctrl Pts',(-18.6997641882881,16.6498584747925,-2.43165835228622));
#44292=CARTESIAN_POINT('Ctrl Pts',(-18.7837627522533,16.6501059764733,-2.43583703036133));
#44293=CARTESIAN_POINT('Ctrl Pts',(-18.8676394869527,16.654490565727,-2.44001570843645));
#44294=CARTESIAN_POINT('Ctrl Pts',(-18.9530196520657,16.6589537456037,-2.44426928632412));
#44295=CARTESIAN_POINT('Ctrl Pts',(-19.0382731002408,16.6677038557804,-2.44852286421179));
#44296=CARTESIAN_POINT('Ctrl Pts',(-19.1229373349573,16.6807178518046,-2.45277644209946));
#44297=CARTESIAN_POINT('Ctrl Pts',(-19.2059601880682,16.6934795460894,-2.4569475560692));
#44298=CARTESIAN_POINT('Ctrl Pts',(-19.2884159943213,16.7103412009492,-2.46111867003895));
#44299=CARTESIAN_POINT('Ctrl Pts',(-19.369872949239,16.7312287217515,-2.46528978400869));
#44300=CARTESIAN_POINT('Ctrl Pts',(-19.4513025704935,16.7521092335458,-2.4694594983211));
#44301=CARTESIAN_POINT('Ctrl Pts',(-19.5317335608288,16.7770128141666,-2.47362921263351));
#44302=CARTESIAN_POINT('Ctrl Pts',(-19.6107456770747,16.8058145564779,-2.47779892694592));
#44303=CARTESIAN_POINT('Ctrl Pts',(-19.6897549817355,16.8346152739014,-2.48196849288227));
#44304=CARTESIAN_POINT('Ctrl Pts',(-19.7673450807723,16.867313718866,-2.48613805881862));
#44305=CARTESIAN_POINT('Ctrl Pts',(-19.8431135303122,16.9037359975767,-2.49030762475498));
#44306=CARTESIAN_POINT('Ctrl Pts',(-19.9215459053917,16.941438838831,-2.49462378750377));
#44307=CARTESIAN_POINT('Ctrl Pts',(-19.9980256738195,16.9831320175018,-2.49893995025257));
#44308=CARTESIAN_POINT('Ctrl Pts',(-20.0721336489296,17.0285705423537,-2.50325611300137));
#44309=CARTESIAN_POINT('Ctrl Pts',(-20.1438275642617,17.072528911864,-2.50743167718609));
#44310=CARTESIAN_POINT('Ctrl Pts',(-20.2133014733529,17.1199920607239,-2.51160724137082));
#44311=CARTESIAN_POINT('Ctrl Pts',(-20.2802065216066,17.1706947795633,-2.51578280555554));
#44312=CARTESIAN_POINT('Ctrl Pts',(-20.3504907852062,17.2239583725079,-2.52016926758637));
#44313=CARTESIAN_POINT('Ctrl Pts',(-20.4179394151737,17.2807970211654,-2.52455572961721));
#44314=CARTESIAN_POINT('Ctrl Pts',(-20.4821902270868,17.3408580455169,-2.52894219164805));
#44315=CARTESIAN_POINT('Ctrl Pts',(-20.546441039,17.4009190698683,-2.53332865367888));
#44316=CARTESIAN_POINT('Ctrl Pts',(-20.6074936847495,17.4642019995334,-2.53771511570972));
#44317=CARTESIAN_POINT('Ctrl Pts',(-20.665034920053,17.5303143846823,-2.54210157774055));
#44318=CARTESIAN_POINT('Ctrl Pts',(-20.7194682477108,17.5928559186633,-2.54625111891261));
#44319=CARTESIAN_POINT('Ctrl Pts',(-20.7709705307844,17.6581717364551,-2.55040066008466));
#44320=CARTESIAN_POINT('Ctrl Pts',(-20.8192426277969,17.7259534743927,-2.55455020125671));
#44321=CARTESIAN_POINT('Ctrl Pts',(-20.8674506257227,17.7936452069694,-2.55869423237604));
#44322=CARTESIAN_POINT('Ctrl Pts',(-20.912436679677,17.8637959851797,-2.56283826349536));
#44323=CARTESIAN_POINT('Ctrl Pts',(-20.953940279832,17.936062686255,-2.56698229461468));
#44324=CARTESIAN_POINT('Ctrl Pts',(-20.9954017278126,18.0082559913218,-2.57112211694435));
#44325=CARTESIAN_POINT('Ctrl Pts',(-21.0333875106824,18.0825605501461,-2.57526193927403));
#44326=CARTESIAN_POINT('Ctrl Pts',(-21.0676798966809,18.1586036203847,-2.5794017616037));
#44327=CARTESIAN_POINT('Ctrl Pts',(-21.1019481578681,18.2345931940623,-2.58353867155416));
#44328=CARTESIAN_POINT('Ctrl Pts',(-21.1325279904635,18.3123184247114,-2.58767558150461));
#44329=CARTESIAN_POINT('Ctrl Pts',(-21.1592478841653,18.3913825890383,-2.59181249145506));
#44330=CARTESIAN_POINT('Ctrl Pts',(-21.185962767493,18.4704319276684,-2.59594862567389));
#44331=CARTESIAN_POINT('Ctrl Pts',(-21.2088189905586,18.5508192612332,-2.60008475989273));
#44332=CARTESIAN_POINT('Ctrl Pts',(-21.2276938748212,18.6321296702378,-2.60422089411156));
#44333=CARTESIAN_POINT('Ctrl Pts',(-21.2465668271893,18.7134317569063,-2.60835660498608));
#44334=CARTESIAN_POINT('Ctrl Pts',(-21.261459151574,18.7956562735645,-2.61249231586059));
#44335=CARTESIAN_POINT('Ctrl Pts',(-21.272298987946,18.8783767179039,-2.61662802673511));
#44336=CARTESIAN_POINT('Ctrl Pts',(-21.2831447249188,18.9611421906275,-2.62076598885936));
#44337=CARTESIAN_POINT('Ctrl Pts',(-21.2899335186437,19.0444036643965,-2.62490395098361));
#44338=CARTESIAN_POINT('Ctrl Pts',(-21.2926453380231,19.1277291514849,-2.62904191310786));
#44339=CARTESIAN_POINT('Ctrl Pts',(-21.2935733586038,19.1562442389939,-2.63045797866241));
#44340=CARTESIAN_POINT('Ctrl Pts',(-21.2940243746441,19.1847668138181,-2.63187404421695));
#44341=CARTESIAN_POINT('Ctrl Pts',(-21.2939989850559,19.2132795861284,-2.6332901097715));
#44342=CARTESIAN_POINT('Ctrl Pts',(-21.2939989850552,19.2132795868247,-2.63329010980608));
#44343=CARTESIAN_POINT('Ctrl Pts',(-21.293907125607,19.3164386732131,-2.63841342883254));
#44344=CARTESIAN_POINT('Ctrl Pts',(-21.2875761055109,19.4193213099601,-2.643536747859));
#44345=CARTESIAN_POINT('Ctrl Pts',(-21.2751280763078,19.5212710102476,-2.64866006688546));
#44346=CARTESIAN_POINT('Ctrl Pts',(-21.2624749613816,19.6249003682273,-2.6538677944211));
#44347=CARTESIAN_POINT('Ctrl Pts',(-21.2435016684883,19.7275658815507,-2.65907552195674));
#44348=CARTESIAN_POINT('Ctrl Pts',(-21.2183850428165,19.8286009707164,-2.66428324949238));
#44349=CARTESIAN_POINT('Ctrl Pts',(-21.2103562166331,19.8608980308362,-2.66594796113558));
#44350=CARTESIAN_POINT('Ctrl Pts',(-21.2017000059957,19.8930286552932,-2.66761267277878));
#44351=CARTESIAN_POINT('Ctrl Pts',(-21.1924232051054,19.9249715292638,-2.66927738442198));
#44352=CARTESIAN_POINT('Ctrl Pts',(-21.1691038390111,20.0052672670978,-2.67346201883512));
#44353=CARTESIAN_POINT('Ctrl Pts',(-21.1418030734501,20.0845687630516,-2.67764665324825));
#44354=CARTESIAN_POINT('Ctrl Pts',(-21.1106233366689,20.1624523191421,-2.68183128766138));
#44355=CARTESIAN_POINT('Ctrl Pts',(-21.0794879803815,20.240225017636,-2.68600996576567));
#44356=CARTESIAN_POINT('Ctrl Pts',(-21.0444847892983,20.3165833617425,-2.69018864386997));
#44357=CARTESIAN_POINT('Ctrl Pts',(-21.0057661997906,20.3911179320259,-2.69436732197426));
#44358=CARTESIAN_POINT('Ctrl Pts',(-20.9663536076312,20.4669884804549,-2.69862089985464));
#44359=CARTESIAN_POINT('Ctrl Pts',(-20.923091244407,20.5409687666864,-2.70287447773502));
#44360=CARTESIAN_POINT('Ctrl Pts',(-20.8761915739271,20.6126473381688,-2.7071280556154));
#44361=CARTESIAN_POINT('Ctrl Pts',(-20.8302011447919,20.6829362811089,-2.71129916961421));
#44362=CARTESIAN_POINT('Ctrl Pts',(-20.7807134458812,20.7510115566354,-2.71547028361303));
#44363=CARTESIAN_POINT('Ctrl Pts',(-20.7279747027012,20.8165107863193,-2.71964139761184));
#44364=CARTESIAN_POINT('Ctrl Pts',(-20.675253656514,20.8819880371064,-2.72381111195321));
#44365=CARTESIAN_POINT('Ctrl Pts',(-20.6192840209111,20.944890600777,-2.72798082629459));
#44366=CARTESIAN_POINT('Ctrl Pts',(-20.560353487436,21.0048876606215,-2.73215054063596));
#44367=CARTESIAN_POINT('Ctrl Pts',(-20.5014250509605,21.064882585515,-2.73632010660112));
#44368=CARTESIAN_POINT('Ctrl Pts',(-20.4395362490684,21.1219718845495,-2.74048967256628));
#44369=CARTESIAN_POINT('Ctrl Pts',(-20.3750119946268,21.1758612249955,-2.74465923853145));
#44370=CARTESIAN_POINT('Ctrl Pts',(-20.3082191477172,21.2316452475716,-2.74897540124578));
#44371=CARTESIAN_POINT('Ctrl Pts',(-20.2386024799585,21.2839997657249,-2.75329156396011));
#44372=CARTESIAN_POINT('Ctrl Pts',(-20.1665585536104,21.3326446428367,-2.75760772667444));
#44373=CARTESIAN_POINT('Ctrl Pts',(-20.0968614498344,21.3797049187001,-2.76178329088732));
#44374=CARTESIAN_POINT('Ctrl Pts',(-20.0248932222208,21.4232933214429,-2.76595885510019));
#44375=CARTESIAN_POINT('Ctrl Pts',(-19.9510397173094,21.463202106049,-2.77013441931307));
#44376=CARTESIAN_POINT('Ctrl Pts',(-19.8734560486687,21.5051265878247,-2.77452088127813));
#44377=CARTESIAN_POINT('Ctrl Pts',(-19.7937921742969,21.5429897170771,-2.77890734324319));
#44378=CARTESIAN_POINT('Ctrl Pts',(-19.7125190809761,21.5766078305936,-2.78329380520824));
#44379=CARTESIAN_POINT('Ctrl Pts',(-19.6312459876554,21.61022594411,-2.7876802671733));
#44380=CARTESIAN_POINT('Ctrl Pts',(-19.5483642476832,21.6395989197709,-2.79206672913836));
#44381=CARTESIAN_POINT('Ctrl Pts',(-19.4643607861727,21.6646041086575,-2.79645319110342));
#44382=CARTESIAN_POINT('Ctrl Pts',(-19.3842194543331,21.6884596629912,-2.80063798179683));
#44383=CARTESIAN_POINT('Ctrl Pts',(-19.3027589678929,21.7084290356266,-2.80482277249024));
#44384=CARTESIAN_POINT('Ctrl Pts',(-19.2203910787649,21.7243689976798,-2.80900756318365));
#44385=CARTESIAN_POINT('Ctrl Pts',(-19.1381412613302,21.7402861103151,-2.81318635511555));
#44386=CARTESIAN_POINT('Ctrl Pts',(-19.0549870728557,21.7521851992274,-2.81736514704745));
#44387=CARTESIAN_POINT('Ctrl Pts',(-18.9713553167734,21.7599728232367,-2.82154393897936));
#44388=CARTESIAN_POINT('Ctrl Pts',(-18.8878237952947,21.7677511135976,-2.825717722532));
#44389=CARTESIAN_POINT('Ctrl Pts',(-18.8038162997617,21.771427693135,-2.82989150608464));
#44390=CARTESIAN_POINT('Ctrl Pts',(-18.7197682827693,21.7709604407538,-2.83406528963728));
#44391=CARTESIAN_POINT('Ctrl Pts',(-18.6357753750469,21.7704934947444,-2.83823633649044));
#44392=CARTESIAN_POINT('Ctrl Pts',(-18.5517424572939,21.7658881143933,-2.8424073833436));
#44393=CARTESIAN_POINT('Ctrl Pts',(-18.468107491185,21.7571541928477,-2.84657843019677));
#44394=CARTESIAN_POINT('Ctrl Pts',(-18.3845022745134,21.7484233780081,-2.85074799338464));
#44395=CARTESIAN_POINT('Ctrl Pts',(-18.3012951853464,21.7355669871492,-2.85491755657251));
#44396=CARTESIAN_POINT('Ctrl Pts',(-18.2189201971796,21.7186468644381,-2.85908711976038));
#44397=CARTESIAN_POINT('Ctrl Pts',(-18.1365498000665,21.7017276847462,-2.86325645056353));
#44398=CARTESIAN_POINT('Ctrl Pts',(-18.0550118619344,21.6807453176235,-2.86742578136668));
#44399=CARTESIAN_POINT('Ctrl Pts',(-17.9747299315205,21.655812664216,-2.87159511216983));
#44400=CARTESIAN_POINT('Ctrl Pts',(-17.8943836665539,21.6308600308318,-2.87576778409883));
#44401=CARTESIAN_POINT('Ctrl Pts',(-17.8152958594601,21.601950925752,-2.87994045602783));
#44402=CARTESIAN_POINT('Ctrl Pts',(-17.7378740400864,21.5692478817941,-2.88411312795683));
#44403=CARTESIAN_POINT('Ctrl Pts',(-17.6604189341951,21.5365307775821,-2.88828759387257));
#44404=CARTESIAN_POINT('Ctrl Pts',(-17.5846316581436,21.5000166836798,-2.89246205978831));
#44405=CARTESIAN_POINT('Ctrl Pts',(-17.510896867848,21.4599150113154,-2.89663652570405));
#44406=CARTESIAN_POINT('Ctrl Pts',(-17.4370550941973,21.4197551545928,-2.90081704844001));
#44407=CARTESIAN_POINT('Ctrl Pts',(-17.3652721469497,21.3759975630386,-2.90499757117598));
#44408=CARTESIAN_POINT('Ctrl Pts',(-17.2959049512236,21.3288958026033,-2.90917809391194));
#44409=CARTESIAN_POINT('Ctrl Pts',(-17.2545431057053,21.3008102541193,-2.91167083033844));
#44410=CARTESIAN_POINT('Ctrl Pts',(-17.2140395717351,21.2715365208939,-2.91416356676495));
#44411=CARTESIAN_POINT('Ctrl Pts',(-17.1744642439897,21.2411350264762,-2.91665630319145));
#44412=CARTESIAN_POINT('',(-21.2939990581246,19.2088040034447,-2.5667098902285));
#44413=CARTESIAN_POINT('Ctrl Pts',(-21.2953148853665,19.2088155456687,-2.56671052144854));
#44414=CARTESIAN_POINT('Ctrl Pts',(-21.2889869060013,19.9045867976347,-2.6013709944024));
#44415=CARTESIAN_POINT('Ctrl Pts',(-20.6359184624636,21.4617758669056,-2.67842340291674));
#44416=CARTESIAN_POINT('Ctrl Pts',(-18.5512406975192,22.0045420360256,-2.77291032223546));
#44417=CARTESIAN_POINT('Ctrl Pts',(-17.454631325708,21.4537986876689,-2.83273676860033));
#44418=CARTESIAN_POINT('Ctrl Pts',(-17.1767158522682,21.2382341403344,-2.85017127940472));
#44419=CARTESIAN_POINT('Ctrl Pts',(-17.1744642439897,21.2411350264762,-2.05017636798559));
#44420=CARTESIAN_POINT('Ctrl Pts',(-17.1080053551432,21.1900817654324,-2.054353901051));
#44421=CARTESIAN_POINT('Ctrl Pts',(-17.0439628152326,21.1356900431327,-2.05853143411641));
#44422=CARTESIAN_POINT('Ctrl Pts',(-16.9826883976904,21.0782192350166,-2.06270896718182));
#44423=CARTESIAN_POINT('Ctrl Pts',(-16.9214787266056,21.0208091542215,-2.06688208599938));
#44424=CARTESIAN_POINT('Ctrl Pts',(-16.863031698376,20.9603267674198,-2.07105520481693));
#44425=CARTESIAN_POINT('Ctrl Pts',(-16.8076662208124,20.8970718167269,-2.07522832363449));
#44426=CARTESIAN_POINT('Ctrl Pts',(-16.7523325270974,20.8338531790195,-2.07939904677548));
#44427=CARTESIAN_POINT('Ctrl Pts',(-16.7000771741035,20.7678654828481,-2.08356976991648));
#44428=CARTESIAN_POINT('Ctrl Pts',(-16.6511815739689,20.6994446258377,-2.08774049305747));
#44429=CARTESIAN_POINT('Ctrl Pts',(-16.6022993757804,20.6310425225115,-2.09191007303207));
#44430=CARTESIAN_POINT('Ctrl Pts',(-16.5567753686354,20.5602089570937,-2.09607965300666));
#44431=CARTESIAN_POINT('Ctrl Pts',(-16.5148492380406,20.4873110497425,-2.10024923298126));
#44432=CARTESIAN_POINT('Ctrl Pts',(-16.4729220223143,20.4144112556488,-2.10441892087286));
#44433=CARTESIAN_POINT('Ctrl Pts',(-16.4345930962794,20.3394474129684,-2.10858860876446));
#44434=CARTESIAN_POINT('Ctrl Pts',(-16.40005685324,20.2628124298998,-2.11275829665606));
#44435=CARTESIAN_POINT('Ctrl Pts',(-16.3654855176096,20.1860995773274,-2.11693222140548));
#44436=CARTESIAN_POINT('Ctrl Pts',(-16.3347147521372,20.1077126129561,-2.1211061461549));
#44437=CARTESIAN_POINT('Ctrl Pts',(-16.307891103021,20.028065248312,-2.12528007090433));
#44438=CARTESIAN_POINT('Ctrl Pts',(-16.281054150168,19.9483783809302,-2.129456065797));
#44439=CARTESIAN_POINT('Ctrl Pts',(-16.2581683384313,19.8674303112531,-2.13363206068967));
#44440=CARTESIAN_POINT('Ctrl Pts',(-16.2393298383502,19.7856484008281,-2.13780805558235));
#44441=CARTESIAN_POINT('Ctrl Pts',(-16.2204575688713,19.7037198903093,-2.14199153625323));
#44442=CARTESIAN_POINT('Ctrl Pts',(-16.2056471887002,19.6209550062764,-2.1461750169241));
#44443=CARTESIAN_POINT('Ctrl Pts',(-16.1949433808616,19.5377896644778,-2.15035849759498));
#44444=CARTESIAN_POINT('Ctrl Pts',(-16.1850243997655,19.4607221885294,-2.15423523625811));
#44445=CARTESIAN_POINT('Ctrl Pts',(-16.1786313156337,19.3833111752999,-2.15811197492124));
#44446=CARTESIAN_POINT('Ctrl Pts',(-16.175759706546,19.3059031134812,-2.16198871358438));
#44447=CARTESIAN_POINT('Ctrl Pts',(-16.1726600297933,19.222347182862,-2.16617334886855));
#44448=CARTESIAN_POINT('Ctrl Pts',(-16.1736524807725,19.1384837389767,-2.17035798415272));
#44449=CARTESIAN_POINT('Ctrl Pts',(-16.1787729918871,19.0547472015922,-2.17454261943689));
#44450=CARTESIAN_POINT('Ctrl Pts',(-16.1838862146021,18.9711298525711,-2.17872129842233));
#44451=CARTESIAN_POINT('Ctrl Pts',(-16.1931157984834,18.8876395064996,-2.18289997740777));
#44452=CARTESIAN_POINT('Ctrl Pts',(-16.2064457142957,18.8047127459324,-2.18707865639321));
#44453=CARTESIAN_POINT('Ctrl Pts',(-16.2200145556268,18.7202996054384,-2.19133223405457));
#44454=CARTESIAN_POINT('Ctrl Pts',(-16.2378321872334,18.6364709352134,-2.19558581171593));
#44455=CARTESIAN_POINT('Ctrl Pts',(-16.2598262335642,18.5536841143858,-2.19983938937729));
#44456=CARTESIAN_POINT('Ctrl Pts',(-16.2813938882842,18.4725022554353,-2.20401050427562));
#44457=CARTESIAN_POINT('Ctrl Pts',(-16.3069773455562,18.3923226754403,-2.20818161917395));
#44458=CARTESIAN_POINT('Ctrl Pts',(-16.3364567548607,18.3135667781462,-2.21235273407229));
#44459=CARTESIAN_POINT('Ctrl Pts',(-16.3659262721024,18.2348373080532,-2.21652244931808));
#44460=CARTESIAN_POINT('Ctrl Pts',(-16.3992889838848,18.157531002365,-2.22069216456387));
#44461=CARTESIAN_POINT('Ctrl Pts',(-16.4363757550798,18.0820523355112,-2.22486187980966));
#44462=CARTESIAN_POINT('Ctrl Pts',(-16.4734612066025,18.0065763544426,-2.22903144668293));
#44463=CARTESIAN_POINT('Ctrl Pts',(-16.5142702504276,17.9329282954129,-2.23320101355621));
#44464=CARTESIAN_POINT('Ctrl Pts',(-16.5585869493337,17.861489696597,-2.23737058042948));
#44465=CARTESIAN_POINT('Ctrl Pts',(-16.6044617469375,17.7875394398614,-2.24168674208251));
#44466=CARTESIAN_POINT('Ctrl Pts',(-16.6540951656361,17.7159573493129,-2.24600290373554));
#44467=CARTESIAN_POINT('Ctrl Pts',(-16.7071987883436,17.647134005604,-2.25031906538857));
#44468=CARTESIAN_POINT('Ctrl Pts',(-16.7585725904851,17.5805525435089,-2.25449463050951));
#44469=CARTESIAN_POINT('Ctrl Pts',(-16.8131936461488,17.5165531861027,-2.25867019563045));
#44470=CARTESIAN_POINT('Ctrl Pts',(-16.8707609575705,17.4554544236146,-2.26284576075139));
#44471=CARTESIAN_POINT('Ctrl Pts',(-16.9312358147182,17.3912697527985,-2.26723222067046));
#44472=CARTESIAN_POINT('Ctrl Pts',(-16.9949619538586,17.3302867948565,-2.27161868058953));
#44473=CARTESIAN_POINT('Ctrl Pts',(-17.0615499834747,17.2728279379207,-2.2760051405086));
#44474=CARTESIAN_POINT('Ctrl Pts',(-17.1281380130909,17.2153690809849,-2.28039160042767));
#44475=CARTESIAN_POINT('Ctrl Pts',(-17.1975874282728,17.1614346208606,-2.28477806034674));
#44476=CARTESIAN_POINT('Ctrl Pts',(-17.2694745299327,17.1112940330789,-2.28916452026581));
#44477=CARTESIAN_POINT('Ctrl Pts',(-17.3380540324817,17.0634604650508,-2.29334915467525));
#44478=CARTESIAN_POINT('Ctrl Pts',(-17.4091070955312,17.0189012759421,-2.29753378908469));
#44479=CARTESIAN_POINT('Ctrl Pts',(-17.4822878905536,16.977881822414,-2.30171842349413));
#44480=CARTESIAN_POINT('Ctrl Pts',(-17.5553645218218,16.9369207549729,-2.30589710159728));
#44481=CARTESIAN_POINT('Ctrl Pts',(-17.6305624715267,16.8994896383272,-2.31007577970044));
#44482=CARTESIAN_POINT('Ctrl Pts',(-17.707505966713,16.865811308311,-2.31425445780359));
#44483=CARTESIAN_POINT('Ctrl Pts',(-17.7858286183102,16.8315293186269,-2.31850803568458));
#44484=CARTESIAN_POINT('Ctrl Pts',(-17.8659596132368,16.8011362520549,-2.32276161356556));
#44485=CARTESIAN_POINT('Ctrl Pts',(-17.9474751923746,16.7748188230368,-2.32701519144655));
#44486=CARTESIAN_POINT('Ctrl Pts',(-18.027410433529,16.7490116085464,-2.33118630545055));
#44487=CARTESIAN_POINT('Ctrl Pts',(-18.1086765943189,16.7271235613587,-2.33535741945454));
#44488=CARTESIAN_POINT('Ctrl Pts',(-18.1908544682415,16.7092820040359,-2.33952853345854));
#44489=CARTESIAN_POINT('Ctrl Pts',(-18.2730047666345,16.6914464336092,-2.34369824780747));
#44490=CARTESIAN_POINT('Ctrl Pts',(-18.3560657213857,16.6776547538851,-2.34786796215639));
#44491=CARTESIAN_POINT('Ctrl Pts',(-18.4396056840353,16.667983683354,-2.35203767650532));
#44492=CARTESIAN_POINT('Ctrl Pts',(-18.5231426740242,16.6583129569554,-2.35620724248039));
#44493=CARTESIAN_POINT('Ctrl Pts',(-18.6071581809429,16.6527626002748,-2.36037680845547));
#44494=CARTESIAN_POINT('Ctrl Pts',(-18.6912145090002,16.6513575636898,-2.36454637443054));
#44495=CARTESIAN_POINT('Ctrl Pts',(-18.7782261526213,16.6499031277724,-2.36886253714027));
#44496=CARTESIAN_POINT('Ctrl Pts',(-18.8652810139811,16.6528909431617,-2.37317869984999));
#44497=CARTESIAN_POINT('Ctrl Pts',(-18.951894561366,16.6602899106078,-2.37749486255972));
#44498=CARTESIAN_POINT('Ctrl Pts',(-19.0356866828631,16.6674478575793,-2.38167042678835));
#44499=CARTESIAN_POINT('Ctrl Pts',(-19.1190653399936,16.6787338735463,-2.38584599101697));
#44500=CARTESIAN_POINT('Ctrl Pts',(-19.2015998086535,16.694067259749,-2.3900215552456));
#44501=CARTESIAN_POINT('Ctrl Pts',(-19.2883028951203,16.7101750984661,-2.39440801719588));
#44502=CARTESIAN_POINT('Ctrl Pts',(-19.3740737042673,16.7307497815343,-2.39879447914615));
#44503=CARTESIAN_POINT('Ctrl Pts',(-19.4584303876714,16.7556383945703,-2.40318094109643));
#44504=CARTESIAN_POINT('Ctrl Pts',(-19.5427870710755,16.7805270076064,-2.4075674030467));
#44505=CARTESIAN_POINT('Ctrl Pts',(-19.6257291067112,16.8097292861734,-2.41195386499698));
#44506=CARTESIAN_POINT('Ctrl Pts',(-19.7068005673283,16.8430348279154,-2.41634032694725));
#44507=CARTESIAN_POINT('Ctrl Pts',(-19.7841418063579,16.8748079308701,-2.42052496109111));
#44508=CARTESIAN_POINT('Ctrl Pts',(-19.8600687027665,16.9104332654798,-2.42470959523496));
#44509=CARTESIAN_POINT('Ctrl Pts',(-19.9341709431984,16.949763677299,-2.42889422937882));
#44510=CARTESIAN_POINT('Ctrl Pts',(-20.0081677081793,16.9890381071006,-2.43307290720919));
#44511=CARTESIAN_POINT('Ctrl Pts',(-20.0803445731189,17.0320069250119,-2.43725158503956));
#44512=CARTESIAN_POINT('Ctrl Pts',(-20.1503107695878,17.0784747823415,-2.44143026286993));
#44513=CARTESIAN_POINT('Ctrl Pts',(-20.2215310652186,17.125775546187,-2.44568384081822));
#44514=CARTESIAN_POINT('Ctrl Pts',(-20.290460214072,17.1767018411764,-2.4499374187665));
#44515=CARTESIAN_POINT('Ctrl Pts',(-20.3567118459902,17.2309984179595,-2.45419099671478));
#44516=CARTESIAN_POINT('Ctrl Pts',(-20.421679055696,17.2842423455132,-2.45836211043023));
#44517=CARTESIAN_POINT('Ctrl Pts',(-20.4840712680033,17.3407267365035,-2.46253322414569));
#44518=CARTESIAN_POINT('Ctrl Pts',(-20.5435545162614,17.4001680219639,-2.46670433786114));
#44519=CARTESIAN_POINT('Ctrl Pts',(-20.6030178043004,17.4595893612863,-2.47087405191626));
#44520=CARTESIAN_POINT('Ctrl Pts',(-20.6595737417694,17.5219652996142,-2.47504376597137));
#44521=CARTESIAN_POINT('Ctrl Pts',(-20.7129241774329,17.5869744152349,-2.47921348002649));
#44522=CARTESIAN_POINT('Ctrl Pts',(-20.7662727146278,17.6519812175144,-2.48338304570285));
#44523=CARTESIAN_POINT('Ctrl Pts',(-20.8164156856331,17.7196206546306,-2.48755261137921));
#44524=CARTESIAN_POINT('Ctrl Pts',(-20.863095194694,17.7895381989196,-2.49172217705558));
#44525=CARTESIAN_POINT('Ctrl Pts',(-20.9114159042677,17.8619139676384,-2.49603834010334));
#44526=CARTESIAN_POINT('Ctrl Pts',(-20.9560247758967,17.9367305826506,-2.5003545031511));
#44527=CARTESIAN_POINT('Ctrl Pts',(-20.9966856911894,18.0135637959011,-2.50467066619885));
#44528=CARTESIAN_POINT('Ctrl Pts',(-21.0360220760754,18.0878941651683,-2.50884623011952));
#44529=CARTESIAN_POINT('Ctrl Pts',(-21.0716636083121,18.1641113216876,-2.51302179404019));
#44530=CARTESIAN_POINT('Ctrl Pts',(-21.1034449999947,18.2418094139954,-2.51719735796086));
#44531=CARTESIAN_POINT('Ctrl Pts',(-21.1368316009424,18.3234318686752,-2.52158382057216));
#44532=CARTESIAN_POINT('Ctrl Pts',(-21.1659576673028,18.4066882444733,-2.52597028318347));
#44533=CARTESIAN_POINT('Ctrl Pts',(-21.1906909603742,18.491090613191,-2.53035674579477));
#44534=CARTESIAN_POINT('Ctrl Pts',(-21.2154242534456,18.5754929819087,-2.53474320840607));
#44535=CARTESIAN_POINT('Ctrl Pts',(-21.2357647130149,18.6610407614697,-2.53912967101737));
#44536=CARTESIAN_POINT('Ctrl Pts',(-21.251642469363,18.7472367021208,-2.54351613362868));
#44537=CARTESIAN_POINT('Ctrl Pts',(-21.2744558894944,18.8710844400873,-2.54981867488504));
#44538=CARTESIAN_POINT('Ctrl Pts',(-21.288135817693,18.9966631545043,-2.5561212161414));
#44539=CARTESIAN_POINT('Ctrl Pts',(-21.2924829866055,19.122881856295,-2.56242375739777));
#44540=CARTESIAN_POINT('Ctrl Pts',(-21.293468437957,19.1514941308042,-2.56385246834134));
#44541=CARTESIAN_POINT('Ctrl Pts',(-21.2939744691008,19.18013916897,-2.56528117928492));
#44542=CARTESIAN_POINT('Ctrl Pts',(-21.2939990581246,19.2088040034447,-2.5667098902285));
#44543=CARTESIAN_POINT('Origin',(-18.734,19.211,1.76670989022852));
#44544=CARTESIAN_POINT('',(-17.1744642439897,21.2411350264762,-1.25003885507116));
#44545=CARTESIAN_POINT('',(-17.1763037754664,21.2387764608408,-1.31677679026378));
#44546=CARTESIAN_POINT('',(-17.1744642439897,21.2411350264762,1.76670989022852));
#44547=CARTESIAN_POINT('',(-21.2937660440385,19.2099923323681,-1.83329006739986));
#44548=CARTESIAN_POINT('Ctrl Pts',(-17.1763037754663,21.2387764608407,-1.31677679026378));
#44549=CARTESIAN_POINT('Ctrl Pts',(-16.7482596486795,20.905321345112,-1.34369096604507));
#44550=CARTESIAN_POINT('Ctrl Pts',(-15.9020680777596,19.7058145697047,-1.41299707738683));
#44551=CARTESIAN_POINT('Ctrl Pts',(-16.4540142581906,17.2197793398558,-1.52469512428907));
#44552=CARTESIAN_POINT('Ctrl Pts',(-19.1741877306222,16.2160836252784,-1.65187093097051));
#44553=CARTESIAN_POINT('Ctrl Pts',(-21.0477248457009,17.6266607733557,-1.75473569409313));
#44554=CARTESIAN_POINT('Ctrl Pts',(-21.2914432046423,18.8451666090485,-1.81520852165527));
#44555=CARTESIAN_POINT('Ctrl Pts',(-21.2901594433486,19.2099805605233,-1.83328941365693));
#44556=CARTESIAN_POINT('Ctrl Pts',(-21.293999801981,19.2099930953476,-1.8332901097715));
#44557=CARTESIAN_POINT('Ctrl Pts',(-21.2940336318695,19.2960037294466,-1.83754657624536));
#44558=CARTESIAN_POINT('Ctrl Pts',(-21.289728450138,19.3819895209311,-1.84180304271922));
#44559=CARTESIAN_POINT('Ctrl Pts',(-21.2811180404437,19.4674950058893,-1.84605950919308));
#44560=CARTESIAN_POINT('Ctrl Pts',(-21.2725026284394,19.5530501661775,-1.85031844850686));
#44561=CARTESIAN_POINT('Ctrl Pts',(-21.2595770559904,19.6381240344265,-1.85457738782065));
#44562=CARTESIAN_POINT('Ctrl Pts',(-21.2424267246312,19.7222683905308,-1.85883632713443));
#44563=CARTESIAN_POINT('Ctrl Pts',(-21.2252479654662,19.8065522214573,-1.86310232592114));
#44564=CARTESIAN_POINT('Ctrl Pts',(-21.203830549429,19.8899030384947,-1.86736832470785));
#44565=CARTESIAN_POINT('Ctrl Pts',(-21.17831059956,19.9718848092049,-1.87163432349455));
#44566=CARTESIAN_POINT('Ctrl Pts',(-21.1527682031271,20.0539386885619,-1.87590407452273));
#44567=CARTESIAN_POINT('Ctrl Pts',(-21.1231162332672,20.1346207166622,-1.88017382555091));
#44568=CARTESIAN_POINT('Ctrl Pts',(-21.0895392515833,20.2135142563825,-1.88444357657908));
#44569=CARTESIAN_POINT('Ctrl Pts',(-21.0558918629605,20.2925732264768,-1.88872228076758));
#44570=CARTESIAN_POINT('Ctrl Pts',(-21.0183032080418,20.3698358258174,-1.89300098495607));
#44571=CARTESIAN_POINT('Ctrl Pts',(-20.9770042478451,20.4449092122797,-1.89727968914457));
#44572=CARTESIAN_POINT('Ctrl Pts',(-20.9482314695913,20.4972124637696,-1.90026064087417));
#44573=CARTESIAN_POINT('Ctrl Pts',(-20.9176587209492,20.5484536579338,-1.90324159260377));
#44574=CARTESIAN_POINT('Ctrl Pts',(-20.8853760800086,20.5985089053289,-1.90622254433338));
#44575=CARTESIAN_POINT('Ctrl Pts',(-20.8400579767351,20.6687760459572,-1.91040717961721));
#44576=CARTESIAN_POINT('Ctrl Pts',(-20.79120937469,20.7369513806192,-1.91459181490104));
#44577=CARTESIAN_POINT('Ctrl Pts',(-20.7390496454785,20.8026582293842,-1.91877645018487));
#44578=CARTESIAN_POINT('Ctrl Pts',(-20.6869641590402,20.8682715527659,-1.92295512916998));
#44579=CARTESIAN_POINT('Ctrl Pts',(-20.631577190453,20.9314230120947,-1.92713380815509));
#44580=CARTESIAN_POINT('Ctrl Pts',(-20.5731519436452,20.9917639170272,-1.9313124871402));
#44581=CARTESIAN_POINT('Ctrl Pts',(-20.5136794822353,21.0531863728336,-1.93556606480165));
#44582=CARTESIAN_POINT('Ctrl Pts',(-20.4510590119848,21.1116961211984,-1.93981964246309));
#44583=CARTESIAN_POINT('Ctrl Pts',(-20.3856118363234,21.1669596984898,-1.94407322012453));
#44584=CARTESIAN_POINT('Ctrl Pts',(-20.3214334643362,21.2211518983045,-1.94824433502252));
#44585=CARTESIAN_POINT('Ctrl Pts',(-20.2545373774524,21.2722223583836,-1.9524154499205));
#44586=CARTESIAN_POINT('Ctrl Pts',(-20.185263188972,21.3198942970985,-1.95658656481849));
#44587=CARTESIAN_POINT('Ctrl Pts',(-20.1160122460259,21.3675502390951,-1.96075628006393));
#44588=CARTESIAN_POINT('Ctrl Pts',(-20.0443851649613,21.4118096640091,-1.96492599530937));
#44589=CARTESIAN_POINT('Ctrl Pts',(-19.9707522614864,21.4524378964647,-1.96909571055481));
#44590=CARTESIAN_POINT('Ctrl Pts',(-19.8971219781182,21.493064683231,-1.97326527742773));
#44591=CARTESIAN_POINT('Ctrl Pts',(-19.8214864174479,21.5300603129431,-1.97743484430066));
#44592=CARTESIAN_POINT('Ctrl Pts',(-19.7442411220083,21.5632357185034,-1.98160441117358));
#44593=CARTESIAN_POINT('Ctrl Pts',(-19.6642800151965,21.5975775141097,-1.98592057282702));
#44594=CARTESIAN_POINT('Ctrl Pts',(-19.5825943571936,21.6278252448873,-1.99023673448046));
#44595=CARTESIAN_POINT('Ctrl Pts',(-19.4996442824009,21.653823946343,-1.99455289613389));
#44596=CARTESIAN_POINT('Ctrl Pts',(-19.4193962595357,21.6789757547542,-1.99872846125448));
#44597=CARTESIAN_POINT('Ctrl Pts',(-19.337965398231,21.7001510303436,-2.00290402637506));
#44598=CARTESIAN_POINT('Ctrl Pts',(-19.2557808536486,21.7172611078588,-2.00707959149565));
#44599=CARTESIAN_POINT('Ctrl Pts',(-19.1694454234896,21.7352353621403,-2.01146605141551));
#44600=CARTESIAN_POINT('Ctrl Pts',(-19.0822787502277,21.7487228765315,-2.01585251133537));
#44601=CARTESIAN_POINT('Ctrl Pts',(-18.9947846789879,21.7576824205631,-2.02023897125523));
#44602=CARTESIAN_POINT('Ctrl Pts',(-18.9072906077481,21.7666419645947,-2.02462543117509));
#44603=CARTESIAN_POINT('Ctrl Pts',(-18.8194697218412,21.7710735849931,-2.02901189109496));
#44604=CARTESIAN_POINT('Ctrl Pts',(-18.7318236815475,21.7709990749291,-2.03339835101482));
#44605=CARTESIAN_POINT('Ctrl Pts',(-18.6482254298112,21.7709280059902,-2.03758222948078));
#44606=CARTESIAN_POINT('Ctrl Pts',(-18.5644751184015,21.7667575762838,-2.04176610794674));
#44607=CARTESIAN_POINT('Ctrl Pts',(-18.4810079806566,21.7584683586158,-2.04594998641271));
#44608=CARTESIAN_POINT('Ctrl Pts',(-18.3976520608152,21.750190186126,-2.05012828996374));
#44609=CARTESIAN_POINT('Ctrl Pts',(-18.3145790190074,21.7378041671174,-2.05430659351478));
#44610=CARTESIAN_POINT('Ctrl Pts',(-18.23222439898,21.7213428543171,-2.05848489706582));
#44611=CARTESIAN_POINT('Ctrl Pts',(-18.1499547981595,21.704898535436,-2.06265888712414));
#44612=CARTESIAN_POINT('Ctrl Pts',(-18.0684025946749,21.6843873684699,-2.06683287718245));
#44613=CARTESIAN_POINT('Ctrl Pts',(-17.987997155172,21.6598935778242,-2.07100686724077));
#44614=CARTESIAN_POINT('Ctrl Pts',(-17.9076457851309,21.635416258279,-2.0751780504567));
#44615=CARTESIAN_POINT('Ctrl Pts',(-17.8284400864338,21.6069617675245,-2.07934923367263));
#44616=CARTESIAN_POINT('Ctrl Pts',(-17.7507969266643,21.5746648909232,-2.08352041688856));
#44617=CARTESIAN_POINT('Ctrl Pts',(-17.6731854101502,21.5423811768249,-2.08768990015028));
#44618=CARTESIAN_POINT('Ctrl Pts',(-17.5971355905954,21.506258367263,-2.09185938341201));
#44619=CARTESIAN_POINT('Ctrl Pts',(-17.5230455881588,21.4664798630097,-2.09602886667374));
#44620=CARTESIAN_POINT('Ctrl Pts',(-17.4489417854745,21.4266939494813,-2.10019912655714));
#44621=CARTESIAN_POINT('Ctrl Pts',(-17.3767989370809,21.3832511941844,-2.10436938644054));
#44622=CARTESIAN_POINT('Ctrl Pts',(-17.3069908375595,21.3363811070749,-2.10853964632394));
#44623=CARTESIAN_POINT('Ctrl Pts',(-17.2618060884471,21.3060434651473,-2.11123893405498));
#44624=CARTESIAN_POINT('Ctrl Pts',(-17.2175989879755,21.274270839954,-2.11393822178602));
#44625=CARTESIAN_POINT('Ctrl Pts',(-17.1744642439897,21.2411350264762,-2.11663750951706));
#44626=CARTESIAN_POINT('',(-21.2939995273705,19.2125555907563,-1.76670989019937));
#44627=CARTESIAN_POINT('Ctrl Pts',(-21.2939995273702,19.2125555913393,-1.7667098902285));
#44628=CARTESIAN_POINT('Ctrl Pts',(-21.2939437779102,19.3043011465908,-1.77129369133236));
#44629=CARTESIAN_POINT('Ctrl Pts',(-21.2889563823285,19.3958958079181,-1.77587749243622));
#44630=CARTESIAN_POINT('Ctrl Pts',(-21.2790836672346,19.4869513123279,-1.78046129354008));
#44631=CARTESIAN_POINT('Ctrl Pts',(-21.2700706759975,19.5700776312323,-1.78464593361015));
#44632=CARTESIAN_POINT('Ctrl Pts',(-21.2569640809886,19.6529166096931,-1.78883057368023));
#44633=CARTESIAN_POINT('Ctrl Pts',(-21.2397911343996,19.7350331962428,-1.7930152137503));
#44634=CARTESIAN_POINT('Ctrl Pts',(-21.2226426310956,19.817032901329,-1.79719389757114));
#44635=CARTESIAN_POINT('Ctrl Pts',(-21.2014393661311,19.8983118104412,-1.80137258139199));
#44636=CARTESIAN_POINT('Ctrl Pts',(-21.1762603200948,19.9784402445079,-1.80555126521283));
#44637=CARTESIAN_POINT('Ctrl Pts',(-21.150630001539,20.0600047838296,-1.80980484167153));
#44638=CARTESIAN_POINT('Ctrl Pts',(-21.1208800342882,20.1403767226468,-1.81405841813022));
#44639=CARTESIAN_POINT('Ctrl Pts',(-21.0871481593181,20.21911395204,-1.81831199458892));
#44640=CARTESIAN_POINT('Ctrl Pts',(-21.0540701851445,20.2963248406336,-1.82248311440869));
#44641=CARTESIAN_POINT('Ctrl Pts',(-21.0171634957605,20.3719633904436,-1.82665423422847));
#44642=CARTESIAN_POINT('Ctrl Pts',(-20.9766076076857,20.4456299518278,-1.83082535404824));
#44643=CARTESIAN_POINT('Ctrl Pts',(-20.9360653282555,20.5192717941858,-1.83499507423679));
#44644=CARTESIAN_POINT('Ctrl Pts',(-20.8918765036875,20.5909425596168,-1.83916479442534));
#44645=CARTESIAN_POINT('Ctrl Pts',(-20.8442669697396,20.6602664752991,-1.84333451461389));
#44646=CARTESIAN_POINT('Ctrl Pts',(-20.7966591297285,20.7295879244518,-1.84750408644471));
#44647=CARTESIAN_POINT('Ctrl Pts',(-20.7456310834599,20.7965623111441,-1.85167365827553));
#44648=CARTESIAN_POINT('Ctrl Pts',(-20.691451661047,20.8608433242779,-1.85584323010635));
#44649=CARTESIAN_POINT('Ctrl Pts',(-20.6353675257683,20.9273841782754,-1.86015938594928));
#44650=CARTESIAN_POINT('Ctrl Pts',(-20.5759066466623,20.9910383508709,-1.86447554179221));
#44651=CARTESIAN_POINT('Ctrl Pts',(-20.5134108769448,21.0514610647907,-1.86879169763514));
#44652=CARTESIAN_POINT('Ctrl Pts',(-20.4529507187175,21.1099156907698,-1.87296726769975));
#44653=CARTESIAN_POINT('Ctrl Pts',(-20.3896507250023,21.1653458615584,-1.87714283776436));
#44654=CARTESIAN_POINT('Ctrl Pts',(-20.3238547775404,21.2174799491478,-1.88131840782897));
#44655=CARTESIAN_POINT('Ctrl Pts',(-20.2547359396678,21.2722469627211,-1.88570485656106));
#44656=CARTESIAN_POINT('Ctrl Pts',(-20.1828628806314,21.3233758659983,-1.89009130529315));
#44657=CARTESIAN_POINT('Ctrl Pts',(-20.1086675060193,21.3706039562602,-1.89447775402525));
#44658=CARTESIAN_POINT('Ctrl Pts',(-20.0344721314073,21.417832046522,-1.89886420275734));
#44659=CARTESIAN_POINT('Ctrl Pts',(-19.9579549835793,21.4611591040721,-1.90325065148943));
#44660=CARTESIAN_POINT('Ctrl Pts',(-19.8795742651121,21.5003797420072,-1.90763710022152));
#44661=CARTESIAN_POINT('Ctrl Pts',(-19.8047997208671,21.5377958997554,-1.91182173531048));
#44662=CARTESIAN_POINT('Ctrl Pts',(-19.7280509965254,21.5716144630821,-1.91600637039945));
#44663=CARTESIAN_POINT('Ctrl Pts',(-19.6497086514407,21.6016228614477,-1.92019100548841));
#44664=CARTESIAN_POINT('Ctrl Pts',(-19.5714778164362,21.6315885467837,-1.92436968429672));
#44665=CARTESIAN_POINT('Ctrl Pts',(-19.4916582921888,21.6577546763365,-1.92854836310503));
#44666=CARTESIAN_POINT('Ctrl Pts',(-19.4106541204074,21.6799550828915,-1.93272704191334));
#44667=CARTESIAN_POINT('Ctrl Pts',(-19.3281980247988,21.7025534109181,-1.93698061962124));
#44668=CARTESIAN_POINT('Ctrl Pts',(-19.2445148260133,21.7210422324063,-1.94123419732914));
#44669=CARTESIAN_POINT('Ctrl Pts',(-19.1600508252197,21.7352980597246,-1.94548777503704));
#44670=CARTESIAN_POINT('Ctrl Pts',(-19.0772243047676,21.7492775132415,-1.94965888980438));
#44671=CARTESIAN_POINT('Ctrl Pts',(-18.9936474610422,21.7591865556584,-1.95383000457171));
#44672=CARTESIAN_POINT('Ctrl Pts',(-18.9097535041071,21.7649598089622,-1.95800111933905));
#44673=CARTESIAN_POINT('Ctrl Pts',(-18.8258876981392,21.7707311250267,-1.96217083447142));
#44674=CARTESIAN_POINT('Ctrl Pts',(-18.7417054488562,21.7723693765771,-1.9663405496038));
#44675=CARTESIAN_POINT('Ctrl Pts',(-18.6576449614605,21.769861056816,-1.97051026473618));
#44676=CARTESIAN_POINT('Ctrl Pts',(-18.573587464861,21.7673528262987,-1.97467983151386));
#44677=CARTESIAN_POINT('Ctrl Pts',(-18.489652181338,21.7606983323727,-1.97884939829155));
#44678=CARTESIAN_POINT('Ctrl Pts',(-18.4062758155004,21.7499361667624,-1.98301896506923));
#44679=CARTESIAN_POINT('Ctrl Pts',(-18.3199680751373,21.7387956212864,-1.9873351268887));
#44680=CARTESIAN_POINT('Ctrl Pts',(-18.2342598094106,21.7232532494571,-1.99165128870818));
#44681=CARTESIAN_POINT('Ctrl Pts',(-18.149625962838,21.7034098749385,-1.99596745052766));
#44682=CARTESIAN_POINT('Ctrl Pts',(-18.0677490202284,21.6842128881249,-2.00014301559882));
#44683=CARTESIAN_POINT('Ctrl Pts',(-17.9868780138841,21.6609909777852,-2.00431858066999));
#44684=CARTESIAN_POINT('Ctrl Pts',(-17.9074274757339,21.6338862668578,-2.00849414574115));
#44685=CARTESIAN_POINT('Ctrl Pts',(-17.8239641319665,21.6054125792212,-2.01288060593478));
#44686=CARTESIAN_POINT('Ctrl Pts',(-17.7420690633811,21.5726537644299,-2.01726706612842));
#44687=CARTESIAN_POINT('Ctrl Pts',(-17.6621969477251,21.5358307932265,-2.02165352632205));
#44688=CARTESIAN_POINT('Ctrl Pts',(-17.5823248320691,21.4990078220231,-2.02603998651568));
#44689=CARTESIAN_POINT('Ctrl Pts',(-17.5044761476508,21.458121031537,-2.03042644670931));
#44690=CARTESIAN_POINT('Ctrl Pts',(-17.4290716121317,21.4134445288214,-2.03481290690294));
#44691=CARTESIAN_POINT('Ctrl Pts',(-17.3571349231711,21.370822693708,-2.03899763425939));
#44692=CARTESIAN_POINT('Ctrl Pts',(-17.2871547392091,21.3245934161538,-2.04318236161584));
#44693=CARTESIAN_POINT('Ctrl Pts',(-17.2195158137623,21.2749616395747,-2.0473670889723));
#44694=CARTESIAN_POINT('Ctrl Pts',(-17.2043800914437,21.2638554195465,-2.04830351531006));
#44695=CARTESIAN_POINT('Ctrl Pts',(-17.1893615177922,21.2525790096887,-2.04923994164783));
#44696=CARTESIAN_POINT('Ctrl Pts',(-17.1744642439897,21.2411350264762,-2.05017636798559));
#44697=CARTESIAN_POINT('Ctrl Pts',(-17.1744642439897,21.2411350264762,-1.25003885507116));
#44698=CARTESIAN_POINT('Ctrl Pts',(-17.1078166447992,21.1899367994448,-1.25422272222311));
#44699=CARTESIAN_POINT('Ctrl Pts',(-17.0437743697779,21.1355158045555,-1.25840658937506));
#44700=CARTESIAN_POINT('Ctrl Pts',(-16.9826476100414,21.0781809784234,-1.26259045652701));
#44701=CARTESIAN_POINT('Ctrl Pts',(-16.9380010114888,21.0363039841833,-1.26564632662279));
#44702=CARTESIAN_POINT('Ctrl Pts',(-16.8949090211694,20.9928733428054,-1.26870219671856));
#44703=CARTESIAN_POINT('Ctrl Pts',(-16.8534788428352,20.9480204884962,-1.27175806681434));
#44704=CARTESIAN_POINT('Ctrl Pts',(-16.7967467984314,20.8866016333375,-1.27594259521698));
#44705=CARTESIAN_POINT('Ctrl Pts',(-16.7429212490902,20.8222861496523,-1.28012712361962));
#44706=CARTESIAN_POINT('Ctrl Pts',(-16.6923122077178,20.755380444983,-1.28431165202226));
#44707=CARTESIAN_POINT('Ctrl Pts',(-16.6417752234727,20.6885700006218,-1.2884902224955));
#44708=CARTESIAN_POINT('Ctrl Pts',(-16.5944459257277,20.6191770244766,-1.29266879296874));
#44709=CARTESIAN_POINT('Ctrl Pts',(-16.5505962863687,20.5475433862397,-1.29684736344198));
#44710=CARTESIAN_POINT('Ctrl Pts',(-16.5059592440482,20.4746234309494,-1.30110096802756));
#44711=CARTESIAN_POINT('Ctrl Pts',(-16.464928391305,20.3993819010163,-1.30535457261313));
#44712=CARTESIAN_POINT('Ctrl Pts',(-16.4277464801527,20.322213166855,-1.30960817719871));
#44713=CARTESIAN_POINT('Ctrl Pts',(-16.3912866103988,20.2465429845162,-1.3137791803658));
#44714=CARTESIAN_POINT('Ctrl Pts',(-16.3585277410935,20.1690202117746,-1.3179501835329));
#44715=CARTESIAN_POINT('Ctrl Pts',(-16.3296531424777,20.0900427684264,-1.32212118669999));
#44716=CARTESIAN_POINT('Ctrl Pts',(-16.3007882398715,20.011091845483,-1.32629078925587));
#44717=CARTESIAN_POINT('Ctrl Pts',(-16.2758051753869,19.9306876537765,-1.33046039181176));
#44718=CARTESIAN_POINT('Ctrl Pts',(-16.2548387836586,19.8492473371574,-1.33462999436764));
#44719=CARTESIAN_POINT('Ctrl Pts',(-16.2338731420879,19.7678099343954,-1.3387994477391));
#44720=CARTESIAN_POINT('Ctrl Pts',(-16.2169240014122,19.6853369261728,-1.34296890111057));
#44721=CARTESIAN_POINT('Ctrl Pts',(-16.2040757356768,19.6022585037906,-1.34713835448203));
#44722=CARTESIAN_POINT('Ctrl Pts',(-16.1907749795004,19.5162542241174,-1.35145464773318));
#44723=CARTESIAN_POINT('Ctrl Pts',(-16.1818694215614,19.4296016124723,-1.35577094098433));
#44724=CARTESIAN_POINT('Ctrl Pts',(-16.1773942973163,19.3427849801953,-1.36008723423547));
#44725=CARTESIAN_POINT('Ctrl Pts',(-16.1730651983007,19.2588012119818,-1.36426268498078));
#44726=CARTESIAN_POINT('Ctrl Pts',(-16.1728818000995,19.1746644338097,-1.36843813572608));
#44727=CARTESIAN_POINT('Ctrl Pts',(-16.1768228602554,19.0908123302178,-1.37261358647139));
#44728=CARTESIAN_POINT('Ctrl Pts',(-16.1809633247949,19.0027175923176,-1.37700030097545));
#44729=CARTESIAN_POINT('Ctrl Pts',(-16.1896565650922,18.9149376772192,-1.38138701547952));
#44730=CARTESIAN_POINT('Ctrl Pts',(-16.2028167402278,18.8279708817217,-1.38577372998358));
#44731=CARTESIAN_POINT('Ctrl Pts',(-16.2159769153634,18.7410040862241,-1.39016044448765));
#44732=CARTESIAN_POINT('Ctrl Pts',(-16.2336038344097,18.6548509637837,-1.39454715899172));
#44733=CARTESIAN_POINT('Ctrl Pts',(-16.2555511520629,18.5699919593647,-1.39893387349578));
#44734=CARTESIAN_POINT('Ctrl Pts',(-16.2764876099038,18.489041430625,-1.40311854265335));
#44735=CARTESIAN_POINT('Ctrl Pts',(-16.3014331762482,18.4089670881459,-1.40730321181092));
#44736=CARTESIAN_POINT('Ctrl Pts',(-16.3302979817924,18.3301954770413,-1.41148788096849));
#44737=CARTESIAN_POINT('Ctrl Pts',(-16.3591217043841,18.2515359806832,-1.41566659413361));
#44738=CARTESIAN_POINT('Ctrl Pts',(-16.3918534291669,18.1741759609909,-1.41984530729872));
#44739=CARTESIAN_POINT('Ctrl Pts',(-16.4283528787703,18.0985291678587,-1.42402402046383));
#44740=CARTESIAN_POINT('Ctrl Pts',(-16.4655061666039,18.0215272648309,-1.42827758961855));
#44741=CARTESIAN_POINT('Ctrl Pts',(-16.5065633783675,17.9463010412761,-1.43253115877328));
#44742=CARTESIAN_POINT('Ctrl Pts',(-16.5513243019902,17.8732680398086,-1.436784727928));
#44743=CARTESIAN_POINT('Ctrl Pts',(-16.5952179124827,17.8016501673418,-1.44095587750601));
#44744=CARTESIAN_POINT('Ctrl Pts',(-16.6426727330391,17.7321416910373,-1.44512702708403));
#44745=CARTESIAN_POINT('Ctrl Pts',(-16.6934533489152,17.6651121111974,-1.44929817666204));
#44746=CARTESIAN_POINT('Ctrl Pts',(-16.7442169264156,17.598105021734,-1.45346792669788));
#44747=CARTESIAN_POINT('Ctrl Pts',(-16.7983038054767,17.5335755432561,-1.45763767673371));
#44748=CARTESIAN_POINT('Ctrl Pts',(-16.8554361909196,17.4718628532479,-1.46180742676954));
#44749=CARTESIAN_POINT('Ctrl Pts',(-16.9125665442965,17.4101523582163,-1.46597702849708));
#44750=CARTESIAN_POINT('Ctrl Pts',(-16.9727418755408,17.3512587894506,-1.47014663022461));
#44751=CARTESIAN_POINT('Ctrl Pts',(-17.0356461063899,17.2954859561832,-1.47431623195215));
#44752=CARTESIAN_POINT('Ctrl Pts',(-17.1007607791355,17.237753276882,-1.47863235263757));
#44753=CARTESIAN_POINT('Ctrl Pts',(-17.1687993162101,17.1833650934407,-1.48294847332299));
#44754=CARTESIAN_POINT('Ctrl Pts',(-17.2393736228791,17.1326131272512,-1.48726459400841));
#44755=CARTESIAN_POINT('Ctrl Pts',(-17.3076502260402,17.0835135041913,-1.49144019378605));
#44756=CARTESIAN_POINT('Ctrl Pts',(-17.3782995960785,17.0378171774819,-1.49561579356368));
#44757=CARTESIAN_POINT('Ctrl Pts',(-17.4509421894257,16.9957432079499,-1.49979139334132));
#44758=CARTESIAN_POINT('Ctrl Pts',(-17.5272517301713,16.9515453738088,-1.50417777448063));
#44759=CARTESIAN_POINT('Ctrl Pts',(-17.6057605029808,16.9113454944654,-1.50856415561995));
#44760=CARTESIAN_POINT('Ctrl Pts',(-17.6860031863916,16.8753410611421,-1.51295053675926));
#44761=CARTESIAN_POINT('Ctrl Pts',(-17.7662458698024,16.8393366278189,-1.51733691789858));
#44762=CARTESIAN_POINT('Ctrl Pts',(-17.8482218954648,16.8075277794807,-1.52172329903789));
#44763=CARTESIAN_POINT('Ctrl Pts',(-17.9314482086486,16.7800514974195,-1.52610968017721));
#44764=CARTESIAN_POINT('Ctrl Pts',(-18.0108467907137,16.7538389000734,-1.53029432358547));
#44765=CARTESIAN_POINT('Ctrl Pts',(-18.0916786884036,16.7314715385808,-1.53447896699374));
#44766=CARTESIAN_POINT('Ctrl Pts',(-18.1735366057567,16.7131047292344,-1.538663610402));
#44767=CARTESIAN_POINT('Ctrl Pts',(-18.2552780138067,16.6947640615763,-1.5428422977598));
#44768=CARTESIAN_POINT('Ctrl Pts',(-18.3380420957822,16.6804127357782,-1.5470209851176));
#44769=CARTESIAN_POINT('Ctrl Pts',(-18.421405029143,16.6701567572566,-1.5511996724754));
#44770=CARTESIAN_POINT('Ctrl Pts',(-18.5062619492397,16.6597169764711,-1.5554532480747));
#44771=CARTESIAN_POINT('Ctrl Pts',(-18.5917389394536,16.6535209329784,-1.559706823674));
#44772=CARTESIAN_POINT('Ctrl Pts',(-18.6773765359446,16.651626290805,-1.5639603992733));
#44773=CARTESIAN_POINT('Ctrl Pts',(-18.7613541238536,16.6497683745839,-1.56813152309571));
#44774=CARTESIAN_POINT('Ctrl Pts',(-18.8454856660802,16.6520466005361,-1.57230264691812));
#44775=CARTESIAN_POINT('Ctrl Pts',(-18.9293330503143,16.6584630268192,-1.57647377074053));
#44776=CARTESIAN_POINT('Ctrl Pts',(-19.0131523026761,16.6648773003091,-1.58064349509743));
#44777=CARTESIAN_POINT('Ctrl Pts',(-19.0966871280817,16.6754269816346,-1.58481321945433));
#44778=CARTESIAN_POINT('Ctrl Pts',(-19.1795019710685,16.6900620805395,-1.58898294381123));
#44779=CARTESIAN_POINT('Ctrl Pts',(-19.2623138707192,16.7046966592958,-1.59315251997126));
#44780=CARTESIAN_POINT('Ctrl Pts',(-19.3444053859658,16.7234162860397,-1.59732209613129));
#44781=CARTESIAN_POINT('Ctrl Pts',(-19.4253499785112,16.7461196363287,-1.60149167229132));
#44782=CARTESIAN_POINT('Ctrl Pts',(-19.5091400540413,16.7696210880709,-1.60580782350526));
#44783=CARTESIAN_POINT('Ctrl Pts',(-19.5917005594529,16.7973914247812,-1.6101239747192));
#44784=CARTESIAN_POINT('Ctrl Pts',(-19.6725761219549,16.8292622177712,-1.61444012593315));
#44785=CARTESIAN_POINT('Ctrl Pts',(-19.7508175783492,16.8600949833538,-1.61861570068712));
#44786=CARTESIAN_POINT('Ctrl Pts',(-19.8274817539353,16.8947649658156,-1.62279127544109));
#44787=CARTESIAN_POINT('Ctrl Pts',(-19.9021790183312,16.9330716031599,-1.62696685019507));
#44788=CARTESIAN_POINT('Ctrl Pts',(-19.9806484617505,16.9733127088547,-1.631353289639));
#44789=CARTESIAN_POINT('Ctrl Pts',(-20.0569466030573,17.0175671444772,-1.63573972908293));
#44790=CARTESIAN_POINT('Ctrl Pts',(-20.130655495903,17.0655505305965,-1.64012616852686));
#44791=CARTESIAN_POINT('Ctrl Pts',(-20.2043643887487,17.1135339167158,-1.64451260797079));
#44792=CARTESIAN_POINT('Ctrl Pts',(-20.275483608608,17.1652458506084,-1.64889904741472));
#44793=CARTESIAN_POINT('Ctrl Pts',(-20.3436364934689,17.2203542859431,-1.65328548685865));
#44794=CARTESIAN_POINT('Ctrl Pts',(-20.4078056279229,17.2722414599601,-1.6574155251252));
#44795=CARTESIAN_POINT('Ctrl Pts',(-20.4695977832764,17.3273436084189,-1.66154556339175));
#44796=CARTESIAN_POINT('Ctrl Pts',(-20.5286666498128,17.3854119807444,-1.6656756016583));
#44797=CARTESIAN_POINT('Ctrl Pts',(-20.5888757459544,17.4446012697411,-1.66988536368084));
#44798=CARTESIAN_POINT('Ctrl Pts',(-20.6462548736576,17.5068722657662,-1.67409512570339));
#44799=CARTESIAN_POINT('Ctrl Pts',(-20.7004701683271,17.5719163910649,-1.67830488772593));
#44800=CARTESIAN_POINT('Ctrl Pts',(-20.7535207653518,17.6355631848541,-1.68242421217099));
#44801=CARTESIAN_POINT('Ctrl Pts',(-20.8035417767949,17.7018647731871,-1.68654353661605));
#44802=CARTESIAN_POINT('Ctrl Pts',(-20.850256855771,17.7704942136866,-1.69066286106111));
#44803=CARTESIAN_POINT('Ctrl Pts',(-20.8969436374088,17.8390820823739,-1.69477969025368));
#44804=CARTESIAN_POINT('Ctrl Pts',(-20.9403281944971,17.9099946152069,-1.69889651944625));
#44805=CARTESIAN_POINT('Ctrl Pts',(-20.9801755816481,17.9828732734739,-1.70301334863882));
#44806=CARTESIAN_POINT('Ctrl Pts',(-21.0200115244872,18.05573100073,-1.70712899546334));
#44807=CARTESIAN_POINT('Ctrl Pts',(-21.0563120879347,18.1305533171676,-1.71124464228787));
#44808=CARTESIAN_POINT('Ctrl Pts',(-21.088887451558,18.206955633204,-1.71536028911239));
#44809=CARTESIAN_POINT('Ctrl Pts',(-21.1227568123705,18.2863928925596,-1.71963942253631));
#44810=CARTESIAN_POINT('Ctrl Pts',(-21.1525985841264,18.3675378137456,-1.72391855596022));
#44811=CARTESIAN_POINT('Ctrl Pts',(-21.1782545843983,18.4499352677678,-1.72819768938414));
#44812=CARTESIAN_POINT('Ctrl Pts',(-21.2029529680662,18.5292572162836,-1.73231710308656));
#44813=CARTESIAN_POINT('Ctrl Pts',(-21.2237724320015,18.6097393655103,-1.73643651678898));
#44814=CARTESIAN_POINT('Ctrl Pts',(-21.2406233770012,18.6909622649548,-1.7405559304914));
#44815=CARTESIAN_POINT('Ctrl Pts',(-21.2574836176246,18.7722299700469,-1.74467761661945));
#44816=CARTESIAN_POINT('Ctrl Pts',(-21.2703709121366,18.8542387712825,-1.74879930274751));
#44817=CARTESIAN_POINT('Ctrl Pts',(-21.279247341302,18.9365624449985,-1.75292098887556));
#44818=CARTESIAN_POINT('Ctrl Pts',(-21.2881358451795,19.0189981045868,-1.75704828178227));
#44819=CARTESIAN_POINT('Ctrl Pts',(-21.2930025796067,19.1017490200354,-1.76117557468897));
#44820=CARTESIAN_POINT('Ctrl Pts',(-21.2938616787506,19.1843882419918,-1.76530286759568));
#44821=CARTESIAN_POINT('Ctrl Pts',(-21.293959303024,19.19377900214,-1.76577187513024));
#44822=CARTESIAN_POINT('Ctrl Pts',(-21.2940052315681,19.2031683255366,-1.76624088266481));
#44823=CARTESIAN_POINT('Ctrl Pts',(-21.2939995273705,19.2125555907563,-1.76670989019937));
#44824=CARTESIAN_POINT('Origin',(-18.734,19.211,1.76670989022852));
#44825=CARTESIAN_POINT('',(-17.1769962363369,21.2378222944355,-0.450077502023298));
#44826=CARTESIAN_POINT('',(-17.1722616682727,21.2439679654049,-0.516748662007315));
#44827=CARTESIAN_POINT('',(-17.1744642439897,21.2411350264762,1.76670989022852));
#44828=CARTESIAN_POINT('',(-21.2914665409842,19.2078565222202,-0.166709890228504));
#44829=CARTESIAN_POINT('Ctrl Pts',(-21.2914665409842,19.2078565222202,-0.166709890228504));
#44830=CARTESIAN_POINT('Ctrl Pts',(-21.286948837742,19.7963214614176,-0.195923797939959));
#44831=CARTESIAN_POINT('Ctrl Pts',(-20.7940989485341,21.2477394666147,-0.267529641211891));
#44832=CARTESIAN_POINT('Ctrl Pts',(-18.7954430158883,22.0506149083018,-0.361985511810154));
#44833=CARTESIAN_POINT('Ctrl Pts',(-17.5432452930182,21.517847446733,-0.427227474696966));
#44834=CARTESIAN_POINT('Ctrl Pts',(-17.1769962363369,21.2378222944355,-0.450077502023298));
#44835=CARTESIAN_POINT('',(-19.3957372685685,16.7380050975816,0.));
#44836=CARTESIAN_POINT('Ctrl Pts',(-19.3957372685684,16.7380050975816,1.38777878078145E-15));
#44837=CARTESIAN_POINT('Ctrl Pts',(-20.2191097516036,16.9583275322964,-0.0423919355604767));
#44838=CARTESIAN_POINT('Ctrl Pts',(-21.1334433095435,17.8262083452195,-0.0979618989699786));
#44839=CARTESIAN_POINT('Ctrl Pts',(-21.2935044203301,18.9424073589822,-0.153531862379481));
#44840=CARTESIAN_POINT('Ctrl Pts',(-21.2914665409842,19.2078565222202,-0.166709890228504));
#44841=CARTESIAN_POINT('',(-18.0722320621911,16.7380133044256,-1.80302994756687E-11));
#44842=CARTESIAN_POINT('Origin',(-18.734,19.211,0.));
#44843=CARTESIAN_POINT('',(-21.2939992552734,19.212952690406,-0.233290109771496));
#44844=CARTESIAN_POINT('Ctrl Pts',(-18.0722320621911,16.7380133044256,-1.80300219199125E-11));
#44845=CARTESIAN_POINT('Ctrl Pts',(-18.1529464922157,16.7164142307207,-0.00418158398862037));
#44846=CARTESIAN_POINT('Ctrl Pts',(-18.2348706569439,16.6987304519573,-0.00836316795921058));
#44847=CARTESIAN_POINT('Ctrl Pts',(-18.3175895998167,16.6850937510234,-0.012544751929801));
#44848=CARTESIAN_POINT('Ctrl Pts',(-18.400190747281,16.6714764693507,-0.0167203811411207));
#44849=CARTESIAN_POINT('Ctrl Pts',(-18.4835839741038,16.6618948926126,-0.0208960103524402));
#44850=CARTESIAN_POINT('Ctrl Pts',(-18.5673406239762,16.656430632693,-0.02507163956376));
#44851=CARTESIAN_POINT('Ctrl Pts',(-18.6514938546105,16.6509404999577,-0.0292670400316576));
#44852=CARTESIAN_POINT('Ctrl Pts',(-18.7360135046785,16.6496069028829,-0.0334624404995552));
#44853=CARTESIAN_POINT('Ctrl Pts',(-18.8204558534901,16.6524603021651,-0.0376578409674528));
#44854=CARTESIAN_POINT('Ctrl Pts',(-18.9043486080215,16.6552951300557,-0.0418259356091481));
#44855=CARTESIAN_POINT('Ctrl Pts',(-18.9881645984016,16.6622626001438,-0.0459940302508442));
#44856=CARTESIAN_POINT('Ctrl Pts',(-19.0714668099551,16.6733404183818,-0.0501621248925395));
#44857=CARTESIAN_POINT('Ctrl Pts',(-19.1547409379247,16.684414501967,-0.0543288143490282));
#44858=CARTESIAN_POINT('Ctrl Pts',(-19.2375011746968,16.6995961209329,-0.0584955038055169));
#44859=CARTESIAN_POINT('Ctrl Pts',(-19.3193159599542,16.7188111574315,-0.0626621932620057));
#44860=CARTESIAN_POINT('Ctrl Pts',(-19.4011278018881,16.7380255026606,-0.0668287328199814));
#44861=CARTESIAN_POINT('Ctrl Pts',(-19.481993811599,16.7612728705988,-0.0709952723779566));
#44862=CARTESIAN_POINT('Ctrl Pts',(-19.5614943032478,16.7884283956728,-0.0751618119359323));
#44863=CARTESIAN_POINT('Ctrl Pts',(-19.6419503629735,16.8159103206512,-0.0793784318407133));
#44864=CARTESIAN_POINT('Ctrl Pts',(-19.721007396075,16.8473948424126,-0.0835950517454946));
#44865=CARTESIAN_POINT('Ctrl Pts',(-19.7982496311477,16.8827017539409,-0.0878116716502757));
#44866=CARTESIAN_POINT('Ctrl Pts',(-19.8746816906651,16.9176383396154,-0.0919840644250511));
#44867=CARTESIAN_POINT('Ctrl Pts',(-19.9493364580842,16.9563172372311,-0.0961564571998266));
#44868=CARTESIAN_POINT('Ctrl Pts',(-20.0218360729121,16.9985176273456,-0.100328849974602));
#44869=CARTESIAN_POINT('Ctrl Pts',(-20.0954884255321,17.0413890001219,-0.104567583444386));
#44870=CARTESIAN_POINT('Ctrl Pts',(-20.1669160788343,17.0878945550855,-0.10880631691417));
#44871=CARTESIAN_POINT('Ctrl Pts',(-20.2357552271545,17.1377582780307,-0.113045050383954));
#44872=CARTESIAN_POINT('Ctrl Pts',(-20.3045943754748,17.187622000976,-0.117283783853738));
#44873=CARTESIAN_POINT('Ctrl Pts',(-20.370844676157,17.2408435335627,-0.121522517323522));
#44874=CARTESIAN_POINT('Ctrl Pts',(-20.4341804449292,17.2971069897509,-0.125761250793306));
#44875=CARTESIAN_POINT('Ctrl Pts',(-20.4958618563844,17.3519008204458,-0.129889266735435));
#44876=CARTESIAN_POINT('Ctrl Pts',(-20.5550187589506,17.4097927026216,-0.134017282677563));
#44877=CARTESIAN_POINT('Ctrl Pts',(-20.611317450137,17.4705175406195,-0.138145298619692));
#44878=CARTESIAN_POINT('Ctrl Pts',(-20.6675250696014,17.5311441469278,-0.142266636866263));
#44879=CARTESIAN_POINT('Ctrl Pts',(-20.7208833454928,17.5945942591679,-0.146387975112834));
#44880=CARTESIAN_POINT('Ctrl Pts',(-20.7710927993391,17.6605636333984,-0.150509313359405));
#44881=CARTESIAN_POINT('Ctrl Pts',(-20.8212566260777,17.7264730589238,-0.154626906400053));
#44882=CARTESIAN_POINT('Ctrl Pts',(-20.8682770216554,17.7948968304612,-0.158744499440701));
#44883=CARTESIAN_POINT('Ctrl Pts',(-20.9118931634006,17.8654958681547,-0.162862092481349));
#44884=CARTESIAN_POINT('Ctrl Pts',(-20.9554835923167,17.9360532859129,-0.166977258095768));
#44885=CARTESIAN_POINT('Ctrl Pts',(-20.9956735017905,18.0087830229833,-0.171092423710186));
#44886=CARTESIAN_POINT('Ctrl Pts',(-21.0322449058945,18.0833163774666,-0.175207589324605));
#44887=CARTESIAN_POINT('Ctrl Pts',(-21.0688064212004,18.1578295783544,-0.179321642210581));
#44888=CARTESIAN_POINT('Ctrl Pts',(-21.1017511664475,18.2341450028519,-0.183435695096556));
#44889=CARTESIAN_POINT('Ctrl Pts',(-21.1309074513388,18.3118700484822,-0.187549747982531));
#44890=CARTESIAN_POINT('Ctrl Pts',(-21.1600799709319,18.3896383727037,-0.19166609164121));
#44891=CARTESIAN_POINT('Ctrl Pts',(-21.1854596457913,18.4688174432781,-0.195782435299889));
#44892=CARTESIAN_POINT('Ctrl Pts',(-21.2069235819087,18.5489962552674,-0.199898778958568));
#44893=CARTESIAN_POINT('Ctrl Pts',(-21.228393434594,18.6291971686732,-0.204016257293894));
#44894=CARTESIAN_POINT('Ctrl Pts',(-21.2459452949941,18.710397909727,-0.208133735629219));
#44895=CARTESIAN_POINT('Ctrl Pts',(-21.259507205158,18.7921762223861,-0.212251213964544));
#44896=CARTESIAN_POINT('Ctrl Pts',(-21.2730871889122,18.8740635187863,-0.216374179551669));
#44897=CARTESIAN_POINT('Ctrl Pts',(-21.2826665466436,18.9565294532014,-0.220497145138794));
#44898=CARTESIAN_POINT('Ctrl Pts',(-21.2882251802136,19.0391461994527,-0.224620110725918));
#44899=CARTESIAN_POINT('Ctrl Pts',(-21.2921215137894,19.0970565470744,-0.227510110407777));
#44900=CARTESIAN_POINT('Ctrl Pts',(-21.2940434286409,19.1550409048321,-0.230400110089637));
#44901=CARTESIAN_POINT('Ctrl Pts',(-21.2939992552734,19.212952690406,-0.233290109771496));
#44902=CARTESIAN_POINT('Ctrl Pts',(-21.2960081472498,19.2129542227284,-0.233290109771496));
#44903=CARTESIAN_POINT('Ctrl Pts',(-21.2971424692952,19.3442911272882,-0.239839092339242));
#44904=CARTESIAN_POINT('Ctrl Pts',(-21.2281784359338,20.3246261525587,-0.288780010467465));
#44905=CARTESIAN_POINT('Ctrl Pts',(-19.9618263685217,21.9781789381743,-0.380112864156167));
#44906=CARTESIAN_POINT('Ctrl Pts',(-17.9636855616863,21.8141356871712,-0.468050065667029));
#44907=CARTESIAN_POINT('Ctrl Pts',(-17.2221125833706,21.2827383699607,-0.513595331617412));
#44908=CARTESIAN_POINT('Ctrl Pts',(-17.1722616682727,21.2439679654049,-0.516748662007315));
#44909=CARTESIAN_POINT('Origin',(18.734,19.211,1.76670989022852));
#44910=CARTESIAN_POINT('',(20.2955779010576,21.2437559712559,-21.2501821977678));
#44911=CARTESIAN_POINT('',(20.2916907287181,21.2386977908337,-21.3166133948081));
#44912=CARTESIAN_POINT('',(20.2935358855687,21.2411349269503,1.76670989022852));
#44913=CARTESIAN_POINT('',(16.1765333526442,19.2141444406009,-21.8332901097715));
#44914=CARTESIAN_POINT('Ctrl Pts',(20.291690728718,21.2386977908338,-21.3166133948081));
#44915=CARTESIAN_POINT('Ctrl Pts',(20.5461545344932,21.0458241145069,-21.3324492520697));
#44916=CARTESIAN_POINT('Ctrl Pts',(21.351877546268,20.1710072872175,-21.3906770448917));
#44917=CARTESIAN_POINT('Ctrl Pts',(21.4520480990298,17.8786570465205,-21.4912967732743));
#44918=CARTESIAN_POINT('Ctrl Pts',(19.0860574232626,16.2052798622314,-21.6184725799557));
#44919=CARTESIAN_POINT('Ctrl Pts',(16.6739013896572,17.1742593445012,-21.7324703587881));
#44920=CARTESIAN_POINT('Ctrl Pts',(16.1810511499193,18.6256790739174,-21.80407620206));
#44921=CARTESIAN_POINT('Ctrl Pts',(16.1765333526442,19.2141444406009,-21.8332901097715));
#44922=CARTESIAN_POINT('',(18.0722627314313,21.6839949024184,-22.));
#44923=CARTESIAN_POINT('Ctrl Pts',(16.1765333526442,19.2141444406009,-21.8332901097715));
#44924=CARTESIAN_POINT('Ctrl Pts',(16.1744954308812,19.4795937966726,-21.8464681376205));
#44925=CARTESIAN_POINT('Ctrl Pts',(16.3345564048251,20.5957933867983,-21.90203810103));
#44926=CARTESIAN_POINT('Ctrl Pts',(17.2488902483962,21.4636724677035,-21.9576080644395));
#44927=CARTESIAN_POINT('Ctrl Pts',(18.0722627314313,21.6839949024184,-22.));
#44928=CARTESIAN_POINT('',(19.3957680159044,21.6839866746762,-21.9999999999818));
#44929=CARTESIAN_POINT('Origin',(18.734,19.211,-22.));
#44930=CARTESIAN_POINT('',(16.1740007447408,19.2090472910618,-21.7667098902285));
#44931=CARTESIAN_POINT('Ctrl Pts',(16.1740007447408,19.2090472910617,-21.7667098902285));
#44932=CARTESIAN_POINT('Ctrl Pts',(16.1739377131957,19.291681576866,-21.770833628557));
#44933=CARTESIAN_POINT('Ctrl Pts',(16.1778799213038,19.3744638154111,-21.7749573668856));
#44934=CARTESIAN_POINT('Ctrl Pts',(16.1858438026722,19.4569674653686,-21.7790811052141));
#44935=CARTESIAN_POINT('Ctrl Pts',(16.1937978799175,19.539369547271,-21.7831997669178));
#44936=CARTESIAN_POINT('Ctrl Pts',(16.2057637505312,19.6214932533812,-21.7873184286214));
#44937=CARTESIAN_POINT('Ctrl Pts',(16.2217058123253,19.7029125070335,-21.7914370903251));
#44938=CARTESIAN_POINT('Ctrl Pts',(16.237637182478,19.7842771563645,-21.795552989823));
#44939=CARTESIAN_POINT('Ctrl Pts',(16.257539363199,19.864937827131,-21.799668889321));
#44940=CARTESIAN_POINT('Ctrl Pts',(16.2813251278132,19.9444752697558,-21.803784788819));
#44941=CARTESIAN_POINT('Ctrl Pts',(16.3051025310591,20.0239847527225,-21.807899241462));
#44942=CARTESIAN_POINT('Ctrl Pts',(16.3327606729939,20.1023713378542,-21.812013694105));
#44943=CARTESIAN_POINT('Ctrl Pts',(16.3641619718452,20.1792291672488,-21.816128146748));
#44944=CARTESIAN_POINT('Ctrl Pts',(16.3955622525032,20.2560845045131,-21.820242465979));
#44945=CARTESIAN_POINT('Ctrl Pts',(16.4307052681111,20.331410746752,-21.8243567852101));
#44946=CARTESIAN_POINT('Ctrl Pts',(16.4694052055202,20.4048217692834,-21.8284711044412));
#44947=CARTESIAN_POINT('Ctrl Pts',(16.5081407935446,20.4783004184906,-21.8325892138079));
#44948=CARTESIAN_POINT('Ctrl Pts',(16.5504396244287,20.5498599054295,-21.8367073231746));
#44949=CARTESIAN_POINT('Ctrl Pts',(16.596070140308,20.6191391674964,-21.8408254325413));
#44950=CARTESIAN_POINT('Ctrl Pts',(16.6417225473624,20.6884516661905,-21.8449455175651));
#44951=CARTESIAN_POINT('Ctrl Pts',(16.6907095403228,20.7554813807654,-21.849065602589));
#44952=CARTESIAN_POINT('Ctrl Pts',(16.7427579777409,20.819898756538,-21.8531856876128));
#44953=CARTESIAN_POINT('Ctrl Pts',(16.7948924451882,20.88442260676,-21.8573125826592));
#44954=CARTESIAN_POINT('Ctrl Pts',(16.8500981442698,20.9463251442536,-21.8614394777056));
#44955=CARTESIAN_POINT('Ctrl Pts',(16.9080639888335,21.0053125934813,-21.865566372752));
#44956=CARTESIAN_POINT('Ctrl Pts',(16.9486676888643,21.0466319033619,-21.8684571649036));
#44957=CARTESIAN_POINT('Ctrl Pts',(16.990624926523,21.0865216582628,-21.8713479570551));
#44958=CARTESIAN_POINT('Ctrl Pts',(17.0338195605382,21.124893015106,-21.8742387492067));
#44959=CARTESIAN_POINT('Ctrl Pts',(17.096294549636,21.1803918092294,-21.8784198752255));
#44960=CARTESIAN_POINT('Ctrl Pts',(17.1616053008015,21.2329308852276,-21.8826010012442));
#44961=CARTESIAN_POINT('Ctrl Pts',(17.2294394909469,21.2822068159887,-21.886782127263));
#44962=CARTESIAN_POINT('Ctrl Pts',(17.2971786580471,21.3314137203636,-21.8909573963043));
#44963=CARTESIAN_POINT('Ctrl Pts',(17.3674338732044,21.377366290339,-21.8951326653455));
#44964=CARTESIAN_POINT('Ctrl Pts',(17.4398581404809,21.4197998658639,-21.8993079343868));
#44965=CARTESIAN_POINT('Ctrl Pts',(17.5126333816213,21.462439077932,-21.9035034371199));
#44966=CARTESIAN_POINT('Ctrl Pts',(17.5875984040009,21.5015247814357,-21.907698939853));
#44967=CARTESIAN_POINT('Ctrl Pts',(17.6643697795486,21.5368312904201,-21.9118944425862));
#44968=CARTESIAN_POINT('Ctrl Pts',(17.7406374344996,21.5719061425448,-21.916062417336));
#44969=CARTESIAN_POINT('Ctrl Pts',(17.8186873858889,21.603251049355,-21.9202303920859));
#44970=CARTESIAN_POINT('Ctrl Pts',(17.8981187211547,21.6306905768457,-21.9243983668358));
#44971=CARTESIAN_POINT('Ctrl Pts',(17.9775250004187,21.6581214487492,-21.9285650268302));
#44972=CARTESIAN_POINT('Ctrl Pts',(18.0583113629463,21.681649237629,-21.9327316868246));
#44973=CARTESIAN_POINT('Ctrl Pts',(18.1400586239765,21.7011473132823,-21.936898346819));
#44974=CARTESIAN_POINT('Ctrl Pts',(18.2218047170262,21.720645110353,-21.9410649472815));
#44975=CARTESIAN_POINT('Ctrl Pts',(18.3045112328003,21.7361132028771,-21.9452315477439));
#44976=CARTESIAN_POINT('Ctrl Pts',(18.3877469394689,21.7474756687327,-21.9493981482063));
#44977=CARTESIAN_POINT('Ctrl Pts',(18.471985895769,21.7589750877077,-21.9536149691876));
#44978=CARTESIAN_POINT('Ctrl Pts',(18.5567664092282,21.7662691624329,-21.9578317901689));
#44979=CARTESIAN_POINT('Ctrl Pts',(18.6416360132955,21.7693332257468,-21.9620486111502));
#44980=CARTESIAN_POINT('Ctrl Pts',(18.7256171152011,21.7723652112997,-21.9662212861195));
#44981=CARTESIAN_POINT('Ctrl Pts',(18.8096849858173,21.7712554086671,-21.9703939610888));
#44982=CARTESIAN_POINT('Ctrl Pts',(18.8934029358148,21.766032427202,-21.9745666360581));
#44983=CARTESIAN_POINT('Ctrl Pts',(18.9784494629181,21.7607265586906,-21.9788055300454));
#44984=CARTESIAN_POINT('Ctrl Pts',(19.0631343741421,21.7511758815698,-21.9830444240327));
#44985=CARTESIAN_POINT('Ctrl Pts',(19.1470089679579,21.7374646430113,-21.98728331802));
#44986=CARTESIAN_POINT('Ctrl Pts',(19.2308835617738,21.7237534044529,-21.9915222120073));
#44987=CARTESIAN_POINT('Ctrl Pts',(19.3139473718607,21.7058817725444,-21.9957611059945));
#44988=CARTESIAN_POINT('Ctrl Pts',(19.3957680159044,21.6839866746762,-21.9999999999818));
#44989=CARTESIAN_POINT('Ctrl Pts',(20.2955779010576,21.2437559712559,-21.2501821977678));
#44990=CARTESIAN_POINT('Ctrl Pts',(20.9031380122802,20.7701939876851,-21.2886333060055));
#44991=CARTESIAN_POINT('Ctrl Pts',(21.7186680886982,19.1595846939594,-21.3694763498038));
#44992=CARTESIAN_POINT('Ctrl Pts',(20.3959082140047,16.6810622569708,-21.4927113291624));
#44993=CARTESIAN_POINT('Ctrl Pts',(17.5061735829933,16.443821090153,-21.6198871358438));
#44994=CARTESIAN_POINT('Ctrl Pts',(16.2398215703271,18.0973737800013,-21.7112199895325));
#44995=CARTESIAN_POINT('Ctrl Pts',(16.1708575106781,19.0777088474958,-21.7601609076608));
#44996=CARTESIAN_POINT('Ctrl Pts',(16.1719918287103,19.2090457587065,-21.7667098902285));
#44997=CARTESIAN_POINT('Origin',(18.734,19.211,1.76670989022852));
#44998=CARTESIAN_POINT('',(20.294072606836,21.2418453397989,-20.4499991791617));
#44999=CARTESIAN_POINT('',(20.2935358855687,21.2411349269503,-20.5167505016347));
#45000=CARTESIAN_POINT('',(20.2935358855687,21.2411349269503,1.76670989022852));
#45001=CARTESIAN_POINT('',(16.1740711622283,19.2096583021525,-21.0332900817674));
#45002=CARTESIAN_POINT('Ctrl Pts',(20.2935358855687,21.2411349269503,-20.5167505016347));
#45003=CARTESIAN_POINT('Ctrl Pts',(20.3601729811252,21.1899447619761,-20.5209209409253));
#45004=CARTESIAN_POINT('Ctrl Pts',(20.424326855727,21.135439617875,-20.5250913802159));
#45005=CARTESIAN_POINT('Ctrl Pts',(20.4856569022985,21.0778953094991,-20.5292618195065));
#45006=CARTESIAN_POINT('Ctrl Pts',(20.5469737333947,21.020363400843,-20.5334313601456));
#45007=CARTESIAN_POINT('Ctrl Pts',(20.6054676099457,20.9597939435863,-20.5376009007847));
#45008=CARTESIAN_POINT('Ctrl Pts',(20.6608329431096,20.8965013525203,-20.5417704414238));
#45009=CARTESIAN_POINT('Ctrl Pts',(20.7162029534294,20.8332034146189,-20.5459403342977));
#45010=CARTESIAN_POINT('Ctrl Pts',(20.768443593682,20.7671822332372,-20.5501102271715));
#45011=CARTESIAN_POINT('Ctrl Pts',(20.8172888253184,20.6987861641726,-20.5542801200453));
#45012=CARTESIAN_POINT('Ctrl Pts',(20.8661854255174,20.6303181657171,-20.5584543982275));
#45013=CARTESIAN_POINT('Ctrl Pts',(20.9116792192141,20.5594706676898,-20.5626286764097));
#45014=CARTESIAN_POINT('Ctrl Pts',(20.9535471859618,20.4866215305838,-20.5668029545919));
#45015=CARTESIAN_POINT('Ctrl Pts',(20.9954381169732,20.4137324362761,-20.5709795223342));
#45016=CARTESIAN_POINT('Ctrl Pts',(21.0336990517046,20.3388399266131,-20.5751560900764));
#45017=CARTESIAN_POINT('Ctrl Pts',(21.0681538129048,20.262344842429,-20.5793326578187));
#45018=CARTESIAN_POINT('Ctrl Pts',(21.102668195464,20.1857173892858,-20.5835164527956));
#45019=CARTESIAN_POINT('Ctrl Pts',(21.1333630817951,20.1074822515155,-20.5877002477726));
#45020=CARTESIAN_POINT('Ctrl Pts',(21.1601112326058,20.0280583131111,-20.5918840427495));
#45021=CARTESIAN_POINT('Ctrl Pts',(21.1796790940316,19.9699549835918,-20.5949447373344));
#45022=CARTESIAN_POINT('Ctrl Pts',(21.1971357839931,19.9112157932946,-20.5980054319194));
#45023=CARTESIAN_POINT('Ctrl Pts',(21.2124488472496,19.8520080432935,-20.6010661265043));
#45024=CARTESIAN_POINT('Ctrl Pts',(21.2333845649191,19.7710603767749,-20.6052506476957));
#45025=CARTESIAN_POINT('Ctrl Pts',(21.2503893834586,19.6889352855203,-20.6094351688871));
#45026=CARTESIAN_POINT('Ctrl Pts',(21.2633350895848,19.60604936982,-20.6136196900785));
#45027=CARTESIAN_POINT('Ctrl Pts',(21.2762623681897,19.5232814377936,-20.6177982548275));
#45028=CARTESIAN_POINT('Ctrl Pts',(21.2851419407631,19.4397552831428,-20.6219768195765));
#45029=CARTESIAN_POINT('Ctrl Pts',(21.2898958841357,19.3559007572729,-20.6261553843254));
#45030=CARTESIAN_POINT('Ctrl Pts',(21.2947352019949,19.2705403158833,-20.630408990528));
#45031=CARTESIAN_POINT('Ctrl Pts',(21.2952991221744,19.1848400591974,-20.6346625967305));
#45032=CARTESIAN_POINT('Ctrl Pts',(21.291560298618,19.099262276142,-20.638916202933));
#45033=CARTESIAN_POINT('Ctrl Pts',(21.2878940830536,19.0153464145152,-20.6430872040592));
#45034=CARTESIAN_POINT('Ctrl Pts',(21.2800907693894,18.9315487929963,-20.6472582051854));
#45035=CARTESIAN_POINT('Ctrl Pts',(21.2681770979566,18.848306691277,-20.6514292063116));
#45036=CARTESIAN_POINT('Ctrl Pts',(21.2562674231734,18.7650925145781,-20.6555988082025));
#45037=CARTESIAN_POINT('Ctrl Pts',(21.2402501942426,18.6824339426084,-20.6597684100934));
#45038=CARTESIAN_POINT('Ctrl Pts',(21.2202039193129,18.6007622827183,-20.6639380119843));
#45039=CARTESIAN_POINT('Ctrl Pts',(21.200158355009,18.519093518029,-20.6681074660658));
#45040=CARTESIAN_POINT('Ctrl Pts',(21.1760841391767,18.4384120424547,-20.6722769201474));
#45041=CARTESIAN_POINT('Ctrl Pts',(21.1481104103814,18.359136791211,-20.6764463742289));
#45042=CARTESIAN_POINT('Ctrl Pts',(21.1191514849296,18.2770695735108,-20.6807626708086));
#45043=CARTESIAN_POINT('Ctrl Pts',(21.0860134223639,18.196509977735,-20.6850789673883));
#45044=CARTESIAN_POINT('Ctrl Pts',(21.0488942540618,18.1179013802444,-20.6893952639681));
#45045=CARTESIAN_POINT('Ctrl Pts',(21.0129862924118,18.0418577986349,-20.693570718838));
#45046=CARTESIAN_POINT('Ctrl Pts',(20.973353301174,17.9676402439562,-20.697746173708));
#45047=CARTESIAN_POINT('Ctrl Pts',(20.93022101813,17.8956242971971,-20.7019216285779));
#45048=CARTESIAN_POINT('Ctrl Pts',(20.8849064011798,17.8199646100352,-20.7063083460125));
#45049=CARTESIAN_POINT('Ctrl Pts',(20.8357293767458,17.7467356778436,-20.7106950634472));
#45050=CARTESIAN_POINT('Ctrl Pts',(20.783001266459,17.6763359292505,-20.7150817808818));
#45051=CARTESIAN_POINT('Ctrl Pts',(20.7302731561721,17.6059361806573,-20.7194684983164));
#45052=CARTESIAN_POINT('Ctrl Pts',(20.6739943900424,17.5383660129748,-20.723855215751));
#45053=CARTESIAN_POINT('Ctrl Pts',(20.6145211534981,17.4739795075341,-20.7282419331856));
#45054=CARTESIAN_POINT('Ctrl Pts',(20.557786240175,17.412557546706,-20.7324266732114));
#45055=CARTESIAN_POINT('Ctrl Pts',(20.4979333333722,17.3538038540671,-20.7366114132371));
#45056=CARTESIAN_POINT('Ctrl Pts',(20.4352433666198,17.2980517499074,-20.7407961532628));
#45057=CARTESIAN_POINT('Ctrl Pts',(20.3726426389602,17.2423790088015,-20.7449749363161));
#45058=CARTESIAN_POINT('Ctrl Pts',(20.3072132139949,17.1896996722069,-20.7491537193694));
#45059=CARTESIAN_POINT('Ctrl Pts',(20.2392743867932,17.1403119451582,-20.7533325024227));
#45060=CARTESIAN_POINT('Ctrl Pts',(20.1701199701232,17.0900405525631,-20.7575860539829));
#45061=CARTESIAN_POINT('Ctrl Pts',(20.0983657943851,17.0431800747247,-20.7618396055431));
#45062=CARTESIAN_POINT('Ctrl Pts',(20.0243857326348,17.0000036949347,-20.7660931571032));
#45063=CARTESIAN_POINT('Ctrl Pts',(19.9518376849991,16.9576630698576,-20.7702643736974));
#45064=CARTESIAN_POINT('Ctrl Pts',(19.877149571062,16.9188654316441,-20.7744355902916));
#45065=CARTESIAN_POINT('Ctrl Pts',(19.8007035800232,16.8838250017745,-20.7786068068857));
#45066=CARTESIAN_POINT('Ctrl Pts',(19.7242832605526,16.8487963389417,-20.7827766227305));
#45067=CARTESIAN_POINT('Ctrl Pts',(19.6461066541874,16.8175225701701,-20.7869464385753));
#45068=CARTESIAN_POINT('Ctrl Pts',(19.5665789492871,16.7901711557394,-20.7911162544201));
#45069=CARTESIAN_POINT('Ctrl Pts',(19.487054097481,16.7628207225537,-20.7952859206708));
#45070=CARTESIAN_POINT('Ctrl Pts',(19.4061786787909,16.739392512731,-20.7994555869215));
#45071=CARTESIAN_POINT('Ctrl Pts',(19.3243748845357,16.7200047178468,-20.8036252531722));
#45072=CARTESIAN_POINT('Ctrl Pts',(19.2396994039173,16.699936322916,-20.8079412937301));
#45073=CARTESIAN_POINT('Ctrl Pts',(19.1540296670697,16.6841974189308,-20.812257334288));
#45074=CARTESIAN_POINT('Ctrl Pts',(19.0678455536436,16.6728614800779,-20.816573374846));
#45075=CARTESIAN_POINT('Ctrl Pts',(18.9844645957683,16.6618942449066,-20.8207490353203));
#45076=CARTESIAN_POINT('Ctrl Pts',(18.9006026820952,16.655047941956,-20.8249246957946));
#45077=CARTESIAN_POINT('Ctrl Pts',(18.8166978402032,16.6523360777105,-20.8291003562689));
#45078=CARTESIAN_POINT('Ctrl Pts',(18.7285618465719,16.6494874596275,-20.8334865868686));
#45079=CARTESIAN_POINT('Ctrl Pts',(18.6403790648446,16.6512012136138,-20.8378728174683));
#45080=CARTESIAN_POINT('Ctrl Pts',(18.5526528284857,16.6574312808574,-20.842259048068));
#45081=CARTESIAN_POINT('Ctrl Pts',(18.4649265921268,16.6636613481009,-20.8466452786677));
#45082=CARTESIAN_POINT('Ctrl Pts',(18.377657467477,16.674407582305,-20.8510315092674));
#45083=CARTESIAN_POINT('Ctrl Pts',(18.291335798662,16.6895622345864,-20.8554177398671));
#45084=CARTESIAN_POINT('Ctrl Pts',(18.2089776381982,16.7040210524186,-20.8596025742027));
#45085=CARTESIAN_POINT('Ctrl Pts',(18.1271754855616,16.7225461173931,-20.8637874085383));
#45086=CARTESIAN_POINT('Ctrl Pts',(18.0463616920216,16.7450815996062,-20.8679722428739));
#45087=CARTESIAN_POINT('Ctrl Pts',(17.9656628851168,16.7675850170052,-20.8721511227802));
#45088=CARTESIAN_POINT('Ctrl Pts',(17.8859500832462,16.7940873946837,-20.8763300026865));
#45089=CARTESIAN_POINT('Ctrl Pts',(17.8076468720086,16.8244816400747,-20.8805088825927));
#45090=CARTESIAN_POINT('Ctrl Pts',(17.7279449225119,16.8554188209751,-20.8847624102576));
#45091=CARTESIAN_POINT('Ctrl Pts',(17.6497038935225,16.8903881967178,-20.8890159379224));
#45092=CARTESIAN_POINT('Ctrl Pts',(17.5733558329037,16.9292232542632,-20.8932694655872));
#45093=CARTESIAN_POINT('Ctrl Pts',(17.4984833659798,16.9673077391602,-20.8974407845024));
#45094=CARTESIAN_POINT('Ctrl Pts',(17.4254317755317,17.0091095912714,-20.9016121034175));
#45095=CARTESIAN_POINT('Ctrl Pts',(17.3545880686222,17.0544233786919,-20.9057834223326));
#45096=CARTESIAN_POINT('Ctrl Pts',(17.2837681207939,17.0997219690822,-20.9099533422992));
#45097=CARTESIAN_POINT('Ctrl Pts',(17.2151549730963,17.1485299079791,-20.9141232622657));
#45098=CARTESIAN_POINT('Ctrl Pts',(17.1491087606961,17.2005971151091,-20.9182931822323));
#45099=CARTESIAN_POINT('Ctrl Pts',(17.0830648915161,17.2526624749729,-20.9224629542563));
#45100=CARTESIAN_POINT('Ctrl Pts',(17.0195881372622,17.3079865877152,-20.9266327262804));
#45101=CARTESIAN_POINT('Ctrl Pts',(16.9590064076373,17.3662784093334,-20.9308024983044));
#45102=CARTESIAN_POINT('Ctrl Pts',(16.8963013152165,17.426613333486,-20.9351184189914));
#45103=CARTESIAN_POINT('Ctrl Pts',(16.8366983378611,17.4901275014,-20.9394343396785));
#45104=CARTESIAN_POINT('Ctrl Pts',(16.7805189594486,17.5564572159638,-20.9437502603655));
#45105=CARTESIAN_POINT('Ctrl Pts',(16.7261639013718,17.6206329969926,-20.947926029593));
#45106=CARTESIAN_POINT('Ctrl Pts',(16.675013743749,17.6874438611075,-20.9521017988205));
#45107=CARTESIAN_POINT('Ctrl Pts',(16.6273169449433,17.7565287883437,-20.9562775680481));
#45108=CARTESIAN_POINT('Ctrl Pts',(16.5772188726476,17.8290917645997,-20.9606635644648));
#45109=CARTESIAN_POINT('Ctrl Pts',(16.5309313071793,17.9041632904916,-20.9650495608815));
#45110=CARTESIAN_POINT('Ctrl Pts',(16.4886879176911,17.9812952984404,-20.9694355572983));
#45111=CARTESIAN_POINT('Ctrl Pts',(16.446444528203,18.0584273063893,-20.973821553715));
#45112=CARTESIAN_POINT('Ctrl Pts',(16.4082454981438,18.137619241256,-20.9782075501317));
#45113=CARTESIAN_POINT('Ctrl Pts',(16.3742656129549,18.2184005729416,-20.9825935465485));
#45114=CARTESIAN_POINT('Ctrl Pts',(16.3382155097944,18.3041034917275,-20.9872467589536));
#45115=CARTESIAN_POINT('Ctrl Pts',(16.306798874077,18.3918657738651,-20.9918999713587));
#45116=CARTESIAN_POINT('Ctrl Pts',(16.2802296051744,18.4811980751755,-20.9965531837637));
#45117=CARTESIAN_POINT('Ctrl Pts',(16.2537435497692,18.5702505926029,-21.001191822562));
#45118=CARTESIAN_POINT('Ctrl Pts',(16.2320746945689,18.6608630689237,-21.0058304613603));
#45119=CARTESIAN_POINT('Ctrl Pts',(16.2153886002422,18.752527953949,-21.0104691001586));
#45120=CARTESIAN_POINT('Ctrl Pts',(16.1987928060345,18.8436967762135,-21.0150826360402));
#45121=CARTESIAN_POINT('Ctrl Pts',(16.1871261070645,18.9359063886952,-21.0196961719218));
#45122=CARTESIAN_POINT('Ctrl Pts',(16.1805035110245,19.0286385984106,-21.0243097078035));
#45123=CARTESIAN_POINT('Ctrl Pts',(16.1762064897689,19.0888071899736,-21.0273031655996));
#45124=CARTESIAN_POINT('Ctrl Pts',(16.1740320413884,19.1491954186321,-21.0302966233957));
#45125=CARTESIAN_POINT('Ctrl Pts',(16.174000351618,19.2096582534287,-21.0332900811918));
#45126=CARTESIAN_POINT('Ctrl Pts',(16.1775161339837,19.2096606725892,-21.0332901097715));
#45127=CARTESIAN_POINT('Ctrl Pts',(16.1799699186122,19.7238724897518,-21.0587831909243));
#45128=CARTESIAN_POINT('Ctrl Pts',(16.5801691862074,21.0966582496844,-21.1266682076376));
#45129=CARTESIAN_POINT('Ctrl Pts',(18.4990491868353,22.0730068113866,-21.2211093026498));
#45130=CARTESIAN_POINT('Ctrl Pts',(19.864965440735,21.5621389766016,-21.2900573165092));
#45131=CARTESIAN_POINT('Ctrl Pts',(20.291690728718,21.2386977908338,-21.3166133948081));
#45132=CARTESIAN_POINT('',(16.1715627854608,19.2128544306465,-20.9667098902285));
#45133=CARTESIAN_POINT('Ctrl Pts',(16.1715627854608,19.2128544306465,-20.9667098902285));
#45134=CARTESIAN_POINT('Ctrl Pts',(16.1706209869532,19.3284704702211,-20.9724759609646));
#45135=CARTESIAN_POINT('Ctrl Pts',(16.2303035804914,20.2931122226394,-21.0206339672611));
#45136=CARTESIAN_POINT('Ctrl Pts',(17.4553333859632,21.9547543997083,-21.1111839091181));
#45137=CARTESIAN_POINT('Ctrl Pts',(19.4740835948961,21.8268017090075,-21.1999086075618));
#45138=CARTESIAN_POINT('Ctrl Pts',(20.2333094880972,21.2922910093709,-21.246241370445));
#45139=CARTESIAN_POINT('Ctrl Pts',(20.2955779010576,21.2437559712559,-21.2501821977678));
#45140=CARTESIAN_POINT('Ctrl Pts',(20.2940726068359,21.241845339799,-20.4499991791617));
#45141=CARTESIAN_POINT('Ctrl Pts',(20.429454357434,21.1400081300327,-20.4584344113448));
#45142=CARTESIAN_POINT('Ctrl Pts',(21.1817798668074,20.4464549008743,-20.5092615790883));
#45143=CARTESIAN_POINT('Ctrl Pts',(21.642413960578,18.3717008291089,-20.6024806823923));
#45144=CARTESIAN_POINT('Ctrl Pts',(19.6025526335179,16.3111911491892,-20.7296564890738));
#45145=CARTESIAN_POINT('Ctrl Pts',(16.8944629772976,16.8838679918332,-20.8510662250192));
#45146=CARTESIAN_POINT('Ctrl Pts',(16.1775450542205,18.4784656881504,-20.9300840254041));
#45147=CARTESIAN_POINT('Ctrl Pts',(16.1715627854608,19.2128544306465,-20.9667098902285));
#45148=CARTESIAN_POINT('Origin',(18.734,19.211,1.76670989022852));
#45149=CARTESIAN_POINT('',(20.2935358855687,21.2411349269503,-19.6501081158318));
#45150=CARTESIAN_POINT('',(20.2935358855687,21.2411349269503,-19.7167245524671));
#45151=CARTESIAN_POINT('',(20.2935358855687,21.2411349269503,1.76670989022852));
#45152=CARTESIAN_POINT('',(16.1740004726297,19.2094444088938,-20.2332901098006));
#45153=CARTESIAN_POINT('Ctrl Pts',(20.2935358855687,21.2411349269503,-19.7167245524671));
#45154=CARTESIAN_POINT('Ctrl Pts',(20.3599060616565,21.1901498077021,-19.7209062209711));
#45155=CARTESIAN_POINT('Ctrl Pts',(20.423885153381,21.1358206778254,-19.7250878894751));
#45156=CARTESIAN_POINT('Ctrl Pts',(20.4851178678972,21.0784009244753,-19.7292695579791));
#45157=CARTESIAN_POINT('Ctrl Pts',(20.5462729398852,21.0210539788531,-19.7334459241653));
#45158=CARTESIAN_POINT('Ctrl Pts',(20.6046882194149,20.9606245074412,-19.7376222903514));
#45159=CARTESIAN_POINT('Ctrl Pts',(20.6600404272569,20.8974069119201,-19.7417986565376));
#45160=CARTESIAN_POINT('Ctrl Pts',(20.715340321286,20.8342490638527,-19.7459710756067));
#45161=CARTESIAN_POINT('Ctrl Pts',(20.7675825950387,20.7683086732424,-19.7501434946759));
#45162=CARTESIAN_POINT('Ctrl Pts',(20.8164808480404,20.6999168941029,-19.7543159137451));
#45163=CARTESIAN_POINT('Ctrl Pts',(20.8653546227575,20.6315593516349,-19.7584862441167));
#45164=CARTESIAN_POINT('Ctrl Pts',(20.9108874334552,20.5607532307721,-19.7626565744883));
#45165=CARTESIAN_POINT('Ctrl Pts',(20.9528339565094,20.4878617283954,-19.76682690486));
#45166=CARTESIAN_POINT('Ctrl Pts',(20.9947720643174,20.4149848493985,-19.7709963985864));
#45167=CARTESIAN_POINT('Ctrl Pts',(21.0331250845316,20.3400238186815,-19.7751658923128));
#45168=CARTESIAN_POINT('Ctrl Pts',(21.0676924581133,20.2633685243036,-19.7793353860393));
#45169=CARTESIAN_POINT('Ctrl Pts',(21.1022632661089,20.1867056139,-19.7835052940224));
#45170=CARTESIAN_POINT('Ctrl Pts',(21.1330474927277,20.1083485254935,-19.7876752020056));
#45171=CARTESIAN_POINT('Ctrl Pts',(21.1598923165065,20.0287080583649,-19.7918451099887));
#45172=CARTESIAN_POINT('Ctrl Pts',(21.1867656112298,19.948983126561,-19.7960194404714));
#45173=CARTESIAN_POINT('Ctrl Pts',(21.2096910141566,19.8679725352515,-19.800193770954));
#45174=CARTESIAN_POINT('Ctrl Pts',(21.2285654629023,19.7861027310794,-19.8043681014367));
#45175=CARTESIAN_POINT('Ctrl Pts',(21.2474505163374,19.7041869280093,-19.8085447772847));
#45176=CARTESIAN_POINT('Ctrl Pts',(21.2622800027704,19.6214114038201,-19.8127214531326));
#45177=CARTESIAN_POINT('Ctrl Pts',(21.2730023683084,19.5382109009864,-19.8168981289806));
#45178=CARTESIAN_POINT('Ctrl Pts',(21.2837431247208,19.4548676936352,-19.8210819686136));
#45179=CARTESIAN_POINT('Ctrl Pts',(21.2903626558656,19.3710985107369,-19.8252658082466));
#45180=CARTESIAN_POINT('Ctrl Pts',(21.2928614750997,19.2873410194495,-19.8294496478795));
#45181=CARTESIAN_POINT('Ctrl Pts',(21.2945659689719,19.230208383083,-19.8323035273916));
#45182=CARTESIAN_POINT('Ctrl Pts',(21.2943542420741,19.173081197621,-19.8351574069036));
#45183=CARTESIAN_POINT('Ctrl Pts',(21.2922402934572,19.1160968866051,-19.8380112864157));
#45184=CARTESIAN_POINT('Ctrl Pts',(21.2891406189063,19.0325410152651,-19.8421959187307));
#45185=CARTESIAN_POINT('Ctrl Pts',(21.2819372856915,18.9489816686976,-19.8463805510458));
#45186=CARTESIAN_POINT('Ctrl Pts',(21.2706266468752,18.8658547344046,-19.8505651833609));
#45187=CARTESIAN_POINT('Ctrl Pts',(21.2593321073605,18.7828461210669,-19.8547438593671));
#45188=CARTESIAN_POINT('Ctrl Pts',(21.2439419362161,18.70026914939,-19.8589225353733));
#45189=CARTESIAN_POINT('Ctrl Pts',(21.2245044655678,18.6185580138218,-19.8631012113796));
#45190=CARTESIAN_POINT('Ctrl Pts',(21.2047185799734,18.5353822133593,-19.8673547897845));
#45191=CARTESIAN_POINT('Ctrl Pts',(21.1807388847065,18.4531040774616,-19.8716083681894));
#45192=CARTESIAN_POINT('Ctrl Pts',(21.1526714444899,18.3721743663851,-19.8758619465942));
#45193=CARTESIAN_POINT('Ctrl Pts',(21.1251481633401,18.2928136846083,-19.8800330585099));
#45194=CARTESIAN_POINT('Ctrl Pts',(21.0936943831903,18.2147500635837,-19.8842041704256));
#45195=CARTESIAN_POINT('Ctrl Pts',(21.0584608475173,18.1383948683887,-19.8883752823413));
#45196=CARTESIAN_POINT('Ctrl Pts',(21.0232391347176,18.0620652947434,-19.8925449946096));
#45197=CARTESIAN_POINT('Ctrl Pts',(20.9842403778953,17.9874434257541,-19.8967147068778));
#45198=CARTESIAN_POINT('Ctrl Pts',(20.9416632153501,17.9149200921278,-19.9008844191461));
#45199=CARTESIAN_POINT('Ctrl Pts',(20.8990875677533,17.8423993389718,-19.9050539830508));
#45200=CARTESIAN_POINT('Ctrl Pts',(20.8529340012278,17.7719773690056,-19.9092235469555));
#45201=CARTESIAN_POINT('Ctrl Pts',(20.8034461281343,17.7040186720632,-19.9133931108602));
#45202=CARTESIAN_POINT('Ctrl Pts',(20.7522182683685,17.6336705568746,-19.9177092760466));
#45203=CARTESIAN_POINT('Ctrl Pts',(20.697417574011,17.5659625868841,-19.922025441233));
#45204=CARTESIAN_POINT('Ctrl Pts',(20.6393606094928,17.5012629009719,-19.9263416064194));
#45205=CARTESIAN_POINT('Ctrl Pts',(20.5831949030629,17.4386708658007,-19.9305171686242));
#45206=CARTESIAN_POINT('Ctrl Pts',(20.523982185993,17.3788944303194,-19.9346927308289));
#45207=CARTESIAN_POINT('Ctrl Pts',(20.4620462260796,17.3222289073231,-19.9388682930336));
#45208=CARTESIAN_POINT('Ctrl Pts',(20.3969819279172,17.2627012518396,-19.9432547597108));
#45209=CARTESIAN_POINT('Ctrl Pts',(20.3289124964447,17.206607414148,-19.9476412263881));
#45210=CARTESIAN_POINT('Ctrl Pts',(20.2582501417826,17.1542400467542,-19.9520276930653));
#45211=CARTESIAN_POINT('Ctrl Pts',(20.1875877871204,17.1018726793603,-19.9564141597426));
#45212=CARTESIAN_POINT('Ctrl Pts',(20.1143330347148,17.0532320398492,-19.9608006264198));
#45213=CARTESIAN_POINT('Ctrl Pts',(20.0389283877504,17.0085554711087,-19.965187093097));
#45214=CARTESIAN_POINT('Ctrl Pts',(19.9669932812562,16.9659345735974,-19.9693717283982));
#45215=CARTESIAN_POINT('Ctrl Pts',(19.8928340180633,16.9267623273783,-19.9735563636994));
#45216=CARTESIAN_POINT('Ctrl Pts',(19.8168151370682,16.8912777366814,-19.9777409990006));
#45217=CARTESIAN_POINT('Ctrl Pts',(19.7409044598177,16.8558436540364,-19.9819196779762));
#45218=CARTESIAN_POINT('Ctrl Pts',(19.6631398357153,16.8240869937955,-19.9860983569517));
#45219=CARTESIAN_POINT('Ctrl Pts',(19.5839125153273,16.796202137592,-19.9902770359273));
#45220=CARTESIAN_POINT('Ctrl Pts',(19.5032651236343,16.7678174729394,-19.9945306135878));
#45221=CARTESIAN_POINT('Ctrl Pts',(19.4211024978258,16.7434450253959,-19.9987841912482));
#45222=CARTESIAN_POINT('Ctrl Pts',(19.337861066102,16.7232395989874,-20.0030377689087));
#45223=CARTESIAN_POINT('Ctrl Pts',(19.2562334111056,16.7034258891344,-20.0072088837319));
#45224=CARTESIAN_POINT('Ctrl Pts',(19.1735688735385,16.6876191861435,-20.0113799985551));
#45225=CARTESIAN_POINT('Ctrl Pts',(19.0902949413653,16.6759154028401,-20.0155511133783));
#45226=CARTESIAN_POINT('Ctrl Pts',(19.0070489529371,16.6642155469066,-20.019720828525));
#45227=CARTESIAN_POINT('Ctrl Pts',(18.9231944312015,16.6566159403015,-20.0238905436717));
#45228=CARTESIAN_POINT('Ctrl Pts',(18.8391675225352,16.6531611090212,-20.0280602588184));
#45229=CARTESIAN_POINT('Ctrl Pts',(18.7551436043077,16.649706400695,-20.0322298255688));
#45230=CARTESIAN_POINT('Ctrl Pts',(18.6709477710271,16.6503961924556,-20.0363993923192));
#45231=CARTESIAN_POINT('Ctrl Pts',(18.5870183641888,16.6552229364175,-20.0405689590696));
#45232=CARTESIAN_POINT('Ctrl Pts',(18.500138140141,16.6602193806036,-20.0448851207954));
#45233=CARTESIAN_POINT('Ctrl Pts',(18.4135439525353,16.6696490660532,-20.0492012825211));
#45234=CARTESIAN_POINT('Ctrl Pts',(18.3277166966719,16.6834450792442,-20.0535174442468));
#45235=CARTESIAN_POINT('Ctrl Pts',(18.2446852202539,16.696791694284,-20.0576930091876));
#45236=CARTESIAN_POINT('Ctrl Pts',(18.1623719289201,16.7142243989078,-20.0618685741284));
#45237=CARTESIAN_POINT('Ctrl Pts',(18.0812003839193,16.7356308030427,-20.0660441390692));
#45238=CARTESIAN_POINT('Ctrl Pts',(17.9959291092702,16.7581183800159,-20.0704305991874));
#45239=CARTESIAN_POINT('Ctrl Pts',(17.9119185059183,16.7849914459601,-20.0748170593056));
#45240=CARTESIAN_POINT('Ctrl Pts',(17.8296377675515,16.8160618061167,-20.0792035194238));
#45241=CARTESIAN_POINT('Ctrl Pts',(17.7473570291847,16.8471321662734,-20.0835899795421));
#45242=CARTESIAN_POINT('Ctrl Pts',(17.6668066567997,16.8823995182561,-20.0879764396603));
#45243=CARTESIAN_POINT('Ctrl Pts',(17.5884257348687,16.9216202580024,-20.0923628997785));
#45244=CARTESIAN_POINT('Ctrl Pts',(17.5136510990685,16.9590364615644,-20.0965475399908));
#45245=CARTESIAN_POINT('Ctrl Pts',(17.44057234666,17.0001895266255,-20.1007321802031));
#45246=CARTESIAN_POINT('Ctrl Pts',(17.369587760884,17.0449023009683,-20.1049168204155));
#45247=CARTESIAN_POINT('Ctrl Pts',(17.2987042121717,17.0895514326572,-20.1090955043522));
#45248=CARTESIAN_POINT('Ctrl Pts',(17.2299092952701,17.1377499663397,-20.1132741882888));
#45249=CARTESIAN_POINT('Ctrl Pts',(17.1635782312953,17.1892741361949,-20.1174528722255));
#45250=CARTESIAN_POINT('Ctrl Pts',(17.0960583483994,17.241721748316,-20.1217064486519));
#45251=CARTESIAN_POINT('Ctrl Pts',(17.0310919386145,17.2976151655664,-20.1259600250784));
#45252=CARTESIAN_POINT('Ctrl Pts',(16.969045396673,17.3566712135668,-20.1302136015048));
#45253=CARTESIAN_POINT('Ctrl Pts',(16.9082016412034,17.4145824465075,-20.1343847213749));
#45254=CARTESIAN_POINT('Ctrl Pts',(16.8501659076493,17.4755344558904,-20.138555841245));
#45255=CARTESIAN_POINT('Ctrl Pts',(16.7952502349704,17.5392197068402,-20.142726961115));
#45256=CARTESIAN_POINT('Ctrl Pts',(16.7403529897255,17.6028835876472,-20.1468966813293));
#45257=CARTESIAN_POINT('Ctrl Pts',(16.6885740262376,17.6692785404175,-20.1510664015437));
#45258=CARTESIAN_POINT('Ctrl Pts',(16.6401868618722,17.7380619352452,-20.155236121758));
#45259=CARTESIAN_POINT('Ctrl Pts',(16.5918014193961,17.8068428823705,-20.1594056935901));
#45260=CARTESIAN_POINT('Ctrl Pts',(16.5468078000507,17.8780117258147,-20.1635752654222));
#45261=CARTESIAN_POINT('Ctrl Pts',(16.5054369234628,17.9511958033507,-20.1677448372542));
#45262=CARTESIAN_POINT('Ctrl Pts',(16.462611627541,18.0269527134222,-20.1720609930214));
#45263=CARTESIAN_POINT('Ctrl Pts',(16.4236688015505,18.104868733296,-20.1763771487885));
#45264=CARTESIAN_POINT('Ctrl Pts',(16.3888124800775,18.1845032896303,-20.1806933045556));
#45265=CARTESIAN_POINT('Ctrl Pts',(16.3550914981959,18.2615439903646,-20.1848688745605));
#45266=CARTESIAN_POINT('Ctrl Pts',(16.3251950198591,18.3401925369042,-20.1890444445653));
#45267=CARTESIAN_POINT('Ctrl Pts',(16.2992578088608,18.4200319458494,-20.1932200145702));
#45268=CARTESIAN_POINT('Ctrl Pts',(16.2720106919424,18.5039034812422,-20.1976064632185));
#45269=CARTESIAN_POINT('Ctrl Pts',(16.2491334314256,18.5890887659587,-20.2019929118667));
#45270=CARTESIAN_POINT('Ctrl Pts',(16.2307217504257,18.6750914208485,-20.206379360515));
#45271=CARTESIAN_POINT('Ctrl Pts',(16.2123100694257,18.7610940757384,-20.2107658091633));
#45272=CARTESIAN_POINT('Ctrl Pts',(16.198363984864,18.8479135158795,-20.2151522578116));
#45273=CARTESIAN_POINT('Ctrl Pts',(16.1889163328193,18.9350486871749,-20.2195387064599));
#45274=CARTESIAN_POINT('Ctrl Pts',(16.1790436177041,19.0261041916152,-20.2241225075637));
#45275=CARTESIAN_POINT('Ctrl Pts',(16.1740562221026,19.1176988529932,-20.2287063086676));
#45276=CARTESIAN_POINT('Ctrl Pts',(16.17400047263,19.2094444083109,-20.2332901097715));
#45277=CARTESIAN_POINT('Ctrl Pts',(16.1740004726297,19.2094444088938,-20.2332901098006));
#45278=CARTESIAN_POINT('Ctrl Pts',(16.1739502760983,19.2920516545602,-20.2374173417146));
#45279=CARTESIAN_POINT('Ctrl Pts',(16.1779027082651,19.3748187791154,-20.2415445736285));
#45280=CARTESIAN_POINT('Ctrl Pts',(16.1858778001794,19.4573194161684,-20.2456718055424));
#45281=CARTESIAN_POINT('Ctrl Pts',(16.1940130436991,19.5414767876655,-20.249881918359));
#45282=CARTESIAN_POINT('Ctrl Pts',(16.2063343518328,19.6253563595504,-20.2540920311757));
#45283=CARTESIAN_POINT('Ctrl Pts',(16.222807033423,19.7085036528651,-20.2583021439923));
#45284=CARTESIAN_POINT('Ctrl Pts',(16.2389199317254,19.7898349087365,-20.2624203028533));
#45285=CARTESIAN_POINT('Ctrl Pts',(16.2590046102348,19.8704650577792,-20.2665384617144));
#45286=CARTESIAN_POINT('Ctrl Pts',(16.2829763020121,19.9499741753957,-20.2706566205754));
#45287=CARTESIAN_POINT('Ctrl Pts',(16.3069370246241,20.0294469105714,-20.2747728950152));
#45288=CARTESIAN_POINT('Ctrl Pts',(16.334781094809,20.1077991798405,-20.278889169455));
#45289=CARTESIAN_POINT('Ctrl Pts',(16.3663732871992,20.1846240284793,-20.2830054438948));
#45290=CARTESIAN_POINT('Ctrl Pts',(16.3979610861523,20.2614381933028,-20.2871211458959));
#45291=CARTESIAN_POINT('Ctrl Pts',(16.4332957916267,20.3367249220046,-20.291236847897));
#45292=CARTESIAN_POINT('Ctrl Pts',(16.4721937795329,20.4100965853743,-20.2953525498981));
#45293=CARTESIAN_POINT('Ctrl Pts',(16.5126461135564,20.4864001474415,-20.2996327135017));
#45294=CARTESIAN_POINT('Ctrl Pts',(16.5569522565608,20.5606318773211,-20.3039128771053));
#45295=CARTESIAN_POINT('Ctrl Pts',(16.6048536565745,20.6323851864564,-20.3081930407089));
#45296=CARTESIAN_POINT('Ctrl Pts',(16.6509736168395,20.7014700099742,-20.3123140262181));
#45297=CARTESIAN_POINT('Ctrl Pts',(16.700425807859,20.7682571429841,-20.3164350117273));
#45298=CARTESIAN_POINT('Ctrl Pts',(16.7529371454851,20.832416037438,-20.3205559972365));
#45299=CARTESIAN_POINT('Ctrl Pts',(16.8054841275711,20.8966184826611,-20.3246797800521));
#45300=CARTESIAN_POINT('Ctrl Pts',(16.8610940675905,20.9581887928557,-20.3288035628677));
#45301=CARTESIAN_POINT('Ctrl Pts',(16.9194565998598,21.0168328408266,-20.3329273456833));
#45302=CARTESIAN_POINT('Ctrl Pts',(16.9779086865543,21.0755668751946,-20.3370574562401));
#45303=CARTESIAN_POINT('Ctrl Pts',(17.0391214360201,21.1313653808553,-20.3411875667969));
#45304=CARTESIAN_POINT('Ctrl Pts',(17.102751683912,21.1839746402982,-20.3453176773537));
#45305=CARTESIAN_POINT('Ctrl Pts',(17.1099251002331,21.189905595038,-20.3457832892829));
#45306=CARTESIAN_POINT('Ctrl Pts',(17.1171292123955,21.1957960624817,-20.3462489012121));
#45307=CARTESIAN_POINT('Ctrl Pts',(17.1243635072226,21.201645714616,-20.3467145131413));
#45308=CARTESIAN_POINT('Ctrl Pts',(17.189381078246,21.254218934563,-20.3508991582794));
#45309=CARTESIAN_POINT('Ctrl Pts',(17.2570980356913,21.3037012786361,-20.3550838034176));
#45310=CARTESIAN_POINT('Ctrl Pts',(17.3271882231611,21.349803549779,-20.3592684485557));
#45311=CARTESIAN_POINT('Ctrl Pts',(17.3971786443956,21.3958401990397,-20.3634471372781));
#45312=CARTESIAN_POINT('Ctrl Pts',(17.469535204727,21.4385060812658,-20.3676258260006));
#45313=CARTESIAN_POINT('Ctrl Pts',(17.5438988654553,21.477552291379,-20.371804514723));
#45314=CARTESIAN_POINT('Ctrl Pts',(17.619595201075,21.5172982505808,-20.3760580899355));
#45315=CARTESIAN_POINT('Ctrl Pts',(17.6973709112596,21.5532932167484,-20.380311665148));
#45316=CARTESIAN_POINT('Ctrl Pts',(17.7768165359119,21.5853209168257,-20.3845652403605));
#45317=CARTESIAN_POINT('Ctrl Pts',(17.8547221935262,21.6167277947667,-20.3887363646432));
#45318=CARTESIAN_POINT('Ctrl Pts',(17.9342331579704,21.6443196566907,-20.3929074889259));
#45319=CARTESIAN_POINT('Ctrl Pts',(18.0149402978303,21.6679397926517,-20.3970786132086));
#45320=CARTESIAN_POINT('Ctrl Pts',(18.0956203528785,21.6915520018428,-20.401248337688));
#45321=CARTESIAN_POINT('Ctrl Pts',(18.1774953449549,21.711195003098,-20.4054180621675));
#45322=CARTESIAN_POINT('Ctrl Pts',(18.2601401458989,21.7267616816128,-20.409587786647));
#45323=CARTESIAN_POINT('Ctrl Pts',(18.3427820028615,21.7423278056098,-20.4137573625921));
#45324=CARTESIAN_POINT('Ctrl Pts',(18.4261931619307,21.7538178112606,-20.4179269385372));
#45325=CARTESIAN_POINT('Ctrl Pts',(18.5099387942267,21.7611757931694,-20.4220965144823));
#45326=CARTESIAN_POINT('Ctrl Pts',(18.596628364788,21.7687924326811,-20.4264126649273));
#45327=CARTESIAN_POINT('Ctrl Pts',(18.6836758371978,21.7719810786796,-20.4307288153724));
#45328=CARTESIAN_POINT('Ctrl Pts',(18.7705956997404,21.7707384152996,-20.4350449658174));
#45329=CARTESIAN_POINT('Ctrl Pts',(18.854684587927,21.7695362253863,-20.4392205395189));
#45330=CARTESIAN_POINT('Ctrl Pts',(18.9386535840458,21.7641870268945,-20.4433961132204));
#45331=CARTESIAN_POINT('Ctrl Pts',(19.0220673263579,21.7547407917249,-20.4475716869219));
#45332=CARTESIAN_POINT('Ctrl Pts',(19.1096934355566,21.7448175247481,-20.4519581257387));
#45333=CARTESIAN_POINT('Ctrl Pts',(19.1967061584007,21.7303726255243,-20.4563445645555));
#45334=CARTESIAN_POINT('Ctrl Pts',(19.2826140302888,21.7115244741394,-20.4607310033724));
#45335=CARTESIAN_POINT('Ctrl Pts',(19.3685219021768,21.6926763227546,-20.4651174421892));
#45336=CARTESIAN_POINT('Ctrl Pts',(19.4533243836774,21.6694251459735,-20.469503881006));
#45337=CARTESIAN_POINT('Ctrl Pts',(19.5365517912822,21.6419485026034,-20.4738903198228));
#45338=CARTESIAN_POINT('Ctrl Pts',(19.6159350028657,21.6157409796609,-20.4780741531382));
#45339=CARTESIAN_POINT('Ctrl Pts',(19.6941808258861,21.5855921973816,-20.4822579864537));
#45340=CARTESIAN_POINT('Ctrl Pts',(19.7708697961334,21.5516197952393,-20.4864418197691));
#45341=CARTESIAN_POINT('Ctrl Pts',(19.8474630714802,21.5176897849252,-20.4906204323662));
#45342=CARTESIAN_POINT('Ctrl Pts',(19.9225029325766,21.4799458077275,-20.4947990449632));
#45343=CARTESIAN_POINT('Ctrl Pts',(19.9955857715563,21.4385550141369,-20.4989776575603));
#45344=CARTESIAN_POINT('Ctrl Pts',(20.0685856279724,21.3972112180934,-20.5031515255144));
#45345=CARTESIAN_POINT('Ctrl Pts',(20.1396324803964,21.3522290606009,-20.5073253934684));
#45346=CARTESIAN_POINT('Ctrl Pts',(20.2083448689615,21.3038227845106,-20.5114992614224));
#45347=CARTESIAN_POINT('Ctrl Pts',(20.237161086268,21.2835224311109,-20.5132496748265));
#45348=CARTESIAN_POINT('Ctrl Pts',(20.2655670177483,21.2626204215672,-20.5150000882306));
#45349=CARTESIAN_POINT('Ctrl Pts',(20.2935358855687,21.2411349269503,-20.5167505016347));
#45350=CARTESIAN_POINT('',(16.1742339579337,19.2120076676078,-20.1667099326005));
#45351=CARTESIAN_POINT('Ctrl Pts',(16.1778405256925,19.2120194393453,-20.1667105863375));
#45352=CARTESIAN_POINT('Ctrl Pts',(16.17655676437,19.5768333952661,-20.1847914783409));
#45353=CARTESIAN_POINT('Ctrl Pts',(16.4202751262482,20.7953392457516,-20.245264305905));
#45354=CARTESIAN_POINT('Ctrl Pts',(18.140176361079,22.0902446734967,-20.3396938368464));
#45355=CARTESIAN_POINT('Ctrl Pts',(19.7490825166988,21.6517991916634,-20.4160424757843));
#45356=CARTESIAN_POINT('Ctrl Pts',(20.2940726068359,21.241845339799,-20.4499991791617));
#45357=CARTESIAN_POINT('Ctrl Pts',(20.2935358855687,21.2411349269503,-19.6501081158318));
#45358=CARTESIAN_POINT('Ctrl Pts',(20.3602263184528,21.1899037886027,-19.6542777829748));
#45359=CARTESIAN_POINT('Ctrl Pts',(20.424386701975,21.135385296707,-19.6584474501178));
#45360=CARTESIAN_POINT('Ctrl Pts',(20.485686563464,21.0778674787943,-19.6626171172608));
#45361=CARTESIAN_POINT('Ctrl Pts',(20.5470483458354,21.0202915603581,-19.6667909963133));
#45362=CARTESIAN_POINT('Ctrl Pts',(20.6055434979418,20.959710579369,-19.6709648753658));
#45363=CARTESIAN_POINT('Ctrl Pts',(20.6608777148422,20.8964501689592,-19.6751387544183));
#45364=CARTESIAN_POINT('Ctrl Pts',(20.7162388970532,20.833158930669,-19.6793146674735));
#45365=CARTESIAN_POINT('Ctrl Pts',(20.7684357897789,20.7671860230858,-19.6834905805287));
#45366=CARTESIAN_POINT('Ctrl Pts',(20.8172153439539,20.6988890518836,-19.6876664935839));
#45367=CARTESIAN_POINT('Ctrl Pts',(20.8660828483171,20.6304689403294,-19.6918499358661));
#45368=CARTESIAN_POINT('Ctrl Pts',(20.9115204527854,20.5597167799375,-19.6960333781483));
#45369=CARTESIAN_POINT('Ctrl Pts',(20.9533193396094,20.4870178951862,-19.7002168204305));
#45370=CARTESIAN_POINT('Ctrl Pts',(20.9933959851083,20.417314425699,-19.7042278921611));
#45371=CARTESIAN_POINT('Ctrl Pts',(21.0301277549889,20.3458218456753,-19.7082389638917));
#45372=CARTESIAN_POINT('Ctrl Pts',(21.0633723464503,20.2728966388461,-19.7122500356223));
#45373=CARTESIAN_POINT('Ctrl Pts',(21.0980554588848,20.1968158979922,-19.7164346697447));
#45374=CARTESIAN_POINT('Ctrl Pts',(21.1290718315298,20.1188925846168,-19.7206193038671));
#45375=CARTESIAN_POINT('Ctrl Pts',(21.1562228177911,20.0395147077584,-19.7248039379896));
#45376=CARTESIAN_POINT('Ctrl Pts',(21.1833351579832,19.9602498154855,-19.7289826158031));
#45377=CARTESIAN_POINT('Ctrl Pts',(21.2065928926838,19.8795349037292,-19.7331612936167));
#45378=CARTESIAN_POINT('Ctrl Pts',(21.2258445987322,19.7977797676888,-19.7373399714302));
#45379=CARTESIAN_POINT('Ctrl Pts',(21.2454413793552,19.7145592228832,-19.7415935493833));
#45380=CARTESIAN_POINT('Ctrl Pts',(21.2608869019344,19.6302612334801,-19.7458471273363));
#45381=CARTESIAN_POINT('Ctrl Pts',(21.2720739254944,19.5453362808993,-19.7501007052894));
#45382=CARTESIAN_POINT('Ctrl Pts',(21.283044065894,19.4620577709144,-19.7542718189995));
#45383=CARTESIAN_POINT('Ctrl Pts',(21.2899192902207,19.3781768678187,-19.7584429327095));
#45384=CARTESIAN_POINT('Ctrl Pts',(21.2926499549084,19.2941288653065,-19.7626140464196));
#45385=CARTESIAN_POINT('Ctrl Pts',(21.2953797032962,19.2101090658848,-19.7667837604736));
#45386=CARTESIAN_POINT('Ctrl Pts',(21.2939676391619,19.1259227378137,-19.7709534745275));
#45387=CARTESIAN_POINT('Ctrl Pts',(21.2884161370472,19.0420082877982,-19.7751231885815));
#45388=CARTESIAN_POINT('Ctrl Pts',(21.2828648324763,18.958096823782,-19.779292754261));
#45389=CARTESIAN_POINT('Ctrl Pts',(21.2731744140079,18.8744576775594,-19.7834623199405));
#45390=CARTESIAN_POINT('Ctrl Pts',(21.2593992661634,18.7915258691394,-19.78763188562));
#45391=CARTESIAN_POINT('Ctrl Pts',(21.2451397991587,18.7056782688699,-19.791948048677));
#45392=CARTESIAN_POINT('Ctrl Pts',(21.2265031054902,18.620589192361,-19.796264211734));
#45393=CARTESIAN_POINT('Ctrl Pts',(21.2036071461028,18.5367296210585,-19.800580374791));
#45394=CARTESIAN_POINT('Ctrl Pts',(21.1814570231814,18.4556017774482,-19.8047559387253));
#45395=CARTESIAN_POINT('Ctrl Pts',(21.1553210566047,18.3756249996565,-19.8089315026597));
#45396=CARTESIAN_POINT('Ctrl Pts',(21.1253562910671,18.2972083994838,-19.8131070665941));
#45397=CARTESIAN_POINT('Ctrl Pts',(21.09387807017,18.2148311468024,-19.8174935292124));
#45398=CARTESIAN_POINT('Ctrl Pts',(21.0581743347953,18.1341763575253,-19.8218799918307));
#45399=CARTESIAN_POINT('Ctrl Pts',(21.0184823804552,18.0556904079902,-19.8262664544489));
#45400=CARTESIAN_POINT('Ctrl Pts',(20.978790426115,17.9772044584551,-19.8306529170672));
#45401=CARTESIAN_POINT('Ctrl Pts',(20.9351106070445,17.9008878144474,-19.8350393796855));
#45402=CARTESIAN_POINT('Ctrl Pts',(20.8877320902706,17.827150989689,-19.8394258423038));
#45403=CARTESIAN_POINT('Ctrl Pts',(20.8425335350801,17.7568069145607,-19.8436104767382));
#45404=CARTESIAN_POINT('Ctrl Pts',(20.7938009308883,17.6885486380927,-19.8477951111726));
#45405=CARTESIAN_POINT('Ctrl Pts',(20.7417530082953,17.6227532126017,-19.851979745607));
#45406=CARTESIAN_POINT('Ctrl Pts',(20.6897791695079,17.5570514387929,-19.8561584237298));
#45407=CARTESIAN_POINT('Ctrl Pts',(20.6344996686009,17.4938059105141,-19.8603371018527));
#45408=CARTESIAN_POINT('Ctrl Pts',(20.5761771160359,17.4333657650817,-19.8645157799755));
#45409=CARTESIAN_POINT('Ctrl Pts',(20.5168091743242,17.3718422741975,-19.8687693578509));
#45410=CARTESIAN_POINT('Ctrl Pts',(20.4542882752167,17.3132261339225,-19.8730229357263));
#45411=CARTESIAN_POINT('Ctrl Pts',(20.388935154738,17.2578513539384,-19.8772765136017));
#45412=CARTESIAN_POINT('Ctrl Pts',(20.3248490313739,17.2035501215667,-19.8814476276122));
#45413=CARTESIAN_POINT('Ctrl Pts',(20.258039890023,17.1523660019974,-19.8856187416228));
#45414=CARTESIAN_POINT('Ctrl Pts',(20.1888468727061,17.1045763538696,-19.8897898556334));
#45415=CARTESIAN_POINT('Ctrl Pts',(20.1196770738139,17.0568027420471,-19.8939595699839));
#45416=CARTESIAN_POINT('Ctrl Pts',(20.0481253658473,17.0124216007145,-19.8981292843345));
#45417=CARTESIAN_POINT('Ctrl Pts',(19.974561664793,16.9716682345293,-19.9022989986851));
#45418=CARTESIAN_POINT('Ctrl Pts',(19.9010005814933,16.9309163185474,-19.9064685646569));
#45419=CARTESIAN_POINT('Ctrl Pts',(19.8254280502798,16.8937921432249,-19.9106381306288));
#45420=CARTESIAN_POINT('Ctrl Pts',(19.7482392914822,16.8604854479043,-19.9148076966006));
#45421=CARTESIAN_POINT('Ctrl Pts',(19.6683366724246,16.8260077308154,-19.9191238592993));
#45422=CARTESIAN_POINT('Ctrl Pts',(19.5867025423552,16.7956211424271,-19.923440021998));
#45423=CARTESIAN_POINT('Ctrl Pts',(19.5037967719895,16.7694814295536,-19.9277561846968));
#45424=CARTESIAN_POINT('Ctrl Pts',(19.4235916472118,16.7441932147113,-19.93193174891));
#45425=CARTESIAN_POINT('Ctrl Pts',(19.3421969248366,16.7228795141862,-19.9361073131233));
#45426=CARTESIAN_POINT('Ctrl Pts',(19.2600416084997,16.7056297227501,-19.9402828773365));
#45427=CARTESIAN_POINT('Ctrl Pts',(19.1737368242851,16.6875086857435,-19.944669339278));
#45428=CARTESIAN_POINT('Ctrl Pts',(19.0865931685398,16.6738729730806,-19.9490558012194));
#45429=CARTESIAN_POINT('Ctrl Pts',(18.9991144164059,16.6647646718707,-19.9534422631609));
#45430=CARTESIAN_POINT('Ctrl Pts',(18.9116356642721,16.6556563706608,-19.9578287251023));
#45431=CARTESIAN_POINT('Ctrl Pts',(18.8238223991415,16.6510754351692,-19.9622151870438));
#45432=CARTESIAN_POINT('Ctrl Pts',(18.7361763184546,16.6510009250709,-19.9666016489852));
#45433=CARTESIAN_POINT('Ctrl Pts',(18.6525629441496,16.6509298432758,-19.970786284297));
#45434=CARTESIAN_POINT('Ctrl Pts',(18.5687904831981,16.6549593424975,-19.9749709196088));
#45435=CARTESIAN_POINT('Ctrl Pts',(18.4852943718234,16.6631095960553,-19.9791555549207));
#45436=CARTESIAN_POINT('Ctrl Pts',(18.4019171067173,16.6712482487469,-19.9833342339276));
#45437=CARTESIAN_POINT('Ctrl Pts',(18.3188158638134,16.6834959609774,-19.9875129129346));
#45438=CARTESIAN_POINT('Ctrl Pts',(18.2364263585563,16.6998209001864,-19.9916915919416));
#45439=CARTESIAN_POINT('Ctrl Pts',(18.1525601036944,16.7164384476282,-19.9959451695968));
#45440=CARTESIAN_POINT('Ctrl Pts',(18.0694318349784,16.7372808264264,-20.000198747252));
#45441=CARTESIAN_POINT('Ctrl Pts',(17.9874960098034,16.7622591413911,-20.0044523249072));
#45442=CARTESIAN_POINT('Ctrl Pts',(17.9071486482815,16.7867532097475,-20.008623439812));
#45443=CARTESIAN_POINT('Ctrl Pts',(17.8279483681485,16.8152241408411,-20.0127945547168));
#45444=CARTESIAN_POINT('Ctrl Pts',(17.7503119553988,16.847536898763,-20.0169656696216));
#45445=CARTESIAN_POINT('Ctrl Pts',(17.6727015943022,16.8798388138249,-20.0211353848683));
#45446=CARTESIAN_POINT('Ctrl Pts',(17.5966544827469,16.9159798187962,-20.0253051001149));
#45447=CARTESIAN_POINT('Ctrl Pts',(17.5225687033403,16.955776238713,-20.0294748153615));
#45448=CARTESIAN_POINT('Ctrl Pts',(17.4484855602554,16.9955712424854,-20.03364438223));
#45449=CARTESIAN_POINT('Ctrl Pts',(17.3763640154128,17.0390211841318,-20.0378139490985));
#45450=CARTESIAN_POINT('Ctrl Pts',(17.3065775349575,17.0858964481014,-20.041983515967));
#45451=CARTESIAN_POINT('Ctrl Pts',(17.2343374823222,17.1344197654313,-20.0462996776086));
#45452=CARTESIAN_POINT('Ctrl Pts',(17.1646001863695,17.1866134577581,-20.0506158392503));
#45453=CARTESIAN_POINT('Ctrl Pts',(17.0977455244312,17.2421751496943,-20.0549320008919));
#45454=CARTESIAN_POINT('Ctrl Pts',(17.0330686155278,17.295926950746,-20.0591075659941));
#45455=CARTESIAN_POINT('Ctrl Pts',(16.9710897386954,17.3528303455358,-20.0632831310963));
#45456=CARTESIAN_POINT('Ctrl Pts',(16.9121162724547,17.4125729975043,-20.0674586961985));
#45457=CARTESIAN_POINT('Ctrl Pts',(16.8501642398155,17.4753330650506,-20.0718451561099));
#45458=CARTESIAN_POINT('Ctrl Pts',(16.7915295867849,17.5412263087853,-20.0762316160212));
#45459=CARTESIAN_POINT('Ctrl Pts',(16.7365203854446,17.6098519152073,-20.0806180759326));
#45460=CARTESIAN_POINT('Ctrl Pts',(16.6815111841043,17.6784775216292,-20.0850045358439));
#45461=CARTESIAN_POINT('Ctrl Pts',(16.6301277117768,17.7498349754449,-20.0893909957553));
#45462=CARTESIAN_POINT('Ctrl Pts',(16.5826239199814,17.8234910946867,-20.0937774556667));
#45463=CARTESIAN_POINT('Ctrl Pts',(16.5362791661082,17.8953500892742,-20.0980568909977));
#45464=CARTESIAN_POINT('Ctrl Pts',(16.4934601213733,17.96965463442,-20.1023363263287));
#45465=CARTESIAN_POINT('Ctrl Pts',(16.4544271375725,18.0460332344294,-20.1066157616597));
#45466=CARTESIAN_POINT('Ctrl Pts',(16.4154575008457,18.1222878787389,-20.1108882518464));
#45467=CARTESIAN_POINT('Ctrl Pts',(16.3802619050974,18.2006095046636,-20.1151607420331));
#45468=CARTESIAN_POINT('Ctrl Pts',(16.3490570392734,18.2805984339648,-20.1194332322197));
#45469=CARTESIAN_POINT('Ctrl Pts',(16.3179055659637,18.3604504996733,-20.1236984120403));
#45470=CARTESIAN_POINT('Ctrl Pts',(16.2907313869123,18.4419637898502,-20.1279635918609));
#45471=CARTESIAN_POINT('Ctrl Pts',(16.267704287416,18.5247161971242,-20.1322287716815));
#45472=CARTESIAN_POINT('Ctrl Pts',(16.2447004012398,18.6073851827702,-20.1364896518296));
#45473=CARTESIAN_POINT('Ctrl Pts',(16.2258353998839,18.6912903879612,-20.1407505319778));
#45474=CARTESIAN_POINT('Ctrl Pts',(16.2112300227061,18.7759923659696,-20.1450114121259));
#45475=CARTESIAN_POINT('Ctrl Pts',(16.1966372355967,18.8606213295208,-20.1492686193273));
#45476=CARTESIAN_POINT('Ctrl Pts',(16.1862968405217,18.946045274463,-20.1535258265288));
#45477=CARTESIAN_POINT('Ctrl Pts',(16.1802787590545,19.0318134392765,-20.1577830337302));
#45478=CARTESIAN_POINT('Ctrl Pts',(16.1760723590125,19.0917619816882,-20.160758652563));
#45479=CARTESIAN_POINT('Ctrl Pts',(16.1739765481557,19.1518784238251,-20.1637342713957));
#45480=CARTESIAN_POINT('Ctrl Pts',(16.1740001980189,19.2120069046219,-20.1667098902285));
#45481=CARTESIAN_POINT('Origin',(18.734,19.211,1.76670989022852));
#45482=CARTESIAN_POINT('',(20.2935358855687,21.2411349269503,-18.8501886410431));
#45483=CARTESIAN_POINT('',(20.2933494018239,21.240883566784,-18.9165759007818));
#45484=CARTESIAN_POINT('',(20.2935358855687,21.2411349269503,1.76670989022852));
#45485=CARTESIAN_POINT('',(16.1740009418753,19.2131959965388,-19.4332901097715));
#45486=CARTESIAN_POINT('Ctrl Pts',(20.2933494018237,21.2408835667842,-18.9165759007818));
#45487=CARTESIAN_POINT('Ctrl Pts',(20.460481259703,21.1151428689567,-18.9269774804031));
#45488=CARTESIAN_POINT('Ctrl Pts',(21.2286611573496,20.3759974962177,-18.9797709955848));
#45489=CARTESIAN_POINT('Ctrl Pts',(21.6004478661678,18.2379803543616,-19.074956446327));
#45490=CARTESIAN_POINT('Ctrl Pts',(19.4673983208532,16.2740938868786,-19.2021322530084));
#45491=CARTESIAN_POINT('Ctrl Pts',(16.8320816456072,16.9602242617438,-19.3215765971066));
#45492=CARTESIAN_POINT('Ctrl Pts',(16.1790132394519,18.5174132428891,-19.3986290056444));
#45493=CARTESIAN_POINT('Ctrl Pts',(16.1726852608311,19.213184455598,-19.4332894786216));
#45494=CARTESIAN_POINT('Ctrl Pts',(16.1740009418753,19.2131959965388,-19.4332901097715));
#45495=CARTESIAN_POINT('Ctrl Pts',(16.1741094126172,19.3396465587508,-19.4395926510338));
#45496=CARTESIAN_POINT('Ctrl Pts',(16.1835900621655,19.4657089276735,-19.4458951922961));
#45497=CARTESIAN_POINT('Ctrl Pts',(16.2022529884087,19.5902849447293,-19.4521977335585));
#45498=CARTESIAN_POINT('Ctrl Pts',(16.2064836512067,19.6185248420538,-19.4536264444961));
#45499=CARTESIAN_POINT('Ctrl Pts',(16.2111860003675,19.6466884926971,-19.4550551554337));
#45500=CARTESIAN_POINT('Ctrl Pts',(16.2163575306344,19.6747632978648,-19.4564838663713));
#45501=CARTESIAN_POINT('Ctrl Pts',(16.2315047248246,19.7569932189491,-19.4606685004926));
#45502=CARTESIAN_POINT('Ctrl Pts',(16.2507129697403,19.838633291604,-19.4648531346138));
#45503=CARTESIAN_POINT('Ctrl Pts',(16.273922855402,19.9192516802849,-19.4690377687351));
#45504=CARTESIAN_POINT('Ctrl Pts',(16.2970997046635,19.9997553186653,-19.4732164465475));
#45505=CARTESIAN_POINT('Ctrl Pts',(16.3242667547551,20.0792397233557,-19.4773951243598));
#45506=CARTESIAN_POINT('Ctrl Pts',(16.3553134075107,20.1572822489679,-19.4815738021722));
#45507=CARTESIAN_POINT('Ctrl Pts',(16.3869165517625,20.2367236371946,-19.4858273801256));
#45508=CARTESIAN_POINT('Ctrl Pts',(16.4225396637635,20.31467047214,-19.4900809580789));
#45509=CARTESIAN_POINT('Ctrl Pts',(16.4620126245789,20.3906920640265,-19.4943345360323));
#45510=CARTESIAN_POINT('Ctrl Pts',(16.500720321909,20.4652398230115,-19.4985056497412));
#45511=CARTESIAN_POINT('Ctrl Pts',(16.543129704132,20.537935895187,-19.5026767634501));
#45512=CARTESIAN_POINT('Ctrl Pts',(16.5890321382678,20.6083950308112,-19.506847877159));
#45513=CARTESIAN_POINT('Ctrl Pts',(16.6349191694141,20.678830523216,-19.5110175912119));
#45514=CARTESIAN_POINT('Ctrl Pts',(16.6842966737088,20.7470301846918,-19.5151873052647));
#45515=CARTESIAN_POINT('Ctrl Pts',(16.7369115952943,20.8126360085207,-19.5193570193175));
#45516=CARTESIAN_POINT('Ctrl Pts',(16.7895246446383,20.8782394978417,-19.5235265849959));
#45517=CARTESIAN_POINT('Ctrl Pts',(16.845374593747,20.9412489746849,-19.5276961506742));
#45518=CARTESIAN_POINT('Ctrl Pts',(16.9041676934323,21.0013389985813,-19.5318657163526));
#45519=CARTESIAN_POINT('Ctrl Pts',(16.9650278943555,21.0635417221558,-19.5361818794109));
#45520=CARTESIAN_POINT('Ctrl Pts',(17.0290416909492,21.1226154992726,-19.5404980424693));
#45521=CARTESIAN_POINT('Ctrl Pts',(17.0958426218354,21.1782418266103,-19.5448142055276));
#45522=CARTESIAN_POINT('Ctrl Pts',(17.1604675106422,21.2320561248729,-19.5489897694609));
#45523=CARTESIAN_POINT('Ctrl Pts',(17.2277003349656,21.2826438809482,-19.5531653333942));
#45524=CARTESIAN_POINT('Ctrl Pts',(17.2971780335787,21.3297596930302,-19.5573408973275));
#45525=CARTESIAN_POINT('Ctrl Pts',(17.3701649002202,21.3792552227006,-19.5617273599483));
#45526=CARTESIAN_POINT('Ctrl Pts',(17.4456288796132,21.4249185512742,-19.5661138225692));
#45527=CARTESIAN_POINT('Ctrl Pts',(17.5231197837688,21.466519696642,-19.5705002851901));
#45528=CARTESIAN_POINT('Ctrl Pts',(17.6006106879243,21.5081208420097,-19.574886747811));
#45529=CARTESIAN_POINT('Ctrl Pts',(17.6801279596808,21.54565962526,-19.5792732104319));
#45530=CARTESIAN_POINT('Ctrl Pts',(17.7611994326903,21.5789651720923,-19.5836596730527));
#45531=CARTESIAN_POINT('Ctrl Pts',(17.8385406770856,21.6107382772506,-19.587844307487));
#45532=CARTESIAN_POINT('Ctrl Pts',(17.9175841221713,21.6387774071546,-19.5920289419213));
#45533=CARTESIAN_POINT('Ctrl Pts',(17.9979345050497,21.6628987717978,-19.5962135763555));
#45534=CARTESIAN_POINT('Ctrl Pts',(18.0781705190567,21.6869858026501,-19.6003922544782));
#45535=CARTESIAN_POINT('Ctrl Pts',(18.1597093389463,21.7071660136985,-19.6045709326009));
#45536=CARTESIAN_POINT('Ctrl Pts',(18.2421357220941,21.723303630559,-19.6087496107235));
#45537=CARTESIAN_POINT('Ctrl Pts',(18.3260395379464,21.7397305024131,-19.613003188599));
#45538=CARTESIAN_POINT('Ctrl Pts',(18.4108626031778,21.751968244467,-19.6172567664744));
#45539=CARTESIAN_POINT('Ctrl Pts',(18.4961506937664,21.7599267756301,-19.6215103443499));
#45540=CARTESIAN_POINT('Ctrl Pts',(18.5797853091396,21.7677310152159,-19.6256814583602));
#45541=CARTESIAN_POINT('Ctrl Pts',(18.6638666007977,21.7714204401678,-19.6298525723706));
#45542=CARTESIAN_POINT('Ctrl Pts',(18.7479577055539,21.7709619494156,-19.634023686381));
#45543=CARTESIAN_POINT('Ctrl Pts',(18.8320205926795,21.7705036125146,-19.6381934007314));
#45544=CARTESIAN_POINT('Ctrl Pts',(18.9160928267202,21.7659001267025,-19.6423631150818));
#45545=CARTESIAN_POINT('Ctrl Pts',(18.9997364062976,21.7571704896507,-19.6465328294322));
#45546=CARTESIAN_POINT('Ctrl Pts',(19.0833770094289,21.7484411632419,-19.6507023954039));
#45547=CARTESIAN_POINT('Ctrl Pts',(19.1665885309657,21.7355860261267,-19.6548719613755));
#45548=CARTESIAN_POINT('Ctrl Pts',(19.2489383260604,21.7186759201209,-19.6590415273471));
#45549=CARTESIAN_POINT('Ctrl Pts',(19.3341834370069,21.7011712759268,-19.6633576900461));
#45550=CARTESIAN_POINT('Ctrl Pts',(19.4185045808362,21.6793213182574,-19.667673852745));
#45551=CARTESIAN_POINT('Ctrl Pts',(19.501435588217,21.653261783253,-19.6719900154439));
#45552=CARTESIAN_POINT('Ctrl Pts',(19.581665127909,21.6280511344978,-19.6761655796569));
#45553=CARTESIAN_POINT('Ctrl Pts',(19.6605932821676,21.5989011580776,-19.68034114387));
#45554=CARTESIAN_POINT('Ctrl Pts',(19.737817188692,21.5659842996688,-19.684516708083));
#45555=CARTESIAN_POINT('Ctrl Pts',(19.8189414894304,21.5314048897282,-19.6889031700249));
#45556=CARTESIAN_POINT('Ctrl Pts',(19.8981843303166,21.4926683234582,-19.6932896319667));
#45557=CARTESIAN_POINT('Ctrl Pts',(19.9751086547793,21.4500286525705,-19.6976760939086));
#45558=CARTESIAN_POINT('Ctrl Pts',(20.052032979242,21.4073889816829,-19.7020625558505));
#45559=CARTESIAN_POINT('Ctrl Pts',(20.1266383352643,21.3608465778203,-19.7064490177923));
#45560=CARTESIAN_POINT('Ctrl Pts',(20.1985254700751,21.3107059669157,-19.7108354797342));
#45561=CARTESIAN_POINT('Ctrl Pts',(20.2306963153617,21.2882671002084,-19.7127985039785));
#45562=CARTESIAN_POINT('Ctrl Pts',(20.26237935926,21.2650691592041,-19.7147615282228));
#45563=CARTESIAN_POINT('Ctrl Pts',(20.2935358855687,21.2411349269503,-19.7167245524671));
#45564=CARTESIAN_POINT('',(16.1740010149448,19.2087204131752,-19.3667098901939));
#45565=CARTESIAN_POINT('Ctrl Pts',(16.1740010149441,19.2087204138715,-19.3667098902285));
#45566=CARTESIAN_POINT('Ctrl Pts',(16.173926819566,19.2920425969752,-19.3708480242598));
#45567=CARTESIAN_POINT('Ctrl Pts',(16.1779248169782,19.3754486069208,-19.374986158291));
#45568=CARTESIAN_POINT('Ctrl Pts',(16.1859928190663,19.4585063754938,-19.3791242923223));
#45569=CARTESIAN_POINT('Ctrl Pts',(16.1940571655297,19.5415265104593,-19.3832605513584));
#45570=CARTESIAN_POINT('Ctrl Pts',(16.2061878113245,19.6241982519121,-19.3873968103945));
#45571=CARTESIAN_POINT('Ctrl Pts',(16.2223305526748,19.7060925038549,-19.3915330694306));
#45572=CARTESIAN_POINT('Ctrl Pts',(16.2384710163523,19.7879752008633,-19.395668744858));
#45573=CARTESIAN_POINT('Ctrl Pts',(16.2586223602412,19.8690801670325,-19.3998044202854));
#45574=CARTESIAN_POINT('Ctrl Pts',(16.2826791433891,19.9489878440355,-19.4039400957128));
#45575=CARTESIAN_POINT('Ctrl Pts',(16.3067400382207,20.0289091785212,-19.4080764779923));
#45576=CARTESIAN_POINT('Ctrl Pts',(16.3347075604893,20.1076323699276,-19.4122128602718));
#45577=CARTESIAN_POINT('Ctrl Pts',(16.3664266589092,20.1847538059263,-19.4163492425514));
#45578=CARTESIAN_POINT('Ctrl Pts',(16.3981808282506,20.2619605129437,-19.4204901983133));
#45579=CARTESIAN_POINT('Ctrl Pts',(16.4336946710478,20.3375614976538,-19.4246311540753));
#45580=CARTESIAN_POINT('Ctrl Pts',(16.4727655806453,20.4111745292772,-19.4287721098372));
#45581=CARTESIAN_POINT('Ctrl Pts',(16.5118617772824,20.4848352039083,-19.4329157456625));
#45582=CARTESIAN_POINT('Ctrl Pts',(16.5545193804039,20.556504964772,-19.4370593814878));
#45583=CARTESIAN_POINT('Ctrl Pts',(16.6004918491551,20.6258296612236,-19.4412030173131));
#45584=CARTESIAN_POINT('Ctrl Pts',(16.6465392454204,20.6952673454551,-19.4453534065789));
#45585=CARTESIAN_POINT('Ctrl Pts',(16.6959120078414,20.7623519651714,-19.4495037958447));
#45586=CARTESIAN_POINT('Ctrl Pts',(16.7483230702952,20.826762089801,-19.4536541851104));
#45587=CARTESIAN_POINT('Ctrl Pts',(16.7661884610687,20.848717608205,-19.4550689308268));
#45588=CARTESIAN_POINT('Ctrl Pts',(16.7844065661404,20.8703626874017,-19.4564836765431));
#45589=CARTESIAN_POINT('Ctrl Pts',(16.8029650799464,20.891685615317,-19.4578984222595));
#45590=CARTESIAN_POINT('Ctrl Pts',(16.8578587574058,20.9547560712656,-19.4620830566462));
#45591=CARTESIAN_POINT('Ctrl Pts',(16.915947800584,21.0152517076035,-19.466267691033));
#45592=CARTESIAN_POINT('Ctrl Pts',(16.9769612646036,21.0728310563305,-19.4704523254198));
#45593=CARTESIAN_POINT('Ctrl Pts',(17.0378878835037,21.1303284479763,-19.4746310034971));
#45594=CARTESIAN_POINT('Ctrl Pts',(17.1017303233983,21.1849174841133,-19.4788096815744));
#45595=CARTESIAN_POINT('Ctrl Pts',(17.1681782563646,21.2362906623887,-19.4829883596517));
#45596=CARTESIAN_POINT('Ctrl Pts',(17.2358172209073,21.2885846680663,-19.4872419375387));
#45597=CARTESIAN_POINT('Ctrl Pts',(17.306155687672,21.3375460297098,-19.4914955154258));
#45598=CARTESIAN_POINT('Ctrl Pts',(17.3788280009098,21.382890617154,-19.4957490933129));
#45599=CARTESIAN_POINT('Ctrl Pts',(17.4500914193923,21.4273561111915,-19.4999202072833));
#45600=CARTESIAN_POINT('Ctrl Pts',(17.5235985912763,21.46834356131,-19.5040913212538));
#45601=CARTESIAN_POINT('Ctrl Pts',(17.5989738385243,21.5056275542592,-19.5082624352243));
#45602=CARTESIAN_POINT('Ctrl Pts',(17.6743237928747,21.5428990362019,-19.5124321495369));
#45603=CARTESIAN_POINT('Ctrl Pts',(17.7515401656511,21.5764693252641,-19.5166018638495));
#45604=CARTESIAN_POINT('Ctrl Pts',(17.8302229081156,21.6061590694952,-19.5207715781621));
#45605=CARTESIAN_POINT('Ctrl Pts',(17.9089028507052,21.6358477572358,-19.5249411440981));
#45606=CARTESIAN_POINT('Ctrl Pts',(17.9890486285244,21.6616560130853,-19.5291107100341));
#45607=CARTESIAN_POINT('Ctrl Pts',(18.0702417419437,21.6834532300656,-19.5332802759701));
#45608=CARTESIAN_POINT('Ctrl Pts',(18.1542895053988,21.7060168103939,-19.5375964387177));
#45609=CARTESIAN_POINT('Ctrl Pts',(18.2394591140179,21.724281910891,-19.5419126014652));
#45610=CARTESIAN_POINT('Ctrl Pts',(18.3252730114509,21.7381609067947,-19.5462287642128));
#45611=CARTESIAN_POINT('Ctrl Pts',(18.4082915298627,21.751587795812,-19.5504043283958));
#45612=CARTESIAN_POINT('Ctrl Pts',(18.4919125329025,21.7609099414411,-19.5545798925789));
#45613=CARTESIAN_POINT('Ctrl Pts',(18.5756985998726,21.7661009112592,-19.5587554567619));
#45614=CARTESIAN_POINT('Ctrl Pts',(18.6637165024322,21.7715540646553,-19.5631419187917));
#45615=CARTESIAN_POINT('Ctrl Pts',(18.7519159980506,21.7724477372193,-19.5675283808216));
#45616=CARTESIAN_POINT('Ctrl Pts',(18.8397925195448,21.7688131172563,-19.5719148428514));
#45617=CARTESIAN_POINT('Ctrl Pts',(18.9276690410391,21.7651784972933,-19.5763013048812));
#45618=CARTESIAN_POINT('Ctrl Pts',(19.0152220177587,21.7570157144011,-19.5806877669111));
#45619=CARTESIAN_POINT('Ctrl Pts',(19.1019580505816,21.7444180217667,-19.5850742289409));
#45620=CARTESIAN_POINT('Ctrl Pts',(19.1847019893298,21.732400147836,-19.5892588006086));
#45621=CARTESIAN_POINT('Ctrl Pts',(19.2670105160923,21.7163018984399,-19.5934433722763));
#45622=CARTESIAN_POINT('Ctrl Pts',(19.3484498725015,21.6961662628852,-19.5976279439439));
#45623=CARTESIAN_POINT('Ctrl Pts',(19.4335631521515,21.6751222608761,-19.6020012916013));
#45624=CARTESIAN_POINT('Ctrl Pts',(19.5177264866766,21.6496679803991,-19.6063746392586));
#45625=CARTESIAN_POINT('Ctrl Pts',(19.600451164542,21.6199131116468,-19.6107479869159));
#45626=CARTESIAN_POINT('Ctrl Pts',(19.6793978228884,21.5915171418087,-19.614921604659));
#45627=CARTESIAN_POINT('Ctrl Pts',(19.7570338492619,21.5592049408122,-19.6190952224021));
#45628=CARTESIAN_POINT('Ctrl Pts',(19.8329471632924,21.5231235114698,-19.6232688401453));
#45629=CARTESIAN_POINT('Ctrl Pts',(19.908808933188,21.4870665809402,-19.6274396240572));
#45630=CARTESIAN_POINT('Ctrl Pts',(19.9829499000485,21.4472457028666,-19.6316104079691));
#45631=CARTESIAN_POINT('Ctrl Pts',(20.0549778814522,21.403855999995,-19.6357811918811));
#45632=CARTESIAN_POINT('Ctrl Pts',(20.1269801303178,21.3604817984211,-19.6399504857491));
#45633=CARTESIAN_POINT('Ctrl Pts',(20.1968705003484,21.3135415429754,-19.6441197796171));
#45634=CARTESIAN_POINT('Ctrl Pts',(20.2642825292425,21.2632756590417,-19.6482890734851));
#45635=CARTESIAN_POINT('Ctrl Pts',(20.2740863744592,21.2559654066454,-19.648895420934));
#45636=CARTESIAN_POINT('Ctrl Pts',(20.283837851539,21.2485848909344,-19.6495017683829));
#45637=CARTESIAN_POINT('Ctrl Pts',(20.2935358855687,21.2411349269503,-19.6501081158318));
#45638=CARTESIAN_POINT('Ctrl Pts',(20.2935358855687,21.2411349269503,-18.8501886410431));
#45639=CARTESIAN_POINT('Ctrl Pts',(20.3600880965346,21.190009969743,-18.8543616962283));
#45640=CARTESIAN_POINT('Ctrl Pts',(20.4241919562629,21.1355565384397,-18.8585347514134));
#45641=CARTESIAN_POINT('Ctrl Pts',(20.4855007784819,21.0780417839398,-18.8627078065986));
#45642=CARTESIAN_POINT('Ctrl Pts',(20.5467748064481,21.0205596704667,-18.8668784934731));
#45643=CARTESIAN_POINT('Ctrl Pts',(20.6052566115097,20.9600199972293,-18.8710491803476));
#45644=CARTESIAN_POINT('Ctrl Pts',(20.6606332957843,20.8967295582552,-18.8752198672221));
#45645=CARTESIAN_POINT('Ctrl Pts',(20.7159951643049,20.8334560523205,-18.8793894382502));
#45646=CARTESIAN_POINT('Ctrl Pts',(20.7682532594284,20.7674335885141,-18.8835590092783));
#45647=CARTESIAN_POINT('Ctrl Pts',(20.8171331635652,20.6990041071365,-18.8877285803065));
#45648=CARTESIAN_POINT('Ctrl Pts',(20.8660146528381,20.6305724066455,-18.8918982865505));
#45649=CARTESIAN_POINT('Ctrl Pts',(20.911517467248,20.5597339086927,-18.8960679927945));
#45650=CARTESIAN_POINT('Ctrl Pts',(20.9534097480727,20.4868606390041,-18.9002376990385));
#45651=CARTESIAN_POINT('Ctrl Pts',(20.9953447652096,20.4139130278199,-18.9044116589985));
#45652=CARTESIAN_POINT('Ctrl Pts',(21.0336616621183,20.338926898568,-18.9085856189586));
#45653=CARTESIAN_POINT('Ctrl Pts',(21.0681741689714,20.2622996475347,-18.9127595789187));
#45654=CARTESIAN_POINT('Ctrl Pts',(21.1027039955892,20.1856339418634,-18.9169356335398));
#45655=CARTESIAN_POINT('Ctrl Pts',(21.133425461192,20.1073259026731,-18.9211116881609));
#45656=CARTESIAN_POINT('Ctrl Pts',(21.1602010975522,20.0277914263976,-18.9252877427821));
#45657=CARTESIAN_POINT('Ctrl Pts',(21.1870245425827,19.9481149390228,-18.929471253869));
#45658=CARTESIAN_POINT('Ctrl Pts',(21.2098879562465,19.8672080828444,-18.9336547649561));
#45659=CARTESIAN_POINT('Ctrl Pts',(21.2287042779432,19.7855002746841,-18.9378382760431));
#45660=CARTESIAN_POINT('Ctrl Pts',(21.2457310804045,19.7115632570501,-18.9416239158733));
#45661=CARTESIAN_POINT('Ctrl Pts',(21.2594446080859,19.6369707745906,-18.9454095557035));
#45662=CARTESIAN_POINT('Ctrl Pts',(21.2698170137415,19.5620442604844,-18.9491951955337));
#45663=CARTESIAN_POINT('Ctrl Pts',(21.2812826384042,19.4792207269144,-18.9533798299225));
#45664=CARTESIAN_POINT('Ctrl Pts',(21.2887076244829,19.3956807451278,-18.9575644643113));
#45665=CARTESIAN_POINT('Ctrl Pts',(21.2920126435715,19.3118529391169,-18.9617490987001));
#45666=CARTESIAN_POINT('Ctrl Pts',(21.2953129583745,19.228144451612,-18.9659277767799));
#45667=CARTESIAN_POINT('Ctrl Pts',(21.294504936491,19.1441494093845,-18.9701064548596));
#45668=CARTESIAN_POINT('Ctrl Pts',(21.2895607321101,19.0603038006549,-18.9742851329393));
#45669=CARTESIAN_POINT('Ctrl Pts',(21.2845279064127,18.9749553195403,-18.9785387108258));
#45670=CARTESIAN_POINT('Ctrl Pts',(21.2752090914542,18.8897621593927,-18.9827922887123));
#45671=CARTESIAN_POINT('Ctrl Pts',(21.2616304174303,18.8051866526579,-18.9870458665988));
#45672=CARTESIAN_POINT('Ctrl Pts',(21.2483149925156,18.7222508072601,-18.9912169805726));
#45673=CARTESIAN_POINT('Ctrl Pts',(21.2309034822292,18.6399093552897,-18.9953880945464));
#45674=CARTESIAN_POINT('Ctrl Pts',(21.2094728610011,18.5585935971749,-18.9995592085202));
#45675=CARTESIAN_POINT('Ctrl Pts',(21.1880494310247,18.4773051253474,-19.0037289228364));
#45676=CARTESIAN_POINT('Ctrl Pts',(21.1626096856898,18.3970421082987,-19.0078986371526));
#45677=CARTESIAN_POINT('Ctrl Pts',(21.1332813336496,18.3182239463334,-19.0120683514689));
#45678=CARTESIAN_POINT('Ctrl Pts',(21.1039540252378,18.2394085890558,-19.0162379174088));
#45679=CARTESIAN_POINT('Ctrl Pts',(21.0707385464732,18.1620384154915,-19.0204074833488));
#45680=CARTESIAN_POINT('Ctrl Pts',(21.0338114728017,18.0865147001541,-19.0245770492887));
#45681=CARTESIAN_POINT('Ctrl Pts',(20.9955860886931,18.0083356639876,-19.0288932120326));
#45682=CARTESIAN_POINT('Ctrl Pts',(20.9533834858384,17.9321358186686,-19.0332093747765));
#45683=CARTESIAN_POINT('Ctrl Pts',(20.9074514472649,17.8583327066931,-19.0375255375203));
#45684=CARTESIAN_POINT('Ctrl Pts',(20.8630156401098,17.7869337234772,-19.041701101708));
#45685=CARTESIAN_POINT('Ctrl Pts',(20.8150899458169,17.7177780846045,-19.0458766658958));
#45686=CARTESIAN_POINT('Ctrl Pts',(20.7639418957711,17.6512128671536,-19.0500522300835));
#45687=CARTESIAN_POINT('Ctrl Pts',(20.7102104791443,17.5812855985968,-19.0544386921054));
#45688=CARTESIAN_POINT('Ctrl Pts',(20.6529230087042,17.5142177570107,-19.0588251541274));
#45689=CARTESIAN_POINT('Ctrl Pts',(20.5924345734847,17.4503691653055,-19.0632116161493));
#45690=CARTESIAN_POINT('Ctrl Pts',(20.5319461382652,17.3865205736004,-19.0675980781713));
#45691=CARTESIAN_POINT('Ctrl Pts',(20.468257210959,17.3258915767387,-19.0719845401932));
#45692=CARTESIAN_POINT('Ctrl Pts',(20.4017623229458,17.2687927931958,-19.0763710022152));
#45693=CARTESIAN_POINT('Ctrl Pts',(20.3383269634738,17.2143212094742,-19.0805556366057));
#45694=CARTESIAN_POINT('Ctrl Pts',(20.2721020634018,17.1628593635266,-19.0847402709962));
#45695=CARTESIAN_POINT('Ctrl Pts',(20.2034050887144,17.114705964026,-19.0889249053867));
#45696=CARTESIAN_POINT('Ctrl Pts',(20.1348058956684,17.0666211049301,-19.093103583468));
#45697=CARTESIAN_POINT('Ctrl Pts',(20.0637419907199,17.0218356001937,-19.0972822615494));
#45698=CARTESIAN_POINT('Ctrl Pts',(19.9905648985565,16.9806088558919,-19.1014609396307));
#45699=CARTESIAN_POINT('Ctrl Pts',(19.91607615955,16.9386431517953,-19.1057145175168));
#45700=CARTESIAN_POINT('Ctrl Pts',(19.8393980962005,16.900365358686,-19.1099680954029));
#45701=CARTESIAN_POINT('Ctrl Pts',(19.7609336007079,16.8660037569887,-19.114221673289));
#45702=CARTESIAN_POINT('Ctrl Pts',(19.6839902926328,16.8323083220184,-19.1183927872642));
#45703=CARTESIAN_POINT('Ctrl Pts',(19.6053296420405,16.8023787805159,-19.1225639012394));
#45704=CARTESIAN_POINT('Ctrl Pts',(19.5253559691354,16.7763838639092,-19.1267350152147));
#45705=CARTESIAN_POINT('Ctrl Pts',(19.4454091321692,16.7503976701479,-19.1309047295323));
#45706=CARTESIAN_POINT('Ctrl Pts',(19.3641505850606,16.7283436212314,-19.13507444385));
#45707=CARTESIAN_POINT('Ctrl Pts',(19.2820021033662,16.7103413478233,-19.1392441581676));
#45708=CARTESIAN_POINT('Ctrl Pts',(19.1998565448679,16.6923397150134,-19.1434137241089));
#45709=CARTESIAN_POINT('Ctrl Pts',(19.1168215642988,16.6783896686896,-19.1475832900501));
#45710=CARTESIAN_POINT('Ctrl Pts',(19.0333301469618,16.6685599391294,-19.1517528559914));
#45711=CARTESIAN_POINT('Ctrl Pts',(18.9469032742682,16.6583846083898,-19.1560690187335));
#45712=CARTESIAN_POINT('Ctrl Pts',(18.8599877947896,16.6526247876704,-19.1603851814756));
#45713=CARTESIAN_POINT('Ctrl Pts',(18.77306891594,16.651298138492,-19.1647013442177));
#45714=CARTESIAN_POINT('Ctrl Pts',(18.6889814105451,16.650014704773,-19.1688769084066));
#45715=CARTESIAN_POINT('Ctrl Pts',(18.6048911930079,16.652879993597,-19.1730524725954));
#45716=CARTESIAN_POINT('Ctrl Pts',(18.5212349098901,16.6598569196475,-19.1772280367843));
#45717=CARTESIAN_POINT('Ctrl Pts',(18.4333533466031,16.667186233662,-19.181614498803));
#45718=CARTESIAN_POINT('Ctrl Pts',(18.345951284399,16.6790533797553,-19.1860009608217));
#45719=CARTESIAN_POINT('Ctrl Pts',(18.2595234803602,16.6953545495618,-19.1903874228404));
#45720=CARTESIAN_POINT('Ctrl Pts',(18.1730956763213,16.7116557193683,-19.1947738848591));
#45721=CARTESIAN_POINT('Ctrl Pts',(18.0876426763664,16.7323907021497,-19.1991603468778));
#45722=CARTESIAN_POINT('Ctrl Pts',(18.0036392138284,16.7573958913421,-19.2035468088965));
#45723=CARTESIAN_POINT('Ctrl Pts',(17.9235008748349,16.7812505547995,-19.2077314433106));
#45724=CARTESIAN_POINT('Ctrl Pts',(17.8443833236132,16.8090798944622,-19.2119160777247));
#45725=CARTESIAN_POINT('Ctrl Pts',(17.7667095652053,16.8407786570123,-19.2161007121388));
#45726=CARTESIAN_POINT('Ctrl Pts',(17.6891463657766,16.8724323002981,-19.2202793902438));
#45727=CARTESIAN_POINT('Ctrl Pts',(17.6130232994518,16.9079442542207,-19.2244580683488));
#45728=CARTESIAN_POINT('Ctrl Pts',(17.5387487593373,16.9471593537322,-19.2286367464538));
#45729=CARTESIAN_POINT('Ctrl Pts',(17.4631429019463,16.9870773554683,-19.232890324334));
#45730=CARTESIAN_POINT('Ctrl Pts',(17.3894529543325,17.0308324287606,-19.2371439022142));
#45731=CARTESIAN_POINT('Ctrl Pts',(17.3180889421074,17.0782093688931,-19.2413974800944));
#45732=CARTESIAN_POINT('Ctrl Pts',(17.2481084600744,17.1246678148849,-19.2455685940934));
#45733=CARTESIAN_POINT('Ctrl Pts',(17.1803649335802,17.1746086808986,-19.2497397080924));
#45734=CARTESIAN_POINT('Ctrl Pts',(17.1152190899139,17.2277833287458,-19.2539108220915));
#45735=CARTESIAN_POINT('Ctrl Pts',(17.0500951065651,17.2809401333258,-19.2580805364329));
#45736=CARTESIAN_POINT('Ctrl Pts',(16.9875674309667,17.337328274007,-19.2622502507743));
#45737=CARTESIAN_POINT('Ctrl Pts',(16.9279649526866,17.3966578580996,-19.2664199651157));
#45738=CARTESIAN_POINT('Ctrl Pts',(16.8683645953195,17.45598533099,-19.2705895310807));
#45739=CARTESIAN_POINT('Ctrl Pts',(16.8116895537474,17.5182537140333,-19.2747590970458));
#45740=CARTESIAN_POINT('Ctrl Pts',(16.7582319859915,17.5831361375039,-19.2789286630108));
#45741=CARTESIAN_POINT('Ctrl Pts',(16.702894916699,17.6502997462159,-19.2832448257247));
#45742=CARTESIAN_POINT('Ctrl Pts',(16.6510061189344,17.7202642276924,-19.2875609884387));
#45743=CARTESIAN_POINT('Ctrl Pts',(16.6028430768051,17.7926311591414,-19.2918771511526));
#45744=CARTESIAN_POINT('Ctrl Pts',(16.556248940208,17.8626407461605,-19.2960527153649));
#45745=CARTESIAN_POINT('Ctrl Pts',(16.5131417547257,17.9348982385108,-19.3002282795771));
#45746=CARTESIAN_POINT('Ctrl Pts',(16.4737266859811,18.0090164119531,-19.3044038437894));
#45747=CARTESIAN_POINT('Ctrl Pts',(16.4323208564697,18.086878116905,-19.3087903057542));
#45748=CARTESIAN_POINT('Ctrl Pts',(16.3949901703488,18.1667928797147,-19.3131767677189));
#45749=CARTESIAN_POINT('Ctrl Pts',(16.3619151438302,18.2482884984951,-19.3175632296837));
#45750=CARTESIAN_POINT('Ctrl Pts',(16.3288401173116,18.3297841172754,-19.3219496916485));
#45751=CARTESIAN_POINT('Ctrl Pts',(16.3000208686933,18.4128600189268,-19.3263361536133));
#45752=CARTESIAN_POINT('Ctrl Pts',(16.2755767948946,18.4970284707363,-19.330722615578));
#45753=CARTESIAN_POINT('Ctrl Pts',(16.2465257453506,18.5970601546401,-19.3359357942368));
#45754=CARTESIAN_POINT('Ctrl Pts',(16.2235642356451,18.6989346521906,-19.3411489728956));
#45755=CARTESIAN_POINT('Ctrl Pts',(16.2068848499389,18.8019901977558,-19.3463621515544));
#45756=CARTESIAN_POINT('Ctrl Pts',(16.1904712789818,18.9034033756426,-19.3514922492292));
#45757=CARTESIAN_POINT('Ctrl Pts',(16.1801412136981,19.0059603454969,-19.356622346904));
#45758=CARTESIAN_POINT('Ctrl Pts',(16.1760324691886,19.1090092586819,-19.3617524445787));
#45759=CARTESIAN_POINT('Ctrl Pts',(16.1747089805831,19.1422028685768,-19.3634049264505));
#45760=CARTESIAN_POINT('Ctrl Pts',(16.1740306434087,19.1754473495068,-19.3650574083222));
#45761=CARTESIAN_POINT('Ctrl Pts',(16.1740010149447,19.2087204131752,-19.3667098901939));
#45762=CARTESIAN_POINT('Origin',(18.734,19.211,1.76670989022852));
#45763=CARTESIAN_POINT('',(20.2935358855687,21.2411349269503,-18.0500683201495));
#45764=CARTESIAN_POINT('',(20.2935358855687,21.2411349269503,-18.1167065565846));
#45765=CARTESIAN_POINT('',(20.2935358855687,21.2411349269503,1.76670989022852));
#45766=CARTESIAN_POINT('',(16.1743944470979,19.2113823947302,-18.633290134885));
#45767=CARTESIAN_POINT('Ctrl Pts',(20.2935358855687,21.2411349269503,-18.1167065565846));
#45768=CARTESIAN_POINT('Ctrl Pts',(20.3602206228857,21.1899081638987,-18.1208760360078));
#45769=CARTESIAN_POINT('Ctrl Pts',(20.4243870798335,21.1353858945908,-18.125045515431));
#45770=CARTESIAN_POINT('Ctrl Pts',(20.4857019867477,21.0778530069677,-18.1292149948543));
#45771=CARTESIAN_POINT('Ctrl Pts',(20.5470276395309,21.020310036301,-18.1333852050081));
#45772=CARTESIAN_POINT('Ctrl Pts',(20.6055004154035,20.9597557153283,-18.137555415162));
#45773=CARTESIAN_POINT('Ctrl Pts',(20.660823359764,20.896512307955,-18.1417256253158));
#45774=CARTESIAN_POINT('Ctrl Pts',(20.7162074113154,20.83319904481,-18.1459004416928));
#45775=CARTESIAN_POINT('Ctrl Pts',(20.7684343845667,20.7671911142531,-18.1500752580698));
#45776=CARTESIAN_POINT('Ctrl Pts',(20.8172475167671,20.698844005225,-18.1542500744469));
#45777=CARTESIAN_POINT('Ctrl Pts',(20.8660913973001,20.6304538430357,-18.1584275206212));
#45778=CARTESIAN_POINT('Ctrl Pts',(20.9115169082914,20.5597219564181,-18.1626049667955));
#45779=CARTESIAN_POINT('Ctrl Pts',(20.953311843756,20.4870309322914,-18.1667824129698));
#45780=CARTESIAN_POINT('Ctrl Pts',(20.9951752878851,20.4142207558097,-18.1709667066546));
#45781=CARTESIAN_POINT('Ctrl Pts',(21.0333960698403,20.3394454413685,-18.1751510003393));
#45782=CARTESIAN_POINT('Ctrl Pts',(21.0678091422995,20.2631097315961,-18.1793352940241));
#45783=CARTESIAN_POINT('Ctrl Pts',(21.0825869336838,20.2303293631612,-18.1811321292017));
#45784=CARTESIAN_POINT('Ctrl Pts',(21.0966631839603,20.1972614661371,-18.1829289643794));
#45785=CARTESIAN_POINT('Ctrl Pts',(21.1100276507034,20.1639389293617,-18.184725799557));
#45786=CARTESIAN_POINT('Ctrl Pts',(21.1411520453503,20.0863343526005,-18.1889104339505));
#45787=CARTESIAN_POINT('Ctrl Pts',(21.1685283427045,20.00705890033,-18.193095068344));
#45788=CARTESIAN_POINT('Ctrl Pts',(21.1919760688457,19.926509360513,-18.1972797027374));
#45789=CARTESIAN_POINT('Ctrl Pts',(21.2153904200511,19.8460744729958,-18.2014583808218));
#45790=CARTESIAN_POINT('Ctrl Pts',(21.2348871797096,19.7643695380467,-18.2056370589062));
#45791=CARTESIAN_POINT('Ctrl Pts',(21.2503340551361,19.6818109206064,-18.2098157369906));
#45792=CARTESIAN_POINT('Ctrl Pts',(21.266057804701,19.5977724992935,-18.2140693148759));
#45793=CARTESIAN_POINT('Ctrl Pts',(21.2775848741471,19.5128499374384,-18.2183228927613));
#45794=CARTESIAN_POINT('Ctrl Pts',(21.2848289888802,19.4274981974251,-18.2225764706466));
#45795=CARTESIAN_POINT('Ctrl Pts',(21.2919326623144,19.3438011674312,-18.226747584625));
#45796=CARTESIAN_POINT('Ctrl Pts',(21.2949179252555,19.2596919311855,-18.2309186986034));
#45797=CARTESIAN_POINT('Ctrl Pts',(21.2937553357682,19.1756076137218,-18.2350898125818));
#45798=CARTESIAN_POINT('Ctrl Pts',(21.2925931363989,19.0915515115629,-18.2392595269026));
#45799=CARTESIAN_POINT('Ctrl Pts',(21.287285855196,19.0075207711856,-18.2434292412234));
#45800=CARTESIAN_POINT('Ctrl Pts',(21.2778561566697,18.9239532195377,-18.2475989555442));
#45801=CARTESIAN_POINT('Ctrl Pts',(21.2684267936926,18.8403886415822,-18.2517685214887));
#45802=CARTESIAN_POINT('Ctrl Pts',(21.2548753574853,18.7572876766215,-18.2559380874332));
#45803=CARTESIAN_POINT('Ctrl Pts',(21.2372763100334,18.6750823611547,-18.2601076533776));
#45804=CARTESIAN_POINT('Ctrl Pts',(21.2190585017879,18.5899868082263,-18.264423816116));
#45805=CARTESIAN_POINT('Ctrl Pts',(21.1965032689153,18.5058515744425,-18.2687399788544));
#45806=CARTESIAN_POINT('Ctrl Pts',(21.1697502461669,18.4231416762528,-18.2730561415928));
#45807=CARTESIAN_POINT('Ctrl Pts',(21.143868700315,18.3431260442794,-18.2772317057849));
#45808=CARTESIAN_POINT('Ctrl Pts',(21.114058861765,18.2644447370881,-18.281407269977));
#45809=CARTESIAN_POINT('Ctrl Pts',(21.0804965434245,18.1874991589174,-18.2855828341691));
#45810=CARTESIAN_POINT('Ctrl Pts',(21.045239072183,18.1066672425405,-18.2899692961807));
#45811=CARTESIAN_POINT('Ctrl Pts',(21.0058403441653,18.0277515290332,-18.2943557581922));
#45812=CARTESIAN_POINT('Ctrl Pts',(20.9625580617871,17.9511869324206,-18.2987422202038));
#45813=CARTESIAN_POINT('Ctrl Pts',(20.9192757794088,17.8746223358079,-18.3031286822153));
#45814=CARTESIAN_POINT('Ctrl Pts',(20.8721103180847,17.8004093049791,-18.3075151442269));
#45815=CARTESIAN_POINT('Ctrl Pts',(20.8213695361433,17.7289445288449,-18.3119016062384));
#45816=CARTESIAN_POINT('Ctrl Pts',(20.7729634127898,17.6607679529896,-18.3160862406309));
#45817=CARTESIAN_POINT('Ctrl Pts',(20.7211235735797,17.5948385205844,-18.3202708750235));
#45818=CARTESIAN_POINT('Ctrl Pts',(20.6660859672865,17.5315227554341,-18.324455509416));
#45819=CARTESIAN_POINT('Ctrl Pts',(20.6111267002136,17.4682971124387,-18.3286341874995));
#45820=CARTESIAN_POINT('Ctrl Pts',(20.5529790062397,17.407678091374,-18.3328128655829));
#45821=CARTESIAN_POINT('Ctrl Pts',(20.491921374867,17.3500022998978,-18.3369915436664));
#45822=CARTESIAN_POINT('Ctrl Pts',(20.4297693293241,17.2912927113015,-18.3412451215519));
#45823=CARTESIAN_POINT('Ctrl Pts',(20.3646022781507,17.23563329804,-18.3454986994375));
#45824=CARTESIAN_POINT('Ctrl Pts',(20.2967560739111,17.1833428659031,-18.349752277323));
#45825=CARTESIAN_POINT('Ctrl Pts',(20.2302252007414,17.1320661858371,-18.3539233913005));
#45826=CARTESIAN_POINT('Ctrl Pts',(20.1611185098597,17.0840293178159,-18.358094505278));
#45827=CARTESIAN_POINT('Ctrl Pts',(20.0897876178817,17.0394936253378,-18.3622656192554));
#45828=CARTESIAN_POINT('Ctrl Pts',(20.0184806616734,16.9949728772414,-18.3664353335753));
#45829=CARTESIAN_POINT('Ctrl Pts',(19.9449513765316,16.9539512148436,-18.3706050478952));
#45830=CARTESIAN_POINT('Ctrl Pts',(19.8695801735014,16.9166465683006,-18.3747747622151));
#45831=CARTESIAN_POINT('Ctrl Pts',(19.7942116525019,16.8793432492171,-18.3789443281586));
#45832=CARTESIAN_POINT('Ctrl Pts',(19.7170017566051,16.8457568863073,-18.3831138941022));
#45833=CARTESIAN_POINT('Ctrl Pts',(19.6383540649958,16.816058721988,-18.3872834600458));
#45834=CARTESIAN_POINT('Ctrl Pts',(19.5569412175515,16.7853164068402,-18.3915996227853));
#45835=CARTESIAN_POINT('Ctrl Pts',(19.473988080848,16.7587409819329,-18.3959157855248));
#45836=CARTESIAN_POINT('Ctrl Pts',(19.3899612417722,16.7364667411221,-18.4002319482643));
#45837=CARTESIAN_POINT('Ctrl Pts',(19.3086715681611,16.7149180813683,-18.4044075124555));
#45838=CARTESIAN_POINT('Ctrl Pts',(19.2263775401993,16.6973947388031,-18.4085830766467));
#45839=CARTESIAN_POINT('Ctrl Pts',(19.1435118395199,16.6839661550955,-18.4127586408379));
#45840=CARTESIAN_POINT('Ctrl Pts',(19.0564607892622,16.6698593255431,-18.4171451028516));
#45841=CARTESIAN_POINT('Ctrl Pts',(18.9687793786238,16.6602718418454,-18.4215315648652));
#45842=CARTESIAN_POINT('Ctrl Pts',(18.880972790904,16.6552224277661,-18.4259180268789));
#45843=CARTESIAN_POINT('Ctrl Pts',(18.7931662031841,16.6501730136867,-18.4303044888925));
#45844=CARTESIAN_POINT('Ctrl Pts',(18.7052350190325,16.6496615965365,-18.4346909509062));
#45845=CARTESIAN_POINT('Ctrl Pts',(18.6176794289206,16.6536440363642,-18.4390774129198));
#45846=CARTESIAN_POINT('Ctrl Pts',(18.5341524013311,16.6574432382304,-18.4432620473123));
#45847=CARTESIAN_POINT('Ctrl Pts',(18.4506562604971,16.6653459878634,-18.4474466817047));
#45848=CARTESIAN_POINT('Ctrl Pts',(18.3676269095308,16.6773522820684,-18.4516313160972));
#45849=CARTESIAN_POINT('Ctrl Pts',(18.2847157405689,16.6893414867996,-18.4558099941805));
#45850=CARTESIAN_POINT('Ctrl Pts',(18.2022704931355,16.7054225689873,-18.4599886722639));
#45851=CARTESIAN_POINT('Ctrl Pts',(18.1207249420869,16.725543562373,-18.4641673503472));
#45852=CARTESIAN_POINT('Ctrl Pts',(18.0377177456267,16.746025210108,-18.4684209282328));
#45853=CARTESIAN_POINT('Ctrl Pts',(17.9556432985583,16.7706930025008,-18.4726745061184));
#45854=CARTESIAN_POINT('Ctrl Pts',(17.8749514567222,16.7994371042222,-18.476928084004));
#45855=CARTESIAN_POINT('Ctrl Pts',(17.7958239837115,16.8276239454371,-18.4810991979813));
#45856=CARTESIAN_POINT('Ctrl Pts',(17.7180264386455,16.8597302905275,-18.4852703119587));
#45857=CARTESIAN_POINT('Ctrl Pts',(17.6419689102697,16.8956019566687,-18.489441425936));
#45858=CARTESIAN_POINT('Ctrl Pts',(17.5659369037323,16.9314615857258,-18.4936111402558));
#45859=CARTESIAN_POINT('Ctrl Pts',(17.491644170023,16.9710838304477,-18.4977808545755));
#45860=CARTESIAN_POINT('Ctrl Pts',(17.4194798631985,17.0142667868074,-18.5019505688953));
#45861=CARTESIAN_POINT('Ctrl Pts',(17.3473181242895,17.0574482065323,-18.5061201348387));
#45862=CARTESIAN_POINT('Ctrl Pts',(17.2772850559938,17.104189849021,-18.5102897007821));
#45863=CARTESIAN_POINT('Ctrl Pts',(17.2097430958424,17.1542450583193,-18.5144592667256));
#45864=CARTESIAN_POINT('Ctrl Pts',(17.1398264436722,17.206060147043,-18.5187754294652));
#45865=CARTESIAN_POINT('Ctrl Pts',(17.0725797574076,17.2614258339336,-18.5230915922048));
#45866=CARTESIAN_POINT('Ctrl Pts',(17.0083685115613,17.3200224839759,-18.5274077549445));
#45867=CARTESIAN_POINT('Ctrl Pts',(16.9462489403141,17.3767103542885,-18.5315833191356));
#45868=CARTESIAN_POINT('Ctrl Pts',(16.8869703858411,17.4364215555155,-18.5357588833266));
#45869=CARTESIAN_POINT('Ctrl Pts',(16.8308254399579,17.4988298583352,-18.5399344475177));
#45870=CARTESIAN_POINT('Ctrl Pts',(16.7718447463028,17.5643902561989,-18.5443209095316));
#45871=CARTESIAN_POINT('Ctrl Pts',(16.7163229051916,17.6329269235817,-18.5487073715455));
#45872=CARTESIAN_POINT('Ctrl Pts',(16.6645491064847,17.7040252160939,-18.5530938335595));
#45873=CARTESIAN_POINT('Ctrl Pts',(16.6127753077779,17.775123508606,-18.5574802955734));
#45874=CARTESIAN_POINT('Ctrl Pts',(16.5647498046499,17.8487828986679,-18.5618667575873));
#45875=CARTESIAN_POINT('Ctrl Pts',(16.5207062260027,17.924558913131,-18.5662532196012));
#45876=CARTESIAN_POINT('Ctrl Pts',(16.4770273612299,17.9997074453442,-18.5706033584188));
#45877=CARTESIAN_POINT('Ctrl Pts',(16.4371122169921,18.0771985084612,-18.5749534972363));
#45878=CARTESIAN_POINT('Ctrl Pts',(16.4012086273385,18.1566355413635,-18.5793036360539));
#45879=CARTESIAN_POINT('Ctrl Pts',(16.3640774712899,18.2387885765663,-18.5838025088637));
#45880=CARTESIAN_POINT('Ctrl Pts',(16.3312374248385,18.3230227236652,-18.5883013816735));
#45881=CARTESIAN_POINT('Ctrl Pts',(16.3029130373493,18.4088677290933,-18.5928002544833));
#45882=CARTESIAN_POINT('Ctrl Pts',(16.2756354411695,18.4915401396801,-18.5971328613513));
#45883=CARTESIAN_POINT('Ctrl Pts',(16.2525458055772,18.5757060184788,-18.6014654682194));
#45884=CARTESIAN_POINT('Ctrl Pts',(16.2337970621827,18.660922487526,-18.6057980750875));
#45885=CARTESIAN_POINT('Ctrl Pts',(16.2150725182344,18.7460289656627,-18.6101250897576));
#45886=CARTESIAN_POINT('Ctrl Pts',(16.2006778102744,18.8321829392905,-18.6144521044276));
#45887=CARTESIAN_POINT('Ctrl Pts',(16.1907160845812,18.9189265065566,-18.6187791190976));
#45888=CARTESIAN_POINT('Ctrl Pts',(16.1807681682272,19.005549826451,-18.6231001354883));
#45889=CARTESIAN_POINT('Ctrl Pts',(16.1752410444519,19.0927607071638,-18.6274211518791));
#45890=CARTESIAN_POINT('Ctrl Pts',(16.1741865858058,19.1800923227742,-18.6317421682699));
#45891=CARTESIAN_POINT('Ctrl Pts',(16.1740606709629,19.190520751334,-18.6322581487704));
#45892=CARTESIAN_POINT('Ctrl Pts',(16.1739984722012,19.2009508929684,-18.632774129271));
#45893=CARTESIAN_POINT('Ctrl Pts',(16.1740000284928,19.2113819467091,-18.6332901097715));
#45894=CARTESIAN_POINT('Ctrl Pts',(16.1781629602604,19.2113866753936,-18.633290374834));
#45895=CARTESIAN_POINT('Ctrl Pts',(16.1776269335845,19.615981772308,-18.6533365919835));
#45896=CARTESIAN_POINT('Ctrl Pts',(16.4590846999913,20.8754715672834,-18.7157747446936));
#45897=CARTESIAN_POINT('Ctrl Pts',(18.237060364334,22.0893673291904,-18.8102032533429));
#45898=CARTESIAN_POINT('Ctrl Pts',(19.7793305876597,21.6276026831124,-18.8845855448426));
#45899=CARTESIAN_POINT('Ctrl Pts',(20.2933494018237,21.2408835667842,-18.9165759007818));
#45900=CARTESIAN_POINT('',(16.1740000028035,19.2111198080496,-18.5667098901964));
#45901=CARTESIAN_POINT('Ctrl Pts',(16.1740000028035,19.2111198086916,-18.5667098902285));
#45902=CARTESIAN_POINT('Ctrl Pts',(16.1740003013853,19.2174997239769,-18.5670291853155));
#45903=CARTESIAN_POINT('Ctrl Pts',(16.1740244495167,19.223879573923,-18.5673484804024));
#45904=CARTESIAN_POINT('Ctrl Pts',(16.1740724460423,19.2302592442234,-18.5676677754894));
#45905=CARTESIAN_POINT('Ctrl Pts',(16.1747014814392,19.31387026376,-18.5718524098819));
#45906=CARTESIAN_POINT('Ctrl Pts',(16.1794322843349,19.3976060296583,-18.5760370442745));
#45907=CARTESIAN_POINT('Ctrl Pts',(16.1882813814472,19.4810309522136,-18.580221678667));
#45908=CARTESIAN_POINT('Ctrl Pts',(16.197117882965,19.5643371297178,-18.5844003567505));
#45909=CARTESIAN_POINT('Ctrl Pts',(16.2100609870472,19.6473328891642,-18.5885790348339));
#45910=CARTESIAN_POINT('Ctrl Pts',(16.2270752140173,19.7295827970784,-18.5927577129174));
#45911=CARTESIAN_POINT('Ctrl Pts',(16.2443944087804,19.8133069754922,-18.5970112908029));
#45912=CARTESIAN_POINT('Ctrl Pts',(16.2659321081158,19.8962578184692,-18.6012648686885));
#45913=CARTESIAN_POINT('Ctrl Pts',(16.2915956147073,19.9779816286607,-18.6055184465741));
#45914=CARTESIAN_POINT('Ctrl Pts',(16.3167615841416,20.058121063309,-18.6096895605515));
#45915=CARTESIAN_POINT('Ctrl Pts',(16.3458946705845,20.1370801583406,-18.613860674529));
#45916=CARTESIAN_POINT('Ctrl Pts',(16.3788563531112,20.2144432731945,-18.6180317885065));
#45917=CARTESIAN_POINT('Ctrl Pts',(16.4118069750271,20.2917804281082,-18.6222015028263));
#45918=CARTESIAN_POINT('Ctrl Pts',(16.4485834613786,20.3675222435802,-18.6263712171462));
#45919=CARTESIAN_POINT('Ctrl Pts',(16.4889988104969,20.4412721890418,-18.6305409314661));
#45920=CARTESIAN_POINT('Ctrl Pts',(16.5294127214636,20.5150195101638,-18.6347104974097));
#45921=CARTESIAN_POINT('Ctrl Pts',(16.5734650159173,20.5867746991837,-18.6388800633532));
#45922=CARTESIAN_POINT('Ctrl Pts',(16.620922959331,20.6561662258016,-18.6430496292968));
#45923=CARTESIAN_POINT('Ctrl Pts',(16.6700494655017,20.7279974729095,-18.6473657920363));
#45924=CARTESIAN_POINT('Ctrl Pts',(16.7228252639787,20.7972953169818,-18.6516819547758));
#45925=CARTESIAN_POINT('Ctrl Pts',(16.7789448088305,20.8636824254772,-18.6559981175153));
#45926=CARTESIAN_POINT('Ctrl Pts',(16.8332362653982,20.9279069808804,-18.6601736817065));
#45927=CARTESIAN_POINT('Ctrl Pts',(16.8906566126945,20.9894072108734,-18.6643492458977));
#45928=CARTESIAN_POINT('Ctrl Pts',(16.9508909514353,21.0478783631277,-18.668524810089));
#45929=CARTESIAN_POINT('Ctrl Pts',(17.0141675834551,21.1093027543025,-18.6729112721026));
#45930=CARTESIAN_POINT('Ctrl Pts',(17.0805495076474,21.1673836440658,-18.6772977341163));
#45931=CARTESIAN_POINT('Ctrl Pts',(17.149633344248,21.2218163268039,-18.6816841961299));
#45932=CARTESIAN_POINT('Ctrl Pts',(17.2187171808487,21.276249009542,-18.6860706581435));
#45933=CARTESIAN_POINT('Ctrl Pts',(17.2905024122582,21.327033212256,-18.6904571201572));
#45934=CARTESIAN_POINT('Ctrl Pts',(17.3645537444777,21.3739186191894,-18.6948435821708));
#45935=CARTESIAN_POINT('Ctrl Pts',(17.435197865104,21.4186467590315,-18.6990282165633));
#45936=CARTESIAN_POINT('Ctrl Pts',(17.5081670866297,21.4599934843659,-18.7032128509557));
#45937=CARTESIAN_POINT('Ctrl Pts',(17.5831040926458,21.497709122393,-18.7073974853482));
#45938=CARTESIAN_POINT('Ctrl Pts',(17.6579344351091,21.5353710768775,-18.7115761634316));
#45939=CARTESIAN_POINT('Ctrl Pts',(17.7347265911908,21.5694120050826,-18.7157548415149));
#45940=CARTESIAN_POINT('Ctrl Pts',(17.8130952257718,21.5996260479204,-18.7199335195983));
#45941=CARTESIAN_POINT('Ctrl Pts',(17.8928685618191,21.630381655767,-18.7241870974839));
#45942=CARTESIAN_POINT('Ctrl Pts',(17.9742750416618,21.6571715770568,-18.7284406753695));
#45943=CARTESIAN_POINT('Ctrl Pts',(18.0568830023299,21.6798281777933,-18.732694253255));
#45944=CARTESIAN_POINT('Ctrl Pts',(18.1378894464698,21.7020455361098,-18.7368653672324));
#45945=CARTESIAN_POINT('Ctrl Pts',(18.2200507369794,21.7202882813848,-18.7410364812097));
#45946=CARTESIAN_POINT('Ctrl Pts',(18.3029424071742,21.734447909442,-18.7452075951871));
#45947=CARTESIAN_POINT('Ctrl Pts',(18.3858062622684,21.7486027860993,-18.7493773095069));
#45948=CARTESIAN_POINT('Ctrl Pts',(18.469399557216,21.7586771892408,-18.7535470238266));
#45949=CARTESIAN_POINT('Ctrl Pts',(18.5532876521045,21.7646137232005,-18.7577167381464));
#45950=CARTESIAN_POINT('Ctrl Pts',(18.6371727618945,21.7705500459129,-18.7618863040899));
#45951=CARTESIAN_POINT('Ctrl Pts',(18.7213521918226,21.7723487605766,-18.7660558700333));
#45952=CARTESIAN_POINT('Ctrl Pts',(18.8053875689174,21.7700044577929,-18.7702254359767));
#45953=CARTESIAN_POINT('Ctrl Pts',(18.8923775262288,21.7675777322146,-18.7745415987164));
#45954=CARTESIAN_POINT('Ctrl Pts',(18.9792125852182,21.7607112463061,-18.778857761456));
#45955=CARTESIAN_POINT('Ctrl Pts',(19.0654100827151,21.7494576728941,-18.7831739241956));
#45956=CARTESIAN_POINT('Ctrl Pts',(19.1487997057715,21.7385706834556,-18.7873494883867));
#45957=CARTESIAN_POINT('Ctrl Pts',(19.2315922114994,21.7235781663988,-18.7915250525778));
#45958=CARTESIAN_POINT('Ctrl Pts',(19.3133609024084,21.7045799455322,-18.7957006167688));
#45959=CARTESIAN_POINT('Ctrl Pts',(19.3992595355479,21.6846221696845,-18.8000870787827));
#45960=CARTESIAN_POINT('Ctrl Pts',(19.4840276488775,21.6602435606427,-18.8044735407967));
#45961=CARTESIAN_POINT('Ctrl Pts',(19.5671906913808,21.6316183655827,-18.8088600028106));
#45962=CARTESIAN_POINT('Ctrl Pts',(19.6503537338841,21.6029931705227,-18.8132464648245));
#45963=CARTESIAN_POINT('Ctrl Pts',(19.7319111958455,21.5701216768946,-18.8176329268384));
#45964=CARTESIAN_POINT('Ctrl Pts',(19.8114169849415,21.5332344068934,-18.8220193888523));
#45965=CARTESIAN_POINT('Ctrl Pts',(19.8872706217464,21.4980415786326,-18.8262043557616));
#45966=CARTESIAN_POINT('Ctrl Pts',(19.9615393050008,21.4590628106808,-18.8303893226708));
#45967=CARTESIAN_POINT('Ctrl Pts',(20.0338195953317,21.4164634478022,-18.8345742895801));
#45968=CARTESIAN_POINT('Ctrl Pts',(20.1059885648699,21.3739296933326,-18.8387528111108));
#45969=CARTESIAN_POINT('Ctrl Pts',(20.1761748342838,21.327786657028,-18.8429313326415));
#45970=CARTESIAN_POINT('Ctrl Pts',(20.2439967783601,21.2782468960775,-18.8471098541722));
#45971=CARTESIAN_POINT('Ctrl Pts',(20.2606541302848,21.2660797244687,-18.8481361164625));
#45972=CARTESIAN_POINT('Ctrl Pts',(20.2771689741761,21.2537078773064,-18.8491623787528));
#45973=CARTESIAN_POINT('Ctrl Pts',(20.2935358855687,21.2411349269503,-18.8501886410431));
#45974=CARTESIAN_POINT('Ctrl Pts',(20.2935358855687,21.2411349269503,-18.0500683201495));
#45975=CARTESIAN_POINT('Ctrl Pts',(20.3406388660272,21.2049507367435,-18.0530337296876));
#45976=CARTESIAN_POINT('Ctrl Pts',(20.3864285990884,21.1671673046285,-18.0559991392257));
#45977=CARTESIAN_POINT('Ctrl Pts',(20.4307957154104,21.1278944415812,-18.0589645487637));
#45978=CARTESIAN_POINT('Ctrl Pts',(20.4934043225861,21.0724745842854,-18.0631491831568));
#45979=CARTESIAN_POINT('Ctrl Pts',(20.5534114448285,21.0138810328615,-18.0673338175499));
#45980=CARTESIAN_POINT('Ctrl Pts',(20.6104778947951,20.9523875818856,-18.071518451943));
#45981=CARTESIAN_POINT('Ctrl Pts',(20.6674631177336,20.8909816592258,-18.0756971300271));
#45982=CARTESIAN_POINT('Ctrl Pts',(20.7215156722283,20.8266843701416,-18.0798758081111));
#45983=CARTESIAN_POINT('Ctrl Pts',(20.7723306651573,20.7598086064712,-18.0840544861951));
#45984=CARTESIAN_POINT('Ctrl Pts',(20.8240564803136,20.691734142801,-18.0883080640805));
#45985=CARTESIAN_POINT('Ctrl Pts',(20.8724271646772,20.620988176579,-18.0925616419659));
#45986=CARTESIAN_POINT('Ctrl Pts',(20.91716165977,20.5479387298267,-18.0968152198513));
#45987=CARTESIAN_POINT('Ctrl Pts',(20.9610288893839,20.4763054891426,-18.1009863338293));
#45988=CARTESIAN_POINT('Ctrl Pts',(21.0013994094997,20.4024576962096,-18.1051574478073));
#45989=CARTESIAN_POINT('Ctrl Pts',(21.0380509604127,20.326772903337,-18.1093285617853));
#45990=CARTESIAN_POINT('Ctrl Pts',(21.0746902125439,20.2511135072277,-18.1134982761058));
#45991=CARTESIAN_POINT('Ctrl Pts',(21.1076127735552,20.1736187490991,-18.1176679904262));
#45992=CARTESIAN_POINT('Ctrl Pts',(21.136642647489,20.0946901654241,-18.1218377047466));
#45993=CARTESIAN_POINT('Ctrl Pts',(21.1656714884152,20.0157643903668,-18.1260072706907));
#45994=CARTESIAN_POINT('Ctrl Pts',(21.1908077596747,19.9354053232572,-18.1301768366348));
#45995=CARTESIAN_POINT('Ctrl Pts',(21.211924363067,19.8540325426593,-18.1343464025789));
#45996=CARTESIAN_POINT('Ctrl Pts',(21.2337834001838,19.7697987954824,-18.1386625653178));
#45997=CARTESIAN_POINT('Ctrl Pts',(21.2513347146947,19.6844792346864,-18.1429787280566));
#45998=CARTESIAN_POINT('Ctrl Pts',(21.2644946836059,19.5985521335796,-18.1472948907955));
#45999=CARTESIAN_POINT('Ctrl Pts',(21.2772259679144,19.5154240987509,-18.1514704549872));
#46000=CARTESIAN_POINT('Ctrl Pts',(21.2858476079666,19.4317279704215,-18.1556460191789));
#46001=CARTESIAN_POINT('Ctrl Pts',(21.290336834896,19.3479013752814,-18.1598215833707));
#46002=CARTESIAN_POINT('Ctrl Pts',(21.2950528020053,19.2598408981036,-18.1642080453831));
#46003=CARTESIAN_POINT('Ctrl Pts',(21.295207927637,19.1716370118692,-18.1685945073955));
#46004=CARTESIAN_POINT('Ctrl Pts',(21.2908376238657,19.083794004918,-18.1729809694079));
#46005=CARTESIAN_POINT('Ctrl Pts',(21.2864673200944,18.9959509979668,-18.1773674314203));
#46006=CARTESIAN_POINT('Ctrl Pts',(21.2775717212916,18.9084694398441,-18.1817538934327));
#46007=CARTESIAN_POINT('Ctrl Pts',(21.2642482087237,18.8218419315364,-18.1861403554451));
#46008=CARTESIAN_POINT('Ctrl Pts',(21.251537730719,18.7392002832971,-18.1903249898381));
#46009=CARTESIAN_POINT('Ctrl Pts',(21.2347505437474,18.6570282117551,-18.194509624231));
#46010=CARTESIAN_POINT('Ctrl Pts',(21.2139332700432,18.5757591195989,-18.198694258624));
#46011=CARTESIAN_POINT('Ctrl Pts',(21.1931456271515,18.4946057039364,-18.2028729367079));
#46012=CARTESIAN_POINT('Ctrl Pts',(21.1683394048595,18.4143531565236,-18.2070516147918));
#46013=CARTESIAN_POINT('Ctrl Pts',(21.1396126628228,18.3354272066433,-18.2112302928757));
#46014=CARTESIAN_POINT('Ctrl Pts',(21.1103710145802,18.2550865658331,-18.2154838707611));
#46015=CARTESIAN_POINT('Ctrl Pts',(21.0770669868029,18.1761210253964,-18.2197374486466));
#46016=CARTESIAN_POINT('Ctrl Pts',(21.0398578961466,18.098966114375,-18.223991026532));
#46017=CARTESIAN_POINT('Ctrl Pts',(21.0033701763209,18.0233070018604,-18.2281621405099));
#46018=CARTESIAN_POINT('Ctrl Pts',(20.9631276659834,17.9493893735374,-18.2323332544878));
#46019=CARTESIAN_POINT('Ctrl Pts',(20.9193275219149,17.8776044765482,-18.2365043684657));
#46020=CARTESIAN_POINT('Ctrl Pts',(20.8755420754078,17.8058436676746,-18.2406740827861));
#46021=CARTESIAN_POINT('Ctrl Pts',(20.8282016054844,17.7362145612029,-18.2448437971064));
#46022=CARTESIAN_POINT('Ctrl Pts',(20.7775484775,17.6690824859586,-18.2490135114267));
#46023=CARTESIAN_POINT('Ctrl Pts',(20.7268971519712,17.6019527995616,-18.2531830773707));
#46024=CARTESIAN_POINT('Ctrl Pts',(20.6729336805178,17.5373203344384,-18.2573526433147));
#46025=CARTESIAN_POINT('Ctrl Pts',(20.6159420664671,17.4755190699804,-18.2615222092586));
#46026=CARTESIAN_POINT('Ctrl Pts',(20.5569466975713,17.4115449493023,-18.2658383719976));
#46027=CARTESIAN_POINT('Ctrl Pts',(20.4947066427113,17.3506052113062,-18.2701545347366));
#46028=CARTESIAN_POINT('Ctrl Pts',(20.4295787905104,17.2930290499668,-18.2744706974756));
#46029=CARTESIAN_POINT('Ctrl Pts',(20.3665724712465,17.2373284260287,-18.2786462616672));
#46030=CARTESIAN_POINT('Ctrl Pts',(20.300864002761,17.1847758643075,-18.2828218258589));
#46031=CARTESIAN_POINT('Ctrl Pts',(20.2328090354887,17.1356273888438,-18.2869973900505));
#46032=CARTESIAN_POINT('Ctrl Pts',(20.1613167736019,17.0839965407216,-18.2913838520632));
#46033=CARTESIAN_POINT('Ctrl Pts',(20.0872352304045,17.0361230139113,-18.2957703140758));
#46034=CARTESIAN_POINT('Ctrl Pts',(20.0110076004693,16.9922499941761,-18.3001567760885));
#46035=CARTESIAN_POINT('Ctrl Pts',(19.9347799705342,16.9483769744409,-18.3045432381012));
#46036=CARTESIAN_POINT('Ctrl Pts',(19.8564068054917,16.9085046570797,-18.3089297001138));
#46037=CARTESIAN_POINT('Ctrl Pts',(19.7763550154481,16.8728177954295,-18.3133161621265));
#46038=CARTESIAN_POINT('Ctrl Pts',(19.6999865269337,16.8387729391862,-18.3175007965194));
#46039=CARTESIAN_POINT('Ctrl Pts',(19.6218062328668,16.8084101229908,-18.3216854309124));
#46040=CARTESIAN_POINT('Ctrl Pts',(19.5422037920521,16.7819247375776,-18.3258700653053));
#46041=CARTESIAN_POINT('Ctrl Pts',(19.4627146554591,16.7554770508322,-18.3300487433892));
#46042=CARTESIAN_POINT('Ctrl Pts',(19.3818078256876,16.7328959763056,-18.334227421473));
#46043=CARTESIAN_POINT('Ctrl Pts',(19.2998943515232,16.7143295005319,-18.3384060995568));
#46044=CARTESIAN_POINT('Ctrl Pts',(19.2165126372019,16.6954302340229,-18.3426596774423));
#46045=CARTESIAN_POINT('Ctrl Pts',(19.1320882756871,16.6806911015683,-18.3469132553277));
#46046=CARTESIAN_POINT('Ctrl Pts',(19.0470726305013,16.6702155683665,-18.3511668332132));
#46047=CARTESIAN_POINT('Ctrl Pts',(18.9637051794946,16.6599431238176,-18.3553379471911));
#46048=CARTESIAN_POINT('Ctrl Pts',(18.8797696442083,16.6537704962434,-18.3595090611689));
#46049=CARTESIAN_POINT('Ctrl Pts',(18.795701718799,16.6517436826497,-18.3636801751467));
#46050=CARTESIAN_POINT('Ctrl Pts',(18.711662003194,16.649717549173,-18.367849889467));
#46051=CARTESIAN_POINT('Ctrl Pts',(18.6274904452109,16.6518344778738,-18.3720196037873));
#46052=CARTESIAN_POINT('Ctrl Pts',(18.5436254163474,16.6580884234077,-18.3761893181075));
#46053=CARTESIAN_POINT('Ctrl Pts',(18.4597633717615,16.6643421463994,-18.3803588840515));
#46054=CARTESIAN_POINT('Ctrl Pts',(18.3762082933037,16.6747325584671,-18.3845284499954));
#46055=CARTESIAN_POINT('Ctrl Pts',(18.2933947304034,16.6892016344672,-18.3886980159393));
#46056=CARTESIAN_POINT('Ctrl Pts',(18.2076695447882,16.7041794253309,-18.3930141786784));
#46057=CARTESIAN_POINT('Ctrl Pts',(18.122739507835,16.7235279374021,-18.3973303414174));
#46058=CARTESIAN_POINT('Ctrl Pts',(18.0390745966233,16.7471252702823,-18.4016465041565));
#46059=CARTESIAN_POINT('Ctrl Pts',(17.958135061099,16.7699539225246,-18.405822068348));
#46060=CARTESIAN_POINT('Ctrl Pts',(17.8783799255841,16.7967586410081,-18.4099976325396));
#46061=CARTESIAN_POINT('Ctrl Pts',(17.8002169726149,16.8273789609572,-18.4141731967312));
#46062=CARTESIAN_POINT('Ctrl Pts',(17.7181061946991,16.8595458404768,-18.418559658744));
#46063=CARTESIAN_POINT('Ctrl Pts',(17.6377532005338,16.895923662579,-18.4229461207568));
#46064=CARTESIAN_POINT('Ctrl Pts',(17.5596023636775,16.9362714026064,-18.4273325827696));
#46065=CARTESIAN_POINT('Ctrl Pts',(17.4814515268212,16.9766191426339,-18.4317190447824));
#46066=CARTESIAN_POINT('Ctrl Pts',(17.4055033100763,17.0209364424643,-18.4361055067952));
#46067=CARTESIAN_POINT('Ctrl Pts',(17.3321657913463,17.0689307080656,-18.4404919688079));
#46068=CARTESIAN_POINT('Ctrl Pts',(17.2622960528831,17.1146555545476,-18.4446710160258));
#46069=CARTESIAN_POINT('Ctrl Pts',(17.19453408493,17.1638887348098,-18.4488500632436));
#46070=CARTESIAN_POINT('Ctrl Pts',(17.1292545139166,17.2164093339998,-18.4530291104615));
#46071=CARTESIAN_POINT('Ctrl Pts',(17.0640679209106,17.2688551278475,-18.4572022054423));
#46072=CARTESIAN_POINT('Ctrl Pts',(17.0013570587502,17.3245787540421,-18.461375300423));
#46073=CARTESIAN_POINT('Ctrl Pts',(16.9414683281886,17.3833156165374,-18.4655483954038));
#46074=CARTESIAN_POINT('Ctrl Pts',(16.8809773183909,17.4426431743496,-18.4697634576868));
#46075=CARTESIAN_POINT('Ctrl Pts',(16.8233659292104,17.5050446643084,-18.4739785199699));
#46076=CARTESIAN_POINT('Ctrl Pts',(16.7689574885197,17.5702050926227,-18.4781935822529));
#46077=CARTESIAN_POINT('Ctrl Pts',(16.7151877112471,17.6346006473008,-18.4823591668069));
#46078=CARTESIAN_POINT('Ctrl Pts',(16.6645463875622,17.701690347722,-18.4865247513609));
#46079=CARTESIAN_POINT('Ctrl Pts',(16.6173078768048,17.7711338758054,-18.4906903359149));
#46080=CARTESIAN_POINT('Ctrl Pts',(16.5700850499658,17.84055434756,-18.4948545374302));
#46081=CARTESIAN_POINT('Ctrl Pts',(16.5262630517187,17.9123267137652,-18.4990187389455));
#46082=CARTESIAN_POINT('Ctrl Pts',(16.4860739671285,17.9860801859963,-18.5031829404608));
#46083=CARTESIAN_POINT('Ctrl Pts',(16.4458860826637,18.0598314558034,-18.5073470176248));
#46084=CARTESIAN_POINT('Ctrl Pts',(16.4093311160891,18.1355633083681,-18.5115110947889));
#46085=CARTESIAN_POINT('Ctrl Pts',(16.3765953977375,18.2128799965778,-18.5156751719529));
#46086=CARTESIAN_POINT('Ctrl Pts',(16.3431614559388,18.2918457802489,-18.5199280651398));
#46087=CARTESIAN_POINT('Ctrl Pts',(16.3137117771032,18.3724643312945,-18.5241809583268));
#46088=CARTESIAN_POINT('Ctrl Pts',(16.2883925214927,18.4542939401133,-18.5284338515138));
#46089=CARTESIAN_POINT('Ctrl Pts',(16.2635663208298,18.534530038676,-18.5326039259141));
#46090=CARTESIAN_POINT('Ctrl Pts',(16.2427111716314,18.6159299801766,-18.5367740003144));
#46091=CARTESIAN_POINT('Ctrl Pts',(16.2259135016088,18.6980651926532,-18.5409440747148));
#46092=CARTESIAN_POINT('Ctrl Pts',(16.2086154222953,18.7826472458752,-18.545238377295));
#46093=CARTESIAN_POINT('Ctrl Pts',(16.1956204803926,18.8680085473305,-18.5495326798753));
#46094=CARTESIAN_POINT('Ctrl Pts',(16.1869656326132,18.9536754357807,-18.5538269824556));
#46095=CARTESIAN_POINT('Ctrl Pts',(16.1783107848339,19.0393423242308,-18.5581212850358));
#46096=CARTESIAN_POINT('Ctrl Pts',(16.1739959871027,19.125314270194,-18.5624155876161));
#46097=CARTESIAN_POINT('Ctrl Pts',(16.1740000028035,19.2111198080496,-18.5667098901964));
#46098=CARTESIAN_POINT('Origin',(18.734,19.211,1.76670989022852));
#46099=CARTESIAN_POINT('',(20.2917780654113,21.2388105542775,-17.2500265414872));
#46100=CARTESIAN_POINT('',(20.2944552762682,21.2423103685662,-17.3168007019908));
#46101=CARTESIAN_POINT('',(20.2935358855687,21.2411349269503,1.76670989022852));
#46102=CARTESIAN_POINT('',(16.1740010840393,19.2086440968075,-17.8332901097715));
#46103=CARTESIAN_POINT('Ctrl Pts',(20.2944552762683,21.2423103685662,-17.3168007019908));
#46104=CARTESIAN_POINT('Ctrl Pts',(20.8466207046277,20.8094281841944,-17.3517574544833));
#46105=CARTESIAN_POINT('Ctrl Pts',(21.6812137731847,19.3312716956158,-17.4291061425363));
#46106=CARTESIAN_POINT('Ctrl Pts',(20.5976437728566,16.8256022375524,-17.5488467661498));
#46107=CARTESIAN_POINT('Ctrl Pts',(17.7370130066076,16.3527999488813,-17.6760225728312));
#46108=CARTESIAN_POINT('Ctrl Pts',(16.286227466659,17.9552740380232,-17.7708370079901));
#46109=CARTESIAN_POINT('Ctrl Pts',(16.1722336618266,19.0070072559387,-17.8232595075886));
#46110=CARTESIAN_POINT('Ctrl Pts',(16.1740883584118,19.2086434103328,-17.8332900716265));
#46111=CARTESIAN_POINT('Ctrl Pts',(16.1740010840393,19.2086440968075,-17.8332901097715));
#46112=CARTESIAN_POINT('Ctrl Pts',(16.1739248258781,19.2915086264566,-17.837412174938));
#46113=CARTESIAN_POINT('Ctrl Pts',(16.177876160498,19.3744847533445,-17.8415342401044));
#46114=CARTESIAN_POINT('Ctrl Pts',(16.1858608731257,19.4571442465142,-17.8456563052709));
#46115=CARTESIAN_POINT('Ctrl Pts',(16.1938402258665,19.5397482529614,-17.8497756034244));
#46116=CARTESIAN_POINT('Ctrl Pts',(16.205847540348,19.6220355783689,-17.853894901578));
#46117=CARTESIAN_POINT('Ctrl Pts',(16.2218365582967,19.7035797825425,-17.8580141997315));
#46118=CARTESIAN_POINT('Ctrl Pts',(16.2378199266111,19.7850951735058,-17.862132042353));
#46119=CARTESIAN_POINT('Ctrl Pts',(16.2577821151893,19.8658675009388,-17.8662498849745));
#46120=CARTESIAN_POINT('Ctrl Pts',(16.2816254461127,19.9454787590162,-17.8703677275959));
#46121=CARTESIAN_POINT('Ctrl Pts',(16.3054679320359,20.0250871956956,-17.8744854242824));
#46122=CARTESIAN_POINT('Ctrl Pts',(16.3331911499574,20.1035341923719,-17.8786031209688));
#46123=CARTESIAN_POINT('Ctrl Pts',(16.364647494651,20.1804166830608,-17.8827208176552));
#46124=CARTESIAN_POINT('Ctrl Pts',(16.396133878009,20.257372591286,-17.8868424464612));
#46125=CARTESIAN_POINT('Ctrl Pts',(16.4313603282317,20.3327605713697,-17.8909640752672));
#46126=CARTESIAN_POINT('Ctrl Pts',(16.4701312380089,20.4061979871474,-17.8950857040732));
#46127=CARTESIAN_POINT('Ctrl Pts',(16.5089205032735,20.479670170733,-17.8992092842006));
#46128=CARTESIAN_POINT('Ctrl Pts',(16.5512573267502,20.5511895451374,-17.903332864328));
#46129=CARTESIAN_POINT('Ctrl Pts',(16.5969016205558,20.6204007650689,-17.9074564444553));
#46130=CARTESIAN_POINT('Ctrl Pts',(16.6426258760309,20.6897332322415,-17.9115872484507));
#46131=CARTESIAN_POINT('Ctrl Pts',(16.6916688941171,20.7567490876318,-17.915718052446));
#46132=CARTESIAN_POINT('Ctrl Pts',(16.743749207993,20.8211247730892,-17.9198488564413));
#46133=CARTESIAN_POINT('Ctrl Pts',(16.7879829276106,20.8758014024869,-17.9233572996922));
#46134=CARTESIAN_POINT('Ctrl Pts',(16.8344068718463,20.9285739549632,-17.9268657429432));
#46135=CARTESIAN_POINT('Ctrl Pts',(16.8828286089276,20.979265953095,-17.9303741861941));
#46136=CARTESIAN_POINT('Ctrl Pts',(16.9405827898753,21.039727948248,-17.9345588205871));
#46137=CARTESIAN_POINT('Ctrl Pts',(17.0014097311532,21.0974699797563,-17.9387434549801));
#46138=CARTESIAN_POINT('Ctrl Pts',(17.0650229727701,21.152163486824,-17.9429280893731));
#46139=CARTESIAN_POINT('Ctrl Pts',(17.1285456688113,21.2067791444541,-17.947106767457));
#46140=CARTESIAN_POINT('Ctrl Pts',(17.1948464417153,21.2583545993042,-17.9512854455409));
#46141=CARTESIAN_POINT('Ctrl Pts',(17.2636010628233,21.3065970427421,-17.9554641236248));
#46142=CARTESIAN_POINT('Ctrl Pts',(17.3335880611026,21.3557041973082,-17.9597177015102));
#46143=CARTESIAN_POINT('Ctrl Pts',(17.4061174102899,21.4013573280785,-17.9639712793957));
#46144=CARTESIAN_POINT('Ctrl Pts',(17.4808106950311,21.4432895345164,-17.9682248572811));
#46145=CARTESIAN_POINT('Ctrl Pts',(17.5540559046944,21.4844088033079,-17.972395971259));
#46146=CARTESIAN_POINT('Ctrl Pts',(17.6293814748144,21.5219498994727,-17.9765670852369));
#46147=CARTESIAN_POINT('Ctrl Pts',(17.7064016963161,21.555705040355,-17.9807381992148));
#46148=CARTESIAN_POINT('Ctrl Pts',(17.7833960729386,21.5894488543737,-17.9849079135351));
#46149=CARTESIAN_POINT('Ctrl Pts',(17.8620835505881,21.6194090516659,-17.9890776278554));
#46150=CARTESIAN_POINT('Ctrl Pts',(17.9420562076474,21.6454249895518,-17.9932473421757));
#46151=CARTESIAN_POINT('Ctrl Pts',(18.0220260189365,21.671440001679,-17.9974169081197));
#46152=CARTESIAN_POINT('Ctrl Pts',(18.1032804809775,21.6935108919569,-18.0015864740637));
#46153=CARTESIAN_POINT('Ctrl Pts',(18.1853954972943,21.7115265644682,-18.0057560400077));
#46154=CARTESIAN_POINT('Ctrl Pts',(18.2703975762873,21.7301756458007,-18.0100722027467));
#46155=CARTESIAN_POINT('Ctrl Pts',(18.3563213344854,21.7444789277004,-18.0143883654857));
#46156=CARTESIAN_POINT('Ctrl Pts',(18.4426856715115,21.7543709839536,-18.0187045282247));
#46157=CARTESIAN_POINT('Ctrl Pts',(18.5262366993405,21.7639408075146,-18.0228800924163));
#46158=CARTESIAN_POINT('Ctrl Pts',(18.6101995699749,21.7693824000208,-18.0270556566079));
#46159=CARTESIAN_POINT('Ctrl Pts',(18.6941361080732,21.7706896042529,-18.0312312207995));
#46160=CARTESIAN_POINT('Ctrl Pts',(18.7823120811743,21.7720628322632,-18.0356176828122));
#46161=CARTESIAN_POINT('Ctrl Pts',(18.870458408217,21.7688730610124,-18.0400041448249));
#46162=CARTESIAN_POINT('Ctrl Pts',(18.9580725064404,21.7611748002554,-18.0443906068375));
#46163=CARTESIAN_POINT('Ctrl Pts',(19.0456866046639,21.7534765394983,-18.0487770688502));
#46164=CARTESIAN_POINT('Ctrl Pts',(19.132767910028,21.7412699451077,-18.0531635308629));
#46165=CARTESIAN_POINT('Ctrl Pts',(19.2188278686568,21.7246710082614,-18.0575499928755));
#46166=CARTESIAN_POINT('Ctrl Pts',(19.3009320014004,21.7088350569554,-18.06173482709));
#46167=CARTESIAN_POINT('Ctrl Pts',(19.3824122424305,21.6889427479766,-18.0659196613044));
#46168=CARTESIAN_POINT('Ctrl Pts',(19.4628372070827,21.665057115385,-18.0701044955188));
#46169=CARTESIAN_POINT('Ctrl Pts',(19.5431287709647,21.641211101857,-18.0742823883549));
#46170=CARTESIAN_POINT('Ctrl Pts',(19.6223681012689,21.6133850633112,-18.078460281191));
#46171=CARTESIAN_POINT('Ctrl Pts',(19.7001337305628,21.5816930663139,-18.0826381740271));
#46172=CARTESIAN_POINT('Ctrl Pts',(19.7778242916652,21.5500316620208,-18.0868120338879));
#46173=CARTESIAN_POINT('Ctrl Pts',(19.8540435523394,21.5145118803042,-18.0909858937488));
#46174=CARTESIAN_POINT('Ctrl Pts',(19.928385767927,21.4752973827158,-18.0951597536096));
#46175=CARTESIAN_POINT('Ctrl Pts',(20.0026788000519,21.4361088287284,-18.0993308521204));
#46176=CARTESIAN_POINT('Ctrl Pts',(20.0750968472972,21.3932306267545,-18.1035019506312));
#46177=CARTESIAN_POINT('Ctrl Pts',(20.145255958728,21.3468737366602,-18.1076730491419));
#46178=CARTESIAN_POINT('Ctrl Pts',(20.1959047149762,21.3134081071941,-18.1106842182895));
#46179=CARTESIAN_POINT('Ctrl Pts',(20.2453766303622,21.2781305402564,-18.113695387437));
#46180=CARTESIAN_POINT('Ctrl Pts',(20.2935358855687,21.2411349269503,-18.1167065565846));
#46181=CARTESIAN_POINT('',(16.1740009581142,19.2132148462219,-17.7667099127475));
#46182=CARTESIAN_POINT('Ctrl Pts',(16.1740009581142,19.2132148462218,-17.7667099127475));
#46183=CARTESIAN_POINT('Ctrl Pts',(16.1740887027227,19.3146332252549,-17.7717442924629));
#46184=CARTESIAN_POINT('Ctrl Pts',(16.1802070184511,19.4157876786429,-17.7767786721782));
#46185=CARTESIAN_POINT('Ctrl Pts',(16.1922394471755,19.5160463769745,-17.7818130518935));
#46186=CARTESIAN_POINT('Ctrl Pts',(16.2044426849033,19.6177283198346,-17.7869188982596));
#46187=CARTESIAN_POINT('Ctrl Pts',(16.2227290670649,19.71848890314,-17.7920247446257));
#46188=CARTESIAN_POINT('Ctrl Pts',(16.2469282568518,19.8176911441861,-17.7971305909918));
#46189=CARTESIAN_POINT('Ctrl Pts',(16.2587491290717,19.8661496680319,-17.7996247057948));
#46190=CARTESIAN_POINT('Ctrl Pts',(16.2719801580739,19.9142366801005,-17.8021188205978));
#46191=CARTESIAN_POINT('Ctrl Pts',(16.2865973915759,19.9618797988219,-17.8046129354008));
#46192=CARTESIAN_POINT('Ctrl Pts',(16.3111222362101,20.0418155872439,-17.8087975697939));
#46193=CARTESIAN_POINT('Ctrl Pts',(16.3396130703746,20.1206973427815,-17.8129822041869));
#46194=CARTESIAN_POINT('Ctrl Pts',(16.3719611025222,20.1981029565358,-17.8171668385799));
#46195=CARTESIAN_POINT('Ctrl Pts',(16.4042630912499,20.2753983929799,-17.8213455166639));
#46196=CARTESIAN_POINT('Ctrl Pts',(16.440411196743,20.351221440268,-17.8255241947478));
#46197=CARTESIAN_POINT('Ctrl Pts',(16.480246839823,20.4251650188471,-17.8297028728317));
#46198=CARTESIAN_POINT('Ctrl Pts',(16.5207965081758,20.5004339829301,-17.8339564507172));
#46199=CARTESIAN_POINT('Ctrl Pts',(16.5651670712162,20.5737549756816,-17.8382100286026));
#46200=CARTESIAN_POINT('Ctrl Pts',(16.6131398985284,20.6447197878197,-17.8424636064881));
#46201=CARTESIAN_POINT('Ctrl Pts',(16.6601826789718,20.7143088085979,-17.846634720466));
#46202=CARTESIAN_POINT('Ctrl Pts',(16.7106890267626,20.7816317931436,-17.8508058344439));
#46203=CARTESIAN_POINT('Ctrl Pts',(16.7644072919754,20.8463301087231,-17.8549769484219));
#46204=CARTESIAN_POINT('Ctrl Pts',(16.8181075315056,20.911006714158,-17.8591466627423));
#46205=CARTESIAN_POINT('Ctrl Pts',(16.8750172543249,20.9730600461346,-17.8633163770626));
#46206=CARTESIAN_POINT('Ctrl Pts',(16.9348438240379,21.032163653958,-17.867486091383));
#46207=CARTESIAN_POINT('Ctrl Pts',(16.9946682648648,21.0912651586214,-17.871655657327));
#46208=CARTESIAN_POINT('Ctrl Pts',(17.0574090183537,21.1474168251239,-17.8758252232711));
#46209=CARTESIAN_POINT('Ctrl Pts',(17.1227367799309,21.2003292426475,-17.8799947892151));
#46210=CARTESIAN_POINT('Ctrl Pts',(17.1903613850148,21.2551019954968,-17.884310951954));
#46211=CARTESIAN_POINT('Ctrl Pts',(17.2607578915088,21.3064031452813,-17.888627114693));
#46212=CARTESIAN_POINT('Ctrl Pts',(17.3335255671369,21.3539585537049,-17.8929432774319));
#46213=CARTESIAN_POINT('Ctrl Pts',(17.4039228433852,21.3999648497008,-17.8971188416236));
#46214=CARTESIAN_POINT('Ctrl Pts',(17.4765387490621,21.4424654946023,-17.9012944058152));
#46215=CARTESIAN_POINT('Ctrl Pts',(17.5509843556047,21.4812585723032,-17.9054699700069));
#46216=CARTESIAN_POINT('Ctrl Pts',(17.6291900327564,21.522010996137,-17.9098564320195));
#46217=CARTESIAN_POINT('Ctrl Pts',(17.7094145736835,21.558671228602,-17.914242894032));
#46218=CARTESIAN_POINT('Ctrl Pts',(17.7911842815276,21.5910627136698,-17.9186293560446));
#46219=CARTESIAN_POINT('Ctrl Pts',(17.8729539893717,21.6234541987376,-17.9230158180571));
#46220=CARTESIAN_POINT('Ctrl Pts',(17.9562682900626,21.6515768229132,-17.9274022800697));
#46221=CARTESIAN_POINT('Ctrl Pts',(18.0406384682269,21.6753152773656,-17.9317887420822));
#46222=CARTESIAN_POINT('Ctrl Pts',(18.1211305077813,21.697962575929,-17.9359735770737));
#46223=CARTESIAN_POINT('Ctrl Pts',(18.2028831083919,21.7167042021064,-17.9401584120652));
#46224=CARTESIAN_POINT('Ctrl Pts',(18.285482396511,21.7314031342943,-17.9443432470566));
#46225=CARTESIAN_POINT('Ctrl Pts',(18.3679630513101,21.7460809551243,-17.9485220715741));
#46226=CARTESIAN_POINT('Ctrl Pts',(18.4512875288659,21.756727535889,-17.9527008960917));
#46227=CARTESIAN_POINT('Ctrl Pts',(18.5350276579567,21.7632558663076,-17.9568797206092));
#46228=CARTESIAN_POINT('Ctrl Pts',(18.6186666109275,21.7697763090965,-17.9610534962063));
#46229=CARTESIAN_POINT('Ctrl Pts',(18.7027197607572,21.7721883584651,-17.9652272718034));
#46230=CARTESIAN_POINT('Ctrl Pts',(18.7867510727816,21.7704564509521,-17.9694010474004));
#46231=CARTESIAN_POINT('Ctrl Pts',(18.8707269523644,21.7687256859164,-17.9735720697075));
#46232=CARTESIAN_POINT('Ctrl Pts',(18.9546805641743,21.7628564016082,-17.9777430920145));
#46233=CARTESIAN_POINT('Ctrl Pts',(19.0381741527011,21.7528650799813,-17.9819141143216));
#46234=CARTESIAN_POINT('Ctrl Pts',(19.1216377101411,21.7428773520466,-17.9860836363897));
#46235=CARTESIAN_POINT('Ctrl Pts',(19.2046411167496,21.7287705870409,-17.9902531584578));
#46236=CARTESIAN_POINT('Ctrl Pts',(19.2867513915052,21.7106131499072,-17.9944226805259));
#46237=CARTESIAN_POINT('Ctrl Pts',(19.3688567634635,21.6924567969525,-17.9985919536323));
#46238=CARTESIAN_POINT('Ctrl Pts',(19.4500686609559,21.6702503538458,-18.0027612267386));
#46239=CARTESIAN_POINT('Ctrl Pts',(19.5299652993015,21.6441130763505,-18.0069304998449));
#46240=CARTESIAN_POINT('Ctrl Pts',(19.6099224331149,21.6179560084503,-18.0111029298065));
#46241=CARTESIAN_POINT('Ctrl Pts',(19.6885618814567,21.5878623064593,-18.0152753597681));
#46242=CARTESIAN_POINT('Ctrl Pts',(19.7654786756144,21.5540005850944,-18.0194477897297));
#46243=CARTESIAN_POINT('Ctrl Pts',(19.84242841653,21.5201243593037,-18.0236220069219));
#46244=CARTESIAN_POINT('Ctrl Pts',(19.9176536212634,21.4824771037163,-18.027796224114));
#46245=CARTESIAN_POINT('Ctrl Pts',(19.9907728936446,21.4412739503927,-18.0319704413061));
#46246=CARTESIAN_POINT('Ctrl Pts',(20.0639908538862,21.4000151858614,-18.0361502923694));
#46247=CARTESIAN_POINT('Ctrl Pts',(20.1350968176442,21.3551911864424,-18.0403301434327));
#46248=CARTESIAN_POINT('Ctrl Pts',(20.2037378785227,21.3070607263234,-18.0445099944961));
#46249=CARTESIAN_POINT('Ctrl Pts',(20.2341639522258,21.2857262523482,-18.0463627697139));
#46250=CARTESIAN_POINT('Ctrl Pts',(20.2641061444964,21.2637426544939,-18.0482155449317));
#46251=CARTESIAN_POINT('Ctrl Pts',(20.2935358855687,21.2411349269503,-18.0500683201495));
#46252=CARTESIAN_POINT('Ctrl Pts',(20.2917780654112,21.2388105542776,-17.2500265414872));
#46253=CARTESIAN_POINT('Ctrl Pts',(20.5375805895458,21.0526898515823,-17.2653209305498));
#46254=CARTESIAN_POINT('Ctrl Pts',(21.3400060558233,20.1920438331041,-17.3230072551729));
#46255=CARTESIAN_POINT('Ctrl Pts',(21.4691813416985,17.9140516551704,-17.4230855153565));
#46256=CARTESIAN_POINT('Ctrl Pts',(19.1239734719678,16.2091318029775,-17.550261322038));
#46257=CARTESIAN_POINT('Ctrl Pts',(16.6895185666654,17.1540155201862,-17.6648027803286));
#46258=CARTESIAN_POINT('Ctrl Pts',(16.1805385807744,18.6141143559075,-17.7369523030588));
#46259=CARTESIAN_POINT('Ctrl Pts',(16.1756125809373,19.2132129985223,-17.7667098902285));
#46260=CARTESIAN_POINT('Origin',(18.734,19.211,1.76670989022852));
#46261=CARTESIAN_POINT('',(20.2935358855687,21.2411349269503,-16.4501666916289));
#46262=CARTESIAN_POINT('',(20.2935358855687,21.2411349269503,-16.5166303570915));
#46263=CARTESIAN_POINT('',(20.2935358855687,21.2411349269503,1.76670989022852));
#46264=CARTESIAN_POINT('',(16.1737370555978,19.211835565301,-17.0332901097715));
#46265=CARTESIAN_POINT('Ctrl Pts',(20.2935358855687,21.2411349269503,-16.5166303570915));
#46266=CARTESIAN_POINT('Ctrl Pts',(20.36010259041,21.1899988356463,-16.5208151874521));
#46267=CARTESIAN_POINT('Ctrl Pts',(20.4240566305495,21.1356583062745,-16.5250000178127));
#46268=CARTESIAN_POINT('Ctrl Pts',(20.4850922765871,21.078424921885,-16.5291848481734));
#46269=CARTESIAN_POINT('Ctrl Pts',(20.4960575744632,21.0681427155182,-16.5299366696817));
#46270=CARTESIAN_POINT('Ctrl Pts',(20.5069287828259,21.0577672286989,-16.53068849119));
#46271=CARTESIAN_POINT('Ctrl Pts',(20.5177042670233,21.0473003806031,-16.5314403126983));
#46272=CARTESIAN_POINT('Ctrl Pts',(20.5776805529837,20.9890419614915,-16.5356249470914));
#46273=CARTESIAN_POINT('Ctrl Pts',(20.6349112416909,20.9277336646777,-16.5398095814844));
#46274=CARTESIAN_POINT('Ctrl Pts',(20.6890701824651,20.8636646912292,-16.5439942158775));
#46275=CARTESIAN_POINT('Ctrl Pts',(20.7431520346907,20.7996869120343,-16.5481728939614));
#46276=CARTESIAN_POINT('Ctrl Pts',(20.7941705292094,20.7329566097132,-16.5523515720454));
#46277=CARTESIAN_POINT('Ctrl Pts',(20.8418355824982,20.6638004533157,-16.5565302501293));
#46278=CARTESIAN_POINT('Ctrl Pts',(20.890354997611,20.5934047225164,-16.5607838280147));
#46279=CARTESIAN_POINT('Ctrl Pts',(20.9353992222982,20.5204956513051,-16.5650374059002));
#46280=CARTESIAN_POINT('Ctrl Pts',(20.9767045339426,20.4454538765922,-16.5692909837856));
#46281=CARTESIAN_POINT('Ctrl Pts',(21.01720906152,20.371866933114,-16.5734620977636));
#46282=CARTESIAN_POINT('Ctrl Pts',(21.0541181225501,20.2962296630072,-16.5776332117415));
#46283=CARTESIAN_POINT('Ctrl Pts',(21.0872271712958,20.2189295016395,-16.5818043257195));
#46284=CARTESIAN_POINT('Ctrl Pts',(21.1203251099804,20.1416552790874,-16.5859740400399));
#46285=CARTESIAN_POINT('Ctrl Pts',(21.149625387836,20.0627196959936,-16.5901437543602));
#46286=CARTESIAN_POINT('Ctrl Pts',(21.1749707834402,19.9825320047745,-16.5943134686806));
#46287=CARTESIAN_POINT('Ctrl Pts',(21.2003152771464,19.9023471669775,-16.5984830346247));
#46288=CARTESIAN_POINT('Ctrl Pts',(21.2217050305799,19.8209107485431,-16.6026526005687));
#46289=CARTESIAN_POINT('Ctrl Pts',(21.2390325027795,19.7386477613126,-16.6068221665128));
#46290=CARTESIAN_POINT('Ctrl Pts',(21.2569691875259,19.6534925089337,-16.6111383292517));
#46291=CARTESIAN_POINT('Ctrl Pts',(21.2705525077455,19.5674519980823,-16.6154544919906));
#46292=CARTESIAN_POINT('Ctrl Pts',(21.2797210678871,19.4810078600997,-16.6197706547295));
#46293=CARTESIAN_POINT('Ctrl Pts',(21.2885909631466,19.3973796308195,-16.6239462189212));
#46294=CARTESIAN_POINT('Ctrl Pts',(21.2933293236125,19.3133741398417,-16.6281217831129));
#46295=CARTESIAN_POINT('Ctrl Pts',(21.2939336612287,19.2294295987025,-16.6322973473046));
#46296=CARTESIAN_POINT('Ctrl Pts',(21.2945685225012,19.1412452183497,-16.6366838093171));
#46297=CARTESIAN_POINT('Ctrl Pts',(21.2906407927078,19.0531286901045,-16.6410702713296));
#46298=CARTESIAN_POINT('Ctrl Pts',(21.2822091879386,18.965582122686,-16.6454567333422));
#46299=CARTESIAN_POINT('Ctrl Pts',(21.2737775831694,18.8780355552674,-16.6498431953547));
#46300=CARTESIAN_POINT('Ctrl Pts',(21.2608422640145,18.7910595113906,-16.6542296573673));
#46301=CARTESIAN_POINT('Ctrl Pts',(21.2435233083642,18.7051415565825,-16.6586161193798));
#46302=CARTESIAN_POINT('Ctrl Pts',(21.2270012235363,18.6231768142361,-16.6628007537728));
#46303=CARTESIAN_POINT('Ctrl Pts',(21.2064285344955,18.5418698437248,-16.6669853881659));
#46304=CARTESIAN_POINT('Ctrl Pts',(21.1818718743958,18.4616514252084,-16.6711700225589));
#46305=CARTESIAN_POINT('Ctrl Pts',(21.1573501676622,18.3815471876817,-16.6753487006429));
#46306=CARTESIAN_POINT('Ctrl Pts',(21.1288558871502,18.3025288606373,-16.6795273787268));
#46307=CARTESIAN_POINT('Ctrl Pts',(21.0965066931249,18.2250171781719,-16.6837060568108));
#46308=CARTESIAN_POINT('Ctrl Pts',(21.0635776630457,18.146116154505,-16.6879596346962));
#46309=CARTESIAN_POINT('Ctrl Pts',(21.0266542567595,18.0687767925293,-16.6922132125816));
#46310=CARTESIAN_POINT('Ctrl Pts',(20.9859137816201,17.9934268727713,-16.6964667904671));
#46311=CARTESIAN_POINT('Ctrl Pts',(20.9459631400899,17.9195377582412,-16.700637904445));
#46312=CARTESIAN_POINT('Ctrl Pts',(20.9023423404875,17.847562059166,-16.704809018423));
#46313=CARTESIAN_POINT('Ctrl Pts',(20.8552664379162,17.7778814775567,-16.7089801324009));
#46314=CARTESIAN_POINT('Ctrl Pts',(20.8082063321188,17.7082242779395,-16.7131498467213));
#46315=CARTESIAN_POINT('Ctrl Pts',(20.7576936832433,17.6408610471354,-16.7173195610417));
#46316=CARTESIAN_POINT('Ctrl Pts',(20.7039875068324,17.5761455040511,-16.721489275362));
#46317=CARTESIAN_POINT('Ctrl Pts',(20.6502832415178,17.5114322638236,-16.7256588413061));
#46318=CARTESIAN_POINT('Ctrl Pts',(20.5933859690518,17.4493668774532,-16.7298284072501));
#46319=CARTESIAN_POINT('Ctrl Pts',(20.5335948472512,17.3902698207184,-16.7339979731942));
#46320=CARTESIAN_POINT('Ctrl Pts',(20.4717015433684,17.3290949843729,-16.7383141359331));
#46321=CARTESIAN_POINT('Ctrl Pts',(20.4067074835552,17.2711014650386,-16.742630298672));
#46322=CARTESIAN_POINT('Ctrl Pts',(20.3389844113023,17.2166015845683,-16.7469464614109));
#46323=CARTESIAN_POINT('Ctrl Pts',(20.273467411005,17.1638770319719,-16.7511220256026));
#46324=CARTESIAN_POINT('Ctrl Pts',(20.2053968718999,17.1144222417057,-16.7552975897943));
#46325=CARTESIAN_POINT('Ctrl Pts',(20.135139913803,17.0684765014245,-16.759473153986));
#46326=CARTESIAN_POINT('Ctrl Pts',(20.0613344437726,17.0202101510273,-16.7638596159985));
#46327=CARTESIAN_POINT('Ctrl Pts',(19.9851163826193,16.9758169447297,-16.7682460780111));
#46328=CARTESIAN_POINT('Ctrl Pts',(19.9069397062212,16.9355192935185,-16.7726325400236));
#46329=CARTESIAN_POINT('Ctrl Pts',(19.8287630298231,16.8952216423072,-16.7770190020362));
#46330=CARTESIAN_POINT('Ctrl Pts',(19.7486282982591,16.8590197157384,-16.7814054640487));
#46331=CARTESIAN_POINT('Ctrl Pts',(19.6670104728629,16.8270764572814,-16.7857919260613));
#46332=CARTESIAN_POINT('Ctrl Pts',(19.5891480046,16.7966029554973,-16.7899765604543));
#46333=CARTESIAN_POINT('Ctrl Pts',(19.5096461031212,16.7698914102528,-16.7941611948473));
#46334=CARTESIAN_POINT('Ctrl Pts',(19.4289030536308,16.7471189667408,-16.7983458292404));
#46335=CARTESIAN_POINT('Ctrl Pts',(19.3482749318773,16.7243789369834,-16.8025245073243));
#46336=CARTESIAN_POINT('Ctrl Pts',(19.2664096101499,16.7055669958483,-16.8067031854083));
#46337=CARTESIAN_POINT('Ctrl Pts',(19.1837245465113,16.6908119450594,-16.8108818634922));
#46338=CARTESIAN_POINT('Ctrl Pts',(19.0995574125317,16.6757924205894,-16.8151354413777));
#46339=CARTESIAN_POINT('Ctrl Pts',(19.0145413088147,16.66497683224,-16.8193890192631));
#46340=CARTESIAN_POINT('Ctrl Pts',(18.929131904193,16.6584476420716,-16.8236425971485));
#46341=CARTESIAN_POINT('Ctrl Pts',(18.8453783275426,16.6520450329952,-16.8278137111265));
#46342=CARTESIAN_POINT('Ctrl Pts',(18.7612470435307,16.6497641415373,-16.8319848251044));
#46343=CARTESIAN_POINT('Ctrl Pts',(18.6771754083917,16.6516307484483,-16.8361559390824));
#46344=CARTESIAN_POINT('Ctrl Pts',(18.5931319843018,16.6534967290012,-16.8403256534028));
#46345=CARTESIAN_POINT('Ctrl Pts',(18.5091486288698,16.659507433716,-16.8444953677231));
#46346=CARTESIAN_POINT('Ctrl Pts',(18.4256629639197,16.6696365328467,-16.8486650820435));
#46347=CARTESIAN_POINT('Ctrl Pts',(18.3421802697478,16.6797652715406,-16.8528346479875));
#46348=CARTESIAN_POINT('Ctrl Pts',(18.259195687427,16.6940120570168,-16.8570042139316));
#46349=CARTESIAN_POINT('Ctrl Pts',(18.1771406148227,16.7122988123547,-16.8611737798756));
#46350=CARTESIAN_POINT('Ctrl Pts',(18.0922005870916,16.7312285074512,-16.8654899426145));
#46351=CARTESIAN_POINT('Ctrl Pts',(18.008257163138,16.7544874341396,-16.8698061053534));
#46352=CARTESIAN_POINT('Ctrl Pts',(17.9257741739149,16.781932068869,-16.8741222680924));
#46353=CARTESIAN_POINT('Ctrl Pts',(17.8459780593899,16.8084826975088,-16.878297832284));
#46354=CARTESIAN_POINT('Ctrl Pts',(17.7675491154086,16.838950308513,-16.8824733964757));
#46355=CARTESIAN_POINT('Ctrl Pts',(17.690887260014,16.8731557340835,-16.8866489606674));
#46356=CARTESIAN_POINT('Ctrl Pts',(17.6103533965496,16.9090887943838,-16.8910354226799));
#46357=CARTESIAN_POINT('Ctrl Pts',(17.5317703445184,16.9491469214588,-16.8954218846925));
#46358=CARTESIAN_POINT('Ctrl Pts',(17.4555708448952,16.9930687802869,-16.899808346705));
#46359=CARTESIAN_POINT('Ctrl Pts',(17.3793713452719,17.0369906391151,-16.9041948087175));
#46360=CARTESIAN_POINT('Ctrl Pts',(17.3055558437866,17.0847758505362,-16.9085812707301));
#46361=CARTESIAN_POINT('Ctrl Pts',(17.2345184376722,17.1361132454423,-16.9129677327426));
#46362=CARTESIAN_POINT('Ctrl Pts',(17.167299168743,17.1846913445463,-16.9171184300414));
#46363=CARTESIAN_POINT('Ctrl Pts',(17.1023079512147,17.2366370916662,-16.9212691273401));
#46364=CARTESIAN_POINT('Ctrl Pts',(17.0399060592653,17.2917173944502,-16.9254198246388));
#46365=CARTESIAN_POINT('Ctrl Pts',(16.9775932241692,17.3467190893861,-16.9295645982704));
#46366=CARTESIAN_POINT('Ctrl Pts',(16.9178627255451,17.4048461509352,-16.9337093719019));
#46367=CARTESIAN_POINT('Ctrl Pts',(16.8610458812396,17.4658229691466,-16.9378541455334));
#46368=CARTESIAN_POINT('Ctrl Pts',(16.8042942087153,17.5267298438772,-16.9419941649009));
#46369=CARTESIAN_POINT('Ctrl Pts',(16.7504498675423,17.5904796396564,-16.9461341842684));
#46370=CARTESIAN_POINT('Ctrl Pts',(16.6998090154256,17.6567583719781,-16.9502742036359));
#46371=CARTESIAN_POINT('Ctrl Pts',(16.6491995836851,17.7229959813207,-16.9544116543072));
#46372=CARTESIAN_POINT('Ctrl Pts',(16.6017899801563,17.7917590422704,-16.9585491049784));
#46373=CARTESIAN_POINT('Ctrl Pts',(16.5578367768805,17.8626997269368,-16.9626865556497));
#46374=CARTESIAN_POINT('Ctrl Pts',(16.5138971231854,17.9336185425139,-16.9668227308571));
#46375=CARTESIAN_POINT('Ctrl Pts',(16.473412000563,18.0067132510728,-16.9709589060645));
#46376=CARTESIAN_POINT('Ctrl Pts',(16.436594403761,18.0816074524907,-16.9750950812719));
#46377=CARTESIAN_POINT('Ctrl Pts',(16.3997766632185,18.1565019463048,-16.9792312726275));
#46378=CARTESIAN_POINT('Ctrl Pts',(16.3666266817619,18.2331955257885,-16.983367463983));
#46379=CARTESIAN_POINT('Ctrl Pts',(16.3373106052885,18.3112889656799,-16.9875036553386));
#46380=CARTESIAN_POINT('Ctrl Pts',(16.3079666664254,18.3894566266172,-16.9916437777855));
#46381=CARTESIAN_POINT('Ctrl Pts',(16.2824640727846,18.4690263650884,-16.9957839002324));
#46382=CARTESIAN_POINT('Ctrl Pts',(16.2609198329123,18.5495814584111,-16.9999240226793));
#46383=CARTESIAN_POINT('Ctrl Pts',(16.2393648184701,18.6301768384414,-17.0040662156583));
#46384=CARTESIAN_POINT('Ctrl Pts',(16.2217721969232,18.711758096276,-17.0082084086373));
#46385=CARTESIAN_POINT('Ctrl Pts',(16.2082078057625,18.7938983438913,-17.0123506016163));
#46386=CARTESIAN_POINT('Ctrl Pts',(16.194621013815,18.8761742412484,-17.016499635181));
#46387=CARTESIAN_POINT('Ctrl Pts',(16.1850757885661,18.9590105062903,-17.0206486687458));
#46388=CARTESIAN_POINT('Ctrl Pts',(16.1795860271471,19.0419755778186,-17.0247977023105));
#46389=CARTESIAN_POINT('Ctrl Pts',(16.1758404729028,19.0985809841505,-17.0276285047975));
#46390=CARTESIAN_POINT('Ctrl Pts',(16.1739816679355,19.1552463005709,-17.0304593072845));
#46391=CARTESIAN_POINT('Ctrl Pts',(16.1740001363332,19.2118354794422,-17.0332901097715));
#46392=CARTESIAN_POINT('Ctrl Pts',(16.1700998775752,19.2118367523274,-17.0332901097715));
#46393=CARTESIAN_POINT('Ctrl Pts',(16.1699051698649,19.2575742435185,-17.0355745863224));
#46394=CARTESIAN_POINT('Ctrl Pts',(16.1917620114795,20.1518505208751,-17.0802509984337));
#46395=CARTESIAN_POINT('Ctrl Pts',(17.2348044634258,21.8407724883182,-17.1673193461055));
#46396=CARTESIAN_POINT('Ctrl Pts',(19.336908367695,21.880117833012,-17.2595384002944));
#46397=CARTESIAN_POINT('Ctrl Pts',(20.1770115565028,21.3343829456268,-17.3093655189228));
#46398=CARTESIAN_POINT('Ctrl Pts',(20.2944552762683,21.2423103685662,-17.3168007019908));
#46399=CARTESIAN_POINT('',(16.1741505176752,19.209803254934,-16.9667098397549));
#46400=CARTESIAN_POINT('Ctrl Pts',(16.1776746320478,19.209805920766,-16.9667098902285));
#46401=CARTESIAN_POINT('Ctrl Pts',(16.1797896414426,19.7131225343252,-16.9916592919231));
#46402=CARTESIAN_POINT('Ctrl Pts',(16.5671403882425,21.07463612297,-17.0590006291781));
#46403=CARTESIAN_POINT('Ctrl Pts',(18.4733994225959,22.0756037013586,-17.153439512931));
#46404=CARTESIAN_POINT('Ctrl Pts',(19.8562820609774,21.5685664127725,-17.2229289949893));
#46405=CARTESIAN_POINT('Ctrl Pts',(20.2917780654112,21.2388105542776,-17.2500265414872));
#46406=CARTESIAN_POINT('Ctrl Pts',(20.2935358855687,21.2411349269503,-16.4501666916289));
#46407=CARTESIAN_POINT('Ctrl Pts',(20.3601794036991,21.1899398281984,-16.4543369074164));
#46408=CARTESIAN_POINT('Ctrl Pts',(20.424336074523,21.1354315300474,-16.4585071232039));
#46409=CARTESIAN_POINT('Ctrl Pts',(20.4856659995229,21.0778867737802,-16.4626773389914));
#46410=CARTESIAN_POINT('Ctrl Pts',(20.5469851014509,21.0203521726051,-16.4668468188487));
#46411=CARTESIAN_POINT('Ctrl Pts',(20.6054781133613,20.9597824927492,-16.471016298706));
#46412=CARTESIAN_POINT('Ctrl Pts',(20.6608402875572,20.8964929564512,-16.4751857785632));
#46413=CARTESIAN_POINT('Ctrl Pts',(20.7162092989616,20.8331956039182,-16.4793557733498));
#46414=CARTESIAN_POINT('Ctrl Pts',(20.7684464030089,20.7671780750758,-16.4835257681363));
#46415=CARTESIAN_POINT('Ctrl Pts',(20.8172865168588,20.6987893966131,-16.4876957629229));
#46416=CARTESIAN_POINT('Ctrl Pts',(20.8661791232192,20.6303272151803,-16.4918702395478));
#46417=CARTESIAN_POINT('Ctrl Pts',(20.911667183017,20.5594891716793,-16.4960447161727));
#46418=CARTESIAN_POINT('Ctrl Pts',(20.9535287381871,20.4866536286788,-16.5002191927976));
#46419=CARTESIAN_POINT('Ctrl Pts',(20.9954147198633,20.413775585637,-16.5043961052584));
#46420=CARTESIAN_POINT('Ctrl Pts',(21.0336697749439,20.3388981323474,-16.5085730177192));
#46421=CARTESIAN_POINT('Ctrl Pts',(21.068118859428,20.2624224412968,-16.5127499301799));
#46422=CARTESIAN_POINT('Ctrl Pts',(21.1026261826924,20.185817462312,-16.5169339040268));
#46423=CARTESIAN_POINT('Ctrl Pts',(21.1333145201899,20.107609278805,-16.5211178778737));
#46424=CARTESIAN_POINT('Ctrl Pts',(21.1600578409485,20.0282168331431,-16.5253018517207));
#46425=CARTESIAN_POINT('Ctrl Pts',(21.1761504170598,19.9804430736308,-16.5278195240093));
#46426=CARTESIAN_POINT('Ctrl Pts',(21.1908155024365,19.9322407738411,-16.5303371962979));
#46427=CARTESIAN_POINT('Ctrl Pts',(21.2040345704695,19.8837029215676,-16.5328548685865));
#46428=CARTESIAN_POINT('Ctrl Pts',(21.2260060426842,19.8030279397969,-16.5370395029795));
#46429=CARTESIAN_POINT('Ctrl Pts',(21.244061800264,19.7211252621464,-16.5412241373726));
#46430=CARTESIAN_POINT('Ctrl Pts',(21.2580683099057,19.6384098348539,-16.5454087717656));
#46431=CARTESIAN_POINT('Ctrl Pts',(21.2720548830146,19.555812142734,-16.5495874498496));
#46432=CARTESIAN_POINT('Ctrl Pts',(21.2820035803663,19.4724044485338,-16.5537661279335));
#46433=CARTESIAN_POINT('Ctrl Pts',(21.28783098536,19.3886155911377,-16.5579448060175));
#46434=CARTESIAN_POINT('Ctrl Pts',(21.2937628424001,19.3033248786908,-16.5621983839029));
#46435=CARTESIAN_POINT('Ctrl Pts',(21.2954240788116,19.2176396691377,-16.5664519617883));
#46436=CARTESIAN_POINT('Ctrl Pts',(21.2927814384536,19.1320218370346,-16.5707055396738));
#46437=CARTESIAN_POINT('Ctrl Pts',(21.2901900308356,19.0480638736762,-16.5748766536517));
#46438=CARTESIAN_POINT('Ctrl Pts',(21.2834601502021,18.9641711795843,-16.5790477676297));
#46439=CARTESIAN_POINT('Ctrl Pts',(21.2726129381323,18.8807813597822,-16.5832188816076));
#46440=CARTESIAN_POINT('Ctrl Pts',(21.2617693659493,18.7974195222394,-16.587388595928));
#46441=CARTESIAN_POINT('Ctrl Pts',(21.246811265521,18.7145606796674,-16.5915583102484));
#46442=CARTESIAN_POINT('Ctrl Pts',(21.2278116184524,18.6326371280314,-16.5957280245688));
#46443=CARTESIAN_POINT('Ctrl Pts',(21.2088126474729,18.550716491587,-16.5998975905128));
#46444=CARTESIAN_POINT('Ctrl Pts',(21.1857725205575,18.4697315278524,-16.6040671564568));
#46445=CARTESIAN_POINT('Ctrl Pts',(21.1588150040535,18.3901028102636,-16.6082367224009));
#46446=CARTESIAN_POINT('Ctrl Pts',(21.1309096945249,18.3076744451972,-16.6125528851398));
#46447=CARTESIAN_POINT('Ctrl Pts',(21.0988065683011,18.2266999715501,-16.6168690478787));
#46448=CARTESIAN_POINT('Ctrl Pts',(21.0626979316573,18.1476252104291,-16.6211852106176));
#46449=CARTESIAN_POINT('Ctrl Pts',(21.0277655300542,18.0711263013344,-16.6253607748093));
#46450=CARTESIAN_POINT('Ctrl Pts',(20.9890848280186,17.9964056357567,-16.629536339001));
#46451=CARTESIAN_POINT('Ctrl Pts',(20.9468767362673,17.9238416763711,-16.6337119031927));
#46452=CARTESIAN_POINT('Ctrl Pts',(20.9025368141418,17.8476126839013,-16.6380983652052));
#46453=CARTESIAN_POINT('Ctrl Pts',(20.854304119971,17.7737644826752,-16.6424848272178));
#46454=CARTESIAN_POINT('Ctrl Pts',(20.8024847707862,17.702699382409,-16.6468712892303));
#46455=CARTESIAN_POINT('Ctrl Pts',(20.7506654216015,17.6316342821428,-16.6512577512428));
#46456=CARTESIAN_POINT('Ctrl Pts',(20.6952598420585,17.5633526854596,-16.6556442132554));
#46457=CARTESIAN_POINT('Ctrl Pts',(20.6366195645773,17.4982131503051,-16.6600306752679));
#46458=CARTESIAN_POINT('Ctrl Pts',(20.5806774131887,17.4360707817229,-16.664215309661));
#46459=CARTESIAN_POINT('Ctrl Pts',(20.5215834617877,17.3765563809788,-16.668399944054));
#46460=CARTESIAN_POINT('Ctrl Pts',(20.4596143354494,17.3200068309771,-16.6725845784471));
#46461=CARTESIAN_POINT('Ctrl Pts',(20.3977334144923,17.2635377722604,-16.676763256531));
#46462=CARTESIAN_POINT('Ctrl Pts',(20.3329857844083,17.2100254892845,-16.6809419346149));
#46463=CARTESIAN_POINT('Ctrl Pts',(20.26568687901,17.1597722445646,-16.6851206126989));
#46464=CARTESIAN_POINT('Ctrl Pts',(20.1971816890993,17.1086182465494,-16.6893741905843));
#46465=CARTESIAN_POINT('Ctrl Pts',(20.1260331836052,17.0608416308411,-16.6936277684697));
#46466=CARTESIAN_POINT('Ctrl Pts',(20.052611725018,17.0167203645284,-16.6978813463552));
#46467=CARTESIAN_POINT('Ctrl Pts',(19.9806136846756,16.9734544750588,-16.7020524603331));
#46468=CARTESIAN_POINT('Ctrl Pts',(19.9064304485064,16.9337037154837,-16.7062235743111));
#46469=CARTESIAN_POINT('Ctrl Pts',(19.8304414166181,16.89768717638,-16.710394688289));
#46470=CARTESIAN_POINT('Ctrl Pts',(19.7544778835833,16.8616827229739,-16.7145644026094));
#46471=CARTESIAN_POINT('Ctrl Pts',(19.6767101736173,16.8294101983214,-16.7187341169298));
#46472=CARTESIAN_POINT('Ctrl Pts',(19.5975412827732,16.8010422300492,-16.7229038312502));
#46473=CARTESIAN_POINT('Ctrl Pts',(19.518375209098,16.772675271231,-16.7270733971942));
#46474=CARTESIAN_POINT('Ctrl Pts',(19.4378084870369,16.7482127469195,-16.7312429631383));
#46475=CARTESIAN_POINT('Ctrl Pts',(19.3562617446687,16.7277782376272,-16.7354125290823));
#46476=CARTESIAN_POINT('Ctrl Pts',(19.2718479194376,16.7066252761968,-16.7397286918212));
#46477=CARTESIAN_POINT('Ctrl Pts',(19.1863843882477,16.6897889781384,-16.7440448545601));
#46478=CARTESIAN_POINT('Ctrl Pts',(19.1003501078363,16.6773489588169,-16.748361017299));
#46479=CARTESIAN_POINT('Ctrl Pts',(19.0171183850602,16.6653141718163,-16.7525365814907));
#46480=CARTESIAN_POINT('Ctrl Pts',(18.9333529997369,16.6573936417868,-16.7567121456824));
#46481=CARTESIAN_POINT('Ctrl Pts',(18.849491753864,16.6536064724432,-16.7608877098741));
#46482=CARTESIAN_POINT('Ctrl Pts',(18.761394875823,16.6496280221792,-16.7652741718866));
#46483=CARTESIAN_POINT('Ctrl Pts',(18.6731927827737,16.6502114543057,-16.7696606338992));
#46484=CARTESIAN_POINT('Ctrl Pts',(18.5853894488637,16.6553171354624,-16.7740470959117));
#46485=CARTESIAN_POINT('Ctrl Pts',(18.4975861149538,16.6604228166191,-16.7784335579242));
#46486=CARTESIAN_POINT('Ctrl Pts',(18.4101821085833,16.6700506076701,-16.7828200199368));
#46487=CARTESIAN_POINT('Ctrl Pts',(18.3236691980735,16.6840990060965,-16.7872064819493));
#46488=CARTESIAN_POINT('Ctrl Pts',(18.2411368748191,16.6975010168866,-16.7913911163424));
#46489=CARTESIAN_POINT('Ctrl Pts',(18.1591082470637,16.7149756618514,-16.7955757507354));
#46490=CARTESIAN_POINT('Ctrl Pts',(18.0780163119231,16.7364726914061,-16.7997603851285));
#46491=CARTESIAN_POINT('Ctrl Pts',(17.9970398011148,16.7579391226001,-16.8039390632124));
#46492=CARTESIAN_POINT('Ctrl Pts',(17.9169977755057,16.7834164491322,-16.8081177412964));
#46493=CARTESIAN_POINT('Ctrl Pts',(17.838315128377,16.8128030500508,-16.8122964193803));
#46494=CARTESIAN_POINT('Ctrl Pts',(17.7582221513469,16.8427163846711,-16.8165499972658));
#46495=CARTESIAN_POINT('Ctrl Pts',(17.6795382417638,16.8766804423688,-16.8208035751512));
#46496=CARTESIAN_POINT('Ctrl Pts',(17.6026975961515,16.9145342652139,-16.8250571530366));
#46497=CARTESIAN_POINT('Ctrl Pts',(17.5273466563965,16.9516542178375,-16.8292282670146));
#46498=CARTESIAN_POINT('Ctrl Pts',(17.453768579546,16.992514247479,-16.8333993809925));
#46499=CARTESIAN_POINT('Ctrl Pts',(17.3823529481855,17.0369139282629,-16.8375704949705));
#46500=CARTESIAN_POINT('Ctrl Pts',(17.31096128103,17.0812987103051,-16.8417402092909));
#46501=CARTESIAN_POINT('Ctrl Pts',(17.2417310086118,17.1292205418819,-16.8459099236112));
#46502=CARTESIAN_POINT('Ctrl Pts',(17.1750254175661,17.1804340071485,-16.8500796379316));
#46503=CARTESIAN_POINT('Ctrl Pts',(17.1083222001915,17.2316456500203,-16.8542492038757));
#46504=CARTESIAN_POINT('Ctrl Pts',(17.0441438499408,17.2861484128723,-16.8584187698197));
#46505=CARTESIAN_POINT('Ctrl Pts',(16.9828219564695,17.3436555058435,-16.8625883357637));
#46506=CARTESIAN_POINT('Ctrl Pts',(16.9193440608725,17.4031844772608,-16.8669044985027));
#46507=CARTESIAN_POINT('Ctrl Pts',(16.8589276101183,17.4659326132811,-16.8712206612416));
#46508=CARTESIAN_POINT('Ctrl Pts',(16.8018987983271,17.5315402813719,-16.8755368239805));
#46509=CARTESIAN_POINT('Ctrl Pts',(16.7467276940816,17.5950107865755,-16.8797123881722));
#46510=CARTESIAN_POINT('Ctrl Pts',(16.6947271674384,17.6611569867928,-16.8838879523639));
#46511=CARTESIAN_POINT('Ctrl Pts',(16.6461502555162,17.729621100306,-16.8880635165556));
#46512=CARTESIAN_POINT('Ctrl Pts',(16.5951198392535,17.8015431734345,-16.8924499785681));
#46513=CARTESIAN_POINT('Ctrl Pts',(16.5478682932593,17.8760229761494,-16.8968364405807));
#46514=CARTESIAN_POINT('Ctrl Pts',(16.5046350837971,17.952615293162,-16.9012229025932));
#46515=CARTESIAN_POINT('Ctrl Pts',(16.4614018743349,18.0292076101746,-16.9056093646057));
#46516=CARTESIAN_POINT('Ctrl Pts',(16.4221871920777,18.1079118882385,-16.9099958266183));
#46517=CARTESIAN_POINT('Ctrl Pts',(16.3871718743353,18.1882596866316,-16.9143822886308));
#46518=CARTESIAN_POINT('Ctrl Pts',(16.3503471043862,18.272759539339,-16.9189954255354));
#46519=CARTESIAN_POINT('Ctrl Pts',(16.3180481684135,18.3593459986726,-16.9236085624399));
#46520=CARTESIAN_POINT('Ctrl Pts',(16.2904920397068,18.4475415217682,-16.9282216993445));
#46521=CARTESIAN_POINT('Ctrl Pts',(16.2630147812854,18.5354846144106,-16.9328216326736));
#46522=CARTESIAN_POINT('Ctrl Pts',(16.240253377301,18.6250273148911,-16.9374215660027));
#46523=CARTESIAN_POINT('Ctrl Pts',(16.2223767943066,18.7156729639699,-16.9420214993319));
#46524=CARTESIAN_POINT('Ctrl Pts',(16.2045882581335,18.8058721596483,-16.9465987767929));
#46525=CARTESIAN_POINT('Ctrl Pts',(16.1916366671697,18.8971631896627,-16.9511760542538));
#46526=CARTESIAN_POINT('Ctrl Pts',(16.1836406660146,18.9890376888893,-16.9557533317148));
#46527=CARTESIAN_POINT('Ctrl Pts',(16.1772607284144,19.0623435277384,-16.9594055003442));
#46528=CARTESIAN_POINT('Ctrl Pts',(16.174034774907,19.1360203999197,-16.9630576689737));
#46529=CARTESIAN_POINT('Ctrl Pts',(16.1740002797795,19.2098031412859,-16.9667098376031));
#46530=CARTESIAN_POINT('Origin',(18.734,19.211,1.76670989022852));
#46531=CARTESIAN_POINT('',(20.2958871626529,21.2441650537926,-15.6501589834813));
#46532=CARTESIAN_POINT('',(20.2935358855687,21.2411349269503,-15.7166572087383));
#46533=CARTESIAN_POINT('',(20.2935358855687,21.2411349269503,1.76670989022852));
#46534=CARTESIAN_POINT('',(16.1740007055014,19.2129005700936,-16.2332901098004));
#46535=CARTESIAN_POINT('Ctrl Pts',(20.2935358855687,21.2411349269503,-15.7166572087383));
#46536=CARTESIAN_POINT('Ctrl Pts',(20.3624598532065,21.1881880023494,-15.7209678973943));
#46537=CARTESIAN_POINT('Ctrl Pts',(20.4286597734137,21.131746121533,-15.7252785860502));
#46538=CARTESIAN_POINT('Ctrl Pts',(20.4917771246324,21.0721339500743,-15.7295892747062));
#46539=CARTESIAN_POINT('Ctrl Pts',(20.5529161163786,21.0143902712218,-15.7337648485075));
#46540=CARTESIAN_POINT('Ctrl Pts',(20.6111626397197,20.9536724844389,-15.7379404223088));
#46541=CARTESIAN_POINT('Ctrl Pts',(20.6662297645119,20.8903118046195,-15.7421159961101));
#46542=CARTESIAN_POINT('Ctrl Pts',(20.7239697147345,20.8238757502104,-15.7464942421934));
#46543=CARTESIAN_POINT('Ctrl Pts',(20.7782134501061,20.7545341994174,-15.7508724882766));
#46544=CARTESIAN_POINT('Ctrl Pts',(20.8286804984858,20.6827043212763,-15.7552507343599));
#46545=CARTESIAN_POINT('Ctrl Pts',(20.8791475468655,20.6108744431352,-15.7596289804432));
#46546=CARTESIAN_POINT('Ctrl Pts',(20.9258376663792,20.5365567644941,-15.7640072265265));
#46547=CARTESIAN_POINT('Ctrl Pts',(20.968526025902,20.4601971179788,-15.7683854726097));
#46548=CARTESIAN_POINT('Ctrl Pts',(21.0093266510939,20.3872141935449,-15.7725701070028));
#46549=CARTESIAN_POINT('Ctrl Pts',(21.0466238491571,20.3120944357929,-15.7767547413958));
#46550=CARTESIAN_POINT('Ctrl Pts',(21.0801878476018,20.235208271674,-15.7809393757889));
#46551=CARTESIAN_POINT('Ctrl Pts',(21.1137040718491,20.1584315454932,-15.7851180538728));
#46552=CARTESIAN_POINT('Ctrl Pts',(21.1434974687763,20.0798938250633,-15.7892967319567));
#46553=CARTESIAN_POINT('Ctrl Pts',(21.1693835453414,19.9999911197727,-15.7934754100407));
#46554=CARTESIAN_POINT('Ctrl Pts',(21.195733611225,19.9186562159148,-15.7977289879261));
#46555=CARTESIAN_POINT('Ctrl Pts',(21.218034666248,19.8359073320104,-15.8019825658116));
#46556=CARTESIAN_POINT('Ctrl Pts',(21.2361429171342,19.7521846470801,-15.806236143697));
#46557=CARTESIAN_POINT('Ctrl Pts',(21.2539001042416,19.6700850897685,-15.8104072576749));
#46558=CARTESIAN_POINT('Ctrl Pts',(21.2676255061034,19.5870496228941,-15.8145783716529));
#46559=CARTESIAN_POINT('Ctrl Pts',(21.2772339776254,19.5035080085254,-15.8187494856308));
#46560=CARTESIAN_POINT('Ctrl Pts',(21.2868392249321,19.4199944273523,-15.8229191999512));
#46561=CARTESIAN_POINT('Ctrl Pts',(21.2923302330118,19.3359754926349,-15.8270889142716));
#46562=CARTESIAN_POINT('Ctrl Pts',(21.2936734448665,19.2518883314074,-15.8312586285919));
#46563=CARTESIAN_POINT('Ctrl Pts',(21.295016608924,19.1678041623622,-15.835428194536));
#46564=CARTESIAN_POINT('Ctrl Pts',(21.2922122637205,19.0836522316218,-15.83959776048));
#46565=CARTESIAN_POINT('Ctrl Pts',(21.2852789648471,18.9998705526723,-15.8437673264241));
#46566=CARTESIAN_POINT('Ctrl Pts',(21.2781018997384,18.9131432132467,-15.848083489163));
#46567=CARTESIAN_POINT('Ctrl Pts',(21.2665001742354,18.8268131717716,-15.8523996519019));
#46568=CARTESIAN_POINT('Ctrl Pts',(21.2505527597976,18.7413594915736,-15.8567158146408));
#46569=CARTESIAN_POINT('Ctrl Pts',(21.2351248307078,18.6586894560199,-15.8608913788325));
#46570=CARTESIAN_POINT('Ctrl Pts',(21.2156301415437,18.576840010886,-15.8650669430242));
#46571=CARTESIAN_POINT('Ctrl Pts',(21.1921916857821,18.4962317606722,-15.8692425072158));
#46572=CARTESIAN_POINT('Ctrl Pts',(21.1675694093397,18.4115521793681,-15.8736289692284));
#46573=CARTESIAN_POINT('Ctrl Pts',(21.138594688676,18.3282430251666,-15.8780154312409));
#46574=CARTESIAN_POINT('Ctrl Pts',(21.1054674445919,18.246768617374,-15.8824018932535));
#46575=CARTESIAN_POINT('Ctrl Pts',(21.0723402005078,18.1652942095814,-15.886788355266));
#46576=CARTESIAN_POINT('Ctrl Pts',(21.0350607478797,18.0856550414426,-15.8911748172785));
#46577=CARTESIAN_POINT('Ctrl Pts',(20.9938836431738,18.0082839406927,-15.8955612792911));
#46578=CARTESIAN_POINT('Ctrl Pts',(20.9546011580944,17.9344727989798,-15.8997459136841));
#46579=CARTESIAN_POINT('Ctrl Pts',(20.9116255956987,17.8624508577059,-15.9039305480772));
#46580=CARTESIAN_POINT('Ctrl Pts',(20.8651440549406,17.7926118242556,-15.9081151824702));
#46581=CARTESIAN_POINT('Ctrl Pts',(20.8187286749023,17.722872198025,-15.9122938605542));
#46582=CARTESIAN_POINT('Ctrl Pts',(20.7688174815647,17.6553096876334,-15.9164725386381));
#46583=CARTESIAN_POINT('Ctrl Pts',(20.7156435935689,17.5902937749033,-15.9206512167221));
#46584=CARTESIAN_POINT('Ctrl Pts',(20.6615166018463,17.5241124986637,-15.9249047946075));
#46585=CARTESIAN_POINT('Ctrl Pts',(20.6040090238884,17.4605704392069,-15.9291583724929));
#46586=CARTESIAN_POINT('Ctrl Pts',(20.5434131480187,17.4000267644779,-15.9334119503784));
#46587=CARTESIAN_POINT('Ctrl Pts',(20.4839920414458,17.3406568470248,-15.9375830643563));
#46588=CARTESIAN_POINT('Ctrl Pts',(20.4216016541568,17.2841704328241,-15.9417541783343));
#46589=CARTESIAN_POINT('Ctrl Pts',(20.3565572606157,17.2308717374818,-15.9459252923122));
#46590=CARTESIAN_POINT('Ctrl Pts',(20.291534693349,17.1775909270315,-15.9500950066326));
#46591=CARTESIAN_POINT('Ctrl Pts',(20.2238602440646,17.1274960023899,-15.954264720953));
#46592=CARTESIAN_POINT('Ctrl Pts',(20.153883303655,17.0808517882547,-15.9584344352734));
#46593=CARTESIAN_POINT('Ctrl Pts',(20.0839088533252,17.0342092339207,-15.9626040012174));
#46594=CARTESIAN_POINT('Ctrl Pts',(20.0116324580342,16.9910174003974,-15.9667735671615));
#46595=CARTESIAN_POINT('Ctrl Pts',(19.9374324615958,16.9514977737614,-15.9709431331055));
#46596=CARTESIAN_POINT('Ctrl Pts',(19.8606236848184,16.9105886858056,-15.9752592958444));
#46597=CARTESIAN_POINT('Ctrl Pts',(19.7817539879923,16.8736150868689,-15.9795754585834));
#46598=CARTESIAN_POINT('Ctrl Pts',(19.7012689333153,16.8407698823441,-15.9838916213223));
#46599=CARTESIAN_POINT('Ctrl Pts',(19.623405670829,16.808994606902,-15.988067185514));
#46600=CARTESIAN_POINT('Ctrl Pts',(19.5440311349285,16.7810830031342,-15.9922427497056));
#46601=CARTESIAN_POINT('Ctrl Pts',(19.4635655614727,16.7571593182293,-15.9964183138973));
#46602=CARTESIAN_POINT('Ctrl Pts',(19.3790358631902,16.7320273048729,-16.0008047759099));
#46603=CARTESIAN_POINT('Ctrl Pts',(19.2933025817199,16.711296794516,-16.0051912379224));
#46604=CARTESIAN_POINT('Ctrl Pts',(19.206864349456,16.6950510126369,-16.009577699935));
#46605=CARTESIAN_POINT('Ctrl Pts',(19.120426117192,16.6788052307578,-16.0139641619475));
#46606=CARTESIAN_POINT('Ctrl Pts',(19.0332835193118,16.6670441795795,-16.01835062396));
#46607=CARTESIAN_POINT('Ctrl Pts',(18.9459382820314,16.6597880988421,-16.0227370859726));
#46608=CARTESIAN_POINT('Ctrl Pts',(18.8626119285951,16.6528658811356,-16.0269217203656));
#46609=CARTESIAN_POINT('Ctrl Pts',(18.7787910168743,16.6500174172728,-16.0311063547587));
#46610=CARTESIAN_POINT('Ctrl Pts',(18.6949078655891,16.6512984929826,-16.0352909891517));
#46611=CARTESIAN_POINT('Ctrl Pts',(18.6111441115869,16.6525777452396,-16.0394696672357));
#46612=CARTESIAN_POINT('Ctrl Pts',(18.5273187500335,16.6579748547684,-16.0436483453196));
#46613=CARTESIAN_POINT('Ctrl Pts',(18.4438686393691,16.6674937991862,-16.0478270234036));
#46614=CARTESIAN_POINT('Ctrl Pts',(18.3589227454458,16.6771833638415,-16.052080601289));
#46615=CARTESIAN_POINT('Ctrl Pts',(18.2743661679605,16.6911440245191,-16.0563341791744));
#46616=CARTESIAN_POINT('Ctrl Pts',(18.1906591204412,16.7093244237911,-16.0605877570599));
#46617=CARTESIAN_POINT('Ctrl Pts',(18.1085748973787,16.7271523605471,-16.0647588710378));
#46618=CARTESIAN_POINT('Ctrl Pts',(18.0273080288925,16.749037778107,-16.0689299850158));
#46619=CARTESIAN_POINT('Ctrl Pts',(17.9472849642517,16.7748802466776,-16.0731010989937));
#46620=CARTESIAN_POINT('Ctrl Pts',(17.8672887521232,16.8007140435583,-16.0772708133141));
#46621=CARTESIAN_POINT('Ctrl Pts',(17.7885359523433,16.8305021131095,-16.0814405276345));
#46622=CARTESIAN_POINT('Ctrl Pts',(17.7114383592365,16.8640940174692,-16.0856102419549));
#46623=CARTESIAN_POINT('Ctrl Pts',(17.6343435095929,16.8976847264847,-16.0897798078989));
#46624=CARTESIAN_POINT('Ctrl Pts',(17.5589041709149,16.9350788166486,-16.0939493738429));
#46625=CARTESIAN_POINT('Ctrl Pts',(17.4855113682728,16.9760780469001,-16.098118939787));
#46626=CARTESIAN_POINT('Ctrl Pts',(17.4095381652295,17.0185187595092,-16.1024351025259));
#46627=CARTESIAN_POINT('Ctrl Pts',(17.3357585487129,17.0648225852952,-16.1067512652648));
#46628=CARTESIAN_POINT('Ctrl Pts',(17.264575895997,17.1147192929918,-16.1110674280038));
#46629=CARTESIAN_POINT('Ctrl Pts',(17.1957120107061,17.1629906206834,-16.1152429921954));
#46630=CARTESIAN_POINT('Ctrl Pts',(17.1292788382185,17.2146240223491,-16.1194185563871));
#46631=CARTESIAN_POINT('Ctrl Pts',(17.0656083164572,17.2693333987821,-16.1235941205788));
#46632=CARTESIAN_POINT('Ctrl Pts',(16.9987219480042,17.3268060157593,-16.1279805825913));
#46633=CARTESIAN_POINT('Ctrl Pts',(16.9348850702689,17.3876731058188,-16.1323670446039));
#46634=CARTESIAN_POINT('Ctrl Pts',(16.8744375629656,17.4515604464004,-16.1367535066164));
#46635=CARTESIAN_POINT('Ctrl Pts',(16.8139900556624,17.515447786982,-16.141139968629));
#46636=CARTESIAN_POINT('Ctrl Pts',(16.7569322374058,17.5823548872471,-16.1455264306415));
#46637=CARTESIAN_POINT('Ctrl Pts',(16.703552701499,17.6518708302357,-16.149912892654));
#46638=CARTESIAN_POINT('Ctrl Pts',(16.652554439824,17.7182856499019,-16.1541036735168));
#46639=CARTESIAN_POINT('Ctrl Pts',(16.6047208600205,17.7873320135743,-16.1582944543796));
#46640=CARTESIAN_POINT('Ctrl Pts',(16.5603345705064,17.8586765917043,-16.1624852352424));
#46641=CARTESIAN_POINT('Ctrl Pts',(16.5160108372518,17.9299206196422,-16.1666701097864));
#46642=CARTESIAN_POINT('Ctrl Pts',(16.4751249866853,18.0034560458725,-16.1708549843304));
#46643=CARTESIAN_POINT('Ctrl Pts',(16.4379187528239,18.0789174471946,-16.1750398588744));
#46644=CARTESIAN_POINT('Ctrl Pts',(16.4007539244062,18.15429487031,-16.1792200762261));
#46645=CARTESIAN_POINT('Ctrl Pts',(16.367260780246,18.2315936031771,-16.1834002935778));
#46646=CARTESIAN_POINT('Ctrl Pts',(16.3376364602561,18.3104214163183,-16.1875805109295));
#46647=CARTESIAN_POINT('Ctrl Pts',(16.3080359860438,18.3891857778597,-16.1917573634602));
#46648=CARTESIAN_POINT('Ctrl Pts',(16.2822983085872,18.4694763469326,-16.1959342159909));
#46649=CARTESIAN_POINT('Ctrl Pts',(16.2605729619713,18.5508797931071,-16.2001110685216));
#46650=CARTESIAN_POINT('Ctrl Pts',(16.238858101653,18.632243947813,-16.2042859049869));
#46651=CARTESIAN_POINT('Ctrl Pts',(16.2211518401951,18.7147194701818,-16.2084607414522));
#46652=CARTESIAN_POINT('Ctrl Pts',(16.2075538451844,18.7978779516685,-16.2126355779176));
#46653=CARTESIAN_POINT('Ctrl Pts',(16.1939550163504,18.8810415323988,-16.2168106703821));
#46654=CARTESIAN_POINT('Ctrl Pts',(16.1844650395064,18.964887705472,-16.2209857628467));
#46655=CARTESIAN_POINT('Ctrl Pts',(16.1791322578277,19.048978951962,-16.2251608553112));
#46656=CARTESIAN_POINT('Ctrl Pts',(16.1756711337435,19.1035565169223,-16.227870606798));
#46657=CARTESIAN_POINT('Ctrl Pts',(16.1739601228212,19.158237148325,-16.2305803582847));
#46658=CARTESIAN_POINT('Ctrl Pts',(16.174000705501,19.2129005695108,-16.2332901097715));
#46659=CARTESIAN_POINT('Ctrl Pts',(16.1740007055014,19.2129005700936,-16.2332901098004));
#46660=CARTESIAN_POINT('Ctrl Pts',(16.1740727513108,19.3099436741144,-16.2381006886061));
#46661=CARTESIAN_POINT('Ctrl Pts',(16.1796667621362,19.4067618611662,-16.2429112674118));
#46662=CARTESIAN_POINT('Ctrl Pts',(16.1906824963736,19.5027808693996,-16.2477218462175));
#46663=CARTESIAN_POINT('Ctrl Pts',(16.201890345519,19.6004744535201,-16.2526163217372));
#46664=CARTESIAN_POINT('Ctrl Pts',(16.218710639996,19.6973405506009,-16.2575107972568));
#46665=CARTESIAN_POINT('Ctrl Pts',(16.2409867483461,19.7927945746377,-16.2624052727765));
#46666=CARTESIAN_POINT('Ctrl Pts',(16.2632628566961,19.8882485986746,-16.2672997482961));
#46667=CARTESIAN_POINT('Ctrl Pts',(16.2909946214077,19.9822904288897,-16.2721942238158));
#46668=CARTESIAN_POINT('Ctrl Pts',(16.3239764935689,20.074357804418,-16.2770886993355));
#46669=CARTESIAN_POINT('Ctrl Pts',(16.3521750361989,20.1530727360925,-16.2812733337285));
#46670=CARTESIAN_POINT('Ctrl Pts',(16.3842865295797,20.2305511910394,-16.2854579681216));
#46671=CARTESIAN_POINT('Ctrl Pts',(16.4201827606335,20.3063765484118,-16.2896426025146));
#46672=CARTESIAN_POINT('Ctrl Pts',(16.4560278978456,20.3820939777733,-16.2938212805986));
#46673=CARTESIAN_POINT('Ctrl Pts',(16.4956468770878,20.4561625710813,-16.2979999586825));
#46674=CARTESIAN_POINT('Ctrl Pts',(16.5388624466769,20.5281830252439,-16.3021786367664));
#46675=CARTESIAN_POINT('Ctrl Pts',(16.5828526242924,20.6014943942872,-16.3064322146519));
#46676=CARTESIAN_POINT('Ctrl Pts',(16.6305694356436,20.6726830222909,-16.3106857925373));
#46677=CARTESIAN_POINT('Ctrl Pts',(16.6817755898824,20.7413512572339,-16.3149393704228));
#46678=CARTESIAN_POINT('Ctrl Pts',(16.7319890129006,20.8086882244474,-16.3191104844007));
#46679=CARTESIAN_POINT('Ctrl Pts',(16.7855574030483,20.8736012662212,-16.3232815983787));
#46680=CARTESIAN_POINT('Ctrl Pts',(16.8422127801055,20.9357437823178,-16.3274527123566));
#46681=CARTESIAN_POINT('Ctrl Pts',(16.8988491459038,20.997865445893,-16.331622426677));
#46682=CARTESIAN_POINT('Ctrl Pts',(16.9585701316818,21.0572180904717,-16.3357921409973));
#46683=CARTESIAN_POINT('Ctrl Pts',(17.0210683042879,21.1134891605013,-16.3399618553177));
#46684=CARTESIAN_POINT('Ctrl Pts',(17.0835642529408,21.1697582281647,-16.3441314212618));
#46685=CARTESIAN_POINT('Ctrl Pts',(17.1488368494857,21.2229456321214,-16.3483009872058));
#46686=CARTESIAN_POINT('Ctrl Pts',(17.2165437463578,21.2727775142537,-16.3524705531499));
#46687=CARTESIAN_POINT('Ctrl Pts',(17.2866311341984,21.3243614238875,-16.3567867158888));
#46688=CARTESIAN_POINT('Ctrl Pts',(17.3593267625536,21.3723491485032,-16.3611028786277));
#46689=CARTESIAN_POINT('Ctrl Pts',(17.4342176396321,21.4164853923063,-16.3654190413666));
#46690=CARTESIAN_POINT('Ctrl Pts',(17.5066689542669,21.4591839026099,-16.3695946055583));
#46691=CARTESIAN_POINT('Ctrl Pts',(17.5811742544608,21.4982778256331,-16.37377016975));
#46692=CARTESIAN_POINT('Ctrl Pts',(17.6573356824291,21.533583464005,-16.3779457339417));
#46693=CARTESIAN_POINT('Ctrl Pts',(17.7373438430675,21.5706723062399,-16.3823321959542));
#46694=CARTESIAN_POINT('Ctrl Pts',(17.8191792885613,21.6035798961265,-16.3867186579667));
#46695=CARTESIAN_POINT('Ctrl Pts',(17.9023606575271,21.6321517928563,-16.3911051199793));
#46696=CARTESIAN_POINT('Ctrl Pts',(17.985542026493,21.6607236895861,-16.3954915819918));
#46697=CARTESIAN_POINT('Ctrl Pts',(18.0700687402226,21.6849598063577,-16.3998780440043));
#46698=CARTESIAN_POINT('Ctrl Pts',(18.1554472698608,21.7047675790756,-16.4042645060169));
#46699=CARTESIAN_POINT('Ctrl Pts',(18.2369040239201,21.7236655019793,-16.4084494803759));
#46700=CARTESIAN_POINT('Ctrl Pts',(18.3194392781939,21.7386033270985,-16.4126344547349));
#46701=CARTESIAN_POINT('Ctrl Pts',(18.4026332182035,21.7494633256996,-16.4168194290939));
#46702=CARTESIAN_POINT('Ctrl Pts',(18.4856850454026,21.7603047731307,-16.4209972546333));
#46703=CARTESIAN_POINT('Ctrl Pts',(18.5693928687513,21.7670821859801,-16.4251750801727));
#46704=CARTESIAN_POINT('Ctrl Pts',(18.6533252588855,21.7697285096598,-16.4293529057122));
#46705=CARTESIAN_POINT('Ctrl Pts',(18.7371760689815,21.7723722611838,-16.4335266705169));
#46706=CARTESIAN_POINT('Ctrl Pts',(18.821250555471,21.7708928806735,-16.4377004353216));
#46707=CARTESIAN_POINT('Ctrl Pts',(18.9051115090561,21.7652750148464,-16.4418742001264));
#46708=CARTESIAN_POINT('Ctrl Pts',(18.9889161108075,21.7596609240425,-16.4460451602969));
#46709=CARTESIAN_POINT('Ctrl Pts',(19.0725070069924,21.7499139014393,-16.4502161204674));
#46710=CARTESIAN_POINT('Ctrl Pts',(19.1554476929899,21.736070660808,-16.4543870806379));
#46711=CARTESIAN_POINT('Ctrl Pts',(19.238357526517,21.7222325696177,-16.4585564892849));
#46712=CARTESIAN_POINT('Ctrl Pts',(19.3206171772896,21.7043013640799,-16.4627258979319));
#46713=CARTESIAN_POINT('Ctrl Pts',(19.4017973253961,21.682365357893,-16.4668953065789));
#46714=CARTESIAN_POINT('Ctrl Pts',(19.4830102717192,21.6604204891714,-16.4710663997407));
#46715=CARTESIAN_POINT('Ctrl Pts',(19.5631423969819,21.6344676983522,-16.4752374929026));
#46716=CARTESIAN_POINT('Ctrl Pts',(19.6417773433648,21.6046458165053,-16.4794085860645));
#46717=CARTESIAN_POINT('Ctrl Pts',(19.7204244341702,21.5748193289513,-16.4835803234122));
#46718=CARTESIAN_POINT('Ctrl Pts',(19.7975734594199,21.5411227351377,-16.4877520607599));
#46719=CARTESIAN_POINT('Ctrl Pts',(19.8728278889751,21.5037431254488,-16.4919237981076));
#46720=CARTESIAN_POINT('Ctrl Pts',(19.9481771492335,21.4663164124239,-16.4961007924055));
#46721=CARTESIAN_POINT('Ctrl Pts',(20.0216266360793,21.425197626564,-16.5002777867034));
#46722=CARTESIAN_POINT('Ctrl Pts',(20.0928045893704,21.3806198026166,-16.5044547810012));
#46723=CARTESIAN_POINT('Ctrl Pts',(20.1619637761317,21.337306305821,-16.5085133063646));
#46724=CARTESIAN_POINT('Ctrl Pts',(20.2289782723143,21.2907276477199,-16.5125718317281));
#46725=CARTESIAN_POINT('Ctrl Pts',(20.2935358855687,21.2411349269503,-16.5166303570915));
#46726=CARTESIAN_POINT('',(16.1740005630998,19.2093020392336,-16.1667098902285));
#46727=CARTESIAN_POINT('Ctrl Pts',(16.1740005630998,19.2093020392336,-16.1667098902285));
#46728=CARTESIAN_POINT('Ctrl Pts',(16.1739457994085,19.2918687402816,-16.1708335669039));
#46729=CARTESIAN_POINT('Ctrl Pts',(16.1778897355288,19.3745927743499,-16.1749572435793));
#46730=CARTESIAN_POINT('Ctrl Pts',(16.185851592152,19.4570481489095,-16.1790809202548));
#46731=CARTESIAN_POINT('Ctrl Pts',(16.193849980064,19.5398818524496,-16.1832235175451));
#46732=CARTESIAN_POINT('Ctrl Pts',(16.2059033176551,19.6224439445466,-16.1873661148355));
#46733=CARTESIAN_POINT('Ctrl Pts',(16.2219780566694,19.7043008779901,-16.1915087121259));
#46734=CARTESIAN_POINT('Ctrl Pts',(16.23794569149,19.7856124078128,-16.1956237077524));
#46735=CARTESIAN_POINT('Ctrl Pts',(16.2578812222445,19.8662276743518,-16.1997387033789));
#46736=CARTESIAN_POINT('Ctrl Pts',(16.2816998746989,19.9457272251988,-16.2038536990054));
#46737=CARTESIAN_POINT('Ctrl Pts',(16.3055083094403,20.0251926723702,-16.2079669293832));
#46738=CARTESIAN_POINT('Ctrl Pts',(16.33319642467,20.1035429002386,-16.2120801597611));
#46739=CARTESIAN_POINT('Ctrl Pts',(16.3646289972004,20.1803714721883,-16.2161933901389));
#46740=CARTESIAN_POINT('Ctrl Pts',(16.3960581246075,20.2571916234494,-16.2203061696919));
#46741=CARTESIAN_POINT('Ctrl Pts',(16.4312307139715,20.3324900117992,-16.2244189492448));
#46742=CARTESIAN_POINT('Ctrl Pts',(16.469963164482,20.405879578626,-16.2285317287978));
#46743=CARTESIAN_POINT('Ctrl Pts',(16.5091807554344,20.48018838104,-16.2326960226666));
#46744=CARTESIAN_POINT('Ctrl Pts',(16.5520477937182,20.552539761255,-16.2368603165354));
#46745=CARTESIAN_POINT('Ctrl Pts',(16.5983263505016,20.6225587351713,-16.2410246104042));
#46746=CARTESIAN_POINT('Ctrl Pts',(16.6440925485817,20.6918025157112,-16.2451428005837));
#46747=CARTESIAN_POINT('Ctrl Pts',(16.6931947649456,20.7587649302322,-16.2492609907631));
#46748=CARTESIAN_POINT('Ctrl Pts',(16.7453611252724,20.8231152024351,-16.2533791809425));
#46749=CARTESIAN_POINT('Ctrl Pts',(16.7984034996618,20.8885460894828,-16.257566526656));
#46750=CARTESIAN_POINT('Ctrl Pts',(16.8546135316783,20.9512759179513,-16.2617538723695));
#46751=CARTESIAN_POINT('Ctrl Pts',(16.9136665630956,21.010996160687,-16.265941218083));
#46752=CARTESIAN_POINT('Ctrl Pts',(16.972719594513,21.0707164034227,-16.2701285637965));
#46753=CARTESIAN_POINT('Ctrl Pts',(17.0346152026565,21.1274267716985,-16.2743159095101));
#46754=CARTESIAN_POINT('Ctrl Pts',(17.0989955289249,21.1808630357374,-16.2785032552236));
#46755=CARTESIAN_POINT('Ctrl Pts',(17.1633341687151,21.2342646996152,-16.2826878896166));
#46756=CARTESIAN_POINT('Ctrl Pts',(17.2304115572045,21.2846103343966,-16.2868725240096));
#46757=CARTESIAN_POINT('Ctrl Pts',(17.29990527078,21.3316065895454,-16.2910571584027));
#46758=CARTESIAN_POINT('Ctrl Pts',(17.3693000686558,21.378535951342,-16.2952358364866));
#46759=CARTESIAN_POINT('Ctrl Pts',(17.4411039821925,21.4221251476138,-16.2994145145706));
#46760=CARTESIAN_POINT('Ctrl Pts',(17.5149611920068,21.4621206952553,-16.3035931926545));
#46761=CARTESIAN_POINT('Ctrl Pts',(17.5901422392269,21.5028331343439,-16.30784677054));
#46762=CARTESIAN_POINT('Ctrl Pts',(17.6674505464319,21.5398215173808,-16.3121003484254));
#46763=CARTESIAN_POINT('Ctrl Pts',(17.7464794551571,21.5728643427414,-16.3163539263108));
#46764=CARTESIAN_POINT('Ctrl Pts',(17.8239762342744,21.6052665684546,-16.3205250402888));
#46765=CARTESIAN_POINT('Ctrl Pts',(17.9031270518499,21.6338746703221,-16.3246961542667));
#46766=CARTESIAN_POINT('Ctrl Pts',(17.983524818815,21.6585267112792,-16.3288672682447));
#46767=CARTESIAN_POINT('Ctrl Pts',(18.0638956075329,21.6831704800059,-16.3330369825651));
#46768=CARTESIAN_POINT('Ctrl Pts',(18.1455120751846,21.7038606894987,-16.3372066968854));
#46769=CARTESIAN_POINT('Ctrl Pts',(18.2279505020329,21.7204847888774,-16.3413764112058));
#46770=CARTESIAN_POINT('Ctrl Pts',(18.3103859953682,21.7371082966994,-16.3455459771499));
#46771=CARTESIAN_POINT('Ctrl Pts',(18.3936429386223,21.7496658919856,-16.3497155430939));
#46772=CARTESIAN_POINT('Ctrl Pts',(18.4772872562561,21.758096104822,-16.353885109038));
#46773=CARTESIAN_POINT('Ctrl Pts',(18.5638724049115,21.7668227135419,-16.3582012717769));
#46774=CARTESIAN_POINT('Ctrl Pts',(18.6508721501767,21.7711262492444,-16.3625174345158));
#46775=CARTESIAN_POINT('Ctrl Pts',(18.7378010569183,21.7709971781169,-16.3668335972547));
#46776=CARTESIAN_POINT('Ctrl Pts',(18.821898263666,21.7708723114677,-16.3710091614464));
#46777=CARTESIAN_POINT('Ctrl Pts',(18.9059287081103,21.7665992585964,-16.3751847256381));
#46778=CARTESIAN_POINT('Ctrl Pts',(18.9894564259431,21.7582224116563,-16.3793602898298));
#46779=CARTESIAN_POINT('Ctrl Pts',(19.0772029302354,21.7494224700914,-16.3837467518423));
#46780=CARTESIAN_POINT('Ctrl Pts',(19.1643940106309,21.7360933624401,-16.3881332138549));
#46781=CARTESIAN_POINT('Ctrl Pts',(19.2505367177895,21.7183471676605,-16.3925196758674));
#46782=CARTESIAN_POINT('Ctrl Pts',(19.3366794249481,21.700600972881,-16.3969061378799));
#46783=CARTESIAN_POINT('Ctrl Pts',(19.4217732165569,21.6784379108237,-16.4012925998925));
#46784=CARTESIAN_POINT('Ctrl Pts',(19.5053461655911,21.652029514944,-16.405679061905));
#46785=CARTESIAN_POINT('Ctrl Pts',(19.5850559562968,21.6268418467719,-16.4098627597761));
#46786=CARTESIAN_POINT('Ctrl Pts',(19.6636790298746,21.5976989266396,-16.4140464576472));
#46787=CARTESIAN_POINT('Ctrl Pts',(19.7407944846494,21.5647129956049,-16.4182301555184));
#46788=CARTESIAN_POINT('Ctrl Pts',(19.817813812667,21.5317681825354,-16.422408638283));
#46789=CARTESIAN_POINT('Ctrl Pts',(19.8933288322741,21.4949900441864,-16.4265871210476));
#46790=CARTESIAN_POINT('Ctrl Pts',(19.9669338586835,21.4545405278514,-16.4307656038122));
#46791=CARTESIAN_POINT('Ctrl Pts',(20.0404561874615,21.4141364578583,-16.4349393919161));
#46792=CARTESIAN_POINT('Ctrl Pts',(20.1120723866535,21.3700694275403,-16.43911318002));
#46793=CARTESIAN_POINT('Ctrl Pts',(20.1813982979661,21.3225487602812,-16.4432869681239));
#46794=CARTESIAN_POINT('Ctrl Pts',(20.2194886441686,21.2964390614196,-16.4455802092922));
#46795=CARTESIAN_POINT('Ctrl Pts',(20.2568879835979,21.2692875967535,-16.4478734504605));
#46796=CARTESIAN_POINT('Ctrl Pts',(20.2935358855687,21.2411349269503,-16.4501666916289));
#46797=CARTESIAN_POINT('Ctrl Pts',(20.2958871626529,21.2441650537926,-15.6501589834813));
#46798=CARTESIAN_POINT('Ctrl Pts',(20.9266956913523,20.7545799070163,-15.6900393318202));
#46799=CARTESIAN_POINT('Ctrl Pts',(21.7315666544893,19.0879531984753,-15.7723116157195));
#46800=CARTESIAN_POINT('Ctrl Pts',(20.3102572494442,16.6266809282313,-15.8969758351793));
#46801=CARTESIAN_POINT('Ctrl Pts',(17.4141947910433,16.4867742032747,-16.0241516418607));
#46802=CARTESIAN_POINT('Ctrl Pts',(16.2227678179363,18.1548349051303,-16.1140629935438));
#46803=CARTESIAN_POINT('Ctrl Pts',(16.1704458861955,19.106523168223,-16.1615824096664));
#46804=CARTESIAN_POINT('Ctrl Pts',(16.1712324881214,19.2093002032634,-16.1667098902285));
#46805=CARTESIAN_POINT('Origin',(18.734,19.211,1.76670989022852));
#46806=CARTESIAN_POINT('',(20.2935358855687,21.2411349269503,-14.8500370294445));
#46807=CARTESIAN_POINT('',(20.2935358855687,21.2411349269503,-14.9167585822245));
#46808=CARTESIAN_POINT('',(20.2935358855687,21.2411349269503,1.76670989022852));
#46809=CARTESIAN_POINT('',(16.174000571626,19.2092892327452,-15.4332901097416));
#46810=CARTESIAN_POINT('Ctrl Pts',(20.2935358855687,21.2411349269503,-14.9167585822245));
#46811=CARTESIAN_POINT('Ctrl Pts',(20.3601520146462,21.1899608682831,-14.9209295765852));
#46812=CARTESIAN_POINT('Ctrl Pts',(20.4242947432533,21.1354675703399,-14.9251005709459));
#46813=CARTESIAN_POINT('Ctrl Pts',(20.4856216544896,21.0779283809303,-14.9292715653066));
#46814=CARTESIAN_POINT('Ctrl Pts',(20.5469290937748,21.0204074608296,-14.9334412353319));
#46815=CARTESIAN_POINT('Ctrl Pts',(20.6054221561177,20.9598428845434,-14.9376109053571));
#46816=CARTESIAN_POINT('Ctrl Pts',(20.6607930923822,20.8965469080237,-14.9417805753824));
#46817=CARTESIAN_POINT('Ctrl Pts',(20.7161630576809,20.8332520414406,-14.9459501722898));
#46818=CARTESIAN_POINT('Ctrl Pts',(20.7684107036615,20.7672262168081,-14.9501197691972));
#46819=CARTESIAN_POINT('Ctrl Pts',(20.8172675280852,20.6988159854048,-14.9542893661046));
#46820=CARTESIAN_POINT('Ctrl Pts',(20.86710676209,20.6290301658912,-14.9585428049726));
#46821=CARTESIAN_POINT('Ctrl Pts',(20.9134170181936,20.5567633970815,-14.9627962438407));
#46822=CARTESIAN_POINT('Ctrl Pts',(20.9559598075288,20.482414414629,-14.9670496827087));
#46823=CARTESIAN_POINT('Ctrl Pts',(20.9977248080393,20.4094247179354,-14.9712253580528));
#46824=CARTESIAN_POINT('Ctrl Pts',(21.0358587895228,20.3344287511086,-14.9754010333968));
#46825=CARTESIAN_POINT('Ctrl Pts',(21.0701835569614,20.2578268186205,-14.9795767087409));
#46826=CARTESIAN_POINT('Ctrl Pts',(21.1054671686548,20.1790850515945,-14.9838690293709));
#46827=CARTESIAN_POINT('Ctrl Pts',(21.1367253886224,20.0986467474965,-14.988161350001));
#46828=CARTESIAN_POINT('Ctrl Pts',(21.1638191362431,20.0169646178008,-14.992453670631));
#46829=CARTESIAN_POINT('Ctrl Pts',(21.1909128838638,19.9352824881052,-14.996745991261));
#46830=CARTESIAN_POINT('Ctrl Pts',(21.2138420873009,19.8523570528488,-15.0010383118911));
#46831=CARTESIAN_POINT('Ctrl Pts',(21.2325245180281,19.7686515334979,-15.0053306325211));
#46832=CARTESIAN_POINT('Ctrl Pts',(21.2507382417699,19.6870460279088,-15.0095152669142));
#46833=CARTESIAN_POINT('Ctrl Pts',(21.2649836214983,19.6043953888037,-15.0136999013072));
#46834=CARTESIAN_POINT('Ctrl Pts',(21.2751464736302,19.5211202985241,-15.0178845357003));
#46835=CARTESIAN_POINT('Ctrl Pts',(21.2852948602001,19.437963740028,-15.0220632137842));
#46836=CARTESIAN_POINT('Ctrl Pts',(21.2913722063419,19.3541849485906,-15.0262418918682));
#46837=CARTESIAN_POINT('Ctrl Pts',(21.2933150345072,19.2702161645608,-15.0304205699521));
#46838=CARTESIAN_POINT('Ctrl Pts',(21.2952926864712,19.1847423004247,-15.0346741478376));
#46839=CARTESIAN_POINT('Ctrl Pts',(21.2929860350543,19.0990720360279,-15.038927725723));
#46840=CARTESIAN_POINT('Ctrl Pts',(21.2863832385264,19.0136682902077,-15.0431813036084));
#46841=CARTESIAN_POINT('Ctrl Pts',(21.2799084500934,18.929920262652,-15.0473524175864));
#46842=CARTESIAN_POINT('Ctrl Pts',(21.2693026454396,18.8464289917131,-15.0515235315643));
#46843=CARTESIAN_POINT('Ctrl Pts',(21.2546071988875,18.7636306348034,-15.0556946455423));
#46844=CARTESIAN_POINT('Ctrl Pts',(21.2399166835344,18.6808600616818,-15.0598643598627));
#46845=CARTESIAN_POINT('Ctrl Pts',(21.2211393320556,18.5987823933899,-15.0640340741831));
#46846=CARTESIAN_POINT('Ctrl Pts',(21.1983680574963,18.5178260844552,-15.0682037885034));
#46847=CARTESIAN_POINT('Ctrl Pts',(21.1755975932368,18.4368726562935,-15.0723733544475));
#46848=CARTESIAN_POINT('Ctrl Pts',(21.1488336138536,18.357040950769,-15.0765429203915));
#46849=CARTESIAN_POINT('Ctrl Pts',(21.1182192201023,18.2787453617736,-15.0807124863356));
#46850=CARTESIAN_POINT('Ctrl Pts',(21.0865284620337,18.1976969964573,-15.0850286490745));
#46851=CARTESIAN_POINT('Ctrl Pts',(21.0507116827587,18.1182952684024,-15.0893448118134));
#46852=CARTESIAN_POINT('Ctrl Pts',(21.0109816181364,18.0409766196058,-15.0936609745523));
#46853=CARTESIAN_POINT('Ctrl Pts',(20.9725457561902,17.9661766176612,-15.097836538744));
#46854=CARTESIAN_POINT('Ctrl Pts',(20.9304479207722,17.8933264506918,-15.1020121029357));
#46855=CARTESIAN_POINT('Ctrl Pts',(20.884926303708,17.8227939504464,-15.1061876671274));
#46856=CARTESIAN_POINT('Ctrl Pts',(20.8371054979832,17.7486990212888,-15.1105741291399));
#46857=CARTESIAN_POINT('Ctrl Pts',(20.7855062921192,17.6771625161638,-15.1149605911524));
#46858=CARTESIAN_POINT('Ctrl Pts',(20.7304530967375,17.6085721443612,-15.119347053165));
#46859=CARTESIAN_POINT('Ctrl Pts',(20.6753999013558,17.5399817725586,-15.1237335151775));
#46860=CARTESIAN_POINT('Ctrl Pts',(20.616893159293,17.4743379166139,-15.12811997719));
#46861=CARTESIAN_POINT('Ctrl Pts',(20.5553006227462,17.4119824788001,-15.1325064392026));
#46862=CARTESIAN_POINT('Ctrl Pts',(20.496542050108,17.352496107113,-15.1366910735956));
#46863=CARTESIAN_POINT('Ctrl Pts',(20.4347566962297,17.2957807737874,-15.1408757079887));
#46864=CARTESIAN_POINT('Ctrl Pts',(20.3702364829786,17.2421601965193,-15.1450603423817));
#46865=CARTESIAN_POINT('Ctrl Pts',(20.3058081062651,17.1886159415061,-15.1492390204657));
#46866=CARTESIAN_POINT('Ctrl Pts',(20.2386529531481,17.1381579843472,-15.1534176985496));
#46867=CARTESIAN_POINT('Ctrl Pts',(20.1691001101646,17.0910736631181,-15.1575963766336));
#46868=CARTESIAN_POINT('Ctrl Pts',(20.0983005824573,17.0431453892698,-15.161849954519));
#46869=CARTESIAN_POINT('Ctrl Pts',(20.0250169010501,16.9987132288229,-15.1661035324044));
#46870=CARTESIAN_POINT('Ctrl Pts',(19.9496318977225,16.9580377079854,-15.1703571102899));
#46871=CARTESIAN_POINT('Ctrl Pts',(19.8757083797862,16.9181507614911,-15.1745282242678));
#46872=CARTESIAN_POINT('Ctrl Pts',(19.7997647128027,16.8818763233781,-15.1786993382458));
#46873=CARTESIAN_POINT('Ctrl Pts',(19.7221900312683,16.8494156881233,-15.1828704522237));
#46874=CARTESIAN_POINT('Ctrl Pts',(19.6446413806673,16.8169659453482,-15.1870401665441));
#46875=CARTESIAN_POINT('Ctrl Pts',(19.5654632264915,16.7883276412413,-15.1912098808645));
#46876=CARTESIAN_POINT('Ctrl Pts',(19.4850661232635,16.7636545649447,-15.1953795951849));
#46877=CARTESIAN_POINT('Ctrl Pts',(19.4046718809096,16.7389823666222,-15.1995491611289));
#46878=CARTESIAN_POINT('Ctrl Pts',(19.3230592157838,16.7182752497195,-15.2037187270729));
#46879=CARTESIAN_POINT('Ctrl Pts',(19.2406540252948,16.7016371927016,-15.207888293017));
#46880=CARTESIAN_POINT('Ctrl Pts',(19.1553515699658,16.6844141621241,-15.2122044557559));
#46881=CARTESIAN_POINT('Ctrl Pts',(19.0692003389648,16.6715517559429,-15.2165206184948));
#46882=CARTESIAN_POINT('Ctrl Pts',(18.9826824608285,16.6631073347418,-15.2208367812337));
#46883=CARTESIAN_POINT('Ctrl Pts',(18.8989828934724,16.6549379896732,-15.2250123454254));
#46884=CARTESIAN_POINT('Ctrl Pts',(18.8149406719769,16.650903193465,-15.2291879096171));
#46885=CARTESIAN_POINT('Ctrl Pts',(18.7309940133495,16.6510017648357,-15.2333634738088));
#46886=CARTESIAN_POINT('Ctrl Pts',(18.6428074085591,16.6511053148121,-15.2377499358213));
#46887=CARTESIAN_POINT('Ctrl Pts',(18.5547268571684,16.6557707277653,-15.2421363978338));
#46888=CARTESIAN_POINT('Ctrl Pts',(18.4672539586503,16.6649350853868,-15.2465228598464));
#46889=CARTESIAN_POINT('Ctrl Pts',(18.3797810601322,16.6740994430083,-15.2509093218589));
#46890=CARTESIAN_POINT('Ctrl Pts',(18.2929163758375,16.6877625800018,-15.2552957838715));
#46891=CARTESIAN_POINT('Ctrl Pts',(18.2071464487601,16.7058003401833,-15.259682245884));
#46892=CARTESIAN_POINT('Ctrl Pts',(18.125322923169,16.7230081562804,-15.2638668802771));
#46893=CARTESIAN_POINT('Ctrl Pts',(18.0441910630359,16.74426092691,-15.2680515146701));
#46894=CARTESIAN_POINT('Ctrl Pts',(17.9641810754836,16.7694884142285,-15.2722361490632));
#46895=CARTESIAN_POINT('Ctrl Pts',(17.8842849722453,16.7946799933414,-15.2764148271471));
#46896=CARTESIAN_POINT('Ctrl Pts',(17.8055080047355,16.8238349143801,-15.2805935052311));
#46897=CARTESIAN_POINT('Ctrl Pts',(17.7282699071042,16.8568319982967,-15.284772183315));
#46898=CARTESIAN_POINT('Ctrl Pts',(17.6496473720828,16.8904205312279,-15.2890257612004));
#46899=CARTESIAN_POINT('Ctrl Pts',(17.5726198898781,16.92799022417,-15.2932793390859));
#46900=CARTESIAN_POINT('Ctrl Pts',(17.4976137413829,16.969360194076,-15.2975329169713));
#46901=CARTESIAN_POINT('Ctrl Pts',(17.4240617334388,17.0099281263886,-15.3017040309493));
#46902=CARTESIAN_POINT('Ctrl Pts',(17.3524538049873,17.0541500666244,-15.3058751449272));
#46903=CARTESIAN_POINT('Ctrl Pts',(17.2831698439506,17.1018077711367,-15.3100462589052));
#46904=CARTESIAN_POINT('Ctrl Pts',(17.213909131816,17.1494494836459,-15.3142159732255));
#46905=CARTESIAN_POINT('Ctrl Pts',(17.1469712170492,17.2005244102484,-15.3183856875459));
#46906=CARTESIAN_POINT('Ctrl Pts',(17.0827076373572,17.2547705827083,-15.3225554018663));
#46907=CARTESIAN_POINT('Ctrl Pts',(17.0184463444391,17.3090148248566,-15.3267249678103));
#46908=CARTESIAN_POINT('Ctrl Pts',(16.9568595483702,17.3664297911053,-15.3308945337544));
#46909=CARTESIAN_POINT('Ctrl Pts',(16.8982652087739,17.4267136507045,-15.3350640996984));
#46910=CARTESIAN_POINT('Ctrl Pts',(16.8376107644814,17.489117016439,-15.3393802624373));
#46911=CARTESIAN_POINT('Ctrl Pts',(16.7801634890495,17.5545943914719,-15.3436964251763));
#46912=CARTESIAN_POINT('Ctrl Pts',(16.7262325806842,17.6227714301985,-15.3480125879152));
#46913=CARTESIAN_POINT('Ctrl Pts',(16.6740584659863,17.6887276090595,-15.3521881521069));
#46914=CARTESIAN_POINT('Ctrl Pts',(16.6251753803868,17.7572098587058,-15.3563637162986));
#46915=CARTESIAN_POINT('Ctrl Pts',(16.5798195291696,17.8278490685782,-15.3605392804902));
#46916=CARTESIAN_POINT('Ctrl Pts',(16.5321728617309,17.9020560970123,-15.3649257425028));
#46917=CARTESIAN_POINT('Ctrl Pts',(16.488419403819,17.9786432012274,-15.3693122045153));
#46918=CARTESIAN_POINT('Ctrl Pts',(16.4487777573745,18.0571545589595,-15.3736986665278));
#46919=CARTESIAN_POINT('Ctrl Pts',(16.4091361109301,18.1356659166917,-15.3780851285404));
#46920=CARTESIAN_POINT('Ctrl Pts',(16.3736064408137,18.2161009664618,-15.3824715905529));
#46921=CARTESIAN_POINT('Ctrl Pts',(16.3423477078172,18.2979833992217,-15.3868580525655));
#46922=CARTESIAN_POINT('Ctrl Pts',(16.3083133302776,18.3871366489943,-15.3916340140293));
#46923=CARTESIAN_POINT('Ctrl Pts',(16.2792349760219,18.4782809296076,-15.396409975493));
#46924=CARTESIAN_POINT('Ctrl Pts',(16.2553188691388,18.5708907503302,-15.4011859369568));
#46925=CARTESIAN_POINT('Ctrl Pts',(16.2315006236311,18.6631216245767,-15.4059423558521));
#46926=CARTESIAN_POINT('Ctrl Pts',(16.2128025911618,18.756805887815,-15.4106987747473));
#46927=CARTESIAN_POINT('Ctrl Pts',(16.1993817363335,18.8514026453261,-15.4154551936426));
#46928=CARTESIAN_POINT('Ctrl Pts',(16.1860549755608,18.9453361818529,-15.4201782651283));
#46929=CARTESIAN_POINT('Ctrl Pts',(16.1779317634136,19.0401692636772,-15.4249013366139));
#46930=CARTESIAN_POINT('Ctrl Pts',(16.1751178968034,19.1353535728534,-15.4296244080995));
#46931=CARTESIAN_POINT('Ctrl Pts',(16.1743899245164,19.1599785991389,-15.4308463086469));
#46932=CARTESIAN_POINT('Ctrl Pts',(16.1740170525925,19.1846270439603,-15.4320682091943));
#46933=CARTESIAN_POINT('Ctrl Pts',(16.174000571626,19.2092892327452,-15.4332901097416));
#46934=CARTESIAN_POINT('Ctrl Pts',(16.1740005716256,19.2092892333484,-15.4332901097715));
#46935=CARTESIAN_POINT('Ctrl Pts',(16.1739440307447,19.2938972788889,-15.437482057942));
#46936=CARTESIAN_POINT('Ctrl Pts',(16.1780862675835,19.3785303101354,-15.4416740061124));
#46937=CARTESIAN_POINT('Ctrl Pts',(16.1864081330308,19.4627452667924,-15.4458659542829));
#46938=CARTESIAN_POINT('Ctrl Pts',(16.1947304086796,19.5469643745742,-15.4500581090829));
#46939=CARTESIAN_POINT('Ctrl Pts',(16.2072326772703,19.6307649161166,-15.4542502638829));
#46940=CARTESIAN_POINT('Ctrl Pts',(16.2238439368849,19.713709199047,-15.458442418683));
#46941=CARTESIAN_POINT('Ctrl Pts',(16.2404607969944,19.7966814466863,-15.4626359868702));
#46942=CARTESIAN_POINT('Ctrl Pts',(16.261189311038,19.8787964183332,-15.4668295550574));
#46943=CARTESIAN_POINT('Ctrl Pts',(16.2859076895266,19.9596281048698,-15.4710231232447));
#46944=CARTESIAN_POINT('Ctrl Pts',(16.3106584247115,20.0405656011923,-15.4752221808702));
#46945=CARTESIAN_POINT('Ctrl Pts',(16.3394093150967,20.1202160261802,-15.4794212384956));
#46946=CARTESIAN_POINT('Ctrl Pts',(16.3719892689075,20.1981703531832,-15.4836202961211));
#46947=CARTESIAN_POINT('Ctrl Pts',(16.4045936038559,20.2761830171373,-15.4878224961023));
#46948=CARTESIAN_POINT('Ctrl Pts',(16.4410325111314,20.3524966484666,-15.4920246960834));
#46949=CARTESIAN_POINT('Ctrl Pts',(16.4810885578785,20.426726134439,-15.4962268960645));
#46950=CARTESIAN_POINT('Ctrl Pts',(16.5212156880345,20.5010873479616,-15.5004365532643));
#46951=CARTESIAN_POINT('Ctrl Pts',(16.5649725361191,20.5733566470847,-15.5046462104641));
#46952=CARTESIAN_POINT('Ctrl Pts',(16.6120981192869,20.6431775059769,-15.5088558676639));
#46953=CARTESIAN_POINT('Ctrl Pts',(16.6314200308982,20.6718046841136,-15.5105818648583));
#46954=CARTESIAN_POINT('Ctrl Pts',(16.6513077816385,20.700020648932,-15.5123078620526));
#46955=CARTESIAN_POINT('Ctrl Pts',(16.6717415022698,20.7278025212728,-15.5140338592469));
#46956=CARTESIAN_POINT('Ctrl Pts',(16.7212825156696,20.7951589334866,-15.5182184936399));
#46957=CARTESIAN_POINT('Ctrl Pts',(16.7742191330187,20.8602110167103,-15.522403128033));
#46958=CARTESIAN_POINT('Ctrl Pts',(16.8303093008605,20.9225962497066,-15.526587762426));
#46959=CARTESIAN_POINT('Ctrl Pts',(16.8863196312909,20.9848926850454,-15.53076644051));
#46960=CARTESIAN_POINT('Ctrl Pts',(16.9454742913218,21.044529470903,-15.5349451185939));
#46961=CARTESIAN_POINT('Ctrl Pts',(17.0074891937054,21.1011747103768,-15.5391237966779));
#46962=CARTESIAN_POINT('Ctrl Pts',(17.0706156686449,21.1588352750579,-15.5433773745633));
#46963=CARTESIAN_POINT('Ctrl Pts',(17.1367056485331,21.2133956031449,-15.5476309524487));
#46964=CARTESIAN_POINT('Ctrl Pts',(17.2054179892121,21.2645425577026,-15.5518845303342));
#46965=CARTESIAN_POINT('Ctrl Pts',(17.2727982070859,21.314697928741,-15.5560556443121));
#46966=CARTESIAN_POINT('Ctrl Pts',(17.3426996279385,21.3615708076596,-15.5602267582901));
#46967=CARTESIAN_POINT('Ctrl Pts',(17.4147663076934,21.4049057557432,-15.564397872268));
#46968=CARTESIAN_POINT('Ctrl Pts',(17.4868088047781,21.4482261623665,-15.5685675865884));
#46969=CARTESIAN_POINT('Ctrl Pts',(17.561014723861,21.4880107590573,-15.5727373009088));
#46970=CARTESIAN_POINT('Ctrl Pts',(17.6370000578042,21.5240480165406,-15.5769070152292));
#46971=CARTESIAN_POINT('Ctrl Pts',(17.7129826878631,21.5600839916636,-15.5810765811732));
#46972=CARTESIAN_POINT('Ctrl Pts',(17.7907441908666,21.5923726963449,-15.5852461471172));
#46973=CARTESIAN_POINT('Ctrl Pts',(17.8698781766135,21.6207496704735,-15.5894157130613));
#46974=CARTESIAN_POINT('Ctrl Pts',(17.951794415677,21.6501243440057,-15.5937318758002));
#46975=CARTESIAN_POINT('Ctrl Pts',(18.0351809497172,21.6753069180702,-15.5980480385391));
#46976=CARTESIAN_POINT('Ctrl Pts',(18.119569008403,21.6961709310559,-15.602364201278));
#46977=CARTESIAN_POINT('Ctrl Pts',(18.2012081349532,21.7163553010131,-15.6065397654697));
#46978=CARTESIAN_POINT('Ctrl Pts',(18.2837840674898,21.7324980994093,-15.6107153296614));
#46979=CARTESIAN_POINT('Ctrl Pts',(18.3668630221883,21.7445371399534,-15.6148908938531));
#46980=CARTESIAN_POINT('Ctrl Pts',(18.4541380973871,21.7571842438152,-15.6192773558656));
#46981=CARTESIAN_POINT('Ctrl Pts',(18.5419677640929,21.7653020795901,-15.6236638178781));
#46982=CARTESIAN_POINT('Ctrl Pts',(18.6298465962985,21.7688803858854,-15.6280502798907));
#46983=CARTESIAN_POINT('Ctrl Pts',(18.7177254285041,21.7724586921808,-15.6324367419032));
#46984=CARTESIAN_POINT('Ctrl Pts',(18.8056528468587,21.771497551399,-15.6368232039158));
#46985=CARTESIAN_POINT('Ctrl Pts',(18.8931294701918,21.7660494734381,-15.6412096659283));
#46986=CARTESIAN_POINT('Ctrl Pts',(18.9765715593009,21.7608526678304,-15.6453938186788));
#46987=CARTESIAN_POINT('Ctrl Pts',(19.0599140713073,21.7515543524027,-15.6495779714293));
#46988=CARTESIAN_POINT('Ctrl Pts',(19.1427213148452,21.7381618244171,-15.6537621241798));
#46989=CARTESIAN_POINT('Ctrl Pts',(19.2254168838743,21.7247873577016,-15.6579406341486));
#46990=CARTESIAN_POINT('Ctrl Pts',(19.307578167734,21.7073297146533,-15.6621191441173));
#46991=CARTESIAN_POINT('Ctrl Pts',(19.3887723742193,21.6858481040176,-15.6662976540861));
#46992=CARTESIAN_POINT('Ctrl Pts',(19.4703186692208,21.6642733410653,-15.6704942836404));
#46993=CARTESIAN_POINT('Ctrl Pts',(19.5508890103775,21.6386396544188,-15.6746909131948));
#46994=CARTESIAN_POINT('Ctrl Pts',(19.6300531105458,21.6090593868963,-15.6788875427491));
#46995=CARTESIAN_POINT('Ctrl Pts',(19.708732915175,21.5796600800816,-15.6830584989368));
#46996=CARTESIAN_POINT('Ctrl Pts',(19.7860231996119,21.5463625042622,-15.6872294551245));
#46997=CARTESIAN_POINT('Ctrl Pts',(19.8615163104711,21.5093269936242,-15.6914004113121));
#46998=CARTESIAN_POINT('Ctrl Pts',(19.9377064421921,21.4719495375657,-15.6956098775498));
#46999=CARTESIAN_POINT('Ctrl Pts',(20.0120655910137,21.430764917828,-15.6998193437875));
#47000=CARTESIAN_POINT('Ctrl Pts',(20.0841966760578,21.3859871116773,-15.7040288100252));
#47001=CARTESIAN_POINT('Ctrl Pts',(20.1563277611019,21.3412093055266,-15.7082382762629));
#47002=CARTESIAN_POINT('Ctrl Pts',(20.2262303717876,21.2928385662724,-15.7124477425006));
#47003=CARTESIAN_POINT('Ctrl Pts',(20.2935358855687,21.2411349269503,-15.7166572087383));
#47004=CARTESIAN_POINT('',(16.1740008768645,19.213118854712,-15.3667098902285));
#47005=CARTESIAN_POINT('Ctrl Pts',(16.1723624648697,19.2131202107894,-15.3667098902285));
#47006=CARTESIAN_POINT('Ctrl Pts',(16.1710770500739,19.3573559412274,-15.3738974629702));
#47007=CARTESIAN_POINT('Ctrl Pts',(16.2478506686825,20.350918062683,-15.4234769712723));
#47008=CARTESIAN_POINT('Ctrl Pts',(17.5479306856132,21.9960550376254,-15.515448415135));
#47009=CARTESIAN_POINT('Ctrl Pts',(19.528832106138,21.8036795310292,-15.6027438734776));
#47010=CARTESIAN_POINT('Ctrl Pts',(20.2561600613117,21.2749981796243,-15.6476473962597));
#47011=CARTESIAN_POINT('Ctrl Pts',(20.2958871626529,21.2441650537926,-15.6501589834813));
#47012=CARTESIAN_POINT('Ctrl Pts',(20.2935358855687,21.2411349269503,-14.8500370294445));
#47013=CARTESIAN_POINT('Ctrl Pts',(20.3601765745563,21.1899420015267,-14.8542147192048));
#47014=CARTESIAN_POINT('Ctrl Pts',(20.424227826631,21.1355151814304,-14.8583924089651));
#47015=CARTESIAN_POINT('Ctrl Pts',(20.4853757374046,21.078159079037,-14.8625700987253));
#47016=CARTESIAN_POINT('Ctrl Pts',(20.5466225419779,21.0207102152913,-14.8667545450143));
#47017=CARTESIAN_POINT('Ctrl Pts',(20.6049563163785,20.9603229457015,-14.8709389913032));
#47018=CARTESIAN_POINT('Ctrl Pts',(20.6601019149597,20.8973366844105,-14.8751234375922));
#47019=CARTESIAN_POINT('Ctrl Pts',(20.6796325157998,20.8750292009606,-14.8766054189707));
#47020=CARTESIAN_POINT('Ctrl Pts',(20.6987636044015,20.8523959980119,-14.8780874003493));
#47021=CARTESIAN_POINT('Ctrl Pts',(20.7174842649081,20.8294530178111,-14.8795693817278));
#47022=CARTESIAN_POINT('Ctrl Pts',(20.770345333846,20.764669488533,-14.8837540161209));
#47023=CARTESIAN_POINT('Ctrl Pts',(20.8201275486196,20.6971728954314,-14.8879386505139));
#47024=CARTESIAN_POINT('Ctrl Pts',(20.8665402687069,20.6272881071108,-14.892123284907));
#47025=CARTESIAN_POINT('Ctrl Pts',(20.9128869260319,20.5575027911363,-14.8963019629909));
#47026=CARTESIAN_POINT('Ctrl Pts',(20.9558733628217,20.4853364119635,-14.9004806410749));
#47027=CARTESIAN_POINT('Ctrl Pts',(20.995249084218,20.4111468989766,-14.9046593191588));
#47028=CARTESIAN_POINT('Ctrl Pts',(21.0353305871215,20.3356275922885,-14.9089128970442));
#47029=CARTESIAN_POINT('Ctrl Pts',(21.0716703524657,20.2580122826047,-14.9131664749297));
#47030=CARTESIAN_POINT('Ctrl Pts',(21.1040502914401,20.1787094688203,-14.9174200528151));
#47031=CARTESIAN_POINT('Ctrl Pts',(21.1358024821133,20.1009440948279,-14.9215911667931));
#47032=CARTESIAN_POINT('Ctrl Pts',(21.1637468322871,20.0215565094717,-14.925762280771));
#47033=CARTESIAN_POINT('Ctrl Pts',(21.1877248192282,19.9409551434873,-14.929933394749));
#47034=CARTESIAN_POINT('Ctrl Pts',(21.2116947601242,19.8603808240696,-14.9341031090693));
#47035=CARTESIAN_POINT('Ctrl Pts',(21.2317008500142,19.7785939734878,-14.9382728233897));
#47036=CARTESIAN_POINT('Ctrl Pts',(21.2476340898708,19.6960192390405,-14.9424425377101));
#47037=CARTESIAN_POINT('Ctrl Pts',(21.2635667627543,19.6134474429566,-14.9466121036541));
#47038=CARTESIAN_POINT('Ctrl Pts',(21.2754267874401,19.5300882706129,-14.9507816695982));
#47039=CARTESIAN_POINT('Ctrl Pts',(21.2831563307876,19.4463762970337,-14.9549512355422));
#47040=CARTESIAN_POINT('Ctrl Pts',(21.2911576353439,19.3597211137333,-14.9592673982811));
#47041=CARTESIAN_POINT('Ctrl Pts',(21.2947325504218,19.2726883838097,-14.9635835610201));
#47042=CARTESIAN_POINT('Ctrl Pts',(21.2938756072079,19.1857636052079,-14.967899723759));
#47043=CARTESIAN_POINT('Ctrl Pts',(21.293046578829,19.1016703921262,-14.9720752879507));
#47044=CARTESIAN_POINT('Ctrl Pts',(21.2880700686645,19.017678672767,-14.9762508521424));
#47045=CARTESIAN_POINT('Ctrl Pts',(21.2789941177452,18.9342240244488,-14.980426416334));
#47046=CARTESIAN_POINT('Ctrl Pts',(21.269459762121,18.8465542802384,-14.9848128783466));
#47047=CARTESIAN_POINT('Ctrl Pts',(21.2554010498833,18.7594778642491,-14.9891993403591));
#47048=CARTESIAN_POINT('Ctrl Pts',(21.2369341836446,18.6734867700758,-14.9935858023717));
#47049=CARTESIAN_POINT('Ctrl Pts',(21.2184673174058,18.5874956759025,-14.9979722643842));
#47050=CARTESIAN_POINT('Ctrl Pts',(21.1955925215496,18.5025904439986,-15.0023587263968));
#47051=CARTESIAN_POINT('Ctrl Pts',(21.1684852750763,18.4192415485537,-15.0067451884093));
#47052=CARTESIAN_POINT('Ctrl Pts',(21.1426252731958,18.3397276593411,-15.0109298228024));
#47053=CARTESIAN_POINT('Ctrl Pts',(21.1128174886273,18.2613340692511,-15.0151144571954));
#47054=CARTESIAN_POINT('Ctrl Pts',(21.0791777662536,18.1844810061817,-15.0192990915885));
#47055=CARTESIAN_POINT('Ctrl Pts',(21.0455859258609,18.1077373339352,-15.0234777696724));
#47056=CARTESIAN_POINT('Ctrl Pts',(21.0081731644857,18.0325302510435,-15.0276564477564));
#47057=CARTESIAN_POINT('Ctrl Pts',(20.9671048559809,17.9592641244279,-15.0318351258403));
#47058=CARTESIAN_POINT('Ctrl Pts',(20.9253004275615,17.8846847551481,-15.0360887037257));
#47059=CARTESIAN_POINT('Ctrl Pts',(20.8797082607491,17.8121170683452,-15.0403422816112));
#47060=CARTESIAN_POINT('Ctrl Pts',(20.8305537911316,17.7419655548996,-15.0445958594966));
#47061=CARTESIAN_POINT('Ctrl Pts',(20.7823522768247,17.6731740654314,-15.0487669734745));
#47062=CARTESIAN_POINT('Ctrl Pts',(20.7307256276405,17.6067062949759,-15.0529380874525));
#47063=CARTESIAN_POINT('Ctrl Pts',(20.675931463843,17.5429166118756,-15.0571092014304));
#47064=CARTESIAN_POINT('Ctrl Pts',(20.6211556867563,17.4791483340195,-15.0612789157508));
#47065=CARTESIAN_POINT('Ctrl Pts',(20.5632148054787,17.4180567074447,-15.0654486300712));
#47066=CARTESIAN_POINT('Ctrl Pts',(20.5024068820801,17.3599632366126,-15.0696183443916));
#47067=CARTESIAN_POINT('Ctrl Pts',(20.4416011224884,17.3018718329955,-15.0737879103356));
#47068=CARTESIAN_POINT('Ctrl Pts',(20.3779288568417,17.2467786901665,-15.0779574762796));
#47069=CARTESIAN_POINT('Ctrl Pts',(20.3117241899802,17.1949676638627,-15.0821270422237));
#47070=CARTESIAN_POINT('Ctrl Pts',(20.2431918487043,17.1413350257899,-15.0864432049626));
#47071=CARTESIAN_POINT('Ctrl Pts',(20.1719461297948,17.0912199219507,-15.0907593677015));
#47072=CARTESIAN_POINT('Ctrl Pts',(20.0983923000268,17.0448897415811,-15.0950755304404));
#47073=CARTESIAN_POINT('Ctrl Pts',(20.0272344785269,17.000068761964,-15.0992510946321));
#47074=CARTESIAN_POINT('Ctrl Pts',(19.9539170439586,16.9587900948023,-15.1034266588238));
#47075=CARTESIAN_POINT('Ctrl Pts',(19.8788322516137,16.921249114933,-15.1076022230155));
#47076=CARTESIAN_POINT('Ctrl Pts',(19.7999551049048,16.8818120294157,-15.111988685028));
#47077=CARTESIAN_POINT('Ctrl Pts',(19.7191279049099,16.846500369128,-15.1163751470405));
#47078=CARTESIAN_POINT('Ctrl Pts',(19.6368272386529,16.8154827328641,-15.1207616090531));
#47079=CARTESIAN_POINT('Ctrl Pts',(19.5545265723959,16.7844650966001,-15.1251480710656));
#47080=CARTESIAN_POINT('Ctrl Pts',(19.470753015767,16.7577415882257,-15.1295345330781));
#47081=CARTESIAN_POINT('Ctrl Pts',(19.3859971465604,16.7354193164275,-15.1339209950907));
#47082=CARTESIAN_POINT('Ctrl Pts',(19.3051410205342,16.7141241254443,-15.1381056294837));
#47083=CARTESIAN_POINT('Ctrl Pts',(19.2230900288855,16.6967547916185,-15.1422902638768));
#47084=CARTESIAN_POINT('Ctrl Pts',(19.140260221412,16.6834413691275,-15.1464748982698));
#47085=CARTESIAN_POINT('Ctrl Pts',(19.0575483119171,16.6701468966454,-15.1506535763538));
#47086=CARTESIAN_POINT('Ctrl Pts',(18.9740602388407,16.66089694071,-15.1548322544377));
#47087=CARTESIAN_POINT('Ctrl Pts',(18.8902255245013,16.6557713242267,-15.1590109325216));
#47088=CARTESIAN_POINT('Ctrl Pts',(18.8048881331583,16.6505538347516,-15.1632645104071));
#47089=CARTESIAN_POINT('Ctrl Pts',(18.7191920174707,16.6496101194126,-15.1675180882925));
#47090=CARTESIAN_POINT('Ctrl Pts',(18.6335993142648,16.652969565798,-15.171771666178));
#47091=CARTESIAN_POINT('Ctrl Pts',(18.549665992631,16.6562638827597,-15.1759427801559));
#47092=CARTESIAN_POINT('Ctrl Pts',(18.4658325904041,16.6636959811426,-15.1801138941339));
#47093=CARTESIAN_POINT('Ctrl Pts',(18.3825365202428,16.6752410559367,-15.1842850081118));
#47094=CARTESIAN_POINT('Ctrl Pts',(18.2992684008824,16.6867822566694,-15.1884547224322));
#47095=CARTESIAN_POINT('Ctrl Pts',(18.2165377107927,16.70243362971,-15.1926244367525));
#47096=CARTESIAN_POINT('Ctrl Pts',(18.1347761196918,16.7221185762941,-15.1967941510729));
#47097=CARTESIAN_POINT('Ctrl Pts',(18.0530174380192,16.7418028224032,-15.200963717017));
#47098=CARTESIAN_POINT('Ctrl Pts',(17.9722282338244,16.7655202481684,-15.205133282961));
#47099=CARTESIAN_POINT('Ctrl Pts',(17.8928280294743,16.7931435700187,-15.209302848905));
#47100=CARTESIAN_POINT('Ctrl Pts',(17.8106362118899,16.8217380937883,-15.213619011644));
#47101=CARTESIAN_POINT('Ctrl Pts',(17.7299333840843,16.8545181133117,-15.2179351743829));
#47102=CARTESIAN_POINT('Ctrl Pts',(17.6511637413086,16.891287596088,-15.2222513371218));
#47103=CARTESIAN_POINT('Ctrl Pts',(17.5749600113613,16.9268593168303,-15.2264269013135));
#47104=CARTESIAN_POINT('Ctrl Pts',(17.5005658480124,16.966164316944,-15.2306024655052));
#47105=CARTESIAN_POINT('Ctrl Pts',(17.4283578509306,17.0089785244977,-15.2347780296969));
#47106=CARTESIAN_POINT('Ctrl Pts',(17.3525027995743,17.0539551758939,-15.2391644917094));
#47107=CARTESIAN_POINT('Ctrl Pts',(17.2790610511154,17.1028045279329,-15.243550953722));
#47108=CARTESIAN_POINT('Ctrl Pts',(17.2084323379752,17.1552171056787,-15.2479374157345));
#47109=CARTESIAN_POINT('Ctrl Pts',(17.137803624835,17.2076296834245,-15.252323877747));
#47110=CARTESIAN_POINT('Ctrl Pts',(17.0699883460668,17.2636050588652,-15.2567103397596));
#47111=CARTESIAN_POINT('Ctrl Pts',(17.0053421035811,17.3227887096121,-15.2610968017721));
#47112=CARTESIAN_POINT('Ctrl Pts',(16.9445899812052,17.3784072924496,-15.2652190348167));
#47113=CARTESIAN_POINT('Ctrl Pts',(16.8863955977243,17.4370795204071,-15.2693412678613));
#47114=CARTESIAN_POINT('Ctrl Pts',(16.8310887538612,17.4985372152019,-15.2734635009059));
#47115=CARTESIAN_POINT('Ctrl Pts',(16.7758743514516,17.5598921878336,-15.2775788439313));
#47116=CARTESIAN_POINT('Ctrl Pts',(16.7235382140142,17.6240230272318,-15.2816941869568));
#47117=CARTESIAN_POINT('Ctrl Pts',(16.6743754759291,17.6906228034315,-15.2858095299822));
#47118=CARTESIAN_POINT('Ctrl Pts',(16.6252589923635,17.7571599195604,-15.2899210011074));
#47119=CARTESIAN_POINT('Ctrl Pts',(16.5793102664133,17.8261609852053,-15.2940324722327));
#47120=CARTESIAN_POINT('Ctrl Pts',(16.5367853878605,17.8972846776411,-15.2981439433579));
#47121=CARTESIAN_POINT('Ctrl Pts',(16.4942868717928,17.9683642783041,-15.3022528656553));
#47122=CARTESIAN_POINT('Ctrl Pts',(16.4552082342176,18.0415634879277,-15.3063617879526));
#47123=CARTESIAN_POINT('Ctrl Pts',(16.4197623875935,18.1165118669794,-15.31047071025));
#47124=CARTESIAN_POINT('Ctrl Pts',(16.3843271437776,18.1914378269504,-15.3145784034579));
#47125=CARTESIAN_POINT('Ctrl Pts',(16.3525227351488,18.2681114878987,-15.3186860966658));
#47126=CARTESIAN_POINT('Ctrl Pts',(16.3245154961046,18.3461390715913,-15.3227937898737));
#47127=CARTESIAN_POINT('Ctrl Pts',(16.2964946934756,18.4242044431483,-15.3269034723904));
#47128=CARTESIAN_POINT('Ctrl Pts',(16.2722748983311,18.5036246009546,-15.331013154907));
#47129=CARTESIAN_POINT('Ctrl Pts',(16.2519734104525,18.5839880313907,-15.3351228374237));
#47130=CARTESIAN_POINT('Ctrl Pts',(16.2316667383952,18.664371983396,-15.339233569387));
#47131=CARTESIAN_POINT('Ctrl Pts',(16.2152804642371,18.7456992225571,-15.3433443013503));
#47132=CARTESIAN_POINT('Ctrl Pts',(16.2028808242116,18.8275476327413,-15.3474550333136));
#47133=CARTESIAN_POINT('Ctrl Pts',(16.1904661338127,18.9094953884816,-15.3515707547807));
#47134=CARTESIAN_POINT('Ctrl Pts',(16.1820477886727,18.9919651056506,-15.3556864762478));
#47135=CARTESIAN_POINT('Ctrl Pts',(16.1776401048969,19.0745299054429,-15.3598021977149));
#47136=CARTESIAN_POINT('Ctrl Pts',(16.175174200724,19.1207212600628,-15.3621047618861));
#47137=CARTESIAN_POINT('Ctrl Pts',(16.173962657598,19.1669423575626,-15.3644073260573));
#47138=CARTESIAN_POINT('Ctrl Pts',(16.1740008768645,19.213118854712,-15.3667098902285));
#47139=CARTESIAN_POINT('Origin',(18.734,19.211,1.76670989022852));
#47140=CARTESIAN_POINT('',(20.2909850521016,21.2378231040073,-14.0501277863708));
#47141=CARTESIAN_POINT('',(20.2961055941918,21.2444717899281,-14.1167030457843));
#47142=CARTESIAN_POINT('',(20.2935358855687,21.2411349269503,1.76670989022852));
#47143=CARTESIAN_POINT('',(16.1738766799073,19.2098698167329,-14.6332901097715));
#47144=CARTESIAN_POINT('Ctrl Pts',(20.2961055941918,21.2444717899281,-14.1167030457843));
#47145=CARTESIAN_POINT('Ctrl Pts',(20.9598513200281,20.733315419597,-14.1585606280004));
#47146=CARTESIAN_POINT('Ctrl Pts',(21.7469835110905,18.9872885505905,-14.2428101457769));
#47147=CARTESIAN_POINT('Ctrl Pts',(20.188947426677,16.556490896078,-14.369451599114));
#47148=CARTESIAN_POINT('Ctrl Pts',(17.2895133755746,16.5507840333809,-14.4966274057954));
#47149=CARTESIAN_POINT('Ctrl Pts',(16.200898327955,18.2345794040693,-14.5845735760146));
#47150=CARTESIAN_POINT('Ctrl Pts',(16.1700292343928,19.1465375881033,-14.6301278106733));
#47151=CARTESIAN_POINT('Ctrl Pts',(16.1703790132248,19.209868272665,-14.6332901097715));
#47152=CARTESIAN_POINT('Ctrl Pts',(16.1740002494514,19.2098698712835,-14.6332901097715));
#47153=CARTESIAN_POINT('Ctrl Pts',(16.1739637014967,19.2926593390013,-14.6374299052976));
#47154=CARTESIAN_POINT('Ctrl Pts',(16.1779474618949,19.3756125071059,-14.6415697008237));
#47155=CARTESIAN_POINT('Ctrl Pts',(16.1859729132155,19.4583013647604,-14.6457094963498));
#47156=CARTESIAN_POINT('Ctrl Pts',(16.1939875490477,19.5408787868903,-14.6498437128862));
#47157=CARTESIAN_POINT('Ctrl Pts',(16.2060330170348,19.6231921412973,-14.6539779294227));
#47158=CARTESIAN_POINT('Ctrl Pts',(16.2220786798975,19.7048130026784,-14.6581121459591));
#47159=CARTESIAN_POINT('Ctrl Pts',(16.2381078732804,19.7863500873324,-14.6622421190812));
#47160=CARTESIAN_POINT('Ctrl Pts',(16.2581290152452,19.8671956313601,-14.6663720922033));
#47161=CARTESIAN_POINT('Ctrl Pts',(16.2820597821147,19.9469274202778,-14.6705020653254));
#47162=CARTESIAN_POINT('Ctrl Pts',(16.3059775967094,20.0266160552067,-14.6746298031431));
#47163=CARTESIAN_POINT('Ctrl Pts',(16.3338007023326,20.1051916814476,-14.6787575409609));
#47164=CARTESIAN_POINT('Ctrl Pts',(16.3653962152437,20.1822446194642,-14.6828852787787));
#47165=CARTESIAN_POINT('Ctrl Pts',(16.3969845852851,20.2592801379472,-14.6870120834293));
#47166=CARTESIAN_POINT('Ctrl Pts',(16.4323434905921,20.3347932165774,-14.69113888808));
#47167=CARTESIAN_POINT('Ctrl Pts',(16.4712914723381,20.4083930511099,-14.6952656927307));
#47168=CARTESIAN_POINT('Ctrl Pts',(16.5102429241535,20.4819994430175,-14.6993928650588));
#47169=CARTESIAN_POINT('Ctrl Pts',(16.5527838651363,20.5536918375771,-14.703520037387));
#47170=CARTESIAN_POINT('Ctrl Pts',(16.5986870593961,20.6231043324377,-14.7076472097152));
#47171=CARTESIAN_POINT('Ctrl Pts',(16.6446377721104,20.6925886823084,-14.7117786544444));
#47172=CARTESIAN_POINT('Ctrl Pts',(16.6939574240325,20.7597880294055,-14.7159100991735));
#47173=CARTESIAN_POINT('Ctrl Pts',(16.7463760416131,20.8243663564257,-14.7200415439027));
#47174=CARTESIAN_POINT('Ctrl Pts',(16.7988250781885,20.8889821588294,-14.7241753861463));
#47175=CARTESIAN_POINT('Ctrl Pts',(16.8543763437708,20.9509735655353,-14.7283092283899));
#47176=CARTESIAN_POINT('Ctrl Pts',(16.9127219511763,21.0100403744422,-14.7324430706336));
#47177=CARTESIAN_POINT('Ctrl Pts',(16.9711635405887,21.0692043517755,-14.7365837132945));
#47178=CARTESIAN_POINT('Ctrl Pts',(17.0324082986529,21.1254338132414,-14.7407243559553));
#47179=CARTESIAN_POINT('Ctrl Pts',(17.0961145829399,21.1784682616454,-14.7448649986162));
#47180=CARTESIAN_POINT('Ctrl Pts',(17.1274705472745,21.2045715933853,-14.7469030054636));
#47181=CARTESIAN_POINT('Ctrl Pts',(17.1594223751536,21.2299015689542,-14.7489410123109));
#47182=CARTESIAN_POINT('Ctrl Pts',(17.1919269101815,21.2544310817,-14.7509790191583));
#47183=CARTESIAN_POINT('Ctrl Pts',(17.2586683911457,21.3047974692387,-14.7551636535514));
#47184=CARTESIAN_POINT('Ctrl Pts',(17.3280042311,21.3519843348469,-14.7593482879444));
#47185=CARTESIAN_POINT('Ctrl Pts',(17.3995987737075,21.395713566413,-14.7635329223375));
#47186=CARTESIAN_POINT('Ctrl Pts',(17.4710914103449,21.4393805548304,-14.7677116004214));
#47187=CARTESIAN_POINT('Ctrl Pts',(17.5448359744303,21.4795994471399,-14.7718902785053));
#47188=CARTESIAN_POINT('Ctrl Pts',(17.6204652949927,21.5161335017183,-14.7760689565893));
#47189=CARTESIAN_POINT('Ctrl Pts',(17.6974502167725,21.5533224029686,-14.7803225344747));
#47190=CARTESIAN_POINT('Ctrl Pts',(17.7763877432988,21.5866927752842,-14.7845761123601));
#47191=CARTESIAN_POINT('Ctrl Pts',(17.8568613993343,21.616042177431,-14.7888296902455));
#47192=CARTESIAN_POINT('Ctrl Pts',(17.9357749165162,21.6448225841466,-14.7930008042235));
#47193=CARTESIAN_POINT('Ctrl Pts',(18.0161650808992,21.6697363732161,-14.7971719182015));
#47194=CARTESIAN_POINT('Ctrl Pts',(18.0976177441658,21.6906406240541,-14.8013430321794));
#47195=CARTESIAN_POINT('Ctrl Pts',(18.1790430752045,21.7115378602688,-14.8055127464998));
#47196=CARTESIAN_POINT('Ctrl Pts',(18.2615297518276,21.7284281160528,-14.8096824608201));
#47197=CARTESIAN_POINT('Ctrl Pts',(18.34464929881,21.7412185738554,-14.8138521751405));
#47198=CARTESIAN_POINT('Ctrl Pts',(18.4277658880424,21.7540085765186,-14.8180217410846));
#47199=CARTESIAN_POINT('Ctrl Pts',(18.5115148480473,21.7626990021398,-14.8221913070286));
#47200=CARTESIAN_POINT('Ctrl Pts',(18.5954597232797,21.7672485387235,-14.8263608729727));
#47201=CARTESIAN_POINT('Ctrl Pts',(18.6823559967678,21.7719580314011,-14.8306770357116));
#47202=CARTESIAN_POINT('Ctrl Pts',(18.7694616919208,21.7722300013651,-14.8349931984505));
#47203=CARTESIAN_POINT('Ctrl Pts',(18.8562914526108,21.7680773943349,-14.8393093611894));
#47204=CARTESIAN_POINT('Ctrl Pts',(18.9402927429791,21.7640600580418,-14.8434849253811));
#47205=CARTESIAN_POINT('Ctrl Pts',(19.0240353356991,21.7559020718403,-14.8476604895728));
#47206=CARTESIAN_POINT('Ctrl Pts',(19.1070857885135,21.7436679597628,-14.8518360537644));
#47207=CARTESIAN_POINT('Ctrl Pts',(19.1943309222659,21.7308159317682,-14.856222515777));
#47208=CARTESIAN_POINT('Ctrl Pts',(19.2808115861344,21.7134653009972,-14.8606089777895));
#47209=CARTESIAN_POINT('Ctrl Pts',(19.3660405469233,21.691750843403,-14.864995439802));
#47210=CARTESIAN_POINT('Ctrl Pts',(19.4512695077122,21.6700363858089,-14.8693819018146));
#47211=CARTESIAN_POINT('Ctrl Pts',(19.5352462338658,21.6439583461085,-14.8737683638271));
#47212=CARTESIAN_POINT('Ctrl Pts',(19.6175072439392,21.6137099179691,-14.8781548258396));
#47213=CARTESIAN_POINT('Ctrl Pts',(19.6959730538369,21.5848570335956,-14.8823389137094));
#47214=CARTESIAN_POINT('Ctrl Pts',(19.7731699980662,21.5521027093326,-14.8865230015791));
#47215=CARTESIAN_POINT('Ctrl Pts',(19.8486827058602,21.5155785873466,-14.8907070894488));
#47216=CARTESIAN_POINT('Ctrl Pts',(19.9270438215451,21.4776767423214,-14.8950490049114));
#47217=CARTESIAN_POINT('Ctrl Pts',(20.003590624008,21.4357151321965,-14.899390920374));
#47218=CARTESIAN_POINT('Ctrl Pts',(20.0778772783341,21.3898973956516,-14.9037328358367));
#47219=CARTESIAN_POINT('Ctrl Pts',(20.1521639326601,21.3440796591068,-14.9080747512993));
#47220=CARTESIAN_POINT('Ctrl Pts',(20.2241899272934,21.2944060218976,-14.9124166667619));
#47221=CARTESIAN_POINT('Ctrl Pts',(20.2935358855687,21.2411349269503,-14.9167585822245));
#47222=CARTESIAN_POINT('',(16.17436451349,19.211560173865,-14.5667099150528));
#47223=CARTESIAN_POINT('Ctrl Pts',(16.1740000613162,19.211560302475,-14.5667099174729));
#47224=CARTESIAN_POINT('Ctrl Pts',(16.1740197372987,19.30145909156,-14.5711571992719));
#47225=CARTESIAN_POINT('Ctrl Pts',(16.1787790795977,19.3912344818004,-14.5756044810709));
#47226=CARTESIAN_POINT('Ctrl Pts',(16.1882138900509,19.4803939167657,-14.5800517628699));
#47227=CARTESIAN_POINT('Ctrl Pts',(16.1976832329532,19.5698796851174,-14.5845153222118));
#47228=CARTESIAN_POINT('Ctrl Pts',(16.2118622325346,19.6587446305158,-14.5889788815537));
#47229=CARTESIAN_POINT('Ctrl Pts',(16.2306352202496,19.7465042292131,-14.5934424408955));
#47230=CARTESIAN_POINT('Ctrl Pts',(16.2494446598929,19.8344342326776,-14.59791466723));
#47231=CARTESIAN_POINT('Ctrl Pts',(16.2728657964751,19.9212542602436,-14.6023868935645));
#47232=CARTESIAN_POINT('Ctrl Pts',(16.3007333122769,20.0064955854165,-14.606859119899));
#47233=CARTESIAN_POINT('Ctrl Pts',(16.3286838403156,20.0919908289195,-14.6113446681784));
#47234=CARTESIAN_POINT('Ctrl Pts',(16.3611071025133,20.175897631469,-14.6158302164578));
#47235=CARTESIAN_POINT('Ctrl Pts',(16.3977895032108,20.2577666954446,-14.6203157647373));
#47236=CARTESIAN_POINT('Ctrl Pts',(16.4111522146037,20.2875900617759,-14.6219497659465));
#47237=CARTESIAN_POINT('Ctrl Pts',(16.4250796827617,20.3171432681483,-14.6235837671557));
#47238=CARTESIAN_POINT('Ctrl Pts',(16.4395601204677,20.3464054955,-14.625217768365));
#47239=CARTESIAN_POINT('Ctrl Pts',(16.4766441429939,20.4213452949944,-14.629402402758));
#47240=CARTESIAN_POINT('Ctrl Pts',(16.5174725051856,20.4946058152549,-14.633587037151));
#47241=CARTESIAN_POINT('Ctrl Pts',(16.5618698248528,20.5657879916116,-14.6377716715441));
#47242=CARTESIAN_POINT('Ctrl Pts',(16.6062039504308,20.636868848951,-14.641950349628));
#47243=CARTESIAN_POINT('Ctrl Pts',(16.6540967016935,20.7058768514384,-14.646129027712));
#47244=CARTESIAN_POINT('Ctrl Pts',(16.7053259809371,20.7724357893872,-14.6503077057959));
#47245=CARTESIAN_POINT('Ctrl Pts',(16.7574735081934,20.8401877484638,-14.6545612836814));
#47246=CARTESIAN_POINT('Ctrl Pts',(16.8130781406444,20.9054015483267,-14.6588148615668));
#47247=CARTESIAN_POINT('Ctrl Pts',(16.8718583319471,20.9677095400496,-14.6630684394523));
#47248=CARTESIAN_POINT('Ctrl Pts',(16.9294989545412,21.0288095697688,-14.6672395534302));
#47249=CARTESIAN_POINT('Ctrl Pts',(16.9901927757377,21.0871151053885,-14.6714106674082));
#47250=CARTESIAN_POINT('Ctrl Pts',(17.0536336491124,21.1423127470207,-14.6755817813861));
#47251=CARTESIAN_POINT('Ctrl Pts',(17.1170532342894,21.1974918665512,-14.6797514957065));
#47252=CARTESIAN_POINT('Ctrl Pts',(17.1832176941668,21.249564861567,-14.6839212100268));
#47253=CARTESIAN_POINT('Ctrl Pts',(17.2517856166925,21.2982566976576,-14.6880909243472));
#47254=CARTESIAN_POINT('Ctrl Pts',(17.3203510992774,21.3469468010837,-14.6922604902913));
#47255=CARTESIAN_POINT('Ctrl Pts',(17.3913194988898,21.3922557191442,-14.6964300562353));
#47256=CARTESIAN_POINT('Ctrl Pts',(17.4643191824367,21.4339508814888,-14.7005996221793));
#47257=CARTESIAN_POINT('Ctrl Pts',(17.5398854448023,21.4771119943049,-14.7049157849183));
#47258=CARTESIAN_POINT('Ctrl Pts',(17.6176280306767,21.5164002423865,-14.7092319476572));
#47259=CARTESIAN_POINT('Ctrl Pts',(17.6971072733111,21.5516096371116,-14.7135481103961));
#47260=CARTESIAN_POINT('Ctrl Pts',(17.7739974879763,21.5856720895068,-14.7177236745878));
#47261=CARTESIAN_POINT('Ctrl Pts',(17.8525124972024,21.6159172197027,-14.7218992387795));
#47262=CARTESIAN_POINT('Ctrl Pts',(17.9322359204944,21.6422084157502,-14.7260748029711));
#47263=CARTESIAN_POINT('Ctrl Pts',(18.0159859843726,21.6698275176087,-14.7304612649837));
#47264=CARTESIAN_POINT('Ctrl Pts',(18.1010691812453,21.6930826078308,-14.7348477269962));
#47265=CARTESIAN_POINT('Ctrl Pts',(18.1869895560291,21.7118757614457,-14.7392341890088));
#47266=CARTESIAN_POINT('Ctrl Pts',(18.2729099308129,21.7306689150606,-14.7436206510213));
#47267=CARTESIAN_POINT('Ctrl Pts',(18.3596668986516,21.7450001125529,-14.7480071130339));
#47268=CARTESIAN_POINT('Ctrl Pts',(18.4467595506039,21.7548342957494,-14.7523935750464));
#47269=CARTESIAN_POINT('Ctrl Pts',(18.5298216106109,21.7642133592694,-14.7565770344168));
#47270=CARTESIAN_POINT('Ctrl Pts',(18.6134980569014,21.7695373443218,-14.7607604937872));
#47271=CARTESIAN_POINT('Ctrl Pts',(18.6973587722112,21.7707377639958,-14.7649439531576));
#47272=CARTESIAN_POINT('Ctrl Pts',(18.7811102468207,21.7719366199497,-14.7691219629677));
#47273=CARTESIAN_POINT('Ctrl Pts',(18.8650450584586,21.7690225671106,-14.7732999727777));
#47274=CARTESIAN_POINT('Ctrl Pts',(18.9487268680233,21.761978708682,-14.7774779825878));
#47275=CARTESIAN_POINT('Ctrl Pts',(19.0323247810394,21.7549419121873,-14.7816518036666));
#47276=CARTESIAN_POINT('Ctrl Pts',(19.1156697399229,21.743783570225,-14.7858256247455));
#47277=CARTESIAN_POINT('Ctrl Pts',(19.1983256615625,21.7285388140036,-14.7899994458244));
#47278=CARTESIAN_POINT('Ctrl Pts',(19.2809235142162,21.7133047678138,-14.7941703346324));
#47279=CARTESIAN_POINT('Ctrl Pts',(19.3628328402605,21.693990093863,-14.7983412234403));
#47280=CARTESIAN_POINT('Ctrl Pts',(19.4436242958245,21.6706815563759,-14.8025121122483));
#47281=CARTESIAN_POINT('Ctrl Pts',(19.5244040000542,21.6473764091781,-14.8066823943892));
#47282=CARTESIAN_POINT('Ctrl Pts',(19.6040657115569,21.6200786673617,-14.8108526765302));
#47283=CARTESIAN_POINT('Ctrl Pts',(19.6821928869638,21.588925618919,-14.8150229586712));
#47284=CARTESIAN_POINT('Ctrl Pts',(19.7603101594136,21.5577765192598,-14.8191927122108));
#47285=CARTESIAN_POINT('Ctrl Pts',(19.8368928571116,21.5227732602624,-14.8233624657505));
#47286=CARTESIAN_POINT('Ctrl Pts',(19.9115437773165,21.4841015490961,-14.8275322192902));
#47287=CARTESIAN_POINT('Ctrl Pts',(19.9862468140608,21.445402839793,-14.8317048838875));
#47288=CARTESIAN_POINT('Ctrl Pts',(20.0590149720293,21.4030307779422,-14.8358775484847));
#47289=CARTESIAN_POINT('Ctrl Pts',(20.129475672665,21.3572170549597,-14.8400502130819));
#47290=CARTESIAN_POINT('Ctrl Pts',(20.1856889996356,21.3206670098067,-14.8433791518695));
#47291=CARTESIAN_POINT('Ctrl Pts',(20.2404341027343,21.2819273564674,-14.846708090657));
#47292=CARTESIAN_POINT('Ctrl Pts',(20.2935358855687,21.2411349269503,-14.8500370294445));
#47293=CARTESIAN_POINT('Ctrl Pts',(20.2909850521016,21.2378231040073,-14.0501277863708));
#47294=CARTESIAN_POINT('Ctrl Pts',(20.6448529615788,20.9653099953601,-14.0722567047936));
#47295=CARTESIAN_POINT('Ctrl Pts',(21.48038594828,19.9142910878859,-14.1367775587769));
#47296=CARTESIAN_POINT('Ctrl Pts',(21.2244734734613,17.4902926282723,-14.2436903483206));
#47297=CARTESIAN_POINT('Ctrl Pts',(18.6352034638416,16.1855196702712,-14.3708661550021));
#47298=CARTESIAN_POINT('Ctrl Pts',(16.5197423492181,17.430869440195,-14.478539335638));
#47299=CARTESIAN_POINT('Ctrl Pts',(16.1790023518676,18.7496082788979,-14.5438205807135));
#47300=CARTESIAN_POINT('Ctrl Pts',(16.1781028428963,19.2115588546613,-14.5667098902285));
#47301=CARTESIAN_POINT('Origin',(18.734,19.211,1.76670989022852));
#47302=CARTESIAN_POINT('',(20.2935358855687,21.2411349269503,-13.2501880127039));
#47303=CARTESIAN_POINT('',(20.2935358855687,21.2411349269503,-13.3166223773735));
#47304=CARTESIAN_POINT('',(20.2935358855687,21.2411349269503,1.76670989022852));
#47305=CARTESIAN_POINT('',(16.1740010575059,19.2133268925441,-13.8332901097715));
#47306=CARTESIAN_POINT('Ctrl Pts',(20.2935358855687,21.2411349269503,-13.3166223773735));
#47307=CARTESIAN_POINT('Ctrl Pts',(20.3602103291409,21.1899160714837,-13.3207986505334));
#47308=CARTESIAN_POINT('Ctrl Pts',(20.4243042199467,21.1354511939907,-13.3249749236932));
#47309=CARTESIAN_POINT('Ctrl Pts',(20.4855003216615,21.07804221249,-13.329151196853));
#47310=CARTESIAN_POINT('Ctrl Pts',(20.5468041075984,21.0205322108043,-13.3333348188261));
#47311=CARTESIAN_POINT('Ctrl Pts',(20.6051995980666,20.9600680873566,-13.3375184407992));
#47312=CARTESIAN_POINT('Ctrl Pts',(20.6604076888247,20.8969873713753,-13.3417020627724));
#47313=CARTESIAN_POINT('Ctrl Pts',(20.7059042993841,20.8450029841342,-13.3451497570691));
#47314=CARTESIAN_POINT('Ctrl Pts',(20.7492369226164,20.7912423162171,-13.3485974513658));
#47315=CARTESIAN_POINT('Ctrl Pts',(20.7902715950829,20.7359088914605,-13.3520451456625));
#47316=CARTESIAN_POINT('Ctrl Pts',(20.8400773745207,20.6687480203407,-13.3562297800555));
#47317=CARTESIAN_POINT('Ctrl Pts',(20.886682020299,20.5990195040797,-13.3604144144486));
#47318=CARTESIAN_POINT('Ctrl Pts',(20.9298102405871,20.5270613159473,-13.3645990488416));
#47319=CARTESIAN_POINT('Ctrl Pts',(20.9728770731918,20.4552055513889,-13.3687777269256));
#47320=CARTESIAN_POINT('Ctrl Pts',(21.0124770746365,20.3811268100632,-13.3729564050095));
#47321=CARTESIAN_POINT('Ctrl Pts',(21.0483765860078,20.3051942323642,-13.3771350830935));
#47322=CARTESIAN_POINT('Ctrl Pts',(21.0849195703198,20.2279006177817,-13.3813886609789));
#47323=CARTESIAN_POINT('Ctrl Pts',(21.1176278099319,20.1486864403634,-13.3856422388643));
#47324=CARTESIAN_POINT('Ctrl Pts',(21.1463023579537,20.0679698558355,-13.3898958167498));
#47325=CARTESIAN_POINT('Ctrl Pts',(21.1744209939084,19.9888181198042,-13.3940669307277));
#47326=CARTESIAN_POINT('Ctrl Pts',(21.1986607834443,19.9082221644554,-13.3982380447057));
#47327=CARTESIAN_POINT('Ctrl Pts',(21.2188822787495,19.8265973202967,-13.4024091586836));
#47328=CARTESIAN_POINT('Ctrl Pts',(21.2390969885367,19.7449998661427,-13.406578873004));
#47329=CARTESIAN_POINT('Ctrl Pts',(21.2552959714612,19.6623746550204,-13.4107485873244));
#47330=CARTESIAN_POINT('Ctrl Pts',(21.2673900009521,19.5791509243178,-13.4149183016447));
#47331=CARTESIAN_POINT('Ctrl Pts',(21.2794836000854,19.4959301550728,-13.4190878675888));
#47332=CARTESIAN_POINT('Ctrl Pts',(21.2874724709,19.4121113639668,-13.4232574335328));
#47333=CARTESIAN_POINT('Ctrl Pts',(21.2913189573957,19.3281313371597,-13.4274269994769));
#47334=CARTESIAN_POINT('Ctrl Pts',(21.2953006816113,19.2411986762106,-13.4317431622158));
#47335=CARTESIAN_POINT('Ctrl Pts',(21.2948432851383,19.1540937573815,-13.4360593249547));
#47336=CARTESIAN_POINT('Ctrl Pts',(21.2899637772452,19.0673018113879,-13.4403754876936));
#47337=CARTESIAN_POINT('Ctrl Pts',(21.2852432188086,18.9833371039062,-13.4445510518853));
#47338=CARTESIAN_POINT('Ctrl Pts',(21.2763843217563,18.89966575566,-13.448726616077));
#47339=CARTESIAN_POINT('Ctrl Pts',(21.2634552371753,18.8167206534363,-13.4529021802687));
#47340=CARTESIAN_POINT('Ctrl Pts',(21.249873135268,18.7295861912824,-13.4572886422812));
#47341=CARTESIAN_POINT('Ctrl Pts',(21.2317989893781,18.6432538400943,-13.4616751042937));
#47342=CARTESIAN_POINT('Ctrl Pts',(21.2093716504547,18.5582096874759,-13.4660615663063));
#47343=CARTESIAN_POINT('Ctrl Pts',(21.1869443115313,18.4731655348574,-13.4704480283188));
#47344=CARTESIAN_POINT('Ctrl Pts',(21.1601640287335,18.3894101102965,-13.4748344903314));
#47345=CARTESIAN_POINT('Ctrl Pts',(21.1292278697973,18.3074052613331,-13.4792209523439));
#47346=CARTESIAN_POINT('Ctrl Pts',(21.0997151293921,18.2291735770309,-13.4834055867369));
#47347=CARTESIAN_POINT('Ctrl Pts',(21.0663106928263,18.1522437219301,-13.48759022113));
#47348=CARTESIAN_POINT('Ctrl Pts',(21.0291497318876,18.0770301114155,-13.491774855523));
#47349=CARTESIAN_POINT('Ctrl Pts',(20.9920416649771,18.0019235581658,-13.495953533607));
#47350=CARTESIAN_POINT('Ctrl Pts',(20.9511878964457,17.9285288061218,-13.5001322116909));
#47351=CARTESIAN_POINT('Ctrl Pts',(20.9067723398089,17.8572421341461,-13.5043108897749));
#47352=CARTESIAN_POINT('Ctrl Pts',(20.8615606662404,17.7846776998082,-13.5085644676603));
#47353=CARTESIAN_POINT('Ctrl Pts',(20.8126584286881,17.7142981146648,-13.5128180455458));
#47354=CARTESIAN_POINT('Ctrl Pts',(20.7603095437651,17.6464970013302,-13.5170716234312));
#47355=CARTESIAN_POINT('Ctrl Pts',(20.7089755441266,17.5800103448805,-13.5212427374092));
#47356=CARTESIAN_POINT('Ctrl Pts',(20.6543276385964,17.5160034559035,-13.5254138513871));
#47357=CARTESIAN_POINT('Ctrl Pts',(20.5966395739482,17.4548183984673,-13.5295849653651));
#47358=CARTESIAN_POINT('Ctrl Pts',(20.5389708670873,17.3936538722681,-13.5337546796854));
#47359=CARTESIAN_POINT('Ctrl Pts',(20.4782643424756,17.3353096315038,-13.5379243940058));
#47360=CARTESIAN_POINT('Ctrl Pts',(20.4148326241777,17.2800930396573,-13.5420941083262));
#47361=CARTESIAN_POINT('Ctrl Pts',(20.3514031630525,17.224878412654,-13.5462636742702));
#47362=CARTESIAN_POINT('Ctrl Pts',(20.2852490485945,17.1727915146886,-13.5504332402143));
#47363=CARTESIAN_POINT('Ctrl Pts',(20.2167171663627,17.1241004325619,-13.5546028061583));
#47364=CARTESIAN_POINT('Ctrl Pts',(20.145775787695,17.0736974320547,-13.5589189688972));
#47365=CARTESIAN_POINT('Ctrl Pts',(20.0722867555764,17.0269337896173,-13.5632351316361));
#47366=CARTESIAN_POINT('Ctrl Pts',(19.9966672790437,16.9840578493296,-13.5675512943751));
#47367=CARTESIAN_POINT('Ctrl Pts',(19.9235110990054,16.9425785882871,-13.5717268585667));
#47368=CARTESIAN_POINT('Ctrl Pts',(19.8483615834561,16.9047378049042,-13.5759024227584));
#47369=CARTESIAN_POINT('Ctrl Pts',(19.7716196105687,16.8707125083094,-13.5800779869501));
#47370=CARTESIAN_POINT('Ctrl Pts',(19.6910015830675,16.8349686748712,-13.5844644489626));
#47371=CARTESIAN_POINT('Ctrl Pts',(19.6086265457422,16.8034361069935,-13.5888509109752));
#47372=CARTESIAN_POINT('Ctrl Pts',(19.524978378728,16.7762611630023,-13.5932373729877));
#47373=CARTESIAN_POINT('Ctrl Pts',(19.4413302117138,16.7490862190112,-13.5976238350002));
#47374=CARTESIAN_POINT('Ctrl Pts',(19.3564094950912,16.7262689760049,-13.6020102970128));
#47375=CARTESIAN_POINT('Ctrl Pts',(19.2707112385803,16.7078937205181,-13.6063967590253));
#47376=CARTESIAN_POINT('Ctrl Pts',(19.1889560858867,16.6903639377749,-13.6105813934184));
#47377=CARTESIAN_POINT('Ctrl Pts',(19.1061890642126,16.676811111084,-13.6147660278114));
#47378=CARTESIAN_POINT('Ctrl Pts',(19.0228317972389,16.6673458975514,-13.6189506622045));
#47379=CARTESIAN_POINT('Ctrl Pts',(18.9395931790174,16.6578941565786,-13.6231293402884));
#47380=CARTESIAN_POINT('Ctrl Pts',(18.8557664374668,16.6525185234246,-13.6273080183724));
#47381=CARTESIAN_POINT('Ctrl Pts',(18.771784329296,16.6512788541602,-13.6314866964563));
#47382=CARTESIAN_POINT('Ctrl Pts',(18.6862969021931,16.6500169647151,-13.6357402743417));
#47383=CARTESIAN_POINT('Ctrl Pts',(18.6006489552155,16.6530408729659,-13.6399938522272));
#47384=CARTESIAN_POINT('Ctrl Pts',(18.5153034901262,16.6603585440974,-13.6442474301126));
#47385=CARTESIAN_POINT('Ctrl Pts',(18.4316126134156,16.6675343478947,-13.6484185440906));
#47386=CARTESIAN_POINT('Ctrl Pts',(18.3482130743119,16.6788388732104,-13.6525896580685));
#47387=CARTESIAN_POINT('Ctrl Pts',(18.2655406685,16.6942270951215,-13.6567607720465));
#47388=CARTESIAN_POINT('Ctrl Pts',(18.1828960042124,16.7096101533661,-13.6609304863668));
#47389=CARTESIAN_POINT('Ctrl Pts',(18.100978440524,16.729074102609,-13.6651002006872));
#47390=CARTESIAN_POINT('Ctrl Pts',(18.0202156389592,16.7525224455095,-13.6692699150076));
#47391=CARTESIAN_POINT('Ctrl Pts',(17.9394557112815,16.7759699540173,-13.6734394809516));
#47392=CARTESIAN_POINT('Ctrl Pts',(17.8598509055789,16.8034014451982,-13.6776090468957));
#47393=CARTESIAN_POINT('Ctrl Pts',(17.7818144029991,16.8346703534938,-13.6817786128397));
#47394=CARTESIAN_POINT('Ctrl Pts',(17.701034233257,16.8670386380308,-13.6860947755786));
#47395=CARTESIAN_POINT('Ctrl Pts',(17.6219351912178,16.9035190114424,-13.6904109383175));
#47396=CARTESIAN_POINT('Ctrl Pts',(17.5449519222901,16.9438950908936,-13.6947271010565));
#47397=CARTESIAN_POINT('Ctrl Pts',(17.4704763752506,16.9829559238034,-13.6989026652481));
#47398=CARTESIAN_POINT('Ctrl Pts',(17.3979812574158,17.0256622753737,-13.7030782294398));
#47399=CARTESIAN_POINT('Ctrl Pts',(17.3278323932023,17.0717728821855,-13.7072537936315));
#47400=CARTESIAN_POINT('Ctrl Pts',(17.2541404766203,17.12021242613,-13.7116402556441));
#47401=CARTESIAN_POINT('Ctrl Pts',(17.1830385318339,17.1724088154586,-13.7160267176566));
#47402=CARTESIAN_POINT('Ctrl Pts',(17.1149115381735,17.2280344045394,-13.7204131796691));
#47403=CARTESIAN_POINT('Ctrl Pts',(17.0467845445131,17.2836599936203,-13.7247996416817));
#47404=CARTESIAN_POINT('Ctrl Pts',(16.9816328807927,17.3427143364292,-13.7291861036942));
#47405=CARTESIAN_POINT('Ctrl Pts',(16.919795358022,17.4048268308312,-13.7335725657068));
#47406=CARTESIAN_POINT('Ctrl Pts',(16.8612222805614,17.4636603639818,-13.7377274633762));
#47407=CARTESIAN_POINT('Ctrl Pts',(16.8053896617353,17.5254713783546,-13.7418823610455));
#47408=CARTESIAN_POINT('Ctrl Pts',(16.7526212754374,17.5899699725635,-13.7460372587149));
#47409=CARTESIAN_POINT('Ctrl Pts',(16.70029462084,17.6539286398257,-13.7501573751423));
#47410=CARTESIAN_POINT('Ctrl Pts',(16.650981430094,17.7205297194408,-13.7542774915697));
#47411=CARTESIAN_POINT('Ctrl Pts',(16.6049624110077,17.7894519196813,-13.7583976079971));
#47412=CARTESIAN_POINT('Ctrl Pts',(16.5589874739682,17.8583080987046,-13.7625137777266));
#47413=CARTESIAN_POINT('Ctrl Pts',(16.5163007099123,17.9294805955777,-13.7666299474561));
#47414=CARTESIAN_POINT('Ctrl Pts',(16.4771421768206,18.0026156381539,-13.7707461171856));
#47415=CARTESIAN_POINT('Ctrl Pts',(16.4380086398887,18.0757039962642,-13.7748596594307));
#47416=CARTESIAN_POINT('Ctrl Pts',(16.4023990866292,18.1507519968567,-13.7789732016757));
#47417=CARTESIAN_POINT('Ctrl Pts',(16.3705090605921,18.2273788435904,-13.7830867439208));
#47418=CARTESIAN_POINT('Ctrl Pts',(16.3380758082444,18.3053109799212,-13.7872703577417));
#47419=CARTESIAN_POINT('Ctrl Pts',(16.3094902338593,18.384875816755,-13.7914539715626));
#47420=CARTESIAN_POINT('Ctrl Pts',(16.2849076425234,18.4656499986249,-13.7956375853835));
#47421=CARTESIAN_POINT('Ctrl Pts',(16.260736137924,18.5450734199358,-13.7997512379815));
#47422=CARTESIAN_POINT('Ctrl Pts',(16.2404348481342,18.625665568199,-13.8038648905794));
#47423=CARTESIAN_POINT('Ctrl Pts',(16.2241009663663,18.7070090864265,-13.8079785431774));
#47424=CARTESIAN_POINT('Ctrl Pts',(16.2073503971231,18.7904277283583,-13.8121971376098));
#47425=CARTESIAN_POINT('Ctrl Pts',(16.1947725425285,18.8746360871018,-13.8164157320421));
#47426=CARTESIAN_POINT('Ctrl Pts',(16.1864159534739,18.9591756050623,-13.8206343264745));
#47427=CARTESIAN_POINT('Ctrl Pts',(16.1780593644194,19.0437151230227,-13.8248529209068));
#47428=CARTESIAN_POINT('Ctrl Pts',(16.1739240322153,19.1285852645551,-13.8290715153392));
#47429=CARTESIAN_POINT('Ctrl Pts',(16.1740010575059,19.2133268925441,-13.8332901097715));
#47430=CARTESIAN_POINT('Ctrl Pts',(16.1735504167883,19.2133273021507,-13.8332901097715));
#47431=CARTESIAN_POINT('Ctrl Pts',(16.1718448984259,19.397218647613,-13.8424428639771));
#47432=CARTESIAN_POINT('Ctrl Pts',(16.2739023704358,20.430943821993,-13.8939875537431));
#47433=CARTESIAN_POINT('Ctrl Pts',(17.6781137250704,22.0479692933859,-13.9879241790696));
#47434=CARTESIAN_POINT('Ctrl Pts',(19.6033699085088,21.7705394915115,-14.073242403535));
#47435=CARTESIAN_POINT('Ctrl Pts',(20.2876322249798,21.2509972054334,-14.1161686924399));
#47436=CARTESIAN_POINT('Ctrl Pts',(20.2961055941918,21.2444717899281,-14.1167030457843));
#47437=CARTESIAN_POINT('',(16.1740010826188,19.2086456408846,-13.7667098774927));
#47438=CARTESIAN_POINT('Ctrl Pts',(16.1744182524956,19.2086462806443,-13.7667098902285));
#47439=CARTESIAN_POINT('Ctrl Pts',(16.1802301046829,19.8484613837252,-13.7985275695778));
#47440=CARTESIAN_POINT('Ctrl Pts',(16.7471749375075,21.3499116609599,-13.8727371844876));
#47441=CARTESIAN_POINT('Ctrl Pts',(18.7905373386876,22.0308988273534,-13.967209816535));
#47442=CARTESIAN_POINT('Ctrl Pts',(19.9669551389709,21.4873580195988,-14.0298647692332));
#47443=CARTESIAN_POINT('Ctrl Pts',(20.2909850521016,21.2378231040073,-14.0501277863708));
#47444=CARTESIAN_POINT('Ctrl Pts',(20.2935358855687,21.2411349269503,-13.2501880127039));
#47445=CARTESIAN_POINT('Ctrl Pts',(20.3621095148682,21.1884571298854,-13.2544909997392));
#47446=CARTESIAN_POINT('Ctrl Pts',(20.428092506028,21.1322385438866,-13.2587939867745));
#47447=CARTESIAN_POINT('Ctrl Pts',(20.4911037546367,21.0727696945223,-13.2630969738097));
#47448=CARTESIAN_POINT('Ctrl Pts',(20.5521864281439,21.0151209986183,-13.2672682600163));
#47449=CARTESIAN_POINT('Ctrl Pts',(20.6104762812547,20.9544184654227,-13.2714395462229));
#47450=CARTESIAN_POINT('Ctrl Pts',(20.6656594856219,20.8909677471924,-13.2756108324295));
#47451=CARTESIAN_POINT('Ctrl Pts',(20.7208228005176,20.8275398982622,-13.2797806151954));
#47452=CARTESIAN_POINT('Ctrl Pts',(20.7728813887447,20.7613661781835,-13.2839503979612));
#47453=CARTESIAN_POINT('Ctrl Pts',(20.8215597165041,20.6927875792533,-13.2881201807271));
#47454=CARTESIAN_POINT('Ctrl Pts',(20.8702351016398,20.6242131259259,-13.2922897114279));
#47455=CARTESIAN_POINT('Ctrl Pts',(20.9155303667627,20.5532344582363,-13.2964592421288));
#47456=CARTESIAN_POINT('Ctrl Pts',(20.9572123825738,20.4802228732459,-13.3006287728297));
#47457=CARTESIAN_POINT('Ctrl Pts',(20.9989043820684,20.4071938005081,-13.3047993022172));
#47458=CARTESIAN_POINT('Ctrl Pts',(21.0369811868537,20.3321312436427,-13.3089698316048));
#47459=CARTESIAN_POINT('Ctrl Pts',(21.0712555039942,20.2554312849818,-13.3131403609924));
#47460=CARTESIAN_POINT('Ctrl Pts',(21.1055689017353,20.178643870736,-13.3173156457422));
#47461=CARTESIAN_POINT('Ctrl Pts',(21.13607097399,20.1002157503588,-13.321490930492));
#47462=CARTESIAN_POINT('Ctrl Pts',(21.1626227258789,20.0205626321321,-13.3256662152417));
#47463=CARTESIAN_POINT('Ctrl Pts',(21.1891927332993,19.9408547487803,-13.3298443706889));
#47464=CARTESIAN_POINT('Ctrl Pts',(21.2118068922775,19.8599206339596,-13.334022526136));
#47465=CARTESIAN_POINT('Ctrl Pts',(21.2303768166874,19.7781884952162,-13.3382006815831));
#47466=CARTESIAN_POINT('Ctrl Pts',(21.2489760425118,19.696327391636,-13.342385429726));
#47467=CARTESIAN_POINT('Ctrl Pts',(21.2635182246709,19.6136662038172,-13.346570177869));
#47468=CARTESIAN_POINT('Ctrl Pts',(21.2739665897943,19.5306399892512,-13.350754926012));
#47469=CARTESIAN_POINT('Ctrl Pts',(21.2762176597463,19.5127522322071,-13.3516565178582));
#47470=CARTESIAN_POINT('Ctrl Pts',(21.2782788975167,19.4948475346138,-13.3525581097044));
#47471=CARTESIAN_POINT('Ctrl Pts',(21.2801502518719,19.4769302444118,-13.3534597015506));
#47472=CARTESIAN_POINT('Ctrl Pts',(21.2888359269133,19.3937692119263,-13.3576443359436));
#47473=CARTESIAN_POINT('Ctrl Pts',(21.2934592377886,19.3100274422731,-13.3618289703367));
#47474=CARTESIAN_POINT('Ctrl Pts',(21.2939552539536,19.2261359755289,-13.3660136047297));
#47475=CARTESIAN_POINT('Ctrl Pts',(21.294450564101,19.1423639179039,-13.3701922828137));
#47476=CARTESIAN_POINT('Ctrl Pts',(21.2908302458307,19.0584430425126,-13.3743709608976));
#47477=CARTESIAN_POINT('Ctrl Pts',(21.2830810689264,18.9748100255276,-13.3785496389816));
#47478=CARTESIAN_POINT('Ctrl Pts',(21.2751929935952,18.8896779468192,-13.382803216867));
#47479=CARTESIAN_POINT('Ctrl Pts',(21.2630265340501,18.804844627276,-13.3870567947524));
#47480=CARTESIAN_POINT('Ctrl Pts',(21.2466232879999,18.7207712650195,-13.3913103726379));
#47481=CARTESIAN_POINT('Ctrl Pts',(21.2305380508827,18.6383278289459,-13.3954814866158));
#47482=CARTESIAN_POINT('Ctrl Pts',(21.2103789301822,18.5566156189164,-13.3996526005938));
#47483=CARTESIAN_POINT('Ctrl Pts',(21.1862373001536,18.4760631158151,-13.4038237145717));
#47484=CARTESIAN_POINT('Ctrl Pts',(21.1621037710821,18.3955376428842,-13.4079934288921));
#47485=CARTESIAN_POINT('Ctrl Pts',(21.1339905186921,18.3161715443229,-13.4121631432125));
#47486=CARTESIAN_POINT('Ctrl Pts',(21.1020392245073,18.2383797086247,-13.4163328575329));
#47487=CARTESIAN_POINT('Ctrl Pts',(21.0700890672866,18.1605906410939,-13.4205024234769));
#47488=CARTESIAN_POINT('Ctrl Pts',(21.0343013153839,18.0843761502596,-13.4246719894209));
#47489=CARTESIAN_POINT('Ctrl Pts',(20.9948658827287,18.0101313725834,-13.428841555365));
#47490=CARTESIAN_POINT('Ctrl Pts',(20.9540439489102,17.933276240115,-13.4331577181039));
#47491=CARTESIAN_POINT('Ctrl Pts',(20.9093133043206,17.8585323739429,-13.4374738808428));
#47492=CARTESIAN_POINT('Ctrl Pts',(20.8609355752997,17.7863087848504,-13.4417900435817));
#47493=CARTESIAN_POINT('Ctrl Pts',(20.8141337457132,17.7164378715759,-13.4459656077734));
#47494=CARTESIAN_POINT('Ctrl Pts',(20.7639191093595,17.6489259106341,-13.4501411719651));
#47495=CARTESIAN_POINT('Ctrl Pts',(20.7105706701801,17.5841108255988,-13.4543167361568));
#47496=CARTESIAN_POINT('Ctrl Pts',(20.6545277281616,17.5160220847016,-13.4587031981693));
#47497=CARTESIAN_POINT('Ctrl Pts',(20.5950264806455,17.450910248947,-13.4630896601819));
#47498=CARTESIAN_POINT('Ctrl Pts',(20.5324338669329,17.3891230485379,-13.4674761221944));
#47499=CARTESIAN_POINT('Ctrl Pts',(20.4698412532203,17.3273358481288,-13.4718625842069));
#47500=CARTESIAN_POINT('Ctrl Pts',(20.4041577572906,17.2688736120053,-13.4762490462195));
#47501=CARTESIAN_POINT('Ctrl Pts',(20.3357880909559,17.2140335727229,-13.480635508232));
#47502=CARTESIAN_POINT('Ctrl Pts',(20.2705642143173,17.1617168049402,-13.4848201426251));
#47503=CARTESIAN_POINT('Ctrl Pts',(20.2026531489501,17.1125015005239,-13.4890047770181));
#47504=CARTESIAN_POINT('Ctrl Pts',(20.1323821856731,17.0666755696043,-13.4931894114112));
#47505=CARTESIAN_POINT('Ctrl Pts',(20.0622112444146,17.0209148662252,-13.4973680894951));
#47506=CARTESIAN_POINT('Ctrl Pts',(19.9896874593622,16.9785342027988,-13.5015467675791));
#47507=CARTESIAN_POINT('Ctrl Pts',(19.9151708448062,16.9397810683732,-13.505725445663));
#47508=CARTESIAN_POINT('Ctrl Pts',(19.8393185734883,16.9003333118644,-13.5099790235484));
#47509=CARTESIAN_POINT('Ctrl Pts',(19.7614017031198,16.8646447120803,-13.5142326014339));
#47510=CARTESIAN_POINT('Ctrl Pts',(19.6818305443853,16.8329299297266,-13.5184861793193));
#47511=CARTESIAN_POINT('Ctrl Pts',(19.6038020278331,16.801830000315,-13.5226572932973));
#47512=CARTESIAN_POINT('Ctrl Pts',(19.5241832407486,16.7745513610798,-13.5268284072752));
#47513=CARTESIAN_POINT('Ctrl Pts',(19.4433839268982,16.7512491093083,-13.5309995212532));
#47514=CARTESIAN_POINT('Ctrl Pts',(19.3626117260379,16.7279546768325,-13.5351692355735));
#47515=CARTESIAN_POINT('Ctrl Pts',(19.2806602267965,16.7086341092198,-13.5393389498939));
#47516=CARTESIAN_POINT('Ctrl Pts',(19.1979549742612,16.6933928460027,-13.5435086642143));
#47517=CARTESIAN_POINT('Ctrl Pts',(19.1152526647337,16.6781521251352,-13.5476782301583));
#47518=CARTESIAN_POINT('Ctrl Pts',(19.0317971078103,16.6669905025844,-13.5518477961024));
#47519=CARTESIAN_POINT('Ctrl Pts',(18.9480233475313,16.6599621706624,-13.5560173620464));
#47520=CARTESIAN_POINT('Ctrl Pts',(18.861304205187,16.6526867312604,-13.5603335247853));
#47521=CARTESIAN_POINT('Ctrl Pts',(18.7742445926769,16.6498406874529,-13.5646496875243));
#47522=CARTESIAN_POINT('Ctrl Pts',(18.687330036718,16.6514254426707,-13.5689658502632));
#47523=CARTESIAN_POINT('Ctrl Pts',(18.6032467132777,16.6529585746541,-13.5731414144549));
#47524=CARTESIAN_POINT('Ctrl Pts',(18.5192996078628,16.6586381931969,-13.5773169786466));
#47525=CARTESIAN_POINT('Ctrl Pts',(18.435923880263,16.6684126117589,-13.5814925428382));
#47526=CARTESIAN_POINT('Ctrl Pts',(18.3483370428692,16.678680712966,-13.5858790048508));
#47527=CARTESIAN_POINT('Ctrl Pts',(18.2613813964209,16.6934680441002,-13.5902654668633));
#47528=CARTESIAN_POINT('Ctrl Pts',(18.1755479442734,16.7126542870422,-13.5946519288759));
#47529=CARTESIAN_POINT('Ctrl Pts',(18.089714492126,16.7318405299841,-13.5990383908884));
#47530=CARTESIAN_POINT('Ctrl Pts',(18.0050037728349,16.7554254558327,-13.6034248529009));
#47531=CARTESIAN_POINT('Ctrl Pts',(17.921884774769,16.783229652346,-13.6078113149135));
#47532=CARTESIAN_POINT('Ctrl Pts',(17.842590205016,16.809754536562,-13.6119959493065));
#47533=CARTESIAN_POINT('Ctrl Pts',(17.7644489508447,16.8402176845382,-13.6161805836996));
#47534=CARTESIAN_POINT('Ctrl Pts',(17.6878802554244,16.8744997367839,-13.6203652180926));
#47535=CARTESIAN_POINT('Ctrl Pts',(17.6114205460648,16.9087329927714,-13.6245438961766));
#47536=CARTESIAN_POINT('Ctrl Pts',(17.536529365682,16.9467741695629,-13.6287225742605));
#47537=CARTESIAN_POINT('Ctrl Pts',(17.4636096823067,16.9884545132414,-13.6329012523445));
#47538=CARTESIAN_POINT('Ctrl Pts',(17.3893829660134,17.0308819471251,-13.6371548302299));
#47539=CARTESIAN_POINT('Ctrl Pts',(17.3171995773182,17.0770801423177,-13.6414084081153));
#47540=CARTESIAN_POINT('Ctrl Pts',(17.2474621052952,17.1268202842349,-13.6456619860008));
#47541=CARTESIAN_POINT('Ctrl Pts',(17.1790766302489,17.1755961164411,-13.6498330999787));
#47542=CARTESIAN_POINT('Ctrl Pts',(17.1130434722312,17.2277775063952,-13.6540042139567));
#47543=CARTESIAN_POINT('Ctrl Pts',(17.0497148300457,17.283103875653,-13.6581753279346));
#47544=CARTESIAN_POINT('Ctrl Pts',(16.9864074383977,17.3384116796134,-13.662345042255));
#47545=CARTESIAN_POINT('Ctrl Pts',(16.9258031063753,17.3968620645642,-13.6665147565754));
#47546=CARTESIAN_POINT('Ctrl Pts',(16.8682208314237,17.4581542868504,-13.6706844708957));
#47547=CARTESIAN_POINT('Ctrl Pts',(16.8106406054967,17.5194443280963,-13.6748540368398));
#47548=CARTESIAN_POINT('Ctrl Pts',(16.7560825371937,17.5835756697509,-13.6790236027838));
#47549=CARTESIAN_POINT('Ctrl Pts',(16.7048276747609,17.650211841894,-13.6831931687278));
#47550=CARTESIAN_POINT('Ctrl Pts',(16.6517707545947,17.7191908596451,-13.6875093314668));
#47551=CARTESIAN_POINT('Ctrl Pts',(16.6022539651133,17.7908537067501,-13.6918254942057));
#47552=CARTESIAN_POINT('Ctrl Pts',(16.5565412927829,17.8647928917271,-13.6961416569446));
#47553=CARTESIAN_POINT('Ctrl Pts',(16.5123177059456,17.9363235155304,-13.7003172211363));
#47554=CARTESIAN_POINT('Ctrl Pts',(16.4716543903427,18.0099840160617,-13.704492785328));
#47555=CARTESIAN_POINT('Ctrl Pts',(16.4347434295141,18.0853805158593,-13.7086683495197));
#47556=CARTESIAN_POINT('Ctrl Pts',(16.3959681838015,18.1645851136235,-13.7130548115322));
#47557=CARTESIAN_POINT('Ctrl Pts',(16.3613345469612,18.2457051531361,-13.7174412735447));
#47558=CARTESIAN_POINT('Ctrl Pts',(16.3310071212994,18.3282626523624,-13.7218277355573));
#47559=CARTESIAN_POINT('Ctrl Pts',(16.3006796956376,18.4108201515888,-13.7262141975698));
#47560=CARTESIAN_POINT('Ctrl Pts',(16.2746585801944,18.494814533789,-13.7306006595824));
#47561=CARTESIAN_POINT('Ctrl Pts',(16.253046772176,18.5797543415202,-13.7349871215949));
#47562=CARTESIAN_POINT('Ctrl Pts',(16.2263033450825,18.6848626949471,-13.7404151277539));
#47563=CARTESIAN_POINT('Ctrl Pts',(16.2062281520531,18.7917315462651,-13.7458431339129));
#47564=CARTESIAN_POINT('Ctrl Pts',(16.1930065418683,18.8996284442475,-13.7512711400719));
#47565=CARTESIAN_POINT('Ctrl Pts',(16.180471247327,19.0019245622985,-13.7564173858788));
#47566=CARTESIAN_POINT('Ctrl Pts',(16.1740962693074,19.1051449394228,-13.7615636316857));
#47567=CARTESIAN_POINT('Ctrl Pts',(16.1740010826188,19.2086456408846,-13.7667098774927));
#47568=CARTESIAN_POINT('Origin',(18.734,19.211,1.76670989022852));
#47569=CARTESIAN_POINT('',(20.2954167287344,21.2436206075649,-12.4500366863435));
#47570=CARTESIAN_POINT('',(20.2935358855687,21.2411349269503,-12.5167193513141));
#47571=CARTESIAN_POINT('',(20.2935358855687,21.2411349269503,1.76670989022852));
#47572=CARTESIAN_POINT('',(16.174000001606,19.2109093211998,-13.0332901097364));
#47573=CARTESIAN_POINT('Ctrl Pts',(20.2935358855687,21.2411349269503,-12.5167193513141));
#47574=CARTESIAN_POINT('Ctrl Pts',(20.3602126462826,21.1899142914712,-12.5208888671653));
#47575=CARTESIAN_POINT('Ctrl Pts',(20.4243799329773,21.1353926325048,-12.5250583830165));
#47576=CARTESIAN_POINT('Ctrl Pts',(20.4857025030192,21.0778525225407,-12.5292278988677));
#47577=CARTESIAN_POINT('Ctrl Pts',(20.5470295679466,21.0203081949416,-12.5333977203404));
#47578=CARTESIAN_POINT('Ctrl Pts',(20.6055111676078,20.959745292768,-12.5375675418131));
#47579=CARTESIAN_POINT('Ctrl Pts',(20.6608480428545,20.8964840906243,-12.5417373632858));
#47580=CARTESIAN_POINT('Ctrl Pts',(20.7162427463173,20.8331567791739,-12.5459115423109));
#47581=CARTESIAN_POINT('Ctrl Pts',(20.7684858595219,20.7671258839871,-12.5500857213361));
#47582=CARTESIAN_POINT('Ctrl Pts',(20.8173179955917,20.6987453173322,-12.5542599003612));
#47583=CARTESIAN_POINT('Ctrl Pts',(20.8661764272834,20.630327928419,-12.5584363271405));
#47584=CARTESIAN_POINT('Ctrl Pts',(20.9116199755333,20.5595587357766,-12.5626127539197));
#47585=CARTESIAN_POINT('Ctrl Pts',(20.9534335841905,20.4868191742436,-12.5667891806989));
#47586=CARTESIAN_POINT('Ctrl Pts',(20.9953200408688,20.4139528852338,-12.5709728836841));
#47587=CARTESIAN_POINT('Ctrl Pts',(21.0335637164752,20.3391097806619,-12.5751565866692));
#47588=CARTESIAN_POINT('Ctrl Pts',(21.067996451488,20.2626941401574,-12.5793402896544));
#47589=CARTESIAN_POINT('Ctrl Pts',(21.094470322618,20.2039413916964,-12.5825569616276));
#47590=CARTESIAN_POINT('Ctrl Pts',(21.1186923490915,20.1442595308903,-12.5857736336007));
#47591=CARTESIAN_POINT('Ctrl Pts',(21.1406062076889,20.0838382216157,-12.5889903055739));
#47592=CARTESIAN_POINT('Ctrl Pts',(21.1691143947643,20.0052349039716,-12.5931749399669));
#47593=CARTESIAN_POINT('Ctrl Pts',(21.193820633909,19.9250871608006,-12.59735957436));
#47594=CARTESIAN_POINT('Ctrl Pts',(21.2145578396958,19.8437976010731,-12.601544208753));
#47595=CARTESIAN_POINT('Ctrl Pts',(21.2352655286368,19.7626237469725,-12.605722886837));
#47596=CARTESIAN_POINT('Ctrl Pts',(21.2520152930198,19.6803117464873,-12.6099015649209));
#47597=CARTESIAN_POINT('Ctrl Pts',(21.2646888572062,19.5972821611367,-12.6140802430048));
#47598=CARTESIAN_POINT('Ctrl Pts',(21.2775895859223,19.5127643301408,-12.6183338208903));
#47599=CARTESIAN_POINT('Ctrl Pts',(21.2862663809328,19.4275033890779,-12.6225873987757));
#47600=CARTESIAN_POINT('Ctrl Pts',(21.290648251397,19.3419569342516,-12.6268409766611));
#47601=CARTESIAN_POINT('Ctrl Pts',(21.2949451707517,19.2580689643825,-12.6310120906391));
#47602=CARTESIAN_POINT('Ctrl Pts',(21.2951121858363,19.1739069330306,-12.635183204617));
#47603=CARTESIAN_POINT('Ctrl Pts',(21.2911345092732,19.089908705993,-12.639354318595));
#47604=CARTESIAN_POINT('Ctrl Pts',(21.2871581674578,19.0059386653716,-12.6435240329154));
#47605=CARTESIAN_POINT('Ctrl Pts',(21.2790399178705,18.9221327790365,-12.6476937472357));
#47606=CARTESIAN_POINT('Ctrl Pts',(21.2668170738606,18.8389278694117,-12.6518634615561));
#47607=CARTESIAN_POINT('Ctrl Pts',(21.2545946647918,18.7557259205746,-12.6560330275001));
#47608=CARTESIAN_POINT('Ctrl Pts',(21.2382680194081,18.6731253609524,-12.6602025934442));
#47609=CARTESIAN_POINT('Ctrl Pts',(21.2179260255781,18.5915554912215,-12.6643721593882));
#47610=CARTESIAN_POINT('Ctrl Pts',(21.1968688323395,18.5071177254981,-12.6686883221272));
#47611=CARTESIAN_POINT('Ctrl Pts',(21.1715088054104,18.4237849880539,-12.6730044848661));
#47612=CARTESIAN_POINT('Ctrl Pts',(21.142001073276,18.342017358573,-12.677320647605));
#47613=CARTESIAN_POINT('Ctrl Pts',(21.1134545524123,18.2629133010222,-12.6814962117967));
#47614=CARTESIAN_POINT('Ctrl Pts',(21.0810266246881,18.1852743669889,-12.6856717759884));
#47615=CARTESIAN_POINT('Ctrl Pts',(21.0449064462661,18.1094958481215,-12.68984734018));
#47616=CARTESIAN_POINT('Ctrl Pts',(21.0069619234994,18.0298899364119,-12.6942338021926));
#47617=CARTESIAN_POINT('Ctrl Pts',(20.964942634636,17.9523378315096,-12.6986202642051));
#47618=CARTESIAN_POINT('Ctrl Pts',(20.9191207015649,17.8772655738144,-12.7030067262177));
#47619=CARTESIAN_POINT('Ctrl Pts',(20.8732987684938,17.8021933161193,-12.7073931882302));
#47620=CARTESIAN_POINT('Ctrl Pts',(20.8236745814509,17.7296013416973,-12.7117796502428));
#47621=CARTESIAN_POINT('Ctrl Pts',(20.7705691100603,17.6598758076968,-12.7161661122553));
#47622=CARTESIAN_POINT('Ctrl Pts',(20.7199071001298,17.593358448874,-12.7203507466484));
#47623=CARTESIAN_POINT('Ctrl Pts',(20.6658885504365,17.5292019583443,-12.7245353810414));
#47624=CARTESIAN_POINT('Ctrl Pts',(20.6087615512377,17.4677647531096,-12.7287200154345));
#47625=CARTESIAN_POINT('Ctrl Pts',(20.5517158652512,17.4064149961321,-12.7328986935184));
#47626=CARTESIAN_POINT('Ctrl Pts',(20.4915708287755,17.3477771703014,-12.7370773716023));
#47627=CARTESIAN_POINT('Ctrl Pts',(20.4286160471331,17.2921783686859,-12.7412560496863));
#47628=CARTESIAN_POINT('Ctrl Pts',(20.3645328462747,17.2355829985097,-12.7455096275717));
#47629=CARTESIAN_POINT('Ctrl Pts',(20.2975384722481,17.1821370567428,-12.7497632054572));
#47630=CARTESIAN_POINT('Ctrl Pts',(20.2279792651328,17.1321479236479,-12.7540167833426));
#47631=CARTESIAN_POINT('Ctrl Pts',(20.159768598981,17.0831279274438,-12.7581878973205));
#47632=CARTESIAN_POINT('Ctrl Pts',(20.0890920516418,17.0374321828769,-12.7623590112985));
#47633=CARTESIAN_POINT('Ctrl Pts',(20.0163097948298,16.9953101322424,-12.7665301252764));
#47634=CARTESIAN_POINT('Ctrl Pts',(19.9435519608069,16.9532022160688,-12.7706998395968));
#47635=CARTESIAN_POINT('Ctrl Pts',(19.8686902184412,16.9146658424621,-12.7748695539172));
#47636=CARTESIAN_POINT('Ctrl Pts',(19.7921120632711,16.8799060804935,-12.7790392682375));
#47637=CARTESIAN_POINT('Ctrl Pts',(19.7155366330805,16.8451475554265,-12.7832088341816));
#47638=CARTESIAN_POINT('Ctrl Pts',(19.6372453307736,16.8141655641666,-12.7873784001256));
#47639=CARTESIAN_POINT('Ctrl Pts',(19.557647243598,16.7871177383971,-12.7915479660697));
#47640=CARTESIAN_POINT('Ctrl Pts',(19.4752505858722,16.7591189444405,-12.7958641288086));
#47641=CARTESIAN_POINT('Ctrl Pts',(19.3914540397877,16.7353362835285,-12.8001802915475));
#47642=CARTESIAN_POINT('Ctrl Pts',(19.3067284276563,16.7158883495614,-12.8044964542864));
#47643=CARTESIAN_POINT('Ctrl Pts',(19.2247627434286,16.6970739299978,-12.8086720184781));
#47644=CARTESIAN_POINT('Ctrl Pts',(19.1419280643013,16.6823162029296,-12.8128475826698));
#47645=CARTESIAN_POINT('Ctrl Pts',(19.0586591546378,16.6716700818307,-12.8170231468614));
#47646=CARTESIAN_POINT('Ctrl Pts',(18.9711845303002,16.6604862504638,-12.821409608874));
#47647=CARTESIAN_POINT('Ctrl Pts',(18.8832312388615,16.6538403392096,-12.8257960708865));
#47648=CARTESIAN_POINT('Ctrl Pts',(18.7953048072929,16.6517341442119,-12.830182532899));
#47649=CARTESIAN_POINT('Ctrl Pts',(18.7073783757243,16.6496279492142,-12.8345689949116));
#47650=CARTESIAN_POINT('Ctrl Pts',(18.6194793819155,16.6520613783803,-12.8389554569241));
#47651=CARTESIAN_POINT('Ctrl Pts',(18.5321062576876,16.6589735665916,-12.8433419189367));
#47652=CARTESIAN_POINT('Ctrl Pts',(18.4487533004234,16.665567714777,-12.8475265533297));
#47653=CARTESIAN_POINT('Ctrl Pts',(18.3655686284663,16.6762620749485,-12.8517111877228));
#47654=CARTESIAN_POINT('Ctrl Pts',(18.2829879003453,16.6910420467863,-12.8558958221158));
#47655=CARTESIAN_POINT('Ctrl Pts',(18.2005247156695,16.7058009811635,-12.8600745001997));
#47656=CARTESIAN_POINT('Ctrl Pts',(18.1186642162797,16.7246338957133,-12.8642531782837));
#47657=CARTESIAN_POINT('Ctrl Pts',(18.0378381935513,16.7474743274644,-12.8684318563676));
#47658=CARTESIAN_POINT('Ctrl Pts',(17.9555634224539,16.7707241575396,-12.872685434253));
#47659=CARTESIAN_POINT('Ctrl Pts',(17.8743610594197,16.7981265494104,-12.8769390121385));
#47660=CARTESIAN_POINT('Ctrl Pts',(17.7946770299218,16.8295566649858,-12.8811925900239));
#47661=CARTESIAN_POINT('Ctrl Pts',(17.7165378308264,16.8603774464399,-12.8853637040019));
#47662=CARTESIAN_POINT('Ctrl Pts',(17.639859066566,16.8950709981002,-12.8895348179798));
#47663=CARTESIAN_POINT('Ctrl Pts',(17.5650454327538,16.9334694909367,-12.8937059319578));
#47664=CARTESIAN_POINT('Ctrl Pts',(17.4902569033788,16.9718550987881,-12.8978756462781));
#47665=CARTESIAN_POINT('Ctrl Pts',(17.4173326704116,17.0139429688568,-12.9020453605985));
#47666=CARTESIAN_POINT('Ctrl Pts',(17.3466549084735,17.0595182787164,-12.9062150749189));
#47667=CARTESIAN_POINT('Ctrl Pts',(17.2759796615535,17.105091966811,-12.9103846408629));
#47668=CARTESIAN_POINT('Ctrl Pts',(17.2075511128834,17.154152597935,-12.914554206807));
#47669=CARTESIAN_POINT('Ctrl Pts',(17.1417232369313,17.2064415174929,-12.918723772751));
#47670=CARTESIAN_POINT('Ctrl Pts',(17.0735809340681,17.260568850957,-12.92303993549));
#47671=CARTESIAN_POINT('Ctrl Pts',(17.0082259988603,17.3181553818453,-12.9273560982289));
#47672=CARTESIAN_POINT('Ctrl Pts',(16.9460129971978,17.3788694157319,-12.9316722609678));
#47673=CARTESIAN_POINT('Ctrl Pts',(16.8858265775208,17.4376056963507,-12.9358478251595));
#47674=CARTESIAN_POINT('Ctrl Pts',(16.8285808237897,17.499268474865,-12.9400233893512));
#47675=CARTESIAN_POINT('Ctrl Pts',(16.7745572392495,17.5635219068702,-12.9441989535429));
#47676=CARTESIAN_POINT('Ctrl Pts',(16.7178050518831,17.631020626978,-12.9485854155554));
#47677=CARTESIAN_POINT('Ctrl Pts',(16.6646094437668,17.7013781204557,-12.9529718775679));
#47678=CARTESIAN_POINT('Ctrl Pts',(16.6152455573348,17.7741702913405,-12.9573583395805));
#47679=CARTESIAN_POINT('Ctrl Pts',(16.5658816709029,17.8469624622252,-12.961744801593));
#47680=CARTESIAN_POINT('Ctrl Pts',(16.5203497415206,17.9221887747551,-12.9661312636056));
#47681=CARTESIAN_POINT('Ctrl Pts',(16.4788683829465,17.9993971815129,-12.9705177256181));
#47682=CARTESIAN_POINT('Ctrl Pts',(16.4371381237559,18.0770688619124,-12.9749305077209));
#47683=CARTESIAN_POINT('Ctrl Pts',(16.3993648293881,18.1570094498413,-12.9793432898236));
#47684=CARTESIAN_POINT('Ctrl Pts',(16.3657873879884,18.2388019624021,-12.9837560719264));
#47685=CARTESIAN_POINT('Ctrl Pts',(16.3323070847556,18.3203578525641,-12.9881560880307));
#47686=CARTESIAN_POINT('Ctrl Pts',(16.3029985969533,18.4037546379833,-12.992556104135));
#47687=CARTESIAN_POINT('Ctrl Pts',(16.2780542372553,18.4885524860197,-12.9969561202393));
#47688=CARTESIAN_POINT('Ctrl Pts',(16.2531532512187,18.5732028861683,-13.0013484855236));
#47689=CARTESIAN_POINT('Ctrl Pts',(16.2326014031163,18.6592491335653,-13.0057408508078));
#47690=CARTESIAN_POINT('Ctrl Pts',(16.2165427462274,18.7462323425329,-13.010133216092));
#47691=CARTESIAN_POINT('Ctrl Pts',(16.2005210016679,18.833015612434,-13.0145154851125));
#47692=CARTESIAN_POINT('Ctrl Pts',(16.1889719431304,18.9207311752712,-13.018897754133));
#47693=CARTESIAN_POINT('Ctrl Pts',(16.1819893075699,19.0089073833058,-13.0232800231536));
#47694=CARTESIAN_POINT('Ctrl Pts',(16.176672671659,19.0760454703589,-13.0266167186812));
#47695=CARTESIAN_POINT('Ctrl Pts',(16.1740023911013,19.1434502453368,-13.0299534142088));
#47696=CARTESIAN_POINT('Ctrl Pts',(16.174000001606,19.2109093211998,-13.0332901097364));
#47697=CARTESIAN_POINT('Ctrl Pts',(16.174000001606,19.2109093219104,-13.0332901097715));
#47698=CARTESIAN_POINT('Ctrl Pts',(16.1739968821085,19.2989781543512,-13.0376462156856));
#47699=CARTESIAN_POINT('Ctrl Pts',(16.1785426714359,19.3869643923453,-13.0420023215996));
#47700=CARTESIAN_POINT('Ctrl Pts',(16.1875860737585,19.4743934627951,-13.0463584275137));
#47701=CARTESIAN_POINT('Ctrl Pts',(16.1966529338893,19.5620493167382,-13.0507258327921));
#47702=CARTESIAN_POINT('Ctrl Pts',(16.2102406836426,19.6491447181138,-13.0550932380704));
#47703=CARTESIAN_POINT('Ctrl Pts',(16.2282463851319,19.7352125728895,-13.0594606433488));
#47704=CARTESIAN_POINT('Ctrl Pts',(16.2462755658189,19.8213926590147,-13.0638337436661));
#47705=CARTESIAN_POINT('Ctrl Pts',(16.2687340840994,19.9065421429603,-13.0682068439834));
#47706=CARTESIAN_POINT('Ctrl Pts',(16.2954690366782,19.9902090482795,-13.0725799443008));
#47707=CARTESIAN_POINT('Ctrl Pts',(16.3222767415773,20.0741036316347,-13.0769649448896));
#47708=CARTESIAN_POINT('Ctrl Pts',(16.3533840099471,20.1565071961889,-13.0813499454785));
#47709=CARTESIAN_POINT('Ctrl Pts',(16.3885892814888,20.2369866283206,-13.0857349460673));
#47710=CARTESIAN_POINT('Ctrl Pts',(16.4205927188907,20.310146651112,-13.0897211414781));
#47711=CARTESIAN_POINT('Ctrl Pts',(16.4559819492917,20.3817167133684,-13.0937073368888));
#47712=CARTESIAN_POINT('Ctrl Pts',(16.4945737975983,20.4513911818441,-13.0976935322996));
#47713=CARTESIAN_POINT('Ctrl Pts',(16.5350868078939,20.524534153289,-13.1018781666926));
#47714=CARTESIAN_POINT('Ctrl Pts',(16.5792624158945,20.5958263313022,-13.1060628010857));
#47715=CARTESIAN_POINT('Ctrl Pts',(16.6269069559,20.6648771968449,-13.1102474354787));
#47716=CARTESIAN_POINT('Ctrl Pts',(16.6744836798,20.7338297770272,-13.1144261135626));
#47717=CARTESIAN_POINT('Ctrl Pts',(16.7255192690591,20.8005470061347,-13.1186047916466));
#47718=CARTESIAN_POINT('Ctrl Pts',(16.7797744504213,20.8646633579341,-13.1227834697305));
#47719=CARTESIAN_POINT('Ctrl Pts',(16.8350021169169,20.9299289492599,-13.127037047616));
#47720=CARTESIAN_POINT('Ctrl Pts',(16.8935656995718,20.9924990829437,-13.1312906255014));
#47721=CARTESIAN_POINT('Ctrl Pts',(16.9551669364597,21.0520195360332,-13.1355442033868));
#47722=CARTESIAN_POINT('Ctrl Pts',(17.0155739131657,21.110386068995,-13.1397153173648));
#47723=CARTESIAN_POINT('Ctrl Pts',(17.0789014673909,21.1658197797781,-13.1438864313427));
#47724=CARTESIAN_POINT('Ctrl Pts',(17.1448292745178,21.2180217749866,-13.1480575453207));
#47725=CARTESIAN_POINT('Ctrl Pts',(17.2107349589323,21.2702062533115,-13.1522272596411));
#47726=CARTESIAN_POINT('Ctrl Pts',(17.279238803008,21.3191608844269,-13.1563969739614));
#47727=CARTESIAN_POINT('Ctrl Pts',(17.3499870301186,21.364626731632,-13.1605666882818));
#47728=CARTESIAN_POINT('Ctrl Pts',(17.4207327397037,21.4100909609672,-13.1647362542259));
#47729=CARTESIAN_POINT('Ctrl Pts',(17.493722286064,21.4520664052353,-13.1689058201699));
#47730=CARTESIAN_POINT('Ctrl Pts',(17.5685736694553,21.490337945122,-13.1730753861139));
#47731=CARTESIAN_POINT('Ctrl Pts',(17.6460567351475,21.5299550651381,-13.1773915488529));
#47732=CARTESIAN_POINT('Ctrl Pts',(17.7255345286225,21.5656027360313,-13.1817077115918));
#47733=CARTESIAN_POINT('Ctrl Pts',(17.8065583197873,21.5970955407955,-13.1860238743307));
#47734=CARTESIAN_POINT('Ctrl Pts',(17.8849427694771,21.627562470757,-13.1901994385224));
#47735=CARTESIAN_POINT('Ctrl Pts',(17.9647735800336,21.654140963194,-13.1943750027141));
#47736=CARTESIAN_POINT('Ctrl Pts',(18.0456284938942,21.6767138255648,-13.1985505669057));
#47737=CARTESIAN_POINT('Ctrl Pts',(18.1305671972396,21.7004267895521,-13.2029370289183));
#47738=CARTESIAN_POINT('Ctrl Pts',(18.2166356079045,21.7197187126534,-13.2073234909308));
#47739=CARTESIAN_POINT('Ctrl Pts',(18.3033337697291,21.7345147311051,-13.2117099529434));
#47740=CARTESIAN_POINT('Ctrl Pts',(18.3900319315536,21.7493107495567,-13.2160964149559));
#47741=CARTESIAN_POINT('Ctrl Pts',(18.4773592594052,21.7596108709354,-13.2204828769685));
#47742=CARTESIAN_POINT('Ctrl Pts',(18.5648137584886,21.7654032601927,-13.224869338981));
#47743=CARTESIAN_POINT('Ctrl Pts',(18.6482240610122,21.7709277894662,-13.2290529559168));
#47744=CARTESIAN_POINT('Ctrl Pts',(18.7320604262274,21.7723728408952,-13.2332365728525));
#47745=CARTESIAN_POINT('Ctrl Pts',(18.8158899787628,21.7696899052793,-13.2374201897883));
#47746=CARTESIAN_POINT('Ctrl Pts',(18.8996093084477,21.7670104973074,-13.2415983059171));
#47747=CARTESIAN_POINT('Ctrl Pts',(18.9833213878538,21.7602138920977,-13.245776422046));
#47748=CARTESIAN_POINT('Ctrl Pts',(19.0665895300205,21.7493034106507,-13.2499545381748));
#47749=CARTESIAN_POINT('Ctrl Pts',(19.1497731758391,21.7384040006148,-13.2541284145603));
#47750=CARTESIAN_POINT('Ctrl Pts',(19.2325133255147,21.7233990640619,-13.2583022909457));
#47751=CARTESIAN_POINT('Ctrl Pts',(19.3143759725405,21.704343885327,-13.2624761673311));
#47752=CARTESIAN_POINT('Ctrl Pts',(19.3961801113252,21.6853023255629,-13.2666470605958));
#47753=CARTESIAN_POINT('Ctrl Pts',(19.4771075468217,21.6622163790719,-13.2708179538604));
#47754=CARTESIAN_POINT('Ctrl Pts',(19.5567334109213,21.6351925943608,-13.274988847125));
#47755=CARTESIAN_POINT('Ctrl Pts',(19.6363403165266,21.608175243869,-13.2791587473222));
#47756=CARTESIAN_POINT('Ctrl Pts',(19.7146458288504,21.5772220585841,-13.2833286475194));
#47757=CARTESIAN_POINT('Ctrl Pts',(19.7912403187455,21.542489418466,-13.2874985477165));
#47758=CARTESIAN_POINT('Ctrl Pts',(19.8678247271476,21.5077613499152,-13.2916678990645));
#47759=CARTESIAN_POINT('Ctrl Pts',(19.9426981444001,21.4692550109384,-13.2958372504126));
#47760=CARTESIAN_POINT('Ctrl Pts',(20.0154725000694,21.4271742331247,-13.3000066017606));
#47761=CARTESIAN_POINT('Ctrl Pts',(20.0882810786145,21.3850736664003,-13.3041779137882));
#47762=CARTESIAN_POINT('Ctrl Pts',(20.1589882301688,21.3393955415644,-13.3083492258158));
#47763=CARTESIAN_POINT('Ctrl Pts',(20.2272328428135,21.2903882939805,-13.3125205378434));
#47764=CARTESIAN_POINT('Ctrl Pts',(20.2496021795281,21.2743246139305,-13.3138878176868));
#47765=CARTESIAN_POINT('Ctrl Pts',(20.2717071834519,21.257903587907,-13.3152550975302));
#47766=CARTESIAN_POINT('Ctrl Pts',(20.2935358855687,21.2411349269503,-13.3166223773735));
#47767=CARTESIAN_POINT('',(16.1736697067219,19.2116425106688,-12.9667098340815));
#47768=CARTESIAN_POINT('Ctrl Pts',(16.1740000808904,19.2116435515775,-12.9667098902285));
#47769=CARTESIAN_POINT('Ctrl Pts',(16.1740088273484,19.2464363059256,-12.9684506873211));
#47770=CARTESIAN_POINT('Ctrl Pts',(16.1747268399112,19.281219269613,-12.9701914844137));
#47771=CARTESIAN_POINT('Ctrl Pts',(16.1761531171477,19.3159729673894,-12.9719322815063));
#47772=CARTESIAN_POINT('Ctrl Pts',(16.1795816894971,19.3995160291397,-12.9761169158993));
#47773=CARTESIAN_POINT('Ctrl Pts',(16.1871139062631,19.4830464110296,-12.9803015502924));
#47774=CARTESIAN_POINT('Ctrl Pts',(16.1987516982625,19.5661282142232,-12.9844861846854));
#47775=CARTESIAN_POINT('Ctrl Pts',(16.2103729253056,19.6490917607534,-12.9886648627694));
#47776=CARTESIAN_POINT('Ctrl Pts',(16.2260880567289,19.7316075451534,-12.9928435408533));
#47777=CARTESIAN_POINT('Ctrl Pts',(16.2458470513545,19.8132415662726,-12.9970222189372));
#47778=CARTESIAN_POINT('Ctrl Pts',(16.2659602117582,19.896338818551,-13.0012757968227));
#47779=CARTESIAN_POINT('Ctrl Pts',(16.2902636140325,19.9785219036749,-13.0055293747081));
#47780=CARTESIAN_POINT('Ctrl Pts',(16.3186494198466,20.0593404829151,-13.0097829525936));
#47781=CARTESIAN_POINT('Ctrl Pts',(16.3464849114246,20.1385922362921,-13.0139540665715));
#47782=CARTESIAN_POINT('Ctrl Pts',(16.3782457689157,20.2165314648406,-13.0181251805495));
#47783=CARTESIAN_POINT('Ctrl Pts',(16.4137796304916,20.2927473997743,-13.0222962945274));
#47784=CARTESIAN_POINT('Ctrl Pts',(16.4493015683371,20.3689377597149,-13.0264660088478));
#47785=CARTESIAN_POINT('Ctrl Pts',(16.4885938016079,20.4434055578922,-13.0306357231682));
#47786=CARTESIAN_POINT('Ctrl Pts',(16.5314561548597,20.5157607482732,-13.0348054374885));
#47787=CARTESIAN_POINT('Ctrl Pts',(16.574316982885,20.5881133639461,-13.0389750034326));
#47788=CARTESIAN_POINT('Ctrl Pts',(16.6207474431038,20.6583531259277,-13.0431445693766));
#47789=CARTESIAN_POINT('Ctrl Pts',(16.6705024900496,20.7261165058927,-13.0473141353206));
#47790=CARTESIAN_POINT('Ctrl Pts',(16.7220068630667,20.7962623627024,-13.0516302980596));
#47791=CARTESIAN_POINT('Ctrl Pts',(16.7770736453881,20.8637540331555,-13.0559464607985));
#47792=CARTESIAN_POINT('Ctrl Pts',(16.8353848266791,20.9282246281822,-13.0602626235374));
#47793=CARTESIAN_POINT('Ctrl Pts',(16.8917965273727,20.9905951003569,-13.0644381877291));
#47794=CARTESIAN_POINT('Ctrl Pts',(16.951244134227,21.0501379976127,-13.0686137519208));
#47795=CARTESIAN_POINT('Ctrl Pts',(17.0134027193005,21.1065592836019,-13.0727893161124));
#47796=CARTESIAN_POINT('Ctrl Pts',(17.0787007867382,21.1658302746177,-13.077175778125));
#47797=CARTESIAN_POINT('Ctrl Pts',(17.1469904406111,21.2216556522274,-13.0815622401375));
#47798=CARTESIAN_POINT('Ctrl Pts',(17.2178583236868,21.273744389726,-13.0859487021501));
#47799=CARTESIAN_POINT('Ctrl Pts',(17.2887262067624,21.3258331272246,-13.0903351641627));
#47800=CARTESIAN_POINT('Ctrl Pts',(17.3621717925896,21.3741849690991,-13.0947216261752));
#47801=CARTESIAN_POINT('Ctrl Pts',(17.4377516489582,21.4185643167123,-13.0991080881878));
#47802=CARTESIAN_POINT('Ctrl Pts',(17.5098539640988,21.4609017047557,-13.1032927225808));
#47803=CARTESIAN_POINT('Ctrl Pts',(17.5841668423744,21.4997817138926,-13.1074773569739));
#47804=CARTESIAN_POINT('Ctrl Pts',(17.660324806961,21.5349667768392,-13.1116619913669));
#47805=CARTESIAN_POINT('Ctrl Pts',(17.7363743701113,21.5701017582038,-13.1158406694508));
#47806=CARTESIAN_POINT('Ctrl Pts',(17.8142633889641,21.6015520487103,-13.1200193475348));
#47807=CARTESIAN_POINT('Ctrl Pts',(17.8935998508933,21.629124808479,-13.1241980256187));
#47808=CARTESIAN_POINT('Ctrl Pts',(17.9743583618844,21.6571917901503,-13.1284516035042));
#47809=CARTESIAN_POINT('Ctrl Pts',(18.0566163014189,21.6812406201864,-13.1327051813896));
#47810=CARTESIAN_POINT('Ctrl Pts',(18.1399366350501,21.701118213745,-13.136958759275));
#47811=CARTESIAN_POINT('Ctrl Pts',(18.2216416414276,21.7206104413645,-13.141129873253));
#47812=CARTESIAN_POINT('Ctrl Pts',(18.3043677482543,21.7360916126581,-13.1453009872309));
#47813=CARTESIAN_POINT('Ctrl Pts',(18.3876870934184,21.7474674984582,-13.1494721012089));
#47814=CARTESIAN_POINT('Ctrl Pts',(18.4709784799716,21.75883956697,-13.1536418155293));
#47815=CARTESIAN_POINT('Ctrl Pts',(18.5548622540875,21.76610902368,-13.1578115298496));
#47816=CARTESIAN_POINT('Ctrl Pts',(18.6389020976073,21.7692330599381,-13.16198124417));
#47817=CARTESIAN_POINT('Ctrl Pts',(18.7229389506288,21.7723569850297,-13.1661508101141));
#47818=CARTESIAN_POINT('Ctrl Pts',(18.8071314022652,21.7713357667235,-13.1703203760581));
#47819=CARTESIAN_POINT('Ctrl Pts',(18.8910411442612,21.7661786784898,-13.1744899420021));
#47820=CARTESIAN_POINT('Ctrl Pts',(18.9779010492718,21.7608402733959,-13.1788061047411));
#47821=CARTESIAN_POINT('Ctrl Pts',(19.0644574681807,21.7510697851064,-13.18312226748));
#47822=CARTESIAN_POINT('Ctrl Pts',(19.1502297723789,21.7369360198915,-13.1874384302189));
#47823=CARTESIAN_POINT('Ctrl Pts',(19.2332080527895,21.7232626605919,-13.1916139944106));
#47824=CARTESIAN_POINT('Ctrl Pts',(19.3154520685911,21.7055060719794,-13.1957895586023));
#47825=CARTESIAN_POINT('Ctrl Pts',(19.3965387044154,21.6837803107335,-13.1999651227939));
#47826=CARTESIAN_POINT('Ctrl Pts',(19.4817208334499,21.6609572329353,-13.2043515848065));
#47827=CARTESIAN_POINT('Ctrl Pts',(19.5656250358875,21.6337536591884,-13.208738046819));
#47828=CARTESIAN_POINT('Ctrl Pts',(19.6477828618951,21.6023596302745,-13.2131245088315));
#47829=CARTESIAN_POINT('Ctrl Pts',(19.7299406879028,21.5709656013606,-13.2175109708441));
#47830=CARTESIAN_POINT('Ctrl Pts',(19.8103516376766,21.5353814216376,-13.2218974328566));
#47831=CARTESIAN_POINT('Ctrl Pts',(19.8885775886019,21.4958524223455,-13.2262838948691));
#47832=CARTESIAN_POINT('Ctrl Pts',(19.9631842212833,21.4581523305529,-13.2304674063033));
#47833=CARTESIAN_POINT('Ctrl Pts',(20.0360812001486,21.4167240952575,-13.2346509177374));
#47834=CARTESIAN_POINT('Ctrl Pts',(20.1068712604686,21.3717462836204,-13.2388344291715));
#47835=CARTESIAN_POINT('Ctrl Pts',(20.1709100371252,21.3310580285051,-13.2426189570156));
#47836=CARTESIAN_POINT('Ctrl Pts',(20.2332245698872,21.2874656707164,-13.2464034848598));
#47837=CARTESIAN_POINT('Ctrl Pts',(20.2935358855687,21.2411349269503,-13.2501880127039));
#47838=CARTESIAN_POINT('Ctrl Pts',(20.2954167287344,21.2436206075649,-12.4500366863435));
#47839=CARTESIAN_POINT('Ctrl Pts',(20.3656979514168,21.1904720313874,-12.4544341424892));
#47840=CARTESIAN_POINT('Ctrl Pts',(21.0821531671319,20.5851355586758,-12.5012235341954));
#47841=CARTESIAN_POINT('Ctrl Pts',(21.7088252035205,18.6509044816894,-12.590404861462));
#47842=CARTESIAN_POINT('Ctrl Pts',(19.8732647667815,16.4064736991244,-12.7175806681434));
#47843=CARTESIAN_POINT('Ctrl Pts',(17.0319370398065,16.7305239353302,-12.8430154491721));
#47844=CARTESIAN_POINT('Ctrl Pts',(16.1727139355615,18.3978728515243,-12.9260582946402));
#47845=CARTESIAN_POINT('Ctrl Pts',(16.1699654719056,19.2116308397489,-12.9667092045479));
#47846=CARTESIAN_POINT('Origin',(18.734,19.211,1.76670989022852));
#47847=CARTESIAN_POINT('',(20.2935358855687,21.2411349269503,-11.650072531177));
#47848=CARTESIAN_POINT('',(20.2935358855687,21.2411349269503,-11.7167617888358));
#47849=CARTESIAN_POINT('',(20.2935358855687,21.2411349269503,1.76670989022852));
#47850=CARTESIAN_POINT('',(16.1740010233873,19.2087109517327,-12.2332901098107));
#47851=CARTESIAN_POINT('Ctrl Pts',(20.2935358855687,21.2411349269503,-11.7167617888358));
#47852=CARTESIAN_POINT('Ctrl Pts',(20.3600167937585,21.1900647440522,-11.7209383136263));
#47853=CARTESIAN_POINT('Ctrl Pts',(20.4240745352904,21.135657894152,-11.7251148384167));
#47854=CARTESIAN_POINT('Ctrl Pts',(20.4853583496099,21.0781753884549,-11.7292913632071));
#47855=CARTESIAN_POINT('Ctrl Pts',(20.5465832892312,21.0207481055799,-11.7334638756552));
#47856=CARTESIAN_POINT('Ctrl Pts',(20.6050392636091,20.9602513525623,-11.7376363881034));
#47857=CARTESIAN_POINT('Ctrl Pts',(20.6604085763013,20.8969863573448,-11.7418089005516));
#47858=CARTESIAN_POINT('Ctrl Pts',(20.7157495989849,20.8337536863006,-11.7459792811255));
#47859=CARTESIAN_POINT('Ctrl Pts',(20.7680067888956,20.7677559268922,-11.7501496616994));
#47860=CARTESIAN_POINT('Ctrl Pts',(20.8169001522236,20.6993302576602,-11.7543200422733));
#47861=CARTESIAN_POINT('Ctrl Pts',(20.865783201272,20.6309190231374,-11.7584895430863));
#47862=CARTESIAN_POINT('Ctrl Pts',(20.9113035661553,20.5600812704941,-11.7626590438993));
#47863=CARTESIAN_POINT('Ctrl Pts',(20.9532231556077,20.4871851690152,-11.7668285447122));
#47864=CARTESIAN_POINT('Ctrl Pts',(20.9951464766831,20.4142825784279,-11.7709984166883));
#47865=CARTESIAN_POINT('Ctrl Pts',(21.0334681576709,20.3393216746274,-11.7751682886644));
#47866=CARTESIAN_POINT('Ctrl Pts',(21.0679955410099,20.2626961607546,-11.7793381606404));
#47867=CARTESIAN_POINT('Ctrl Pts',(21.1025593312112,20.1859898503005,-11.7835124294732));
#47868=CARTESIAN_POINT('Ctrl Pts',(21.1333206459673,20.1076158454035,-11.7876866983059));
#47869=CARTESIAN_POINT('Ctrl Pts',(21.1601347931878,20.0279883507638,-11.7918609671386));
#47870=CARTESIAN_POINT('Ctrl Pts',(21.1869637575432,19.9483168550479,-11.7960375426158));
#47871=CARTESIAN_POINT('Ctrl Pts',(21.2098410861947,19.8673909332363,-11.800214118093));
#47872=CARTESIAN_POINT('Ctrl Pts',(21.2286725239124,19.7856381456505,-11.8043906935702));
#47873=CARTESIAN_POINT('Ctrl Pts',(21.24753646193,19.7037442647422,-11.8085744772042));
#47874=CARTESIAN_POINT('Ctrl Pts',(21.2623404822881,19.621021121095,-11.8127582608381));
#47875=CARTESIAN_POINT('Ctrl Pts',(21.2730418536683,19.5379043672401,-11.8169420444721));
#47876=CARTESIAN_POINT('Ctrl Pts',(21.280709708626,19.4783487093277,-11.8199398514765));
#47877=CARTESIAN_POINT('Ctrl Pts',(21.2862722939427,19.4185911058323,-11.8229376584808));
#47878=CARTESIAN_POINT('Ctrl Pts',(21.2897303495757,19.3587916785811,-11.8259354654852));
#47879=CARTESIAN_POINT('Ctrl Pts',(21.2945574443532,19.2753177459375,-11.8301200998782));
#47880=CARTESIAN_POINT('Ctrl Pts',(21.295299648515,19.1914517330296,-11.8343047342713));
#47881=CARTESIAN_POINT('Ctrl Pts',(21.2919120526423,19.1076272233756,-11.8384893686643));
#47882=CARTESIAN_POINT('Ctrl Pts',(21.2885292785931,19.0239220275358,-11.8426680467483));
#47883=CARTESIAN_POINT('Ctrl Pts',(21.2810283989992,18.940258673335,-11.8468467248322));
#47884=CARTESIAN_POINT('Ctrl Pts',(21.2694164102341,18.8570739812961,-11.8510254029161));
#47885=CARTESIAN_POINT('Ctrl Pts',(21.2575962849158,18.772398263436,-11.8552789808016));
#47886=CARTESIAN_POINT('Ctrl Pts',(21.2415161896732,18.6882190178967,-11.859532558687));
#47887=CARTESIAN_POINT('Ctrl Pts',(21.221239025086,18.604995023049,-11.8637861365725));
#47888=CARTESIAN_POINT('Ctrl Pts',(21.2013549729019,18.5233844877397,-11.8679572505504));
#47889=CARTESIAN_POINT('Ctrl Pts',(21.1774352498115,18.4426929623941,-11.8721283645284));
#47890=CARTESIAN_POINT('Ctrl Pts',(21.1495909652084,18.3633442392081,-11.8762994785063));
#47891=CARTESIAN_POINT('Ctrl Pts',(21.1217560240238,18.2840221422525,-11.8804691928267));
#47892=CARTESIAN_POINT('Ctrl Pts',(21.0899992889567,18.2060423862984,-11.8846389071471));
#47893=CARTESIAN_POINT('Ctrl Pts',(21.0544814935988,18.1298128571493,-11.8888086214674));
#47894=CARTESIAN_POINT('Ctrl Pts',(21.0189649621164,18.0535860405741,-11.8929781874115));
#47895=CARTESIAN_POINT('Ctrl Pts',(20.9796878315031,17.9791097436055,-11.8971477533555));
#47896=CARTESIAN_POINT('Ctrl Pts',(20.9368581017986,17.9067698886545,-11.9013173192996));
#47897=CARTESIAN_POINT('Ctrl Pts',(20.8925225316338,17.8318866536443,-11.9056334820385));
#47898=CARTESIAN_POINT('Ctrl Pts',(20.8443801641988,17.7592933443553,-11.9099496447774));
#47899=CARTESIAN_POINT('Ctrl Pts',(20.7927112772811,17.6893864233007,-11.9142658075163));
#47900=CARTESIAN_POINT('Ctrl Pts',(20.7427254989202,17.6217567128466,-11.918441371708));
#47901=CARTESIAN_POINT('Ctrl Pts',(20.6894397604074,17.5566413947911,-11.9226169358997));
#47902=CARTESIAN_POINT('Ctrl Pts',(20.6331484080961,17.4943651162737,-11.9267925000914));
#47903=CARTESIAN_POINT('Ctrl Pts',(20.5740139133994,17.4289434109761,-11.9311789621039));
#47904=CARTESIAN_POINT('Ctrl Pts',(20.5115626117394,17.3666554945532,-11.9355654241165));
#47905=CARTESIAN_POINT('Ctrl Pts',(20.4461771444977,17.3078317400031,-11.939951886129));
#47906=CARTESIAN_POINT('Ctrl Pts',(20.3807916772559,17.2490079854529,-11.9443383481416));
#47907=CARTESIAN_POINT('Ctrl Pts',(20.3124725431188,17.1936486989611,-11.9487248101541));
#47908=CARTESIAN_POINT('Ctrl Pts',(20.2416377781113,17.1420320616279,-11.9531112721667));
#47909=CARTESIAN_POINT('Ctrl Pts',(20.1740622256442,17.0927903822927,-11.9572959065597));
#47910=CARTESIAN_POINT('Ctrl Pts',(20.1039459219087,17.0467712239067,-11.9614805409528));
#47911=CARTESIAN_POINT('Ctrl Pts',(20.0316291334109,17.0042470387188,-11.9656651753458));
#47912=CARTESIAN_POINT('Ctrl Pts',(19.9594152789105,16.9617833814451,-11.9698438534298));
#47913=CARTESIAN_POINT('Ctrl Pts',(19.8850075541817,16.9228050473158,-11.9740225315137));
#47914=CARTESIAN_POINT('Ctrl Pts',(19.8087770431601,16.887542596152,-11.9782012095977));
#47915=CARTESIAN_POINT('Ctrl Pts',(19.7311801550143,16.8516480908937,-11.9824547874831));
#47916=CARTESIAN_POINT('Ctrl Pts',(19.6516948805984,16.8196042772378,-11.9867083653685));
#47917=CARTESIAN_POINT('Ctrl Pts',(19.57074102681,16.7916065937816,-11.990961943254));
#47918=CARTESIAN_POINT('Ctrl Pts',(19.4913566214457,16.7641517000523,-11.9951330572319));
#47919=CARTESIAN_POINT('Ctrl Pts',(19.4105605259053,16.7405876095593,-11.9993041712099));
#47920=CARTESIAN_POINT('Ctrl Pts',(19.3287692237664,16.721050287564,-12.0034752851878));
#47921=CARTESIAN_POINT('Ctrl Pts',(19.2470053674889,16.7015195215057,-12.0076449995082));
#47922=CARTESIAN_POINT('Ctrl Pts',(19.1642474149177,16.68601294719,-12.0118147138286));
#47923=CARTESIAN_POINT('Ctrl Pts',(19.0809253355089,16.6746161939521,-12.015984428149));
#47924=CARTESIAN_POINT('Ctrl Pts',(18.9976062210572,16.6632198462596,-12.020153994093));
#47925=CARTESIAN_POINT('Ctrl Pts',(18.9137234755848,16.6559330903703,-12.024323560037));
#47926=CARTESIAN_POINT('Ctrl Pts',(18.8297141852422,16.6527899236491,-12.0284931259811));
#47927=CARTESIAN_POINT('Ctrl Pts',(18.7427512318879,16.6495362470634,-12.03280928872));
#47928=CARTESIAN_POINT('Ctrl Pts',(18.6556531965159,16.6507229779044,-12.0371254514589));
#47929=CARTESIAN_POINT('Ctrl Pts',(18.5689051504086,16.6563290445464,-12.0414416141978));
#47930=CARTESIAN_POINT('Ctrl Pts',(18.4849829127789,16.6617524941571,-12.0456171783895));
#47931=CARTESIAN_POINT('Ctrl Pts',(18.4013886754037,16.6713116809417,-12.0497927425812));
#47932=CARTESIAN_POINT('Ctrl Pts',(18.3185547392491,16.6849348315375,-12.0539683067729));
#47933=CARTESIAN_POINT('Ctrl Pts',(18.2315370578984,16.6992460550839,-12.0583547687854));
#47934=CARTESIAN_POINT('Ctrl Pts',(18.1453590723574,16.7180424488713,-12.062741230798));
#47935=CARTESIAN_POINT('Ctrl Pts',(18.0605056905574,16.7411810966898,-12.0671276928105));
#47936=CARTESIAN_POINT('Ctrl Pts',(17.9756523087575,16.7643197445083,-12.071514154823));
#47937=CARTESIAN_POINT('Ctrl Pts',(17.8921240580815,16.7918003927741,-12.0759006168356));
#47938=CARTESIAN_POINT('Ctrl Pts',(17.8103811197834,16.8234221134992,-12.0802870788481));
#47939=CARTESIAN_POINT('Ctrl Pts',(17.7323992952485,16.8535888719792,-12.0844717132412));
#47940=CARTESIAN_POINT('Ctrl Pts',(17.6557518403844,16.8876362896632,-12.0886563476342));
#47941=CARTESIAN_POINT('Ctrl Pts',(17.5808520242221,16.9254257295027,-12.0928409820273));
#47942=CARTESIAN_POINT('Ctrl Pts',(17.5060588186774,16.963161380752,-12.0970196601112));
#47943=CARTESIAN_POINT('Ctrl Pts',(17.4330087179883,17.0046282689895,-12.1011983381951));
#47944=CARTESIAN_POINT('Ctrl Pts',(17.3620964471734,17.0496391690091,-12.1053770162791));
#47945=CARTESIAN_POINT('Ctrl Pts',(17.2899131248678,17.0954568570628,-12.1096305941645));
#47946=CARTESIAN_POINT('Ctrl Pts',(17.2199454771428,17.1449466854561,-12.11388417205));
#47947=CARTESIAN_POINT('Ctrl Pts',(17.1525850704413,17.1978614502303,-12.1181377499354));
#47948=CARTESIAN_POINT('Ctrl Pts',(17.0865305766667,17.2497503590347,-12.1223088639134));
#47949=CARTESIAN_POINT('Ctrl Pts',(17.0229835115634,17.3049322938693,-12.1264799778913));
#47950=CARTESIAN_POINT('Ctrl Pts',(16.9622836350606,17.3631306533724,-12.1306510918693));
#47951=CARTESIAN_POINT('Ctrl Pts',(16.9016041269875,17.421309483854,-12.1348208061896));
#47952=CARTESIAN_POINT('Ctrl Pts',(16.8437702418585,17.4825024106647,-12.13899052051));
#47953=CARTESIAN_POINT('Ctrl Pts',(16.789086714705,17.5463942470714,-12.1431602348304));
#47954=CARTESIAN_POINT('Ctrl Pts',(16.734405133426,17.6102838099324,-12.1473298007744));
#47955=CARTESIAN_POINT('Ctrl Pts',(16.6828739857151,17.6768717413838,-12.1514993667185));
#47956=CARTESIAN_POINT('Ctrl Pts',(16.6347584444193,17.7458089232721,-12.1556689326625));
#47957=CARTESIAN_POINT('Ctrl Pts',(16.5849512200484,17.8171698514323,-12.1599850954014));
#47958=CARTESIAN_POINT('Ctrl Pts',(16.5388045582795,17.8910478705134,-12.1643012581403));
#47959=CARTESIAN_POINT('Ctrl Pts',(16.496563301095,17.9670237066595,-12.1686174208793));
#47960=CARTESIAN_POINT('Ctrl Pts',(16.4556980484203,18.0405246379344,-12.1727929850709));
#47961=CARTESIAN_POINT('Ctrl Pts',(16.4184878365309,18.1159883689942,-12.1769685492626));
#47962=CARTESIAN_POINT('Ctrl Pts',(16.3851063117011,18.1930125535796,-12.1811441134543));
#47963=CARTESIAN_POINT('Ctrl Pts',(16.3500387654091,18.2739270466208,-12.1855305754669));
#47964=CARTESIAN_POINT('Ctrl Pts',(16.3191970489119,18.3565632259542,-12.1899170374794));
#47965=CARTESIAN_POINT('Ctrl Pts',(16.2927234637602,18.4404360029142,-12.1943034994919));
#47966=CARTESIAN_POINT('Ctrl Pts',(16.2662498786085,18.5243087798742,-12.1986899615045));
#47967=CARTESIAN_POINT('Ctrl Pts',(16.2441444970407,18.6094175737551,-12.203076423517));
#47968=CARTESIAN_POINT('Ctrl Pts',(16.2264874578015,18.6952666864385,-12.2074628855296));
#47969=CARTESIAN_POINT('Ctrl Pts',(16.2025156137663,18.811818590295,-12.2134181072293));
#47970=CARTESIAN_POINT('Ctrl Pts',(16.1866633864877,18.9300931627176,-12.219373328929));
#47971=CARTESIAN_POINT('Ctrl Pts',(16.1791211348988,19.0491544419537,-12.2253285506288));
#47972=CARTESIAN_POINT('Ctrl Pts',(16.1757600463661,19.10221227165,-12.2279824036764));
#47973=CARTESIAN_POINT('Ctrl Pts',(16.1740486686438,19.1554260264049,-12.2306362567239));
#47974=CARTESIAN_POINT('Ctrl Pts',(16.174001023388,19.2087109509454,-12.2332901097715));
#47975=CARTESIAN_POINT('Ctrl Pts',(16.1740010233873,19.2087109517327,-12.2332901098107));
#47976=CARTESIAN_POINT('Ctrl Pts',(16.1739252094451,19.293498859929,-12.2375129674107));
#47977=CARTESIAN_POINT('Ctrl Pts',(16.1780663695147,19.3784221563148,-12.2417358250107));
#47978=CARTESIAN_POINT('Ctrl Pts',(16.1864353355331,19.4630203967139,-12.2459586826108));
#47979=CARTESIAN_POINT('Ctrl Pts',(16.1945865434513,19.5454174151127,-12.2500716626647));
#47980=CARTESIAN_POINT('Ctrl Pts',(16.2067481850334,19.6275055813485,-12.2541846427187));
#47981=CARTESIAN_POINT('Ctrl Pts',(16.2228775801224,19.7088596111236,-12.2582976227727));
#47982=CARTESIAN_POINT('Ctrl Pts',(16.2389992540558,19.7901746966527,-12.2624086339395));
#47983=CARTESIAN_POINT('Ctrl Pts',(16.25908482094,19.8707558783837,-12.2665196451063));
#47984=CARTESIAN_POINT('Ctrl Pts',(16.2830401055299,19.9501857653521,-12.2706306562731));
#47985=CARTESIAN_POINT('Ctrl Pts',(16.3069915898918,20.0296030516901,-12.2747410152757));
#47986=CARTESIAN_POINT('Ctrl Pts',(16.3348114354692,20.1078689519365,-12.2788513742782));
#47987=CARTESIAN_POINT('Ctrl Pts',(16.366355393672,20.1845805144548,-12.2829617332808));
#47988=CARTESIAN_POINT('Ctrl Pts',(16.3994039228381,20.264951034063,-12.2872681465249));
#47989=CARTESIAN_POINT('Ctrl Pts',(16.4365404963283,20.3436147061446,-12.2915745597691));
#47990=CARTESIAN_POINT('Ctrl Pts',(16.4775431085385,20.4201328698599,-12.2958809730133));
#47991=CARTESIAN_POINT('Ctrl Pts',(16.5167281737211,20.4932591677035,-12.2999964933322));
#47992=CARTESIAN_POINT('Ctrl Pts',(16.5594435017451,20.5644257408165,-12.304112013651));
#47993=CARTESIAN_POINT('Ctrl Pts',(16.6054498638678,20.6332778624347,-12.3082275339699));
#47994=CARTESIAN_POINT('Ctrl Pts',(16.6514869443887,20.7021759565399,-12.3123458022172));
#47995=CARTESIAN_POINT('Ctrl Pts',(16.7008191449123,20.768756147345,-12.3164640704645));
#47996=CARTESIAN_POINT('Ctrl Pts',(16.7531665958489,20.8326963417974,-12.3205823387118));
#47997=CARTESIAN_POINT('Ctrl Pts',(16.8055945346489,20.8967348487664,-12.3247069390843));
#47998=CARTESIAN_POINT('Ctrl Pts',(16.8610466479906,20.9581249187389,-12.3288315394568));
#47999=CARTESIAN_POINT('Ctrl Pts',(16.9192065009781,21.0165815007659,-12.3329561398293));
#48000=CARTESIAN_POINT('Ctrl Pts',(16.9271149034352,21.0245302515482,-12.3335169906232));
#48001=CARTESIAN_POINT('Ctrl Pts',(16.93507332294,21.0324248251516,-12.3340778414171));
#48002=CARTESIAN_POINT('Ctrl Pts',(16.9430809195058,21.040264564551,-12.334638692211));
#48003=CARTESIAN_POINT('Ctrl Pts',(17.0028274053093,21.0987586301397,-12.338823326604));
#48004=CARTESIAN_POINT('Ctrl Pts',(17.0655538444182,21.1544313597729,-12.3430079609971));
#48005=CARTESIAN_POINT('Ctrl Pts',(17.1309629349571,21.2069639696394,-12.3471925953901));
#48006=CARTESIAN_POINT('Ctrl Pts',(17.1962789237517,21.259421805838,-12.3513712734741));
#48007=CARTESIAN_POINT('Ctrl Pts',(17.2642696237805,21.3087481146435,-12.355549951558));
#48008=CARTESIAN_POINT('Ctrl Pts',(17.3346011829193,21.3546611091199,-12.3597286296419));
#48009=CARTESIAN_POINT('Ctrl Pts',(17.4061933847094,21.4013970610253,-12.3639822075274));
#48010=CARTESIAN_POINT('Ctrl Pts',(17.4802108463241,21.4445957903897,-12.3682357854128));
#48011=CARTESIAN_POINT('Ctrl Pts',(17.5562664269212,21.484003218397,-12.3724893632982));
#48012=CARTESIAN_POINT('Ctrl Pts',(17.6308475216781,21.522646656515,-12.3766604772762));
#48013=CARTESIAN_POINT('Ctrl Pts',(17.7073879875327,21.5576442636058,-12.3808315912541));
#48014=CARTESIAN_POINT('Ctrl Pts',(17.7854953736982,21.5888012898231,-12.3850027052321));
#48015=CARTESIAN_POINT('Ctrl Pts',(17.863576550176,21.6199478609992,-12.3891724195525));
#48016=CARTESIAN_POINT('Ctrl Pts',(17.9432231757909,21.6472562404631,-12.3933421338728));
#48017=CARTESIAN_POINT('Ctrl Pts',(18.0240221782528,21.6705795357392,-12.3975118481932));
#48018=CARTESIAN_POINT('Ctrl Pts',(18.1048183055395,21.6939020010724,-12.4016814141373));
#48019=CARTESIAN_POINT('Ctrl Pts',(18.186766285918,21.713239537401,-12.4058509800813));
#48020=CARTESIAN_POINT('Ctrl Pts',(18.2694385404879,21.7284953128727,-12.4100205460253));
#48021=CARTESIAN_POINT('Ctrl Pts',(18.3550174495411,21.7442874625899,-12.4143367087643));
#48022=CARTESIAN_POINT('Ctrl Pts',(18.4413719926986,21.7557053858609,-12.4186528715032));
#48023=CARTESIAN_POINT('Ctrl Pts',(18.5280191484746,21.762699803818,-12.4229690342421));
#48024=CARTESIAN_POINT('Ctrl Pts',(18.6118437822649,21.7694663793459,-12.4271445984338));
#48025=CARTESIAN_POINT('Ctrl Pts',(18.6959417854331,21.7720932477196,-12.4313201626255));
#48026=CARTESIAN_POINT('Ctrl Pts',(18.7798750222012,21.7705889283903,-12.4354957268171));
#48027=CARTESIAN_POINT('Ctrl Pts',(18.8680475272262,21.7690086294678,-12.4398821888297));
#48028=CARTESIAN_POINT('Ctrl Pts',(18.9560376012523,21.7628688832023,-12.4442686508422));
#48029=CARTESIAN_POINT('Ctrl Pts',(19.0433447687653,21.7522409988109,-12.4486551128548));
#48030=CARTESIAN_POINT('Ctrl Pts',(19.1306519362783,21.7416131144196,-12.4530415748673));
#48031=CARTESIAN_POINT('Ctrl Pts',(19.2172756387742,21.7264972665759,-12.4574280368799));
#48032=CARTESIAN_POINT('Ctrl Pts',(19.3027314805894,21.7070257416514,-12.4618144988924));
#48033=CARTESIAN_POINT('Ctrl Pts',(19.3842631981423,21.6884483473301,-12.4659995349797));
#48034=CARTESIAN_POINT('Ctrl Pts',(19.4650354649563,21.6658373731213,-12.4701845710669));
#48035=CARTESIAN_POINT('Ctrl Pts',(19.5446191872091,21.6392702760048,-12.4743696071542));
#48036=CARTESIAN_POINT('Ctrl Pts',(19.6240693838798,21.6127477531682,-12.4785476215872));
#48037=CARTESIAN_POINT('Ctrl Pts',(19.7023345681446,21.5822824489793,-12.4827256360202));
#48038=CARTESIAN_POINT('Ctrl Pts',(19.7789972930808,21.5480024941052,-12.4869036504532));
#48039=CARTESIAN_POINT('Ctrl Pts',(19.8555857432778,21.5137557513914,-12.4910776170138));
#48040=CARTESIAN_POINT('Ctrl Pts',(19.9305743987691,21.4757018818008,-12.4952515835744));
#48041=CARTESIAN_POINT('Ctrl Pts',(20.003563194091,21.4340180602527,-12.4994255501349));
#48042=CARTESIAN_POINT('Ctrl Pts',(20.0764986900058,21.392364677938,-12.5035964686942));
#48043=CARTESIAN_POINT('Ctrl Pts',(20.1474368294337,21.3470868385682,-12.5077673872535));
#48044=CARTESIAN_POINT('Ctrl Pts',(20.2160009920406,21.2984082158483,-12.5119383058127));
#48045=CARTESIAN_POINT('Ctrl Pts',(20.2421989287405,21.2798084192757,-12.5135319876465));
#48046=CARTESIAN_POINT('Ctrl Pts',(20.2680505424068,21.2607125947641,-12.5151256694803));
#48047=CARTESIAN_POINT('Ctrl Pts',(20.2935358855687,21.2411349269503,-12.5167193513141));
#48048=CARTESIAN_POINT('',(16.1740007840082,19.2130035272629,-12.1667098902285));
#48049=CARTESIAN_POINT('Ctrl Pts',(16.1763509819005,19.2130199893541,-12.1667107986141));
#48050=CARTESIAN_POINT('Ctrl Pts',(16.174290235218,19.4962014494758,-12.1807663462153));
#48051=CARTESIAN_POINT('Ctrl Pts',(16.3483939114844,20.6310006362221,-12.237213829377));
#48052=CARTESIAN_POINT('Ctrl Pts',(17.9381456425209,22.083154657165,-12.3316557919534));
#48053=CARTESIAN_POINT('Ctrl Pts',(19.6881796398412,21.7028298450405,-12.4120422069287));
#48054=CARTESIAN_POINT('Ctrl Pts',(20.2954167287344,21.2436206075649,-12.4500366863435));
#48055=CARTESIAN_POINT('Ctrl Pts',(20.2935358855687,21.2411349269503,-11.650072531177));
#48056=CARTESIAN_POINT('Ctrl Pts',(20.3602862218061,21.1898577712529,-11.6542476714699));
#48057=CARTESIAN_POINT('Ctrl Pts',(20.4244786660862,21.1353052511714,-11.6584228117628));
#48058=CARTESIAN_POINT('Ctrl Pts',(20.485787760444,21.0777725202494,-11.6625979520557));
#48059=CARTESIAN_POINT('Ctrl Pts',(20.5471067961931,21.0202304602811,-11.6667737693559));
#48060=CARTESIAN_POINT('Ctrl Pts',(20.6055412401485,20.9597075680707,-11.6709495866561));
#48061=CARTESIAN_POINT('Ctrl Pts',(20.6608038249164,20.8965346393022,-11.6751254039563));
#48062=CARTESIAN_POINT('Ctrl Pts',(20.7161667197055,20.8332470420314,-11.6793088010019));
#48063=CARTESIAN_POINT('Ctrl Pts',(20.768345963538,20.7673001572432,-11.6834921980475));
#48064=CARTESIAN_POINT('Ctrl Pts',(20.8170955352535,20.6990567835292,-11.687675595093));
#48065=CARTESIAN_POINT('Ctrl Pts',(20.8656447840932,20.6310938370762,-11.691841801626));
#48066=CARTESIAN_POINT('Ctrl Pts',(20.9107923286134,20.560853665295,-11.696008008159));
#48067=CARTESIAN_POINT('Ctrl Pts',(20.9523407266398,20.4887184433713,-11.700174214692));
#48068=CARTESIAN_POINT('Ctrl Pts',(20.9940729004966,20.4162641547461,-11.704358849085));
#48069=CARTESIAN_POINT('Ctrl Pts',(21.0323293070735,20.3416283299438,-11.7085434834781));
#48070=CARTESIAN_POINT('Ctrl Pts',(21.06687544764,20.265178422184,-11.7127281178711));
#48071=CARTESIAN_POINT('Ctrl Pts',(21.1013724160514,20.1888373314053,-11.7169067959551));
#48072=CARTESIAN_POINT('Ctrl Pts',(21.1321694205716,20.11068770221,-11.721085474039));
#48073=CARTESIAN_POINT('Ctrl Pts',(21.159076910497,20.0311231481761,-11.725264152123));
#48074=CARTESIAN_POINT('Ctrl Pts',(21.1864666978413,19.9501324566932,-11.7295177300084));
#48075=CARTESIAN_POINT('Ctrl Pts',(21.2098259193361,19.8676760341796,-11.7337713078938));
#48076=CARTESIAN_POINT('Ctrl Pts',(21.2290051549002,19.7841921815775,-11.7380248857793));
#48077=CARTESIAN_POINT('Ctrl Pts',(21.2478125635577,19.7023268263635,-11.7421959997572));
#48078=CARTESIAN_POINT('Ctrl Pts',(21.2626005065823,19.6194739920339,-11.7463671137352));
#48079=CARTESIAN_POINT('Ctrl Pts',(21.2732783407021,19.5360623147049,-11.7505382277131));
#48080=CARTESIAN_POINT('Ctrl Pts',(21.2839525917715,19.4526786269698,-11.7547079420335));
#48081=CARTESIAN_POINT('Ctrl Pts',(21.2905194146576,19.3687369245927,-11.7588776563539));
#48082=CARTESIAN_POINT('Ctrl Pts',(21.2929396556081,19.2846738688838,-11.7630473706742));
#48083=CARTESIAN_POINT('Ctrl Pts',(21.295359810436,19.2006138044992,-11.7672169366183));
#48084=CARTESIAN_POINT('Ctrl Pts',(21.2936336643145,19.1164328552356,-11.7713865025623));
#48085=CARTESIAN_POINT('Ctrl Pts',(21.2877741604491,19.0325692363337,-11.7755560685064));
#48086=CARTESIAN_POINT('Ctrl Pts',(21.2817086436563,18.945757076048,-11.7798722312453));
#48087=CARTESIAN_POINT('Ctrl Pts',(21.2712137402019,18.859285502122,-11.7841883939842));
#48088=CARTESIAN_POINT('Ctrl Pts',(21.2563622783628,18.7736345501841,-11.7885045567231));
#48089=CARTESIAN_POINT('Ctrl Pts',(21.241994601331,18.6907736689967,-11.7926801209148));
#48090=CARTESIAN_POINT('Ctrl Pts',(21.2235499863026,18.6086812165374,-11.7968556851065));
#48091=CARTESIAN_POINT('Ctrl Pts',(21.2011460288054,18.5277793383177,-11.8010312492982));
#48092=CARTESIAN_POINT('Ctrl Pts',(21.1776105006754,18.442791298555,-11.8054177113107));
#48093=CARTESIAN_POINT('Ctrl Pts',(21.1497053305466,18.3591178195345,-11.8098041733232));
#48094=CARTESIAN_POINT('Ctrl Pts',(21.1176244749813,18.27722574341,-11.8141906353358));
#48095=CARTESIAN_POINT('Ctrl Pts',(21.085543619416,18.1953336672855,-11.8185770973483));
#48096=CARTESIAN_POINT('Ctrl Pts',(21.0492873869465,18.115223491295,-11.8229635593609));
#48097=CARTESIAN_POINT('Ctrl Pts',(21.0091047687183,18.0373312684769,-11.8273500213734));
#48098=CARTESIAN_POINT('Ctrl Pts',(20.9707710123198,17.9630229822945,-11.8315346557664));
#48099=CARTESIAN_POINT('Ctrl Pts',(20.9287215623263,17.8904564421858,-11.8357192901595));
#48100=CARTESIAN_POINT('Ctrl Pts',(20.8831384590298,17.8200277199315,-11.8399039245525));
#48101=CARTESIAN_POINT('Ctrl Pts',(20.8376202376387,17.7496992442458,-11.8440826026365));
#48102=CARTESIAN_POINT('Ctrl Pts',(20.7885786013676,17.6815029251172,-11.8482612807204));
#48103=CARTESIAN_POINT('Ctrl Pts',(20.7362419167444,17.615811200255,-11.8524399588044));
#48104=CARTESIAN_POINT('Ctrl Pts',(20.682967134663,17.5489419984366,-11.8566935366898));
#48105=CARTESIAN_POINT('Ctrl Pts',(20.6262782358934,17.4846684922396,-11.8609471145753));
#48106=CARTESIAN_POINT('Ctrl Pts',(20.566462883909,17.423353564293,-11.8652006924607));
#48107=CARTESIAN_POINT('Ctrl Pts',(20.5078071692429,17.3632273458709,-11.8693718064386));
#48108=CARTESIAN_POINT('Ctrl Pts',(20.4461454804008,17.3059463582357,-11.8735429204166));
#48109=CARTESIAN_POINT('Ctrl Pts',(20.3817891690391,17.2518188306343,-11.8777140343945));
#48110=CARTESIAN_POINT('Ctrl Pts',(20.3174544530593,17.1977094660475,-11.8818837487149));
#48111=CARTESIAN_POINT('Ctrl Pts',(20.2504272621012,17.1467517558061,-11.8860534630353));
#48112=CARTESIAN_POINT('Ctrl Pts',(20.1810535660399,17.0992149785049,-11.8902231773557));
#48113=CARTESIAN_POINT('Ctrl Pts',(20.1116823385924,17.0516798927661,-11.8943927432997));
#48114=CARTESIAN_POINT('Ctrl Pts',(20.0399651520288,17.0075657572672,-11.8985623092438));
#48115=CARTESIAN_POINT('Ctrl Pts',(19.9662774819293,16.967098886419,-11.9027318751878));
#48116=CARTESIAN_POINT('Ctrl Pts',(19.8899990442531,16.9252092503133,-11.9070480379267));
#48117=CARTESIAN_POINT('Ctrl Pts',(19.8116094428164,16.887228380361,-11.9113642006657));
#48118=CARTESIAN_POINT('Ctrl Pts',(19.7315517321804,16.8533548736877,-11.9156803634046));
#48119=CARTESIAN_POINT('Ctrl Pts',(19.6541018930477,16.8205847929315,-11.9198559275963));
#48120=CARTESIAN_POINT('Ctrl Pts',(19.5750914116565,16.791658707737,-11.9240314917879));
#48121=CARTESIAN_POINT('Ctrl Pts',(19.4949388978049,16.7667062382341,-11.9282070559796));
#48122=CARTESIAN_POINT('Ctrl Pts',(19.4107380710233,16.7404934788156,-11.9325935179922));
#48123=CARTESIAN_POINT('Ctrl Pts',(19.325277377455,16.7186664436044,-11.9369799800047));
#48124=CARTESIAN_POINT('Ctrl Pts',(19.2390543424806,16.7013147386293,-11.9413664420172));
#48125=CARTESIAN_POINT('Ctrl Pts',(19.1528313075062,16.6839630336542,-11.9457529040298));
#48126=CARTESIAN_POINT('Ctrl Pts',(19.0658465162266,16.6710866686339,-11.9501393660423));
#48127=CARTESIAN_POINT('Ctrl Pts',(18.9786013944249,16.662712308658,-11.9545258280548));
#48128=CARTESIAN_POINT('Ctrl Pts',(18.8953705500055,16.6547232653983,-11.9587104624479));
#48129=CARTESIAN_POINT('Ctrl Pts',(18.8115930039275,16.6508013065455,-11.9628950968409));
#48130=CARTESIAN_POINT('Ctrl Pts',(18.727700324836,16.6510077511655,-11.967079731234));
#48131=CARTESIAN_POINT('Ctrl Pts',(18.6439270565895,16.6512139019371,-11.9712584093179));
#48132=CARTESIAN_POINT('Ctrl Pts',(18.5600394369387,16.655536782935,-11.9754370874018));
#48133=CARTESIAN_POINT('Ctrl Pts',(18.4764742375278,16.6639859675174,-11.9796157654858));
#48134=CARTESIAN_POINT('Ctrl Pts',(18.3914111919746,16.6725865976612,-11.9838693433712));
#48135=CARTESIAN_POINT('Ctrl Pts',(18.3066827190517,16.6854629604527,-11.9881229212567));
#48136=CARTESIAN_POINT('Ctrl Pts',(18.2227496524051,16.702569597919,-11.9923764991421));
#48137=CARTESIAN_POINT('Ctrl Pts',(18.1404437920373,16.7193445898372,-11.9965476131201));
#48138=CARTESIAN_POINT('Ctrl Pts',(18.0589032436851,16.7401871997925,-12.000718727098));
#48139=CARTESIAN_POINT('Ctrl Pts',(17.9785557081131,16.7650024689597,-12.004889841076));
#48140=CARTESIAN_POINT('Ctrl Pts',(17.8982351339326,16.7898094111236,-12.0090595553964));
#48141=CARTESIAN_POINT('Ctrl Pts',(17.8191072166575,16.8185862293723,-12.0132292697167));
#48142=CARTESIAN_POINT('Ctrl Pts',(17.7415856439034,16.8511877731876,-12.0173989840371));
#48143=CARTESIAN_POINT('Ctrl Pts',(17.6640668296998,16.8837881569,-12.0215685499812));
#48144=CARTESIAN_POINT('Ctrl Pts',(17.5881546700958,16.9202128164542,-12.0257381159252));
#48145=CARTESIAN_POINT('Ctrl Pts',(17.5142426975062,16.9602685360059,-12.0299076818693));
#48146=CARTESIAN_POINT('Ctrl Pts',(17.4377320711406,17.0017325652429,-12.0342238446082));
#48147=CARTESIAN_POINT('Ctrl Pts',(17.3633653656324,17.0470874900869,-12.0385400073471));
#48148=CARTESIAN_POINT('Ctrl Pts',(17.2915493867661,17.096068268624,-12.042856170086));
#48149=CARTESIAN_POINT('Ctrl Pts',(17.2220728058576,17.1434535034522,-12.0470317342777));
#48150=CARTESIAN_POINT('Ctrl Pts',(17.1549836708367,17.1942316733332,-12.0512072984694));
#48151=CARTESIAN_POINT('Ctrl Pts',(17.0906175572635,17.2481209545911,-12.055382862661));
#48152=CARTESIAN_POINT('Ctrl Pts',(17.0230004643096,17.3047320553358,-12.0597693246736));
#48153=CARTESIAN_POINT('Ctrl Pts',(16.9583891293618,17.3647764140015,-12.0641557866861));
#48154=CARTESIAN_POINT('Ctrl Pts',(16.897128197962,17.427884192522,-12.0685422486987));
#48155=CARTESIAN_POINT('Ctrl Pts',(16.8358672665622,17.4909919710426,-12.0729287107112));
#48156=CARTESIAN_POINT('Ctrl Pts',(16.7779570635865,17.5571626827012,-12.0773151727237));
#48157=CARTESIAN_POINT('Ctrl Pts',(16.7236914224212,17.6259891410741,-12.0817016347363));
#48158=CARTESIAN_POINT('Ctrl Pts',(16.6719732357611,17.6915845997261,-12.0858821780095));
#48159=CARTESIAN_POINT('Ctrl Pts',(16.62336875941,17.759841108002,-12.0900627212828));
#48160=CARTESIAN_POINT('Ctrl Pts',(16.5781640651477,17.8304307616062,-12.094243264556));
#48161=CARTESIAN_POINT('Ctrl Pts',(16.5330221281563,17.9009224162283,-12.0984180040186));
#48162=CARTESIAN_POINT('Ctrl Pts',(16.4912708487475,17.9737404018919,-12.1025927434812));
#48163=CARTESIAN_POINT('Ctrl Pts',(16.4531558825329,18.0485241457064,-12.1067674829438));
#48164=CARTESIAN_POINT('Ctrl Pts',(16.4150823671077,18.1232265607011,-12.1109376822935));
#48165=CARTESIAN_POINT('Ctrl Pts',(16.3806375190246,18.1998900805266,-12.1151078816433));
#48166=CARTESIAN_POINT('Ctrl Pts',(16.350022764859,18.2781267276155,-12.1192780809931));
#48167=CARTESIAN_POINT('Ctrl Pts',(16.3194306012405,18.3563056440868,-12.1234452031636));
#48168=CARTESIAN_POINT('Ctrl Pts',(16.2926630858421,18.4360549550053,-12.1276123253342));
#48169=CARTESIAN_POINT('Ctrl Pts',(16.2698743296475,18.5169649283287,-12.1317794475047));
#48170=CARTESIAN_POINT('Ctrl Pts',(16.2470959536793,18.597838047344,-12.1359446715606));
#48171=CARTESIAN_POINT('Ctrl Pts',(16.2282928589741,18.6798703351889,-12.1401098956165));
#48172=CARTESIAN_POINT('Ctrl Pts',(16.2135694673997,18.7626363860258,-12.1442751196725));
#48173=CARTESIAN_POINT('Ctrl Pts',(16.1988435352844,18.8454167182549,-12.1484410624433));
#48174=CARTESIAN_POINT('Ctrl Pts',(16.1881988016352,18.9289306143268,-12.1526070052142));
#48175=CARTESIAN_POINT('Ctrl Pts',(16.181688476361,19.0127428783137,-12.1567729479851));
#48176=CARTESIAN_POINT('Ctrl Pts',(16.1765121589546,19.0793814658902,-12.1600852620662));
#48177=CARTESIAN_POINT('Ctrl Pts',(16.1739485082683,19.146208402676,-12.1633975761474));
#48178=CARTESIAN_POINT('Ctrl Pts',(16.1740007840082,19.2130035272629,-12.1667098902285));
#48179=CARTESIAN_POINT('Origin',(18.734,19.211,1.76670989022852));
#48180=CARTESIAN_POINT('',(20.2922820246455,21.2395345685085,-10.8502164908111));
#48181=CARTESIAN_POINT('',(20.294805058443,21.242816933186,-10.916593671796));
#48182=CARTESIAN_POINT('',(20.2935358855687,21.2411349269503,1.76670989022852));
#48183=CARTESIAN_POINT('',(16.1739804710165,19.212301045312,-11.4332901033202));
#48184=CARTESIAN_POINT('Ctrl Pts',(20.2948050584429,21.242816933186,-10.916593671796));
#48185=CARTESIAN_POINT('Ctrl Pts',(20.3968578837659,21.1659198988778,-10.9229640541024));
#48186=CARTESIAN_POINT('Ctrl Pts',(21.1313726010512,20.5183599193142,-10.9717263719693));
#48187=CARTESIAN_POINT('Ctrl Pts',(21.6797114024885,18.5138092582024,-11.0628806253966));
#48188=CARTESIAN_POINT('Ctrl Pts',(19.7422306313066,16.3567467541765,-11.1900564320781));
#48189=CARTESIAN_POINT('Ctrl Pts',(16.9631832240595,16.8048336241861,-11.3135258905591));
#48190=CARTESIAN_POINT('Ctrl Pts',(16.1754043777096,18.4373668536376,-11.3946034134798));
#48191=CARTESIAN_POINT('Ctrl Pts',(16.1705865747788,19.2122806865248,-11.4332890008399));
#48192=CARTESIAN_POINT('Ctrl Pts',(16.1740003306697,19.212301164443,-11.4332901097715));
#48193=CARTESIAN_POINT('Ctrl Pts',(16.174038011382,19.2864367677247,-11.436996088328));
#48194=CARTESIAN_POINT('Ctrl Pts',(16.1772957565522,19.3604881810636,-11.4407020668845));
#48195=CARTESIAN_POINT('Ctrl Pts',(16.1837535357011,19.4342553948533,-11.444408045441));
#48196=CARTESIAN_POINT('Ctrl Pts',(16.1910453870482,19.5175502156942,-11.448592679834));
#48197=CARTESIAN_POINT('Ctrl Pts',(16.2024358975503,19.6006424250678,-11.4527773142271));
#48198=CARTESIAN_POINT('Ctrl Pts',(16.217906819526,19.6830965019697,-11.4569619486201));
#48199=CARTESIAN_POINT('Ctrl Pts',(16.2333557205591,19.765433215699,-11.4611406267041));
#48200=CARTESIAN_POINT('Ctrl Pts',(16.2528734125179,19.8471331528557,-11.465319304788));
#48201=CARTESIAN_POINT('Ctrl Pts',(16.2763898192683,19.927765093712,-11.4694979828719));
#48202=CARTESIAN_POINT('Ctrl Pts',(16.3003277407088,20.0098423041589,-11.4737515607574));
#48203=CARTESIAN_POINT('Ctrl Pts',(16.3284090988417,20.0908123737401,-11.4780051386428));
#48204=CARTESIAN_POINT('Ctrl Pts',(16.3605053261111,20.1702304379142,-11.4822587165282));
#48205=CARTESIAN_POINT('Ctrl Pts',(16.3919793053844,20.2481088279428,-11.4864298305062));
#48206=CARTESIAN_POINT('Ctrl Pts',(16.4273136905277,20.3244944066986,-11.4906009444841));
#48207=CARTESIAN_POINT('Ctrl Pts',(16.4663372697809,20.3989838980285,-11.4947720584621));
#48208=CARTESIAN_POINT('Ctrl Pts',(16.5053477542952,20.4734483936902,-11.4989417727825));
#48209=CARTESIAN_POINT('Ctrl Pts',(16.5480447610381,20.5460176583688,-11.5031114871028));
#48210=CARTESIAN_POINT('Ctrl Pts',(16.5942102750742,20.6163113296,-11.5072812014232));
#48211=CARTESIAN_POINT('Ctrl Pts',(16.6403741463432,20.6866024994807,-11.5114507673673));
#48212=CARTESIAN_POINT('Ctrl Pts',(16.6900060262588,20.7546178528607,-11.5156203333113));
#48213=CARTESIAN_POINT('Ctrl Pts',(16.7428443053794,20.8200055934583,-11.5197898992554));
#48214=CARTESIAN_POINT('Ctrl Pts',(16.7975403132109,20.8876922863507,-11.5241060619943));
#48215=CARTESIAN_POINT('Ctrl Pts',(16.8556720579015,20.9525627446115,-11.5284222247332));
#48216=CARTESIAN_POINT('Ctrl Pts',(16.916904887788,21.0142651921377,-11.5327383874721));
#48217=CARTESIAN_POINT('Ctrl Pts',(16.9761430646815,21.0739576889257,-11.5369139516638));
#48218=CARTESIAN_POINT('Ctrl Pts',(17.0382830139766,21.1306851185866,-11.5410895158555));
#48219=CARTESIAN_POINT('Ctrl Pts',(17.1029865459478,21.1841687998498,-11.5452650800472));
#48220=CARTESIAN_POINT('Ctrl Pts',(17.1709580995008,21.2403538147083,-11.5496515420597));
#48221=CARTESIAN_POINT('Ctrl Pts',(17.2417585461138,21.2929584378007,-11.5540380040722));
#48222=CARTESIAN_POINT('Ctrl Pts',(17.3149615008576,21.3417110873959,-11.5584244660848));
#48223=CARTESIAN_POINT('Ctrl Pts',(17.3881644556013,21.390463736991,-11.5628109280973));
#48224=CARTESIAN_POINT('Ctrl Pts',(17.4637693807619,21.4353641822178,-11.5671973901099));
#48225=CARTESIAN_POINT('Ctrl Pts',(17.5413224142637,21.4761976020829,-11.5715838521224));
#48226=CARTESIAN_POINT('Ctrl Pts',(17.6153071177329,21.5151522157705,-11.5757684865154));
#48227=CARTESIAN_POINT('Ctrl Pts',(17.6913399834856,21.5505508359911,-11.5799531209085));
#48228=CARTESIAN_POINT('Ctrl Pts',(17.7690449301557,21.5821730668978,-11.5841377553015));
#48229=CARTESIAN_POINT('Ctrl Pts',(17.8466392734521,21.6137502874729,-11.5883164333855));
#48230=CARTESIAN_POINT('Ctrl Pts',(17.9259005477805,21.6415616236984,-11.5924951114694));
#48231=CARTESIAN_POINT('Ctrl Pts',(18.0064282347094,21.6654325874532,-11.5966737895534));
#48232=CARTESIAN_POINT('Ctrl Pts',(18.0883993225523,21.6897314210775,-11.6009273674388));
#48233=CARTESIAN_POINT('Ctrl Pts',(18.1716822438311,21.7099470058045,-11.6051809453242));
#48234=CARTESIAN_POINT('Ctrl Pts',(18.2558333466883,21.7259466498637,-11.6094345232097));
#48235=CARTESIAN_POINT('Ctrl Pts',(18.3383530162092,21.7416361096021,-11.6136056371876));
#48236=CARTESIAN_POINT('Ctrl Pts',(18.4217070321714,21.7532715484977,-11.6177767511656));
#48237=CARTESIAN_POINT('Ctrl Pts',(18.5054636294713,21.7607786428131,-11.6219478651435));
#48238=CARTESIAN_POINT('Ctrl Pts',(18.589192121436,21.7682832180504,-11.6261175794639));
#48239=CARTESIAN_POINT('Ctrl Pts',(18.6733224686327,21.7716621589129,-11.6302872937843));
#48240=CARTESIAN_POINT('Ctrl Pts',(18.7574168390729,21.7708928984721,-11.6344570081046));
#48241=CARTESIAN_POINT('Ctrl Pts',(18.8415082170745,21.7701236654049,-11.6386265740487));
#48242=CARTESIAN_POINT('Ctrl Pts',(18.9255631608593,21.7652065295826,-11.6427961399927));
#48243=CARTESIAN_POINT('Ctrl Pts',(19.0091442611983,21.75617104249,-11.6469657059368));
#48244=CARTESIAN_POINT('Ctrl Pts',(19.095663969917,21.7468178788177,-11.6512818686757));
#48245=CARTESIAN_POINT('Ctrl Pts',(19.1816753701872,21.7330514297719,-11.6555980314146));
#48246=CARTESIAN_POINT('Ctrl Pts',(19.2667015333779,21.7149626747092,-11.6599141941535));
#48247=CARTESIAN_POINT('Ctrl Pts',(19.3489579782457,21.6974631589401,-11.6640897583452));
#48248=CARTESIAN_POINT('Ctrl Pts',(19.4302919452563,21.6759187771978,-11.6682653225369));
#48249=CARTESIAN_POINT('Ctrl Pts',(19.510286051879,21.6504630486355,-11.6724408867286));
#48250=CARTESIAN_POINT('Ctrl Pts',(19.5943204706596,21.6237216117387,-11.6768273487411));
#48251=CARTESIAN_POINT('Ctrl Pts',(19.6768755727334,21.5926635253051,-11.6812138107537));
#48252=CARTESIAN_POINT('Ctrl Pts',(19.757492206768,21.557500309543,-11.6856002727662));
#48253=CARTESIAN_POINT('Ctrl Pts',(19.8381088408025,21.5223370937809,-11.6899867347787));
#48254=CARTESIAN_POINT('Ctrl Pts',(19.9167865216175,21.4830690758565,-11.6943731967913));
#48255=CARTESIAN_POINT('Ctrl Pts',(19.9930989518204,21.4399616034209,-11.6987596588038));
#48256=CARTESIAN_POINT('Ctrl Pts',(20.0658940459184,21.3988410087297,-11.7029439432528));
#48257=CARTESIAN_POINT('Ctrl Pts',(20.1368080586073,21.3540740524687,-11.7071282277018));
#48258=CARTESIAN_POINT('Ctrl Pts',(20.2054522028114,21.3058576120685,-11.7113125121507));
#48259=CARTESIAN_POINT('Ctrl Pts',(20.2352510799466,21.2849265363003,-11.7131289377124));
#48260=CARTESIAN_POINT('Ctrl Pts',(20.2646224642289,21.2633460211763,-11.7149453632741));
#48261=CARTESIAN_POINT('Ctrl Pts',(20.2935358855687,21.2411349269503,-11.7167617888358));
#48262=CARTESIAN_POINT('',(16.1740004874608,19.2094201902091,-11.3667098902285));
#48263=CARTESIAN_POINT('Ctrl Pts',(16.1740004874608,19.2094201902091,-11.3667098902285));
#48264=CARTESIAN_POINT('Ctrl Pts',(16.1739481146197,19.2942876523606,-11.3709134538372));
#48265=CARTESIAN_POINT('Ctrl Pts',(16.1781202862138,19.3791700299234,-11.3751170174459));
#48266=CARTESIAN_POINT('Ctrl Pts',(16.1864949217896,19.463622003183,-11.3793205810546));
#48267=CARTESIAN_POINT('Ctrl Pts',(16.1948707822013,19.5480863280015,-11.3835247594573));
#48268=CARTESIAN_POINT('Ctrl Pts',(16.2074502833288,19.6321196761629,-11.3877289378599));
#48269=CARTESIAN_POINT('Ctrl Pts',(16.2241595327125,19.7152824890538,-11.3919331162626));
#48270=CARTESIAN_POINT('Ctrl Pts',(16.2408759290273,19.7984808725962,-11.3961390928892));
#48271=CARTESIAN_POINT('Ctrl Pts',(16.2617254950327,19.8808075406061,-11.4003450695159));
#48272=CARTESIAN_POINT('Ctrl Pts',(16.2865836343726,19.9618349574034,-11.4045510461425));
#48273=CARTESIAN_POINT('Ctrl Pts',(16.3114761780105,20.0429745182097,-11.408762843948));
#48274=CARTESIAN_POINT('Ctrl Pts',(16.3403882340966,20.1228108093805,-11.4129746417534));
#48275=CARTESIAN_POINT('Ctrl Pts',(16.3731460171587,20.200933569338,-11.4171864395589));
#48276=CARTESIAN_POINT('Ctrl Pts',(16.4059305542806,20.27912013401,-11.4214016772397));
#48277=CARTESIAN_POINT('Ctrl Pts',(16.4425668768386,20.3555899771936,-11.4256169149205));
#48278=CARTESIAN_POINT('Ctrl Pts',(16.4828349986459,20.4299569872143,-11.4298321526013));
#48279=CARTESIAN_POINT('Ctrl Pts',(16.5231739006092,20.5044547137505,-11.4340547994973));
#48280=CARTESIAN_POINT('Ctrl Pts',(16.5671571084148,20.5768418481604,-11.4382774463933));
#48281=CARTESIAN_POINT('Ctrl Pts',(16.6145212917448,20.646761124022,-11.4425000932893));
#48282=CARTESIAN_POINT('Ctrl Pts',(16.6269438222718,20.6650993339888,-11.4436075959693));
#48283=CARTESIAN_POINT('Ctrl Pts',(16.6395987151329,20.6832679625289,-11.4447150986492));
#48284=CARTESIAN_POINT('Ctrl Pts',(16.6524807786036,20.7012609606902,-11.4458226013291));
#48285=CARTESIAN_POINT('Ctrl Pts',(16.7011549053849,20.7692464566217,-11.4500072357222));
#48286=CARTESIAN_POINT('Ctrl Pts',(16.7532538754925,20.8349713096213,-11.4541918701152));
#48287=CARTESIAN_POINT('Ctrl Pts',(16.8085402991528,20.8980699275411,-11.4583765045082));
#48288=CARTESIAN_POINT('Ctrl Pts',(16.8637480294321,20.9610787323883,-11.4625551825922));
#48289=CARTESIAN_POINT('Ctrl Pts',(16.9221339008884,21.0214683841931,-11.4667338606761));
#48290=CARTESIAN_POINT('Ctrl Pts',(16.9834181011141,21.0789033741853,-11.4709125387601));
#48291=CARTESIAN_POINT('Ctrl Pts',(17.0458007765846,21.1373678450953,-11.4751661166455));
#48292=CARTESIAN_POINT('Ctrl Pts',(17.1111864272472,21.1927702956729,-11.479419694531));
#48293=CARTESIAN_POINT('Ctrl Pts',(17.1792379481545,21.2447932446887,-11.4836732724164));
#48294=CARTESIAN_POINT('Ctrl Pts',(17.2459701575374,21.2958076273233,-11.4878443863943));
#48295=CARTESIAN_POINT('Ctrl Pts',(17.3152654110889,21.3435720832561,-11.4920155003723));
#48296=CARTESIAN_POINT('Ctrl Pts',(17.3867710660548,21.3878266351598,-11.4961866143502));
#48297=CARTESIAN_POINT('Ctrl Pts',(17.4582527266078,21.4320663370212,-11.5003563286706));
#48298=CARTESIAN_POINT('Ctrl Pts',(17.5319429246536,21.4727982320514,-11.504526042991));
#48299=CARTESIAN_POINT('Ctrl Pts',(17.6074603942082,21.5098058892787,-11.5086957573114));
#48300=CARTESIAN_POINT('Ctrl Pts',(17.6829751765272,21.5468122296147,-11.5128653232554));
#48301=CARTESIAN_POINT('Ctrl Pts',(17.7603166876031,21.5800943939659,-11.5170348891995));
#48302=CARTESIAN_POINT('Ctrl Pts',(17.8390806772785,21.6094827299398,-11.5212044551435));
#48303=CARTESIAN_POINT('Ctrl Pts',(17.9206139116649,21.6399043235521,-11.5255206178824));
#48304=CARTESIAN_POINT('Ctrl Pts',(18.0036710203273,21.6661529958308,-11.5298367806213));
#48305=CARTESIAN_POINT('Ctrl Pts',(18.0877848913439,21.6880962906889,-11.5341529433603));
#48306=CARTESIAN_POINT('Ctrl Pts',(18.1691587618594,21.709324785025,-11.5383285075519));
#48307=CARTESIAN_POINT('Ctrl Pts',(18.2515211332009,21.7265240396989,-11.5425040717436));
#48308=CARTESIAN_POINT('Ctrl Pts',(18.3344390537293,21.7396263168399,-11.5466796359353));
#48309=CARTESIAN_POINT('Ctrl Pts',(18.4215449613048,21.7533903588515,-11.5510660979478));
#48310=CARTESIAN_POINT('Ctrl Pts',(18.5092634338797,21.7626326086007,-11.5554525599604));
#48311=CARTESIAN_POINT('Ctrl Pts',(18.5970892183629,21.7673363311332,-11.5598390219729));
#48312=CARTESIAN_POINT('Ctrl Pts',(18.6849150028461,21.7720400536657,-11.5642254839854));
#48313=CARTESIAN_POINT('Ctrl Pts',(18.7728475188788,21.7722053239559,-11.568611945998));
#48314=CARTESIAN_POINT('Ctrl Pts',(18.8603867536229,21.7678782506229,-11.5729984080105));
#48315=CARTESIAN_POINT('Ctrl Pts',(18.9438873685616,21.7637508066803,-11.5771825007379));
#48316=CARTESIAN_POINT('Ctrl Pts',(19.0273409554121,21.7555210317051,-11.5813665934653));
#48317=CARTESIAN_POINT('Ctrl Pts',(19.1103117838489,21.7431906407963,-11.5855506861926));
#48318=CARTESIAN_POINT('Ctrl Pts',(19.1931709965624,21.7308768372295,-11.5897291503088));
#48319=CARTESIAN_POINT('Ctrl Pts',(19.2755482894351,21.7144734377188,-11.5939076144249));
#48320=CARTESIAN_POINT('Ctrl Pts',(19.3570101615098,21.6940340993743,-11.5980860785411));
#48321=CARTESIAN_POINT('Ctrl Pts',(19.4414693000141,21.6728427264754,-11.6024182829274));
#48322=CARTESIAN_POINT('Ctrl Pts',(19.5249438445757,21.6473126685892,-11.6067504873137));
#48323=CARTESIAN_POINT('Ctrl Pts',(19.6069591087771,21.6175623603811,-11.6110826917));
#48324=CARTESIAN_POINT('Ctrl Pts',(19.6859209478749,21.5889196549931,-11.6152536082852));
#48325=CARTESIAN_POINT('Ctrl Pts',(19.7635297647264,21.5563655402172,-11.6194245248703));
#48326=CARTESIAN_POINT('Ctrl Pts',(19.8393764665943,21.520056705042,-11.6235954414554));
#48327=CARTESIAN_POINT('Ctrl Pts',(19.9151926435138,21.4837624825697,-11.6277646794308));
#48328=CARTESIAN_POINT('Ctrl Pts',(19.9892477014193,21.4437167433873,-11.6319339174062));
#48329=CARTESIAN_POINT('Ctrl Pts',(20.0611538610254,21.4001237126223,-11.6361031553816));
#48330=CARTESIAN_POINT('Ctrl Pts',(20.1330612495339,21.3565299368366,-11.6402724646108));
#48331=CARTESIAN_POINT('Ctrl Pts',(20.2028192725658,21.3093889858049,-11.64444177384));
#48332=CARTESIAN_POINT('Ctrl Pts',(20.2700670841355,21.2589496851816,-11.6486110830691));
#48333=CARTESIAN_POINT('Ctrl Pts',(20.2779244358431,21.2530562692379,-11.6490982324384));
#48334=CARTESIAN_POINT('Ctrl Pts',(20.2857475522636,21.2471178717865,-11.6495853818077));
#48335=CARTESIAN_POINT('Ctrl Pts',(20.2935358855687,21.2411349269503,-11.650072531177));
#48336=CARTESIAN_POINT('Ctrl Pts',(20.2922820246457,21.2395345685083,-10.8502164908111));
#48337=CARTESIAN_POINT('Ctrl Pts',(20.7519191422662,20.8801556606603,-10.8791841187419));
#48338=CARTESIAN_POINT('Ctrl Pts',(21.5989576388621,19.6129801404785,-10.9505436822331));
#48339=CARTESIAN_POINT('Ctrl Pts',(20.9146849580311,17.1114988461662,-11.0642951812848));
#48340=CARTESIAN_POINT('Ctrl Pts',(18.1490151907075,16.2409688967909,-11.1914709879662));
#48341=CARTESIAN_POINT('Ctrl Pts',(16.3822353164858,17.7107520392007,-11.2922755723079));
#48342=CARTESIAN_POINT('Ctrl Pts',(16.1753926962513,18.8863578053553,-11.3506882210889));
#48343=CARTESIAN_POINT('Ctrl Pts',(16.1772046638934,19.209402892261,-11.3667089343096));
#48344=CARTESIAN_POINT('Origin',(18.734,19.211,1.76670989022852));
#48345=CARTESIAN_POINT('',(20.2935358855687,21.2411349269503,-10.0501312779792));
#48346=CARTESIAN_POINT('',(20.2935358855687,21.2411349269503,-10.1166694969415));
#48347=CARTESIAN_POINT('',(20.2935358855687,21.2411349269503,1.76670989022852));
#48348=CARTESIAN_POINT('',(16.1740004874608,19.2125798097913,-10.6332901097715));
#48349=CARTESIAN_POINT('Ctrl Pts',(20.2935358855687,21.2411349269503,-10.1166694969415));
#48350=CARTESIAN_POINT('Ctrl Pts',(20.3602256392546,21.1899043103582,-10.1208396570584));
#48351=CARTESIAN_POINT('Ctrl Pts',(20.4243735057776,21.1353955467902,-10.1250098171752));
#48352=CARTESIAN_POINT('Ctrl Pts',(20.485652031861,21.0778998792858,-10.1291799772921));
#48353=CARTESIAN_POINT('Ctrl Pts',(20.5469978512285,21.0203410726601,-10.1333547168887));
#48354=CARTESIAN_POINT('Ctrl Pts',(20.6054677052745,20.9597891308285,-10.1375294564853));
#48355=CARTESIAN_POINT('Ctrl Pts',(20.6607708292776,20.8965723572261,-10.1417041960819));
#48356=CARTESIAN_POINT('Ctrl Pts',(20.7161082312277,20.8333164006436,-10.1458815232629));
#48357=CARTESIAN_POINT('Ctrl Pts',(20.7682747110444,20.7673926852028,-10.150058850444));
#48358=CARTESIAN_POINT('Ctrl Pts',(20.817021149451,20.6991609089544,-10.154236177625));
#48359=CARTESIAN_POINT('Ctrl Pts',(20.8658480288831,20.6308165371147,-10.1584203982016));
#48360=CARTESIAN_POINT('Ctrl Pts',(20.9112433534327,20.5601568885703,-10.1626046187782));
#48361=CARTESIAN_POINT('Ctrl Pts',(20.953002718353,20.4875684219587,-10.1667888393548));
#48362=CARTESIAN_POINT('Ctrl Pts',(20.9725011688784,20.4536751233502,-10.1687425524454));
#48363=CARTESIAN_POINT('Ctrl Pts',(20.9912075871119,20.4193616240964,-10.170696265536));
#48364=CARTESIAN_POINT('Ctrl Pts',(21.0091047687182,20.3846687315233,-10.1726499786266));
#48365=CARTESIAN_POINT('Ctrl Pts',(21.0474385251168,20.310360445341,-10.1768346130196));
#48366=CARTESIAN_POINT('Ctrl Pts',(21.0821992629534,20.2340338438632,-10.1810192474127));
#48367=CARTESIAN_POINT('Ctrl Pts',(21.1131697431269,20.1560668406994,-10.1852038818057));
#48368=CARTESIAN_POINT('Ctrl Pts',(21.1440961406553,20.0782108139141,-10.1893825598897));
#48369=CARTESIAN_POINT('Ctrl Pts',(21.1712428282377,19.9987194471871,-10.1935612379736));
#48370=CARTESIAN_POINT('Ctrl Pts',(21.194438677507,19.9179947059402,-10.1977399160576));
#48371=CARTESIAN_POINT('Ctrl Pts',(21.218050295704,19.8358230317223,-10.201993493943));
#48372=CARTESIAN_POINT('Ctrl Pts',(21.2375678238504,19.75237376008,-10.2062470718284));
#48373=CARTESIAN_POINT('Ctrl Pts',(21.252862289631,19.668091638378,-10.2105006497139));
#48374=CARTESIAN_POINT('Ctrl Pts',(21.2678602423477,19.5854434900683,-10.2146717636918));
#48375=CARTESIAN_POINT('Ctrl Pts',(21.2787973301571,19.5019949698563,-10.2188428776698));
#48376=CARTESIAN_POINT('Ctrl Pts',(21.2856028472,19.4181784500402,-10.2230139916477));
#48377=CARTESIAN_POINT('Ctrl Pts',(21.2924060805859,19.3343900556667,-10.2271837059681));
#48378=CARTESIAN_POINT('Ctrl Pts',(21.2950804593957,19.2502343650762,-10.2313534202885));
#48379=CARTESIAN_POINT('Ctrl Pts',(21.2936070835643,19.1661493838665,-10.2355231346088));
#48380=CARTESIAN_POINT('Ctrl Pts',(21.2921337601619,19.0820673947614,-10.2396927005529));
#48381=CARTESIAN_POINT('Ctrl Pts',(21.2865129844866,18.9980565699817,-10.2438622664969));
#48382=CARTESIAN_POINT('Ctrl Pts',(21.2767779695197,18.9145540559809,-10.248031832441));
#48383=CARTESIAN_POINT('Ctrl Pts',(21.2667006834359,18.8281156965991,-10.2523479951799));
#48384=CARTESIAN_POINT('Ctrl Pts',(21.2522145228803,18.7422225813446,-10.2566641579188));
#48385=CARTESIAN_POINT('Ctrl Pts',(21.2334144574581,18.6573508603372,-10.2609803206577));
#48386=CARTESIAN_POINT('Ctrl Pts',(21.2152268021896,18.5752438267147,-10.2651558848494));
#48387=CARTESIAN_POINT('Ctrl Pts',(21.1930021468741,18.4940931072451,-10.2693314490411));
#48388=CARTESIAN_POINT('Ctrl Pts',(21.1668775008283,18.4143149518391,-10.2735070132328));
#48389=CARTESIAN_POINT('Ctrl Pts',(21.1394333610162,18.3305073914579,-10.2778934752453));
#48390=CARTESIAN_POINT('Ctrl Pts',(21.1076851096665,18.2482152402674,-10.2822799372578));
#48391=CARTESIAN_POINT('Ctrl Pts',(21.071848104157,18.1678958623945,-10.2866663992704));
#48392=CARTESIAN_POINT('Ctrl Pts',(21.0360110986474,18.0875764845216,-10.2910528612829));
#48393=CARTESIAN_POINT('Ctrl Pts',(20.9960856701952,18.0092303623902,-10.2954393232955));
#48394=CARTESIAN_POINT('Ctrl Pts',(20.9523407266399,17.9332815566288,-10.299825785308));
#48395=CARTESIAN_POINT('Ctrl Pts',(20.9106085527831,17.8608272680037,-10.3040104197011));
#48396=CARTESIAN_POINT('Ctrl Pts',(20.8652452879883,17.7902848467577,-10.3081950540941));
#48397=CARTESIAN_POINT('Ctrl Pts',(20.8164511103896,17.7220415140652,-10.3123796884872));
#48398=CARTESIAN_POINT('Ctrl Pts',(20.7677263852631,17.6538953173098,-10.3165583665711));
#48399=CARTESIAN_POINT('Ctrl Pts',(20.7155807127379,17.5880420799731,-10.3207370446551));
#48400=CARTESIAN_POINT('Ctrl Pts',(20.6602594535819,17.5248432701892,-10.324915722739));
#48401=CARTESIAN_POINT('Ctrl Pts',(20.6039466006143,17.4605116671601,-10.3291693006244));
#48402=CARTESIAN_POINT('Ctrl Pts',(20.5443434371031,17.3989310067054,-10.3334228785099));
#48403=CARTESIAN_POINT('Ctrl Pts',(20.4817541149312,17.3404504674452,-10.3376764563953));
#48404=CARTESIAN_POINT('Ctrl Pts',(20.4203782089026,17.2831036875539,-10.3418475703733));
#48405=CARTESIAN_POINT('Ctrl Pts',(20.3561312476119,17.2287382262735,-10.3460186843512));
#48406=CARTESIAN_POINT('Ctrl Pts',(20.2893385159968,17.1776475709664,-10.3501897983292));
#48407=CARTESIAN_POINT('Ctrl Pts',(20.2225681973279,17.1265740596221,-10.3543595126496));
#48408=CARTESIAN_POINT('Ctrl Pts',(20.1532541699942,17.078773451095,-10.3585292269699));
#48409=CARTESIAN_POINT('Ctrl Pts',(20.0817544971409,17.0344987214715,-10.3626989412903));
#48410=CARTESIAN_POINT('Ctrl Pts',(20.0102573685527,16.9902255673327,-10.3668685072343));
#48411=CARTESIAN_POINT('Ctrl Pts',(19.9365751406475,16.9494782841066,-10.3710380731784));
#48412=CARTESIAN_POINT('Ctrl Pts',(19.8610933619694,16.912465564016,-10.3752076391224));
#48413=CARTESIAN_POINT('Ctrl Pts',(19.78295773707,16.8741515223472,-10.3795238018614));
#48414=CARTESIAN_POINT('Ctrl Pts',(19.7028941360643,16.8398397766944,-10.3838399646003));
#48415=CARTESIAN_POINT('Ctrl Pts',(19.6213543310965,16.8097082036778,-10.3881561273392));
#48416=CARTESIAN_POINT('Ctrl Pts',(19.5424706766991,16.780558163483,-10.3923316915309));
#48417=CARTESIAN_POINT('Ctrl Pts',(19.4622059796066,16.7553202361716,-10.3965072557226));
#48418=CARTESIAN_POINT('Ctrl Pts',(19.3809844006654,16.7341045267723,-10.4006828199142));
#48419=CARTESIAN_POINT('Ctrl Pts',(19.2956605128579,16.7118172623269,-10.4050692819268));
#48420=CARTESIAN_POINT('Ctrl Pts',(19.2092811104196,16.693969336797,-10.4094557439393));
#48421=CARTESIAN_POINT('Ctrl Pts',(19.122347333066,16.6806272312364,-10.4138422059519));
#48422=CARTESIAN_POINT('Ctrl Pts',(19.0354135557124,16.6672851256757,-10.4182286679644));
#48423=CARTESIAN_POINT('Ctrl Pts',(18.9479259883671,16.65844882271,-10.4226151299769));
#48424=CARTESIAN_POINT('Ctrl Pts',(18.8603867536229,16.6541217493771,-10.4270015919895));
#48425=CARTESIAN_POINT('Ctrl Pts',(18.7768753288335,16.6499937711024,-10.4311862263825));
#48426=CARTESIAN_POINT('Ctrl Pts',(18.6930060412947,16.6499538232249,-10.4353708607756));
#48427=CARTESIAN_POINT('Ctrl Pts',(18.6092128353623,16.6540431830902,-10.4395554951686));
#48428=CARTESIAN_POINT('Ctrl Pts',(18.5255388986872,16.6581267222578,-10.4437341732526));
#48429=CARTESIAN_POINT('Ctrl Pts',(18.441941284071,16.6663278722549,-10.4479128513365));
#48430=CARTESIAN_POINT('Ctrl Pts',(18.3588567381408,16.6786359793502,-10.4520915294204));
#48431=CARTESIAN_POINT('Ctrl Pts',(18.2742829614366,16.6911647004195,-10.4563451073059));
#48432=CARTESIAN_POINT('Ctrl Pts',(18.1902413093998,16.7079490849927,-10.4605986851913));
#48433=CARTESIAN_POINT('Ctrl Pts',(18.1071900176367,16.7289223932339,-10.4648522630768));
#48434=CARTESIAN_POINT('Ctrl Pts',(18.0257488372257,16.7494890929688,-10.4690233770547));
#48435=CARTESIAN_POINT('Ctrl Pts',(17.945260426203,16.7740836270436,-10.4731944910327));
#48436=CARTESIAN_POINT('Ctrl Pts',(17.8661476315623,16.8025913414461,-10.4773656050106));
#48437=CARTESIAN_POINT('Ctrl Pts',(17.7870613839839,16.8310894898098,-10.481535319331));
#48438=CARTESIAN_POINT('Ctrl Pts',(17.7093502684716,16.8634980548293,-10.4857050336514));
#48439=CARTESIAN_POINT('Ctrl Pts',(17.633420810669,16.8996528932219,-10.4898747479717));
#48440=CARTESIAN_POINT('Ctrl Pts',(17.5574940547624,16.9358064450701,-10.4940443139158));
#48441=CARTESIAN_POINT('Ctrl Pts',(17.4833492454956,16.975705806696,-10.4982138798598));
#48442=CARTESIAN_POINT('Ctrl Pts',(17.4113705501161,17.0191397539305,-10.5023834458039));
#48443=CARTESIAN_POINT('Ctrl Pts',(17.3368611726025,17.0641007851681,-10.5066996085428));
#48444=CARTESIAN_POINT('Ctrl Pts',(17.2646735157618,17.1128493061263,-10.5110157712817));
#48445=CARTESIAN_POINT('Ctrl Pts',(17.1952016813754,17.1651017291669,-10.5153319340206));
#48446=CARTESIAN_POINT('Ctrl Pts',(17.1279928846869,17.2156520350229,-10.5195074982123));
#48447=CARTESIAN_POINT('Ctrl Pts',(17.0633260236108,17.2694811317355,-10.523683062404));
#48448=CARTESIAN_POINT('Ctrl Pts',(17.001523269273,17.3262919649215,-10.5278586265957));
#48449=CARTESIAN_POINT('Ctrl Pts',(16.9365990047358,17.3859721782367,-10.5322450886082));
#48450=CARTESIAN_POINT('Ctrl Pts',(16.8748361916357,17.4489428422738,-10.5366315506207));
#48451=CARTESIAN_POINT('Ctrl Pts',(16.8165619874411,17.5148185627727,-10.5410180126333));
#48452=CARTESIAN_POINT('Ctrl Pts',(16.7582877832466,17.5806942832717,-10.5454044746458));
#48453=CARTESIAN_POINT('Ctrl Pts',(16.7035024899566,17.6494745589998,-10.5497909366584));
#48454=CARTESIAN_POINT('Ctrl Pts',(16.6524807786037,17.7207390393097,-10.5541773986709));
#48455=CARTESIAN_POINT('Ctrl Pts',(16.6033728384837,17.789330463214,-10.5583993290636));
#48456=CARTESIAN_POINT('Ctrl Pts',(16.5575691753499,17.8604769154311,-10.5626212594564));
#48457=CARTESIAN_POINT('Ctrl Pts',(16.5153433201941,17.9338302629828,-10.5668431898491));
#48458=CARTESIAN_POINT('Ctrl Pts',(16.4731798646834,18.0070752119517,-10.5710588812454));
#48459=CARTESIAN_POINT('Ctrl Pts',(16.4345839361663,18.082520192057,-10.5752745726418));
#48460=CARTESIAN_POINT('Ctrl Pts',(16.3997870211447,18.1597865253224,-10.5794902640381));
#48461=CARTESIAN_POINT('Ctrl Pts',(16.3650317212893,18.2369604523703,-10.5837009137031));
#48462=CARTESIAN_POINT('Ctrl Pts',(16.3340665899183,18.3159509969196,-10.587911563368));
#48463=CARTESIAN_POINT('Ctrl Pts',(16.3070776023613,18.3963542635971,-10.592122213033));
#48464=CARTESIAN_POINT('Ctrl Pts',(16.2801155537106,18.4766772762055,-10.5963286598617));
#48465=CARTESIAN_POINT('Ctrl Pts',(16.2571218975382,18.5584097818784,-10.6005351066903));
#48466=CARTESIAN_POINT('Ctrl Pts',(16.238234292144,18.6411284956326,-10.604741553519));
#48467=CARTESIAN_POINT('Ctrl Pts',(16.2193575415099,18.7237996707085,-10.6089455828908));
#48468=CARTESIAN_POINT('Ctrl Pts',(16.2045822501751,18.807455489948,-10.6131496122625));
#48469=CARTESIAN_POINT('Ctrl Pts',(16.19399578679,18.8916591211959,-10.6173536416343));
#48470=CARTESIAN_POINT('Ctrl Pts',(16.1834116610726,18.975844158877,-10.6215567426863));
#48471=CARTESIAN_POINT('Ctrl Pts',(16.1770145819501,19.0605763228053,-10.6257598437382));
#48472=CARTESIAN_POINT('Ctrl Pts',(16.1748403468596,19.145411359684,-10.6299629447902));
#48473=CARTESIAN_POINT('Ctrl Pts',(16.1742666403856,19.1677964320708,-10.631071999784));
#48474=CARTESIAN_POINT('Ctrl Pts',(16.1739866695752,19.1901886456578,-10.6321810547777));
#48475=CARTESIAN_POINT('Ctrl Pts',(16.1740004874608,19.2125798097913,-10.6332901097715));
#48476=CARTESIAN_POINT('Ctrl Pts',(16.1772048569635,19.2125971087803,-10.6332910657481));
#48477=CARTESIAN_POINT('Ctrl Pts',(16.1753928896008,19.5356421709025,-10.6493117789495));
#48478=CARTESIAN_POINT('Ctrl Pts',(16.3822354944161,20.7112478477878,-10.7077244277114));
#48479=CARTESIAN_POINT('Ctrl Pts',(18.0373629477008,22.0881474066249,-10.8021586297274));
#48480=CARTESIAN_POINT('Ctrl Pts',(19.7177437291103,21.6776339477978,-10.8805721185419));
#48481=CARTESIAN_POINT('Ctrl Pts',(20.2948050584429,21.242816933186,-10.916593671796));
#48482=CARTESIAN_POINT('',(16.1739802642219,19.2096989559289,-10.5667098967469));
#48483=CARTESIAN_POINT('Ctrl Pts',(16.1705863812103,19.2097193146384,-10.566710999223));
#48484=CARTESIAN_POINT('Ctrl Pts',(16.1754041849044,19.9846332056276,-10.6053965865622));
#48485=CARTESIAN_POINT('Ctrl Pts',(16.9631830908079,21.6171665575917,-10.6864741094618));
#48486=CARTESIAN_POINT('Ctrl Pts',(19.0902280311167,21.9601261297055,-10.7809759399911));
#48487=CARTESIAN_POINT('Ctrl Pts',(20.0792749368812,21.4060795485156,-10.8367921831814));
#48488=CARTESIAN_POINT('Ctrl Pts',(20.2922820246457,21.2395345685083,-10.8502164908111));
#48489=CARTESIAN_POINT('Ctrl Pts',(20.2935358855687,21.2411349269503,-10.0501312779792));
#48490=CARTESIAN_POINT('Ctrl Pts',(20.3598784985668,21.1901709814807,-10.0543142410822));
#48491=CARTESIAN_POINT('Ctrl Pts',(20.4238373144014,21.1358617299933,-10.0584972041852));
#48492=CARTESIAN_POINT('Ctrl Pts',(20.4850560901097,21.0784588534395,-10.0626801672881));
#48493=CARTESIAN_POINT('Ctrl Pts',(20.5461929654509,21.0211327722253,-10.066857534294));
#48494=CARTESIAN_POINT('Ctrl Pts',(20.6045967494064,20.9607215996642,-10.0710349012998));
#48495=CARTESIAN_POINT('Ctrl Pts',(20.6599429808172,20.8975181987281,-10.0752122683057));
#48496=CARTESIAN_POINT('Ctrl Pts',(20.7152315969333,20.8343805923813,-10.0793852866824));
#48497=CARTESIAN_POINT('Ctrl Pts',(20.7674686848818,20.7684568792845,-10.0835583050592));
#48498=CARTESIAN_POINT('Ctrl Pts',(20.8163664780353,20.7000768452819,-10.087731323436));
#48499=CARTESIAN_POINT('Ctrl Pts',(20.8652367012063,20.6317353659098,-10.091901988945));
#48500=CARTESIAN_POINT('Ctrl Pts',(20.9107711007099,20.5609406886882,-10.0960726544539));
#48501=CARTESIAN_POINT('Ctrl Pts',(20.9527227999439,20.4880548684411,-10.1002433199629));
#48502=CARTESIAN_POINT('Ctrl Pts',(20.9946634302466,20.4151882790751,-10.1044128850442));
#48503=CARTESIAN_POINT('Ctrl Pts',(21.0330230085846,20.3402320411324,-10.1085824501255));
#48504=CARTESIAN_POINT('Ctrl Pts',(21.0675992698966,20.2635751505417,-10.1127520152067));
#48505=CARTESIAN_POINT('Ctrl Pts',(21.1021767802658,20.1869154907437,-10.1169217309123));
#48506=CARTESIAN_POINT('Ctrl Pts',(21.1329705142616,20.1085554762028,-10.1210914466179));
#48507=CARTESIAN_POINT('Ctrl Pts',(21.1598258280554,20.0289052829879,-10.1252611623235));
#48508=CARTESIAN_POINT('Ctrl Pts',(21.186708599274,19.9491736537782,-10.1294351412322));
#48509=CARTESIAN_POINT('Ctrl Pts',(21.2096447603305,19.8681496481244,-10.1336091201408));
#48510=CARTESIAN_POINT('Ctrl Pts',(21.2285293380277,19.7862594038511,-10.1377830990495));
#48511=CARTESIAN_POINT('Ctrl Pts',(21.2474234553482,19.7043277923787,-10.141959186461));
#48512=CARTESIAN_POINT('Ctrl Pts',(21.2622618315702,19.6215295239771,-10.1461352738725));
#48513=CARTESIAN_POINT('Ctrl Pts',(21.2729909701164,19.5382993334354,-10.150311361284));
#48514=CARTESIAN_POINT('Ctrl Pts',(21.2837392233131,19.4549208629554,-10.1544948886639));
#48515=CARTESIAN_POINT('Ctrl Pts',(21.2903635757193,19.3711093924122,-10.1586784160438));
#48516=CARTESIAN_POINT('Ctrl Pts',(21.2928626077066,19.2873030463401,-10.1628619434237));
#48517=CARTESIAN_POINT('Ctrl Pts',(21.2950932320049,19.2124978926481,-10.166596140454));
#48518=CARTESIAN_POINT('Ctrl Pts',(21.2940378520455,19.1376970537945,-10.1703303374844));
#48519=CARTESIAN_POINT('Ctrl Pts',(21.2897303495757,19.0632083214199,-10.1740645345147));
#48520=CARTESIAN_POINT('Ctrl Pts',(21.2849032547982,18.9797343887762,-10.1782491689078));
#48521=CARTESIAN_POINT('Ctrl Pts',(21.2759733033623,18.8963418534062,-10.1824338033008));
#48522=CARTESIAN_POINT('Ctrl Pts',(21.262945864237,18.8134665853561,-10.1866184376939));
#48523=CARTESIAN_POINT('Ctrl Pts',(21.2499369680589,18.7307092799923,-10.1907971157778));
#48524=CARTESIAN_POINT('Ctrl Pts',(21.2328422397339,18.6484682300579,-10.1949757938618));
#48525=CARTESIAN_POINT('Ctrl Pts',(21.2117189811603,18.5671765378629,-10.1991544719457));
#48526=CARTESIAN_POINT('Ctrl Pts',(21.1902171033576,18.4844277505086,-10.2034080498311));
#48527=CARTESIAN_POINT('Ctrl Pts',(21.1645408797953,18.4026631714651,-10.2076616277166));
#48528=CARTESIAN_POINT('Ctrl Pts',(21.1348056750071,18.3223312704649,-10.211915205602));
#48529=CARTESIAN_POINT('Ctrl Pts',(21.1056469451872,18.2435567601204,-10.21608631958));
#48530=CARTESIAN_POINT('Ctrl Pts',(21.0725853792787,18.1661603243174,-10.2202574335579));
#48531=CARTESIAN_POINT('Ctrl Pts',(21.0357801964354,18.0905501228087,-10.2244285475359));
#48532=CARTESIAN_POINT('Ctrl Pts',(20.9989873639266,18.0149652930333,-10.2285982618562));
#48533=CARTESIAN_POINT('Ctrl Pts',(20.9584536105076,17.9411659204442,-10.2327679761766));
#48534=CARTESIAN_POINT('Ctrl Pts',(20.9143856152223,17.8695386442646,-10.236937690497));
#48535=CARTESIAN_POINT('Ctrl Pts',(20.8703191880655,17.7979139168908,-10.241107256441));
#48536=CARTESIAN_POINT('Ctrl Pts',(20.8227190108795,17.7284615236186,-10.2452768223851));
#48537=CARTESIAN_POINT('Ctrl Pts',(20.7718361823765,17.6615408382932,-10.2494463883291));
#48538=CARTESIAN_POINT('Ctrl Pts',(20.719164376394,17.5922673042273,-10.2537625510681));
#48539=CARTESIAN_POINT('Ctrl Pts',(20.6629751073579,17.5257072400677,-10.258078713807));
#48540=CARTESIAN_POINT('Ctrl Pts',(20.6035924848956,17.462222158071,-10.2623948765459));
#48541=CARTESIAN_POINT('Ctrl Pts',(20.546144245114,17.4008050959428,-10.2665704407376));
#48542=CARTESIAN_POINT('Ctrl Pts',(20.4857078751411,17.3422660512048,-10.2707460049293));
#48543=CARTESIAN_POINT('Ctrl Pts',(20.4226131812576,17.2868935777657,-10.2749215691209));
#48544=CARTESIAN_POINT('Ctrl Pts',(20.3563317243794,17.2287243723288,-10.2793080311335));
#48545=CARTESIAN_POINT('Ctrl Pts',(20.2871168004273,17.1740503939331,-10.283694493146));
#48546=CARTESIAN_POINT('Ctrl Pts',(20.2153865821741,17.1231557064392,-10.2880809551586));
#48547=CARTESIAN_POINT('Ctrl Pts',(20.1436563639208,17.0722610189452,-10.2924674171711));
#48548=CARTESIAN_POINT('Ctrl Pts',(20.0694113820225,17.0251458690141,-10.2968538791836));
#48549=CARTESIAN_POINT('Ctrl Pts',(19.9930989518198,16.9820383965787,-10.3012403411962));
#48550=CARTESIAN_POINT('Ctrl Pts',(19.9202977696528,16.9409143628506,-10.3054249755892));
#48551=CARTESIAN_POINT('Ctrl Pts',(19.8453442312191,16.9032842410815,-10.3096096099823));
#48552=CARTESIAN_POINT('Ctrl Pts',(19.7686077403709,16.8693794450073,-10.3137942443753));
#48553=CARTESIAN_POINT('Ctrl Pts',(19.6919804744194,16.8355229082136,-10.3179729224593));
#48554=CARTESIAN_POINT('Ctrl Pts',(19.6135757141379,16.8053813489309,-10.3221516005432));
#48555=CARTESIAN_POINT('Ctrl Pts',(19.5337886464594,16.7791410153969,-10.3263302786272));
#48556=CARTESIAN_POINT('Ctrl Pts',(19.4525714529348,16.752430342743,-10.3305838565126));
#48557=CARTESIAN_POINT('Ctrl Pts',(19.3699223286582,16.7297623675601,-10.334837434398));
#48558=CARTESIAN_POINT('Ctrl Pts',(19.2862808103369,16.7112828346924,-10.3390910122835));
#48559=CARTESIAN_POINT('Ctrl Pts',(19.2042608460612,16.6931615636291,-10.3432621262614));
#48560=CARTESIAN_POINT('Ctrl Pts',(19.1212870932384,16.6790678856914,-10.3474332402394));
#48561=CARTESIAN_POINT('Ctrl Pts',(19.0377889319358,16.6690888519003,-10.3516043542173));
#48562=CARTESIAN_POINT('Ctrl Pts',(18.9543187892476,16.6591131666705,-10.3557740685377));
#48563=CARTESIAN_POINT('Ctrl Pts',(18.8703250439618,16.6532494380237,-10.3599437828581));
#48564=CARTESIAN_POINT('Ctrl Pts',(18.7862446699247,16.6515331620698,-10.3641134971784));
#48565=CARTESIAN_POINT('Ctrl Pts',(18.7021672878281,16.6498169471884,-10.3682830631225));
#48566=CARTESIAN_POINT('Ctrl Pts',(18.6180037430638,16.652247900101,-10.3724526290665));
#48567=CARTESIAN_POINT('Ctrl Pts',(18.5341921271337,16.6588094087744,-10.3766221950106));
#48568=CARTESIAN_POINT('Ctrl Pts',(18.4474337981803,16.6656016119982,-10.3809383577495));
#48569=CARTESIAN_POINT('Ctrl Pts',(18.361053131965,16.6768201947949,-10.3852545204884));
#48570=CARTESIAN_POINT('Ctrl Pts',(18.2755295374795,16.6923883119869,-10.3895706832273));
#48571=CARTESIAN_POINT('Ctrl Pts',(18.1927918650888,16.7074492993989,-10.393746247419));
#48572=CARTESIAN_POINT('Ctrl Pts',(18.1108567316689,16.7265806476473,-10.3979218116107));
#48573=CARTESIAN_POINT('Ctrl Pts',(18.030145283277,16.749661230601,-10.4020973758024));
#48574=CARTESIAN_POINT('Ctrl Pts',(17.9453572914999,16.7739075589308,-10.4064838378149));
#48575=CARTESIAN_POINT('Ctrl Pts',(17.8619204024433,16.8025123689437,-10.4108702998274));
#48576=CARTESIAN_POINT('Ctrl Pts',(17.7802998178505,16.8352778018952,-10.41525676184));
#48577=CARTESIAN_POINT('Ctrl Pts',(17.6986792332576,16.8680432348467,-10.4196432238525));
#48578=CARTESIAN_POINT('Ctrl Pts',(17.6188754477656,16.9049689780518,-10.4240296858651));
#48579=CARTESIAN_POINT('Ctrl Pts',(17.5413224142637,16.9458023979171,-10.4284161478776));
#48580=CARTESIAN_POINT('Ctrl Pts',(17.4673377107945,16.9847570116046,-10.4326007822707));
#48581=CARTESIAN_POINT('Ctrl Pts',(17.3951258047347,17.0274126045708,-10.4367854166637));
#48582=CARTESIAN_POINT('Ctrl Pts',(17.3250812297131,17.0735838265015,-10.4409700510568));
#48583=CARTESIAN_POINT('Ctrl Pts',(17.2551363544742,17.1196893294125,-10.4451487291407));
#48584=CARTESIAN_POINT('Ctrl Pts',(17.1873530634461,17.1693002706272,-10.4493274072246));
#48585=CARTESIAN_POINT('Ctrl Pts',(17.1221018691139,17.2221851731129,-10.4535060853086));
#48586=CARTESIAN_POINT('Ctrl Pts',(17.0556810940185,17.276017999468,-10.457759663194));
#48587=CARTESIAN_POINT('Ctrl Pts',(16.9918845107683,17.3332430884428,-10.4620132410795));
#48588=CARTESIAN_POINT('Ctrl Pts',(16.9310725805955,17.3935697481445,-10.4662668189649));
#48589=CARTESIAN_POINT('Ctrl Pts',(16.8714396083539,17.4527268578301,-10.4704379329429));
#48590=CARTESIAN_POINT('Ctrl Pts',(16.8146769368999,17.5148660125131,-10.4746090469208));
#48591=CARTESIAN_POINT('Ctrl Pts',(16.7610901776527,17.5796732905743,-10.4787801608988));
#48592=CARTESIAN_POINT('Ctrl Pts',(16.7075213999602,17.6444588219275,-10.4829498752191));
#48593=CARTESIAN_POINT('Ctrl Pts',(16.6571267108676,17.7119103443124,-10.4871195895395));
#48594=CARTESIAN_POINT('Ctrl Pts',(16.610172482641,17.7816796452478,-10.4912893038599));
#48595=CARTESIAN_POINT('Ctrl Pts',(16.5632199252474,17.8514464634922,-10.4954588698039));
#48596=CARTESIAN_POINT('Ctrl Pts',(16.5197078414472,17.9235305141742,-10.499628435748));
#48597=CARTESIAN_POINT('Ctrl Pts',(16.4798593937703,17.9975544398918,-10.503798001692));
#48598=CARTESIAN_POINT('Ctrl Pts',(16.4386099238315,18.0741809555191,-10.5081141644309));
#48599=CARTESIAN_POINT('Ctrl Pts',(16.4012867603008,18.1528858318599,-10.5124303271698));
#48600=CARTESIAN_POINT('Ctrl Pts',(16.3680847835396,18.2332243669834,-10.5167464899088));
#48601=CARTESIAN_POINT('Ctrl Pts',(16.3359643576791,18.3109458827753,-10.5209220541004));
#48602=CARTESIAN_POINT('Ctrl Pts',(16.3077008602571,18.3901957994176,-10.5250976182921));
#48603=CARTESIAN_POINT('Ctrl Pts',(16.2834204017388,18.4705544364466,-10.5292731824838));
#48604=CARTESIAN_POINT('Ctrl Pts',(16.2579135949821,18.5549717971974,-10.5336596444963));
#48605=CARTESIAN_POINT('Ctrl Pts',(16.236802907853,18.6406122578469,-10.5380461065089));
#48606=CARTESIAN_POINT('Ctrl Pts',(16.2201737773398,18.726977560163,-10.5424325685214));
#48607=CARTESIAN_POINT('Ctrl Pts',(16.2035446468265,18.8133428624791,-10.546819030534));
#48608=CARTESIAN_POINT('Ctrl Pts',(16.1913970777482,18.9004324212999,-10.5512054925465));
#48609=CARTESIAN_POINT('Ctrl Pts',(16.1837535357011,18.9877446051473,-10.555591954559));
#48610=CARTESIAN_POINT('Ctrl Pts',(16.1772957565522,19.0615118189368,-10.5592979331155));
#48611=CARTESIAN_POINT('Ctrl Pts',(16.174038011382,19.1355632322755,-10.563003911672));
#48612=CARTESIAN_POINT('Ctrl Pts',(16.1740003306697,19.2096988355574,-10.5667098902285));
#48613=CARTESIAN_POINT('Origin',(18.734,19.211,1.76670989022852));
#48614=CARTESIAN_POINT('',(20.2935358855687,21.2411349269503,-9.25004024781016));
#48615=CARTESIAN_POINT('',(20.2929505577762,21.2403915309055,-9.31680761603243));
#48616=CARTESIAN_POINT('',(20.2935358855687,21.2411349269503,1.76670989022852));
#48617=CARTESIAN_POINT('',(16.1740007840082,19.2089964727374,-9.83329010977151));
#48618=CARTESIAN_POINT('Ctrl Pts',(20.2929505577765,21.2403915309053,-9.31680761603245));
#48619=CARTESIAN_POINT('Ctrl Pts',(20.7827497205508,20.8565253562616,-9.34773679020097));
#48620=CARTESIAN_POINT('Ctrl Pts',(21.628276822644,19.5224825845314,-9.42105789992997));
#48621=CARTESIAN_POINT('Ctrl Pts',(20.8151679973455,17.0128120271405,-9.53677094521944));
#48622=CARTESIAN_POINT('Ctrl Pts',(18.012168550104,16.271229608432,-9.66394675190087));
#48623=CARTESIAN_POINT('Ctrl Pts',(16.3483940920526,17.7909994706266,-9.76278617059815));
#48624=CARTESIAN_POINT('Ctrl Pts',(16.1742904286681,18.9257985710608,-9.81923365373494));
#48625=CARTESIAN_POINT('Ctrl Pts',(16.1763511750307,19.2089800092947,-9.83328920131125));
#48626=CARTESIAN_POINT('Ctrl Pts',(16.1740007840082,19.2089964727374,-9.83329010977151));
#48627=CARTESIAN_POINT('Ctrl Pts',(16.1739350379054,19.2930033015151,-9.83745593779553));
#48628=CARTESIAN_POINT('Ctrl Pts',(16.1780086491546,19.3770604200798,-9.84162176581954));
#48629=CARTESIAN_POINT('Ctrl Pts',(16.186209790272,19.4607299485725,-9.84578759384356));
#48630=CARTESIAN_POINT('Ctrl Pts',(16.1944094741073,19.544384609609,-9.84995268163076));
#48631=CARTESIAN_POINT('Ctrl Pts',(16.2067351859308,19.6276513592373,-9.85411776941796));
#48632=CARTESIAN_POINT('Ctrl Pts',(16.2231231591268,19.7100966739689,-9.85828285720516));
#48633=CARTESIAN_POINT('Ctrl Pts',(16.2395131466373,19.7925521223991,-9.86244845694073));
#48634=CARTESIAN_POINT('Ctrl Pts',(16.2599662961795,19.8741854840192,-9.8666140566763));
#48635=CARTESIAN_POINT('Ctrl Pts',(16.2843678510517,19.9545740278134,-9.87077965641186));
#48636=CARTESIAN_POINT('Ctrl Pts',(16.3087969918046,20.035053450603,-9.87494996534479));
#48637=CARTESIAN_POINT('Ctrl Pts',(16.3371833165997,20.1142848040861,-9.87912027427772));
#48638=CARTESIAN_POINT('Ctrl Pts',(16.3693624790257,20.191861557204,-9.88329058321065));
#48639=CARTESIAN_POINT('Ctrl Pts',(16.4015603628986,20.2694834435371,-9.88746331837879));
#48640=CARTESIAN_POINT('Ctrl Pts',(16.437555280145,20.3454483968708,-9.89163605354694));
#48641=CARTESIAN_POINT('Ctrl Pts',(16.4771361744286,20.4193731513184,-9.89580878871509));
#48642=CARTESIAN_POINT('Ctrl Pts',(16.5167895617082,20.4934333000524,-9.8999891663097));
#48643=CARTESIAN_POINT('Ctrl Pts',(16.5600418069655,20.5654453913553,-9.90416954390431));
#48644=CARTESIAN_POINT('Ctrl Pts',(16.6066377495773,20.6350540212634,-9.90834992149893));
#48645=CARTESIAN_POINT('Ctrl Pts',(16.6436006876733,20.6902721225405,-9.91166606942054));
#48646=CARTESIAN_POINT('Ctrl Pts',(16.6826668124624,20.7439783287842,-9.91498221734214));
#48647=CARTESIAN_POINT('Ctrl Pts',(16.7236914224215,20.7960108589263,-9.91829836526375));
#48648=CARTESIAN_POINT('Ctrl Pts',(16.7754602209958,20.8616705099242,-9.9224829996568));
#48649=CARTESIAN_POINT('Ctrl Pts',(16.8305455538229,20.924913415419,-9.92666763404985));
#48650=CARTESIAN_POINT('Ctrl Pts',(16.8886933634204,20.9853853631597,-9.93085226844291));
#48651=CARTESIAN_POINT('Ctrl Pts',(16.9467584068082,21.0457712365676,-9.93503094652685));
#48652=CARTESIAN_POINT('Ctrl Pts',(17.0078769523777,21.1033936577097,-9.9392096246108));
#48653=CARTESIAN_POINT('Ctrl Pts',(17.07175395795,21.157930429083,-9.94338830269474));
#48654=CARTESIAN_POINT('Ctrl Pts',(17.1367759129396,21.2134447328882,-9.94764188058018));
#48655=CARTESIAN_POINT('Ctrl Pts',(17.2046558928942,21.2657612997092,-9.95189545846561));
#48656=CARTESIAN_POINT('Ctrl Pts',(17.2750424589418,21.314578592159,-9.95614903635105));
#48657=CARTESIAN_POINT('Ctrl Pts',(17.3440644440585,21.3624494661354,-9.960320150329));
#48658=CARTESIAN_POINT('Ctrl Pts',(17.4154962970282,21.406955261226,-9.96449126430695));
#48659=CARTESIAN_POINT('Ctrl Pts',(17.4889737195064,21.4478526015096,-9.9686623782849));
#48660=CARTESIAN_POINT('Ctrl Pts',(17.5624264859259,21.4887362182957,-9.97283209260528));
#48661=CARTESIAN_POINT('Ctrl Pts',(17.6379230570028,21.5260135615005,-9.97700180692565));
#48662=CARTESIAN_POINT('Ctrl Pts',(17.7150725574696,21.5594860797668,-9.98117152124602));
#48663=CARTESIAN_POINT('Ctrl Pts',(17.7922193126263,21.5929574069373,-9.98534108719007));
#48664=CARTESIAN_POINT('Ctrl Pts',(17.871018457864,21.6226239960436,-9.98951065313412));
#48665=CARTESIAN_POINT('Ctrl Pts',(17.9510583236147,21.6483350880375,-9.99368021907817));
#48666=CARTESIAN_POINT('Ctrl Pts',(18.0339122923051,21.6749501503078,-9.99799638181709));
#48667=CARTESIAN_POINT('Ctrl Pts',(18.118095350145,21.6973262283485,-10.002312544556));
#48668=CARTESIAN_POINT('Ctrl Pts',(18.2031347548814,21.7153526292288,-10.0066287072949));
#48669=CARTESIAN_POINT('Ctrl Pts',(18.2854040099532,21.7327918219965,-10.0108042714866));
#48670=CARTESIAN_POINT('Ctrl Pts',(18.3684742051326,21.7461603390116,-10.0149798356783));
#48671=CARTESIAN_POINT('Ctrl Pts',(18.4519097174451,21.7554105550182,-10.01915539987));
#48672=CARTESIAN_POINT('Ctrl Pts',(18.5395593591353,21.765127977445,-10.0235418618825));
#48673=CARTESIAN_POINT('Ctrl Pts',(18.6276116092813,21.7703001003685,-10.027928323895));
#48674=CARTESIAN_POINT('Ctrl Pts',(18.7155609817199,21.7709335933975,-10.0323147859076));
#48675=CARTESIAN_POINT('Ctrl Pts',(18.8035103541584,21.7715670864265,-10.0367012479201));
#48676=CARTESIAN_POINT('Ctrl Pts',(18.891356272623,21.767662051318,-10.0410877099327));
#48677=CARTESIAN_POINT('Ctrl Pts',(18.9786013944248,21.7592876913421,-10.0454741719452));
#48678=CARTESIAN_POINT('Ctrl Pts',(19.0618259169023,21.7512992549039,-10.0496584884871));
#48679=CARTESIAN_POINT('Ctrl Pts',(19.14481355195,21.7392146225067,-10.0538428050291));
#48680=CARTESIAN_POINT('Ctrl Pts',(19.2271290458152,21.7230556809461,-10.058027121571));
#48681=CARTESIAN_POINT('Ctrl Pts',(19.3093328037827,21.7069186736988,-10.0622057582787));
#48682=CARTESIAN_POINT('Ctrl Pts',(19.3908657848194,21.6867184269618,-10.0663843949863));
#48683=CARTESIAN_POINT('Ctrl Pts',(19.4712973833544,21.6625286187395,-10.070563031694));
#48684=CARTESIAN_POINT('Ctrl Pts',(19.5516353626659,21.6383669665044,-10.0747368046325));
#48685=CARTESIAN_POINT('Ctrl Pts',(19.6308740694803,21.6102251148652,-10.0789105775711));
#48686=CARTESIAN_POINT('Ctrl Pts',(19.708594110491,21.578227559783,-10.0830843505096));
#48687=CARTESIAN_POINT('Ctrl Pts',(19.786260803981,21.5462519680221,-10.0872552585444));
#48688=CARTESIAN_POINT('Ctrl Pts',(19.8624104781162,21.5104261042933,-10.0914261665791));
#48689=CARTESIAN_POINT('Ctrl Pts',(19.9366409846833,21.4709235964873,-10.0955970746139));
#48690=CARTESIAN_POINT('Ctrl Pts',(20.0108540887569,21.4314303495925,-10.099767004827));
#48691=CARTESIAN_POINT('Ctrl Pts',(20.08314850986,21.3882623802746,-10.1039369350401));
#48692=CARTESIAN_POINT('Ctrl Pts',(20.1531451666036,21.3416400437675,-10.1081068652532));
#48693=CARTESIAN_POINT('Ctrl Pts',(20.2010560876092,21.3097282470417,-10.1109610758159));
#48694=CARTESIAN_POINT('Ctrl Pts',(20.2478909716886,21.276199040298,-10.1138152863787));
#48695=CARTESIAN_POINT('Ctrl Pts',(20.2935358855687,21.2411349269503,-10.1166694969415));
#48696=CARTESIAN_POINT('',(16.1740010233873,19.2132890482674,-9.76670989018929));
#48697=CARTESIAN_POINT('Ctrl Pts',(16.174001023388,19.2132890490549,-9.76670989022851));
#48698=CARTESIAN_POINT('Ctrl Pts',(16.1741079389015,19.3328599270272,-9.77266511192853));
#48699=CARTESIAN_POINT('Ctrl Pts',(16.1825955516607,19.4520702292312,-9.77862033362856));
#48700=CARTESIAN_POINT('Ctrl Pts',(16.1992930219785,19.5699714968759,-9.78457555532858));
#48701=CARTESIAN_POINT('Ctrl Pts',(16.2067339930653,19.6225123852222,-9.78722940837587));
#48702=CARTESIAN_POINT('Ctrl Pts',(16.2158047738395,19.6747937484515,-9.78988326142315));
#48703=CARTESIAN_POINT('Ctrl Pts',(16.2264874578014,19.7267333135613,-9.79253711447044));
#48704=CARTESIAN_POINT('Ctrl Pts',(16.2433320704913,19.8086323813112,-9.79672174886349));
#48705=CARTESIAN_POINT('Ctrl Pts',(16.2642246666771,19.8898577370365,-9.80090638325653));
#48706=CARTESIAN_POINT('Ctrl Pts',(16.2890969179465,19.969978866218,-9.80509101764958));
#48707=CARTESIAN_POINT('Ctrl Pts',(16.3139337666449,20.0499859528891,-9.80926969573353));
#48708=CARTESIAN_POINT('Ctrl Pts',(16.3427388836329,20.1288914993742,-9.81344837381748));
#48709=CARTESIAN_POINT('Ctrl Pts',(16.3753929533288,20.2062752380084,-9.81762705190142));
#48710=CARTESIAN_POINT('Ctrl Pts',(16.4086323237558,20.2850460245429,-9.82188062978686));
#48711=CARTESIAN_POINT('Ctrl Pts',(16.4458598919279,20.3622394375428,-9.82613420767229));
#48712=CARTESIAN_POINT('Ctrl Pts',(16.4868966678982,20.4374283977701,-9.83038778555773));
#48713=CARTESIAN_POINT('Ctrl Pts',(16.5271378658896,20.5111596732842,-9.83455889953568));
#48714=CARTESIAN_POINT('Ctrl Pts',(16.5710416613174,20.5829631005169,-9.83873001351363));
#48715=CARTESIAN_POINT('Ctrl Pts',(16.6183914981669,20.6524578269833,-9.84290112749158));
#48716=CARTESIAN_POINT('Ctrl Pts',(16.6657254463213,20.7219292338231,-9.84707084181195));
#48717=CARTESIAN_POINT('Ctrl Pts',(16.7165028805481,20.7890930986176,-9.85124055613233));
#48718=CARTESIAN_POINT('Ctrl Pts',(16.7704633948897,20.8535967248207,-9.8554102704527));
#48719=CARTESIAN_POINT('Ctrl Pts',(16.8244219890847,20.9180980557081,-9.85957983639674));
#48720=CARTESIAN_POINT('Ctrl Pts',(16.8815631423605,20.9799389839165,-9.86374940234079));
#48721=CARTESIAN_POINT('Ctrl Pts',(16.9415864376591,21.0388002137915,-9.86791896828483));
#48722=CARTESIAN_POINT('Ctrl Pts',(17.0037200779736,21.0997309318957,-9.87223513102375));
#48723=CARTESIAN_POINT('Ctrl Pts',(17.0689419268742,21.1574681514489,-9.87655129376267));
#48724=CARTESIAN_POINT('Ctrl Pts',(17.1368790142891,21.2117010163945,-9.88086745650159));
#48725=CARTESIAN_POINT('Ctrl Pts',(17.2026030582273,21.2641672514687,-9.88504302069327));
#48726=CARTESIAN_POINT('Ctrl Pts',(17.270867749702,21.3133536974898,-9.88921858488495));
#48727=CARTESIAN_POINT('Ctrl Pts',(17.3413050297812,21.3590225138316,-9.89339414907663));
#48728=CARTESIAN_POINT('Ctrl Pts',(17.4152999294285,21.4069979535195,-9.89778061108917));
#48729=CARTESIAN_POINT('Ctrl Pts',(17.4916921547949,21.4510907819032,-9.9021670731017));
#48730=CARTESIAN_POINT('Ctrl Pts',(17.5700268579946,21.4910803768047,-9.90655353511425));
#48731=CARTESIAN_POINT('Ctrl Pts',(17.6483615611942,21.5310699717063,-9.91093999712678));
#48732=CARTESIAN_POINT('Ctrl Pts',(17.7286381814852,21.5669561657755,-9.91532645913933));
#48733=CARTESIAN_POINT('Ctrl Pts',(17.8103811197832,21.5985778865007,-9.91971292115187));
#48734=CARTESIAN_POINT('Ctrl Pts',(17.8883629443181,21.6287446449807,-9.92389755554492));
#48735=CARTESIAN_POINT('Ctrl Pts',(17.9679693803479,21.6551430224068,-9.92808218993796));
#48736=CARTESIAN_POINT('Ctrl Pts',(18.0488014484185,21.6775974428168,-9.93226682433101));
#48737=CARTESIAN_POINT('Ctrl Pts',(18.1295184620453,21.7000199021387,-9.93644550241496));
#48738=CARTESIAN_POINT('Ctrl Pts',(18.2114572030592,21.7185094330108,-9.9406241804989));
#48739=CARTESIAN_POINT('Ctrl Pts',(18.2941997096014,21.7329388780391,-9.94480285858285));
#48740=CARTESIAN_POINT('Ctrl Pts',(18.3784253161073,21.7476269604994,-9.94905643646828));
#48741=CARTESIAN_POINT('Ctrl Pts',(18.4634833368926,21.758107797425,-9.95331001435372));
#48742=CARTESIAN_POINT('Ctrl Pts',(18.5489177820416,21.7643007211442,-9.95756359223915));
#48743=CARTESIAN_POINT('Ctrl Pts',(18.6326959137598,21.7703735829526,-9.96173470621711));
#48744=CARTESIAN_POINT('Ctrl Pts',(18.7168355246875,21.7723232722254,-9.96590582019506));
#48745=CARTESIAN_POINT('Ctrl Pts',(18.8008991604928,21.7701257300737,-9.97007693417301));
#48746=CARTESIAN_POINT('Ctrl Pts',(18.8849345879333,21.7679289253285,-9.97424664849339));
#48747=CARTESIAN_POINT('Ctrl Pts',(18.9688936313901,21.7615876649968,-9.97841636281376));
#48748=CARTESIAN_POINT('Ctrl Pts',(19.0523387760779,21.7511300013277,-9.98258607713413));
#48749=CARTESIAN_POINT('Ctrl Pts',(19.1357809514293,21.7406727097872,-9.98675564307818));
#48750=CARTESIAN_POINT('Ctrl Pts',(19.2187088080141,21.726099364199,-9.99092520902222));
#48751=CARTESIAN_POINT('Ctrl Pts',(19.3006912586606,21.7074897390852,-9.99509477496627));
#48752=CARTESIAN_POINT('Ctrl Pts',(19.3855561111356,21.6882258225098,-9.99941093770518));
#48753=CARTESIAN_POINT('Ctrl Pts',(19.4694073254465,21.6646366310369,-10.0037271004441));
#48754=CARTESIAN_POINT('Ctrl Pts',(19.5517816392177,21.6368675129855,-10.008043263183));
#48755=CARTESIAN_POINT('Ctrl Pts',(19.631472618382,21.6100029710338,-10.0122188273747));
#48756=CARTESIAN_POINT('Ctrl Pts',(19.7097810183149,21.5792268589616,-10.0163943915664));
#48757=CARTESIAN_POINT('Ctrl Pts',(19.7863076293697,21.5447199174645,-10.0205699557581));
#48758=CARTESIAN_POINT('Ctrl Pts',(19.8666994176241,21.5084701123847,-10.0249564177706));
#48759=CARTESIAN_POINT('Ctrl Pts',(19.9451241711511,21.4681029519008,-10.0293428797831));
#48760=CARTESIAN_POINT('Ctrl Pts',(20.0211501810795,21.423881472503,-10.0337293417957));
#48761=CARTESIAN_POINT('Ctrl Pts',(20.0971761910079,21.3796599931052,-10.0381158038082));
#48762=CARTESIAN_POINT('Ctrl Pts',(20.1708030131037,21.3315845757053,-10.0425022658208));
#48763=CARTESIAN_POINT('Ctrl Pts',(20.2416377781111,21.2799679383722,-10.0468887278333));
#48764=CARTESIAN_POINT('Ctrl Pts',(20.2590918809816,21.267249295235,-10.0479695778819));
#48765=CARTESIAN_POINT('Ctrl Pts',(20.2763933923835,21.2543036739806,-10.0490504279306));
#48766=CARTESIAN_POINT('Ctrl Pts',(20.2935358855687,21.2411349269503,-10.0501312779792));
#48767=CARTESIAN_POINT('Ctrl Pts',(20.2935358855687,21.2411349269503,-9.25004024781016));
#48768=CARTESIAN_POINT('Ctrl Pts',(20.3602016680315,21.1899227248892,-9.25421688790189));
#48769=CARTESIAN_POINT('Ctrl Pts',(20.4242843918201,21.1354677868026,-9.25839352799362));
#48770=CARTESIAN_POINT('Ctrl Pts',(20.4854677333106,21.0780727835764,-9.26257016808535));
#48771=CARTESIAN_POINT('Ctrl Pts',(20.546756242997,21.0205791239384,-9.26675398741399));
#48772=CARTESIAN_POINT('Ctrl Pts',(20.6051350976159,20.9601356375273,-9.27093780674262));
#48773=CARTESIAN_POINT('Ctrl Pts',(20.6603262817686,20.8970803824752,-9.27512162607126));
#48774=CARTESIAN_POINT('Ctrl Pts',(20.6986357784777,20.8533122495207,-9.27802571329574));
#48775=CARTESIAN_POINT('Ctrl Pts',(20.7354102689322,20.8082864597362,-9.28092980052022));
#48776=CARTESIAN_POINT('Ctrl Pts',(20.7705691100607,20.7621241923026,-9.28383388774471));
#48777=CARTESIAN_POINT('Ctrl Pts',(20.8212311199913,20.6956068334797,-9.28801852213775));
#48778=CARTESIAN_POINT('Ctrl Pts',(20.8687251499198,20.6264810343216,-9.2922031565308));
#48779=CARTESIAN_POINT('Ctrl Pts',(20.9127716012343,20.5550812139358,-9.29638779092385));
#48780=CARTESIAN_POINT('Ctrl Pts',(20.9567553578771,20.4837830223567,-9.30056646900779));
#48781=CARTESIAN_POINT('Ctrl Pts',(20.9973010436861,20.4102176270062,-9.30474514709174));
#48782=CARTESIAN_POINT('Ctrl Pts',(21.0341702903064,20.3347511448678,-9.30892382517568));
#48783=CARTESIAN_POINT('Ctrl Pts',(21.071700391675,20.2579319802738,-9.31317740306112));
#48784=CARTESIAN_POINT('Ctrl Pts',(21.1054206649962,20.17914328813,-9.31743098094655));
#48785=CARTESIAN_POINT('Ctrl Pts',(21.1351268232138,20.0988006413847,-9.32168455883199));
#48786=CARTESIAN_POINT('Ctrl Pts',(21.1642570695877,20.0200155936222,-9.32585567280994));
#48787=CARTESIAN_POINT('Ctrl Pts',(21.1895272879509,19.939736757811,-9.33002678678789));
#48788=CARTESIAN_POINT('Ctrl Pts',(21.2107927216344,19.8583776440833,-9.33419790076585));
#48789=CARTESIAN_POINT('Ctrl Pts',(21.2320510194963,19.7770458311919,-9.33836761508622));
#48790=CARTESIAN_POINT('Ctrl Pts',(21.2493070853372,19.6946349050202,-9.34253732940659));
#48791=CARTESIAN_POINT('Ctrl Pts',(21.2624662014641,19.6115729247637,-9.34670704372696));
#48792=CARTESIAN_POINT('Ctrl Pts',(21.2756248493332,19.5285139002089,-9.350876609671));
#48793=CARTESIAN_POINT('Ctrl Pts',(21.284686766209,19.4448043221314,-9.35504617561505));
#48794=CARTESIAN_POINT('Ctrl Pts',(21.2896087040397,19.3608804584878,-9.35921574155909));
#48795=CARTESIAN_POINT('Ctrl Pts',(21.2947036911327,19.2740059353297,-9.36353190429801));
#48796=CARTESIAN_POINT('Ctrl Pts',(21.2953621283496,19.1869023041988,-9.36784806703693));
#48797=CARTESIAN_POINT('Ctrl Pts',(21.2915948078576,19.1000549738832,-9.37216422977585));
#48798=CARTESIAN_POINT('Ctrl Pts',(21.2879502074343,19.0160366862179,-9.37633979396754));
#48799=CARTESIAN_POINT('Ctrl Pts',(21.2801638500694,18.9322587224487,-9.38051535815921));
#48800=CARTESIAN_POINT('Ctrl Pts',(21.2682983360669,18.8491548068461,-9.38469092235089));
#48801=CARTESIAN_POINT('Ctrl Pts',(21.2558335231597,18.7618535100273,-9.38907738436343));
#48802=CARTESIAN_POINT('Ctrl Pts',(21.2388667599596,18.675296716199,-9.39346384637597));
#48803=CARTESIAN_POINT('Ctrl Pts',(21.2175306593405,18.5899722517346,-9.39785030838851));
#48804=CARTESIAN_POINT('Ctrl Pts',(21.1961945587214,18.5046477872701,-9.40223677040106));
#48805=CARTESIAN_POINT('Ctrl Pts',(21.1704893630394,18.4205561848055,-9.4066232324136));
#48806=CARTESIAN_POINT('Ctrl Pts',(21.1406062076889,18.3381617783842,-9.41100969442614));
#48807=CARTESIAN_POINT('Ctrl Pts',(21.1120980206135,18.2595584607401,-9.41519432881919));
#48808=CARTESIAN_POINT('Ctrl Pts',(21.0796817805212,18.1822070136536,-9.41937896321224));
#48809=CARTESIAN_POINT('Ctrl Pts',(21.0434873395327,18.1065235500301,-9.42356359760529));
#48810=CARTESIAN_POINT('Ctrl Pts',(21.007344416851,18.0309478124492,-9.42774227568923));
#48811=CARTESIAN_POINT('Ctrl Pts',(20.967434172056,17.9570357539526,-9.43192095377318));
#48812=CARTESIAN_POINT('Ctrl Pts',(20.9239354273224,17.8851859767831,-9.43609963185712));
#48813=CARTESIAN_POINT('Ctrl Pts',(20.8796569988514,17.8120483439955,-9.44035320974256));
#48814=CARTESIAN_POINT('Ctrl Pts',(20.8316603217325,17.7410481057697,-9.44460678762799));
#48815=CARTESIAN_POINT('Ctrl Pts',(20.7801842503405,17.6725819769456,-9.44886036551343));
#48816=CARTESIAN_POINT('Ctrl Pts',(20.7297061430397,17.6054431976295,-9.45303147949138));
#48817=CARTESIAN_POINT('Ctrl Pts',(20.6758826364361,17.5407415318687,-9.45720259346933));
#48818=CARTESIAN_POINT('Ctrl Pts',(20.618983073072,17.4788225223055,-9.46137370744728));
#48819=CARTESIAN_POINT('Ctrl Pts',(20.5621026029059,17.416924290264,-9.46554342176766));
#48820=CARTESIAN_POINT('Ctrl Pts',(20.5021484369599,17.3578071984335,-9.46971313608803));
#48821=CARTESIAN_POINT('Ctrl Pts',(20.4394292363846,17.3017825897283,-9.4738828504084));
#48822=CARTESIAN_POINT('Ctrl Pts',(20.3767122676277,17.2457599746191,-9.47805241635244));
#48823=CARTESIAN_POINT('Ctrl Pts',(20.3112308035245,17.1928299296704,-9.48222198229649));
#48824=CARTESIAN_POINT('Ctrl Pts',(20.2433282670354,17.1432649632199,-9.48639154824053));
#48825=CARTESIAN_POINT('Ctrl Pts',(20.1730383611302,17.0919573536941,-9.49070771097945));
#48826=CARTESIAN_POINT('Ctrl Pts',(20.1001543913748,17.0442561687145,-9.49502387371837));
#48827=CARTESIAN_POINT('Ctrl Pts',(20.025090351338,17.000415076347,-9.49934003645729));
#48828=CARTESIAN_POINT('Ctrl Pts',(19.9524715145099,16.9580021029521,-9.50351560064897));
#48829=CARTESIAN_POINT('Ctrl Pts',(19.8778128975685,16.9192017744647,-9.50769116484065));
#48830=CARTESIAN_POINT('Ctrl Pts',(19.8015130783443,16.8841962206572,-9.51186672903234));
#48831=CARTESIAN_POINT('Ctrl Pts',(19.7213595366366,16.8474226195447,-9.51625319104488));
#48832=CARTESIAN_POINT('Ctrl Pts',(19.6393951838166,16.8148374315278,-9.52063965305742));
#48833=CARTESIAN_POINT('Ctrl Pts',(19.5561019854973,16.7865932013292,-9.52502611506996));
#48834=CARTESIAN_POINT('Ctrl Pts',(19.472808787178,16.7583489711306,-9.5294125770825));
#48835=CARTESIAN_POINT('Ctrl Pts',(19.3881873224049,16.7344457832731,-9.53379903909503));
#48836=CARTESIAN_POINT('Ctrl Pts',(19.3027314805897,16.7149742583486,-9.53818550110757));
#48837=CARTESIAN_POINT('Ctrl Pts',(19.2212075887324,16.6963986471497,-9.54237013550062));
#48838=CARTESIAN_POINT('Ctrl Pts',(19.1386209669252,16.6817867038644,-9.54655476989367));
#48839=CARTESIAN_POINT('Ctrl Pts',(19.0553917867604,16.6712544774322,-9.55073940428672));
#48840=CARTESIAN_POINT('Ctrl Pts',(18.9722810730319,16.6607372423208,-9.55491808237066));
#48841=CARTESIAN_POINT('Ctrl Pts',(18.8885300701232,16.654288246849,-9.5590967604546));
#48842=CARTESIAN_POINT('Ctrl Pts',(18.8045707324921,16.6519728857014,-9.56327543853854));
#48843=CARTESIAN_POINT('Ctrl Pts',(18.7191064840744,16.6496160233692,-9.56752901642398));
#48844=CARTESIAN_POINT('Ctrl Pts',(18.6334268287623,16.6515425508617,-9.57178259430941));
#48845=CARTESIAN_POINT('Ctrl Pts',(18.5479946282975,16.6577663636679,-9.57603617219485));
#48846=CARTESIAN_POINT('Ctrl Pts',(18.464218697746,16.663869515718,-9.5802072861728));
#48847=CARTESIAN_POINT('Ctrl Pts',(18.3806811928208,16.6741047825048,-9.58437840015076));
#48848=CARTESIAN_POINT('Ctrl Pts',(18.2978184502104,16.6884327252533,-9.58854951412871));
#48849=CARTESIAN_POINT('Ctrl Pts',(18.2149835129936,16.7027558601221,-9.59271922844908));
#48850=CARTESIAN_POINT('Ctrl Pts',(18.1328233413408,16.7211688651668,-9.59688894276946));
#48851=CARTESIAN_POINT('Ctrl Pts',(18.0517667977986,16.7435807292205,-9.60105865708983));
#48852=CARTESIAN_POINT('Ctrl Pts',(17.970713138596,16.7659917957639,-9.60522822303387));
#48853=CARTESIAN_POINT('Ctrl Pts',(17.8907634725905,16.7924013149753,-9.60939778897792));
#48854=CARTESIAN_POINT('Ctrl Pts',(17.8123328245036,16.8226680260876,-9.61356735492196));
#48855=CARTESIAN_POINT('Ctrl Pts',(17.7311446515846,16.8539988774245,-9.61788351766088));
#48856=CARTESIAN_POINT('Ctrl Pts',(17.6515847934182,16.8894630151456,-9.6221996803998));
#48857=CARTESIAN_POINT('Ctrl Pts',(17.5740906315705,16.9288496418883,-9.62651584313872));
#48858=CARTESIAN_POINT('Ctrl Pts',(17.4991208338941,16.9669532534076,-9.6306914073304));
#48859=CARTESIAN_POINT('Ctrl Pts',(17.4260846045836,17.0087274533692,-9.63486697152208));
#48860=CARTESIAN_POINT('Ctrl Pts',(17.3553508285749,17.0539356842855,-9.63904253571376));
#48861=CARTESIAN_POINT('Ctrl Pts',(17.2810444576937,17.101427275473,-9.64342899772631));
#48862=CARTESIAN_POINT('Ctrl Pts',(17.2092797216846,17.1527085808079,-9.64781545973885));
#48863=CARTESIAN_POINT('Ctrl Pts',(17.1404457653641,17.2074569130478,-9.65220192175139));
#48864=CARTESIAN_POINT('Ctrl Pts',(17.0716118090436,17.2622052452876,-9.65658838376393));
#48865=CARTESIAN_POINT('Ctrl Pts',(17.0057090169082,17.3204201632973,-9.66097484577647));
#48866=CARTESIAN_POINT('Ctrl Pts',(16.9430809195061,17.3817354354488,-9.66536130778901));
#48867=CARTESIAN_POINT('Ctrl Pts',(16.8827886985013,17.4407637964061,-9.66958416538902));
#48868=CARTESIAN_POINT('Ctrl Pts',(16.8252872091303,17.5029045422553,-9.67380702298903));
#48869=CARTESIAN_POINT('Ctrl Pts',(16.7709203169311,17.5678572314245,-9.67802988058904));
#48870=CARTESIAN_POINT('Ctrl Pts',(16.7179063153622,17.6311936081462,-9.68214765466764));
#48871=CARTESIAN_POINT('Ctrl Pts',(16.6678730797622,17.6972032456021,-9.68626542874624));
#48872=CARTESIAN_POINT('Ctrl Pts',(16.6211045875939,17.7655682388182,-9.69038320282484));
#48873=CARTESIAN_POINT('Ctrl Pts',(16.57438033231,17.833868567681,-9.69449708202705));
#48874=CARTESIAN_POINT('Ctrl Pts',(16.530914960773,17.9045194435154,-9.69861096122926));
#48875=CARTESIAN_POINT('Ctrl Pts',(16.4909521572678,17.9771700379653,-9.70272484043147));
#48876=CARTESIAN_POINT('Ctrl Pts',(16.451014356568,18.0497751784301,-9.70683614577719));
#48877=CARTESIAN_POINT('Ctrl Pts',(16.4145750025456,18.1243771397533,-9.7109474511229));
#48878=CARTESIAN_POINT('Ctrl Pts',(16.3818335581791,18.2005975900802,-9.71505875646862));
#48879=CARTESIAN_POINT('Ctrl Pts',(16.3475554603697,18.2803952930204,-9.71936301761201));
#48880=CARTESIAN_POINT('Ctrl Pts',(16.3173311789841,18.3619666588744,-9.7236672787554));
#48881=CARTESIAN_POINT('Ctrl Pts',(16.2913340385439,18.4448518415191,-9.72797153989879));
#48882=CARTESIAN_POINT('Ctrl Pts',(16.2665001036005,18.5240284432035,-9.73208321292914));
#48883=CARTESIAN_POINT('Ctrl Pts',(16.2455232446819,18.6044033134949,-9.73619488595948));
#48884=CARTESIAN_POINT('Ctrl Pts',(16.2285034541843,18.685560128173,-9.74030655898983));
#48885=CARTESIAN_POINT('Ctrl Pts',(16.2114791195103,18.7667386112068,-9.74441932981085));
#48886=CARTESIAN_POINT('Ctrl Pts',(16.1984140354435,18.84869898642,-9.74853210063186));
#48887=CARTESIAN_POINT('Ctrl Pts',(16.1893567554131,18.9310165044539,-9.75264487145288));
#48888=CARTESIAN_POINT('Ctrl Pts',(16.1802905487374,19.0134151527258,-9.7567616957255));
#48889=CARTESIAN_POINT('Ctrl Pts',(16.1752400549859,19.0961711731434,-9.76087851999813));
#48890=CARTESIAN_POINT('Ctrl Pts',(16.1742017924823,19.1788575547115,-9.76499534427075));
#48891=CARTESIAN_POINT('Ctrl Pts',(16.1740576564023,19.1903364349233,-9.76556685957693));
#48892=CARTESIAN_POINT('Ctrl Pts',(16.1739907628404,19.2018139780891,-9.76613837488311));
#48893=CARTESIAN_POINT('Ctrl Pts',(16.1740010233873,19.2132890482674,-9.76670989018929));
#48894=CARTESIAN_POINT('Origin',(18.734,19.211,1.76670989022852));
#48895=CARTESIAN_POINT('',(20.2935358855687,21.2411349269503,-8.45013430427981));
#48896=CARTESIAN_POINT('',(20.2935358855687,21.2411349269503,-8.51667715193081));
#48897=CARTESIAN_POINT('',(20.2935358855687,21.2411349269503,1.76670989022852));
#48898=CARTESIAN_POINT('',(16.1736699135442,19.2103574886798,-9.03329016588334));
#48899=CARTESIAN_POINT('Ctrl Pts',(20.2935358855687,21.2411349269503,-8.51667715193082));
#48900=CARTESIAN_POINT('Ctrl Pts',(20.3077409106736,21.2302227229818,-8.51757293187653));
#48901=CARTESIAN_POINT('Ctrl Pts',(20.3218260012755,21.2191655684692,-8.51846871182225));
#48902=CARTESIAN_POINT('Ctrl Pts',(20.3357880909557,21.2079664272773,-8.51936449176796));
#48903=CARTESIAN_POINT('Ctrl Pts',(20.4010119675942,21.1556496594946,-8.52354912616101));
#48904=CARTESIAN_POINT('Ctrl Pts',(20.463791413314,21.1000367097147,-8.52773376055406));
#48905=CARTESIAN_POINT('Ctrl Pts',(20.5237743555653,21.0413845924179,-8.53191839494711));
#48906=CARTESIAN_POINT('Ctrl Pts',(20.5836719195227,20.9828159591504,-8.53609707303105));
#48907=CARTESIAN_POINT('Ctrl Pts',(20.6407805603834,20.9212170697946,-8.540275751115));
#48908=CARTESIAN_POINT('Ctrl Pts',(20.6947805623983,20.8568856540237,-8.54445442919895));
#48909=CARTESIAN_POINT('Ctrl Pts',(20.7497484756403,20.7914011438593,-8.54870800708438));
#48910=CARTESIAN_POINT('Ctrl Pts',(20.8014948330691,20.7230854843409,-8.55296158496981));
#48911=CARTESIAN_POINT('Ctrl Pts',(20.8497210505506,20.6522926268656,-8.55721516285525));
#48912=CARTESIAN_POINT('Ctrl Pts',(20.8970123087005,20.5828722270732,-8.5613862768332));
#48913=CARTESIAN_POINT('Ctrl Pts',(20.9409184275291,20.5110702205223,-8.56555739081116));
#48914=CARTESIAN_POINT('Ctrl Pts',(20.9811990900047,20.4372529306314,-8.56972850478911));
#48915=CARTESIAN_POINT('Ctrl Pts',(21.021466235915,20.363460410845,-8.57389821910948));
#48916=CARTESIAN_POINT('Ctrl Pts',(21.058110121399,20.2876543542438,-8.57806793342985));
#48917=CARTESIAN_POINT('Ctrl Pts',(21.0909354749524,20.210227284911,-8.58223764775023));
#48918=CARTESIAN_POINT('Ctrl Pts',(21.123759660439,20.1328029707657,-8.58640721369427));
#48919=CARTESIAN_POINT('Ctrl Pts',(21.1527654053819,20.0537581824512,-8.59057677963832));
#48920=CARTESIAN_POINT('Ctrl Pts',(21.1778054030264,19.9735058374459,-8.59474634558236));
#48921=CARTESIAN_POINT('Ctrl Pts',(21.2037257760978,19.8904319189921,-8.59906250832128));
#48922=CARTESIAN_POINT('Ctrl Pts',(21.2253961847597,19.8060644520147,-8.6033786710602));
#48923=CARTESIAN_POINT('Ctrl Pts',(21.2427098983461,19.7208770890524,-8.60769483379912));
#48924=CARTESIAN_POINT('Ctrl Pts',(21.2594596195334,19.6384646954784,-8.6118703979908));
#48925=CARTESIAN_POINT('Ctrl Pts',(21.2721321012068,19.5552854746202,-8.61604596218248));
#48926=CARTESIAN_POINT('Ctrl Pts',(21.2806833673555,19.4717754329589,-8.62022152637416));
#48927=CARTESIAN_POINT('Ctrl Pts',(21.2896665376286,19.3840474976196,-8.6246079883867));
#48928=CARTESIAN_POINT('Ctrl Pts',(21.2941011966021,19.2959550268227,-8.62899445039924));
#48929=CARTESIAN_POINT('Ctrl Pts',(21.2939982462078,19.2080034331647,-8.63338091241178));
#48930=CARTESIAN_POINT('Ctrl Pts',(21.2938952958136,19.1200518395066,-8.63776737442432));
#48931=CARTESIAN_POINT('Ctrl Pts',(21.2892548426303,19.0322416983818,-8.64215383643686));
#48932=CARTESIAN_POINT('Ctrl Pts',(21.2801502518719,18.9450697555886,-8.6465402984494));
#48933=CARTESIAN_POINT('Ctrl Pts',(21.2714645768305,18.8619087231031,-8.65072493284245));
#48934=CARTESIAN_POINT('Ctrl Pts',(21.2586842102674,18.7790189093826,-8.65490956723549));
#48935=CARTESIAN_POINT('Ctrl Pts',(21.2418346904937,18.6968354687883,-8.65909420162854));
#48936=CARTESIAN_POINT('Ctrl Pts',(21.2250091539259,18.6147690061494,-8.66327287971249));
#48937=CARTESIAN_POINT('Ctrl Pts',(21.2041260603601,18.533407366331,-8.66745155779643));
#48938=CARTESIAN_POINT('Ctrl Pts',(21.1792626972637,18.4531805351071,-8.67163023588037));
#48939=CARTESIAN_POINT('Ctrl Pts',(21.1539536762528,18.3715156955914,-8.67588381376581));
#48940=CARTESIAN_POINT('Ctrl Pts',(21.1245203396143,18.2910272272441,-8.68013739165124));
#48941=CARTESIAN_POINT('Ctrl Pts',(21.0910986865303,18.2121577792478,-8.68439096953668));
#48942=CARTESIAN_POINT('Ctrl Pts',(21.0583249774083,18.1348173694021,-8.68856208351463));
#48943=CARTESIAN_POINT('Ctrl Pts',(21.0217164021894,18.0590342074479,-8.69273319749258));
#48944=CARTESIAN_POINT('Ctrl Pts',(20.9814509018453,17.9852086458966,-8.69690431147054));
#48945=CARTESIAN_POINT('Ctrl Pts',(20.9411989129789,17.9114078572255,-8.70107402579091));
#48946=CARTESIAN_POINT('Ctrl Pts',(20.897292656152,17.8395637678915,-8.70524374011128));
#48947=CARTESIAN_POINT('Ctrl Pts',(20.849956485239,17.7700530361685,-8.70941345443166));
#48948=CARTESIAN_POINT('Ctrl Pts',(20.80262199875,17.7005447779357,-8.7135830203757));
#48949=CARTESIAN_POINT('Ctrl Pts',(20.7518581004866,17.6333700919857,-8.71775258631974));
#48950=CARTESIAN_POINT('Ctrl Pts',(20.6979322543499,17.5688763443869,-8.72192215226378));
#48951=CARTESIAN_POINT('Ctrl Pts',(20.6421104419877,17.5021150761842,-8.7262383150027));
#48952=CARTESIAN_POINT('Ctrl Pts',(20.5829005348977,17.4382271821969,-8.73055447774163));
#48953=CARTESIAN_POINT('Ctrl Pts',(20.5206430286226,17.3775587851599,-8.73487064048055));
#48954=CARTESIAN_POINT('Ctrl Pts',(20.460413554066,17.3188666547752,-8.73904620467223));
#48955=CARTESIAN_POINT('Ctrl Pts',(20.3973323666986,17.2631877685198,-8.74322176886391));
#48956=CARTESIAN_POINT('Ctrl Pts',(20.3317422755907,17.2107951052979,-8.74739733305559));
#48957=CARTESIAN_POINT('Ctrl Pts',(20.2628393849066,17.1557562132084,-8.75178379506813));
#48958=CARTESIAN_POINT('Ctrl Pts',(20.1911679546945,17.1043445831752,-8.75617025708067));
#48959=CARTESIAN_POINT('Ctrl Pts',(20.1171588579738,17.0568246186513,-8.76055671909321));
#48960=CARTESIAN_POINT('Ctrl Pts',(20.043149761253,17.0093046541274,-8.76494318110575));
#48961=CARTESIAN_POINT('Ctrl Pts',(19.9668035395282,16.9656765769471,-8.76932964311829));
#48962=CARTESIAN_POINT('Ctrl Pts',(19.8885775886028,16.9261475776549,-8.77371610513083));
#48963=CARTESIAN_POINT('Ctrl Pts',(19.8139509296381,16.8884373662162,-8.77790073952388));
#48964=CARTESIAN_POINT('Ctrl Pts',(19.7373359438749,16.8543169479217,-8.78208537391693));
#48965=CARTESIAN_POINT('Ctrl Pts',(19.6591123506695,16.8240003898955,-8.78627000830997));
#48966=CARTESIAN_POINT('Ctrl Pts',(19.5810000990668,16.7937269837373,-8.79044868639392));
#48967=CARTESIAN_POINT('Ctrl Pts',(19.5012842132702,16.7672468481168,-8.79462736447787));
#48968=CARTESIAN_POINT('Ctrl Pts',(19.420368077509,16.7447277396491,-8.79880604256181));
#48969=CARTESIAN_POINT('Ctrl Pts',(19.3380015781677,16.7218049923462,-8.80305962044725));
#48970=CARTESIAN_POINT('Ctrl Pts',(19.2543918069889,16.7029868892007,-8.80731319833268));
#48971=CARTESIAN_POINT('Ctrl Pts',(19.1699845756622,16.6883986740302,-8.81156677621811));
#48972=CARTESIAN_POINT('Ctrl Pts',(19.0872137432219,16.6740932798773,-8.81573789019606));
#48973=CARTESIAN_POINT('Ctrl Pts',(19.0036765695344,16.6638553099793,-8.81990900417402));
#48974=CARTESIAN_POINT('Ctrl Pts',(18.9198060037776,16.6577518473599,-8.82408011815197));
#48975=CARTESIAN_POINT('Ctrl Pts',(18.8359635815991,16.6516504328162,-8.82824983247234));
#48976=CARTESIAN_POINT('Ctrl Pts',(18.7517884479705,16.6496808035662,-8.83241954679272));
#48977=CARTESIAN_POINT('Ctrl Pts',(18.6677187513895,16.6518581914863,-8.83658926111309));
#48978=CARTESIAN_POINT('Ctrl Pts',(18.5836520463691,16.6540355019256,-8.84075882705714));
#48979=CARTESIAN_POINT('Ctrl Pts',(18.4996912307931,16.660359523368,-8.84492839300118));
#48980=CARTESIAN_POINT('Ctrl Pts',(18.4162731576902,16.6707933836643,-8.84909795894523));
#48981=CARTESIAN_POINT('Ctrl Pts',(18.3299222080443,16.681594085617,-8.85341412168415));
#48982=CARTESIAN_POINT('Ctrl Pts',(18.2441533999762,16.6967989420232,-8.85773028442307));
#48983=CARTESIAN_POINT('Ctrl Pts',(18.1594420717103,16.7163089996876,-8.86204644716199));
#48984=CARTESIAN_POINT('Ctrl Pts',(18.0774902060527,16.7351835192758,-8.86622201135367));
#48985=CARTESIAN_POINT('Ctrl Pts',(17.996528423794,16.758086889941,-8.87039757554535));
#48986=CARTESIAN_POINT('Ctrl Pts',(17.9169718130409,16.7848786218092,-8.87457313973703));
#48987=CARTESIAN_POINT('Ctrl Pts',(17.8333969870066,16.8130235403628,-8.87895960174957));
#48988=CARTESIAN_POINT('Ctrl Pts',(17.7513735563979,16.8454597306831,-8.88334606376211));
#48989=CARTESIAN_POINT('Ctrl Pts',(17.6713570660694,16.8819680133224,-8.88773252577465));
#48990=CARTESIAN_POINT('Ctrl Pts',(17.5913405757408,16.9184762959617,-8.89211898778719));
#48991=CARTESIAN_POINT('Ctrl Pts',(17.513331505326,16.959056335675,-8.89650544979973));
#48992=CARTESIAN_POINT('Ctrl Pts',(17.4377516489576,17.003435683288,-8.90089191181227));
#48993=CARTESIAN_POINT('Ctrl Pts',(17.365649333817,17.0457730713314,-8.90507654620532));
#48994=CARTESIAN_POINT('Ctrl Pts',(17.2954892230291,17.091725414496,-8.90926118059837));
#48995=CARTESIAN_POINT('Ctrl Pts',(17.2276568480541,17.1410892993693,-8.91344581499142));
#48996=CARTESIAN_POINT('Ctrl Pts',(17.159921024069,17.1903829208624,-8.91762449307535));
#48997=CARTESIAN_POINT('Ctrl Pts',(17.0945067235342,17.2430781703289,-8.92180317115929));
#48998=CARTESIAN_POINT('Ctrl Pts',(17.0317733474474,17.2989266689429,-8.92598184924323));
#48999=CARTESIAN_POINT('Ctrl Pts',(16.9679155206799,17.3557762117571,-8.93023542712867));
#49000=CARTESIAN_POINT('Ctrl Pts',(16.9068360906096,17.4158929154663,-8.9344890050141));
#49001=CARTESIAN_POINT('Ctrl Pts',(16.8488816768788,17.4789697150936,-8.93874258289954));
#49002=CARTESIAN_POINT('Ctrl Pts',(16.792050822547,17.540823647876,-8.94291369687749));
#49003=CARTESIAN_POINT('Ctrl Pts',(16.7382252223475,17.6055235719755,-8.94708481085544));
#49004=CARTESIAN_POINT('Ctrl Pts',(16.6876956296653,17.6727417564176,-8.9512559248334));
#49005=CARTESIAN_POINT('Ctrl Pts',(16.637182992676,17.7399373851488,-8.95542563915377));
#49006=CARTESIAN_POINT('Ctrl Pts',(16.5899644428518,17.8096492285707,-8.95959535347414));
#49007=CARTESIAN_POINT('Ctrl Pts',(16.5462899492621,17.8815171178611,-8.96376506779451));
#49008=CARTESIAN_POINT('Ctrl Pts',(16.5026170097983,17.9533824497836,-8.96793463373855));
#49009=CARTESIAN_POINT('Ctrl Pts',(16.4624881140049,18.0274032814579,-8.9721041996826));
#49010=CARTESIAN_POINT('Ctrl Pts',(16.4261087184981,18.1031923304257,-8.97627376562664));
#49011=CARTESIAN_POINT('Ctrl Pts',(16.3884502683242,18.1816460288594,-8.98058992836556));
#49012=CARTESIAN_POINT('Ctrl Pts',(16.3548101172679,18.2619941236263,-8.98490609110448));
#49013=CARTESIAN_POINT('Ctrl Pts',(16.3253623529172,18.3437833690158,-8.9892222538434));
#49014=CARTESIAN_POINT('Ctrl Pts',(16.296873846393,18.4229083383394,-8.99339781803508));
#49015=CARTESIAN_POINT('Ctrl Pts',(16.2723088794104,18.5033815448835,-8.99757338222676));
#49016=CARTESIAN_POINT('Ctrl Pts',(16.2517740015379,18.5847779207351,-9.00174894641844));
#49017=CARTESIAN_POINT('Ctrl Pts',(16.2302019558011,18.6702854340295,-9.00613540843099));
#49018=CARTESIAN_POINT('Ctrl Pts',(16.213077931431,18.7568112533014,-9.01052187044352));
#49019=CARTESIAN_POINT('Ctrl Pts',(16.2004642109876,18.8438536997419,-9.01490833245606));
#49020=CARTESIAN_POINT('Ctrl Pts',(16.1878504905441,18.9308961461825,-9.01929479446861));
#49021=CARTESIAN_POINT('Ctrl Pts',(16.179747051756,19.0184546350337,-9.02368125648115));
#49022=CARTESIAN_POINT('Ctrl Pts',(16.1761531171477,19.10602703261,-9.02806771849369));
#49023=CARTESIAN_POINT('Ctrl Pts',(16.1747268399112,19.1407807303868,-9.0298085155863));
#49024=CARTESIAN_POINT('Ctrl Pts',(16.1740088273484,19.1755636940745,-9.0315493126789));
#49025=CARTESIAN_POINT('Ctrl Pts',(16.1740000808904,19.2103564484228,-9.0332901097715));
#49026=CARTESIAN_POINT('Ctrl Pts',(16.1699656655267,19.2103691596404,-9.03329079541918));
#49027=CARTESIAN_POINT('Ctrl Pts',(16.1727141287504,20.0241270866321,-9.07394170533784));
#49028=CARTESIAN_POINT('Ctrl Pts',(17.0319371680896,21.691475877328,-9.15698455081697));
#49029=CARTESIAN_POINT('Ctrl Pts',(19.1726622419323,21.9356231677813,-9.25149015768804));
#49030=CARTESIAN_POINT('Ctrl Pts',(20.1114245040166,21.382657416907,-9.30534485464049));
#49031=CARTESIAN_POINT('Ctrl Pts',(20.2929505577765,21.2403915309053,-9.31680761603245));
#49032=CARTESIAN_POINT('',(16.174000001606,19.2110906788005,-8.96670989026365));
#49033=CARTESIAN_POINT('Ctrl Pts',(16.174000001606,19.2110906788005,-8.96670989026365));
#49034=CARTESIAN_POINT('Ctrl Pts',(16.1740031377284,19.2996281672636,-8.97108917708311));
#49035=CARTESIAN_POINT('Ctrl Pts',(16.1786036643305,19.388071802769,-8.97546846390256));
#49036=CARTESIAN_POINT('Ctrl Pts',(16.1877467776184,19.4759424985001,-8.97984775072202));
#49037=CARTESIAN_POINT('Ctrl Pts',(16.1969159526896,19.5640636632955,-8.98423952038188));
#49038=CARTESIAN_POINT('Ctrl Pts',(16.2106535575187,19.6516082364872,-8.98863129004175));
#49039=CARTESIAN_POINT('Ctrl Pts',(16.2288531973791,19.7381048257399,-8.99302305970162));
#49040=CARTESIAN_POINT('Ctrl Pts',(16.2470794228643,19.8247277672657,-8.99742124475987));
#49041=CARTESIAN_POINT('Ctrl Pts',(16.2697805833341,19.9102992971043,-9.00181942981813));
#49042=CARTESIAN_POINT('Ctrl Pts',(16.2968004138021,19.9943633748375,-9.00621761487638));
#49043=CARTESIAN_POINT('Ctrl Pts',(16.3238953969119,20.0786612674176,-9.01062803299533));
#49044=CARTESIAN_POINT('Ctrl Pts',(16.3553329301083,20.1614429605719,-9.01503845111429));
#49045=CARTESIAN_POINT('Ctrl Pts',(16.3909082116845,20.2422714829415,-9.01944886923325));
#49046=CARTESIAN_POINT('Ctrl Pts',(16.4178853374884,20.3035646370615,-9.02279333761611));
#49047=CARTESIAN_POINT('Ctrl Pts',(16.4472408225494,20.363735085321,-9.02613780599897));
#49048=CARTESIAN_POINT('Ctrl Pts',(16.478868382946,20.422602818486,-9.02948227438183));
#49049=CARTESIAN_POINT('Ctrl Pts',(16.5184411227219,20.4962587519986,-9.03366690877488));
#49050=CARTESIAN_POINT('Ctrl Pts',(16.5616998679758,20.5681109610611,-9.03785154316793));
#49051=CARTESIAN_POINT('Ctrl Pts',(16.6084559713663,20.6377664778581,-9.04203617756098));
#49052=CARTESIAN_POINT('Ctrl Pts',(16.6551455232309,20.7073228486487,-9.04621485564492));
#49053=CARTESIAN_POINT('Ctrl Pts',(16.7053222910481,20.7746883591286,-9.05039353372887));
#49054=CARTESIAN_POINT('Ctrl Pts',(16.7587517035101,20.8394944480144,-9.05457221181282));
#49055=CARTESIAN_POINT('Ctrl Pts',(16.8131387997914,20.9054621394682,-9.05882578969825));
#49056=CARTESIAN_POINT('Ctrl Pts',(16.8708960667842,20.9687773268414,-9.06307936758369));
#49057=CARTESIAN_POINT('Ctrl Pts',(16.9317298045576,21.0290819955712,-9.06733294546912));
#49058=CARTESIAN_POINT('Ctrl Pts',(16.9913841616171,21.0882175406228,-9.07150405944708));
#49059=CARTESIAN_POINT('Ctrl Pts',(17.0539964254171,21.1444579161298,-9.07567517342503));
#49060=CARTESIAN_POINT('Ctrl Pts',(17.1192501263854,21.1975001499274,-9.07984628740298));
#49061=CARTESIAN_POINT('Ctrl Pts',(17.1844819308442,21.2505245848913,-9.08401600172335));
#49062=CARTESIAN_POINT('Ctrl Pts',(17.2523530554692,21.3003527195435,-9.08818571604372));
#49063=CARTESIAN_POINT('Ctrl Pts',(17.3225130695873,21.3467211066228,-9.0923554303641));
#49064=CARTESIAN_POINT('Ctrl Pts',(17.392670587111,21.3930878437159,-9.09652499630815));
#49065=CARTESIAN_POINT('Ctrl Pts',(17.4651164479275,21.4359948250818,-9.10069456225219));
#49066=CARTESIAN_POINT('Ctrl Pts',(17.5394714392698,21.475222055718,-9.10486412819624));
#49067=CARTESIAN_POINT('Ctrl Pts',(17.6164406603809,21.5158284673913,-9.10918029093516));
#49068=CARTESIAN_POINT('Ctrl Pts',(17.6954552934395,21.5524913076844,-9.11349645367408));
#49069=CARTESIAN_POINT('Ctrl Pts',(17.7760690203245,21.585019426664,-9.117812616413));
#49070=CARTESIAN_POINT('Ctrl Pts',(17.8540567635352,21.6164879455891,-9.12198818060468));
#49071=CARTESIAN_POINT('Ctrl Pts',(17.9335405590285,21.6440868736177,-9.12616374479636));
#49072=CARTESIAN_POINT('Ctrl Pts',(18.0140996850997,21.6676936187906,-9.13033930898804));
#49073=CARTESIAN_POINT('Ctrl Pts',(18.0987276611176,21.6924926845425,-9.13472577100058));
#49074=CARTESIAN_POINT('Ctrl Pts',(18.1845418843916,21.7128855434687,-9.13911223301312));
#49075=CARTESIAN_POINT('Ctrl Pts',(18.2710433987723,21.7287909336122,-9.14349869502566));
#49076=CARTESIAN_POINT('Ctrl Pts',(18.3575449131529,21.7446963237556,-9.1478851570382));
#49077=CARTESIAN_POINT('Ctrl Pts',(18.4447331334585,21.756114245197,-9.15227161905073));
#49078=CARTESIAN_POINT('Ctrl Pts',(18.5321062576865,21.7630264334083,-9.15665808106327));
#49079=CARTESIAN_POINT('Ctrl Pts',(18.615438042294,21.7696189066005,-9.1608416525087));
#49080=CARTESIAN_POINT('Ctrl Pts',(18.6992481014932,21.7721377831227,-9.16502522395414));
#49081=CARTESIAN_POINT('Ctrl Pts',(18.7831042309699,21.770529014194,-9.16920879539957));
#49082=CARTESIAN_POINT('Ctrl Pts',(18.8668503855921,21.7689223551186,-9.17338688021374));
#49083=CARTESIAN_POINT('Ctrl Pts',(18.950642035037,21.763198805827,-9.17756496502792));
#49084=CARTESIAN_POINT('Ctrl Pts',(19.0340424954892,21.7533560924663,-9.18174304984209));
#49085=CARTESIAN_POINT('Ctrl Pts',(19.1173586063393,21.7435233338343,-9.18591690902262));
#49086=CARTESIAN_POINT('Ctrl Pts',(19.2002838596484,21.7295797379332,-9.19009076820316));
#49087=CARTESIAN_POINT('Ctrl Pts',(19.2823835816277,21.7115750233499,-9.19426462738369));
#49088=CARTESIAN_POINT('Ctrl Pts',(19.3644249023172,21.6935831163441,-9.19843551750716));
#49089=CARTESIAN_POINT('Ctrl Pts',(19.4456414103873,21.6715359284697,-9.20260640763063));
#49090=CARTESIAN_POINT('Ctrl Pts',(19.5256069084361,21.6455345556217,-9.2067772977541));
#49091=CARTESIAN_POINT('Ctrl Pts',(19.6055553058999,21.6195387431554,-9.21094729593464));
#49092=CARTESIAN_POINT('Ctrl Pts',(19.6842527850321,21.5895905593686,-9.21511729411517));
#49093=CARTESIAN_POINT('Ctrl Pts',(19.7612877178885,21.5558411342083,-9.21928729229571));
#49094=CARTESIAN_POINT('Ctrl Pts',(19.8383126150256,21.5220961057515,-9.22345674723009));
#49095=CARTESIAN_POINT('Ctrl Pts',(19.9136749774785,21.4845510104536,-9.22762620216447));
#49096=CARTESIAN_POINT('Ctrl Pts',(19.9869841268054,21.4434047074788,-9.23179565709885));
#49097=CARTESIAN_POINT('Ctrl Pts',(20.0603319682225,21.4022366877541,-9.23596731264431));
#49098=CARTESIAN_POINT('Ctrl Pts',(20.1316240343934,21.3574638959363,-9.24013896818976));
#49099=CARTESIAN_POINT('Ctrl Pts',(20.2004959726192,21.3093301842874,-9.24431062373522));
#49100=CARTESIAN_POINT('Ctrl Pts',(20.2320270447196,21.287293523616,-9.24622049842687));
#49101=CARTESIAN_POINT('Ctrl Pts',(20.2630512644551,21.2645530061891,-9.24813037311851));
#49102=CARTESIAN_POINT('Ctrl Pts',(20.2935358855687,21.2411349269503,-9.25004024781016));
#49103=CARTESIAN_POINT('Ctrl Pts',(20.2935358855687,21.2411349269503,-8.4501343042798));
#49104=CARTESIAN_POINT('Ctrl Pts',(20.3602160797285,21.1899116539213,-8.45430378913366));
#49105=CARTESIAN_POINT('Ctrl Pts',(20.4243834024368,21.1353894300217,-8.45847327398753));
#49106=CARTESIAN_POINT('Ctrl Pts',(20.4857033606994,21.0778517177629,-8.46264275884139));
#49107=CARTESIAN_POINT('Ctrl Pts',(20.5470302049274,21.0203075442685,-8.46681271191031));
#49108=CARTESIAN_POINT('Ctrl Pts',(20.6055087152443,20.9597475257638,-8.47098266497924));
#49109=CARTESIAN_POINT('Ctrl Pts',(20.6608405095296,20.8964927026943,-8.47515261804817));
#49110=CARTESIAN_POINT('Ctrl Pts',(20.7162314101251,20.8331703098081,-8.47932702552786));
#49111=CARTESIAN_POINT('Ctrl Pts',(20.7684685805212,20.7671477122994,-8.48350143300755));
#49112=CARTESIAN_POINT('Ctrl Pts',(20.8172936334879,20.6987794314578,-8.48767584048725));
#49113=CARTESIAN_POINT('Ctrl Pts',(20.8661466856643,20.630371944149,-8.49185264182222));
#49114=CARTESIAN_POINT('Ctrl Pts',(20.9115834762052,20.5596164825491,-8.49602944315718));
#49115=CARTESIAN_POINT('Ctrl Pts',(20.9533900358615,20.4868949285575,-8.50020624449215));
#49116=CARTESIAN_POINT('Ctrl Pts',(20.9952677481271,20.4140496062299,-8.50439015452768));
#49117=CARTESIAN_POINT('Ctrl Pts',(21.0335026827121,20.3392319193496,-8.50857406456321));
#49118=CARTESIAN_POINT('Ctrl Pts',(21.0679278688898,20.2628463304207,-8.51275797459873));
#49119=CARTESIAN_POINT('Ctrl Pts',(21.0899269822391,20.2140327896478,-8.51543166561785));
#49120=CARTESIAN_POINT('Ctrl Pts',(21.1103712764704,20.1645793566965,-8.51810535663697));
#49121=CARTESIAN_POINT('Ctrl Pts',(21.1292278697972,20.1145947386671,-8.52077904765609));
#49122=CARTESIAN_POINT('Ctrl Pts',(21.1587406102023,20.0363630543649,-8.52496368204914));
#49123=CARTESIAN_POINT('Ctrl Pts',(21.1844714983966,19.9565383690801,-8.52914831644219));
#49124=CARTESIAN_POINT('Ctrl Pts',(21.2062483053234,19.8755211184195,-8.53333295083523));
#49125=CARTESIAN_POINT('Ctrl Pts',(21.227994115661,19.7946191857873,-8.53751162891918));
#49126=CARTESIAN_POINT('Ctrl Pts',(21.2457969056055,19.7125284999513,-8.54169030700313));
#49127=CARTESIAN_POINT('Ctrl Pts',(21.2595330219156,19.6296680728378,-8.54586898508708));
#49128=CARTESIAN_POINT('Ctrl Pts',(21.2735153482386,19.5453224321191,-8.55012256297251));
#49129=CARTESIAN_POINT('Ctrl Pts',(21.2832836065124,19.4601796345795,-8.55437614085795));
#49130=CARTESIAN_POINT('Ctrl Pts',(21.288760950006,19.3746963295992,-8.55862971874338));
#49131=CARTESIAN_POINT('Ctrl Pts',(21.2941321045079,19.290870285293,-8.56280083272133));
#49132=CARTESIAN_POINT('Ctrl Pts',(21.2953772042646,19.206717298763,-8.56697194669928));
#49133=CARTESIAN_POINT('Ctrl Pts',(21.2924758541409,19.1226750104567,-8.57114306067723));
#49134=CARTESIAN_POINT('Ctrl Pts',(21.2895754775933,19.0386609233517,-8.57531277499761));
#49135=CARTESIAN_POINT('Ctrl Pts',(21.2825314303294,18.9547579200745,-8.57948248931798));
#49136=CARTESIAN_POINT('Ctrl Pts',(21.2713754270314,18.8714032651847,-8.58365220363836));
#49137=CARTESIAN_POINT('Ctrl Pts',(21.2602198207119,18.7880515764114,-8.5878217695824));
#49138=CARTESIAN_POINT('Ctrl Pts',(21.2449526111524,18.7052486530836,-8.59199133552644));
#49139=CARTESIAN_POINT('Ctrl Pts',(21.2256571796748,18.6234248992895,-8.59616090147048));
#49140=CARTESIAN_POINT('Ctrl Pts',(21.2056833446299,18.5387243232523,-8.6004770642094));
#49141=CARTESIAN_POINT('Ctrl Pts',(21.181392873751,18.4550735664103,-8.60479322694832));
#49142=CARTESIAN_POINT('Ctrl Pts',(21.1529349892686,18.3729346578625,-8.60910938968724));
#49143=CARTESIAN_POINT('Ctrl Pts',(21.12540411738,18.2934714156211,-8.61328495387892));
#49144=CARTESIAN_POINT('Ctrl Pts',(21.0939733891636,18.2154234566592,-8.61746051807061));
#49145=CARTESIAN_POINT('Ctrl Pts',(21.0588268816571,18.1391884632433,-8.62163608226229));
#49146=CARTESIAN_POINT('Ctrl Pts',(21.0219052076092,18.0591030215416,-8.62602254427483));
#49147=CARTESIAN_POINT('Ctrl Pts',(20.9808827929501,17.981019021216,-8.63040900628737));
#49148=CARTESIAN_POINT('Ctrl Pts',(20.936026279751,17.905365953536,-8.63479546829991));
#49149=CARTESIAN_POINT('Ctrl Pts',(20.8911697665519,17.829712885856,-8.63918193031245));
#49150=CARTESIAN_POINT('Ctrl Pts',(20.842479539431,17.7564911918506,-8.64356839232499));
#49151=CARTESIAN_POINT('Ctrl Pts',(20.790271595083,17.6860911085397,-8.64795485433753));
#49152=CARTESIAN_POINT('Ctrl Pts',(20.7404658156452,17.6189302374198,-8.65213948873058));
#49153=CARTESIAN_POINT('Ctrl Pts',(20.6872735296056,17.5540870442999,-8.65632412312363));
#49154=CARTESIAN_POINT('Ctrl Pts',(20.6309382156176,17.49192309476,-8.66050875751668));
#49155=CARTESIAN_POINT('Ctrl Pts',(20.574683087976,17.4298476279077,-8.66468743560064));
#49156=CARTESIAN_POINT('Ctrl Pts',(20.515294124861,17.370444167647,-8.66886611368458));
#49157=CARTESIAN_POINT('Ctrl Pts',(20.4530567178379,17.3140434899934,-8.67304479176854));
#49158=CARTESIAN_POINT('Ctrl Pts',(20.3897037500234,17.2566318707275,-8.67729836965397));
#49159=CARTESIAN_POINT('Ctrl Pts',(20.3233995043663,17.2023321299324,-8.68155194753941));
#49160=CARTESIAN_POINT('Ctrl Pts',(20.2544863550513,17.1514560591959,-8.68580552542484));
#49161=CARTESIAN_POINT('Ctrl Pts',(20.1869092216086,17.1015663203671,-8.68997663940279));
#49162=CARTESIAN_POINT('Ctrl Pts',(20.1168238263188,17.054968972992,-8.69414775338075));
#49163=CARTESIAN_POINT('Ctrl Pts',(20.0445871160401,17.0119180526252,-8.6983188673587));
#49164=CARTESIAN_POINT('Ctrl Pts',(19.9723746454872,16.9688815784106,-8.70248858167907));
#49165=CARTESIAN_POINT('Ctrl Pts',(19.8980126884862,16.9293894030873,-8.70665829599945));
#49166=CARTESIAN_POINT('Ctrl Pts',(19.8218860818892,16.8936515426394,-8.71082801031982));
#49167=CARTESIAN_POINT('Ctrl Pts',(19.7457621842035,16.8579149538979,-8.71499757626386));
#49168=CARTESIAN_POINT('Ctrl Pts',(19.6678741785624,16.8259326091334,-8.71916714220791));
#49169=CARTESIAN_POINT('Ctrl Pts',(19.5886290994192,16.7978673674193,-8.72333670815195));
#49170=CARTESIAN_POINT('Ctrl Pts',(19.5065978610527,16.7688153864287,-8.72765287089087));
#49171=CARTESIAN_POINT('Ctrl Pts',(19.4231128413864,16.7439612602711,-8.73196903362979));
#49172=CARTESIAN_POINT('Ctrl Pts',(19.338643304938,16.7234296042536,-8.7362851963687));
#49173=CARTESIAN_POINT('Ctrl Pts',(19.2569253547548,16.7035667647714,-8.74046076056038));
#49174=CARTESIAN_POINT('Ctrl Pts',(19.1742865155725,16.6877491532913,-8.74463632475206));
#49175=CARTESIAN_POINT('Ctrl Pts',(19.0911608126521,16.676037248024,-8.74881188894374));
#49176=CARTESIAN_POINT('Ctrl Pts',(19.0038366280897,16.663733802264,-8.75319835095627));
#49177=CARTESIAN_POINT('Ctrl Pts',(18.9159756858735,16.6559617726585,-8.75758481296882));
#49178=CARTESIAN_POINT('Ctrl Pts',(18.8280834484886,16.6527294309005,-8.76197127498135));
#49179=CARTESIAN_POINT('Ctrl Pts',(18.7401912111037,16.6494970891426,-8.76635773699389));
#49180=CARTESIAN_POINT('Ctrl Pts',(18.6522682575722,16.65080435055,-8.77074419900643));
#49181=CARTESIAN_POINT('Ctrl Pts',(18.5648137584889,16.6565967398073,-8.77513066101897));
#49182=CARTESIAN_POINT('Ctrl Pts',(18.481383170547,16.6621226126484,-8.77931529541201));
#49183=CARTESIAN_POINT('Ctrl Pts',(18.3980683312293,16.6717505167586,-8.78349992980506));
#49184=CARTESIAN_POINT('Ctrl Pts',(18.3153050503466,16.6854714337124,-8.78768456419811));
#49185=CARTESIAN_POINT('Ctrl Pts',(18.2326595727499,16.6991728206392,-8.79186324228206));
#49186=CARTESIAN_POINT('Ctrl Pts',(18.1505645441385,16.7169555737484,-8.79604192036602));
#49187=CARTESIAN_POINT('Ctrl Pts',(18.0694525718368,16.7387587666812,-8.80022059844998));
#49188=CARTESIAN_POINT('Ctrl Pts',(17.9868867257259,16.7609527661775,-8.80447417633541));
#49189=CARTESIAN_POINT('Ctrl Pts',(17.9053400062228,16.7873127240844,-8.80872775422085));
#49190=CARTESIAN_POINT('Ctrl Pts',(17.8252599013632,16.8177195247674,-8.81298133210628));
#49191=CARTESIAN_POINT('Ctrl Pts',(17.7467323055997,16.8475368302852,-8.81715244608423));
#49192=CARTESIAN_POINT('Ctrl Pts',(17.6696154154516,16.8812452961241,-8.82132356006219));
#49193=CARTESIAN_POINT('Ctrl Pts',(17.5943160431827,16.918682291092,-8.82549467404014));
#49194=CARTESIAN_POINT('Ctrl Pts',(17.5190419383454,16.9561067237147,-8.82966438836052));
#49195=CARTESIAN_POINT('Ctrl Pts',(17.4455845517321,16.9972569960436,-8.83383410268089));
#49196=CARTESIAN_POINT('Ctrl Pts',(17.3743287784388,17.0419231988567,-8.83800381700126));
#49197=CARTESIAN_POINT('Ctrl Pts',(17.3030755407317,17.0865878122545,-8.8421733829453));
#49198=CARTESIAN_POINT('Ctrl Pts',(17.23402414991,17.1347678623266,-8.84634294888934));
#49199=CARTESIAN_POINT('Ctrl Pts',(17.1675318647109,17.18620925004,-8.85051251483338));
#49200=CARTESIAN_POINT('Ctrl Pts',(17.0987017927912,17.2394592534855,-8.8548286775723));
#49201=CARTESIAN_POINT('Ctrl Pts',(17.0326145482166,17.2962038761407,-8.85914484031122));
#49202=CARTESIAN_POINT('Ctrl Pts',(16.9696289167229,17.3561159927113,-8.86346100305014));
#49203=CARTESIAN_POINT('Ctrl Pts',(16.9086950355501,17.4140764783862,-8.86763656724182));
#49204=CARTESIAN_POINT('Ctrl Pts',(16.8506640912069,17.4750008911692,-8.87181213143349));
#49205=CARTESIAN_POINT('Ctrl Pts',(16.795821865939,17.5385570202103,-8.87598769562517));
#49206=CARTESIAN_POINT('Ctrl Pts',(16.738209690248,17.6053232182388,-8.88037415763771));
#49207=CARTESIAN_POINT('Ctrl Pts',(16.684117181693,17.6749935141298,-8.88476061965025));
#49208=CARTESIAN_POINT('Ctrl Pts',(16.6338248927154,17.747147371235,-8.88914708166279));
#49209=CARTESIAN_POINT('Ctrl Pts',(16.5835326037379,17.8193012283402,-8.89353354367533));
#49210=CARTESIAN_POINT('Ctrl Pts',(16.5370407765469,17.8939381139568,-8.89792000568786));
#49211=CARTESIAN_POINT('Ctrl Pts',(16.4945737975988,17.9706088181549,-8.9023064677004));
#49212=CARTESIAN_POINT('Ctrl Pts',(16.4520961746313,18.0472987392713,-8.90669402914567));
#49213=CARTESIAN_POINT('Ctrl Pts',(16.4134992022808,18.1262856298358,-8.91108159059094));
#49214=CARTESIAN_POINT('Ctrl Pts',(16.3790251742671,18.2071605854698,-8.91546915203621));
#49215=CARTESIAN_POINT('Ctrl Pts',(16.3446454932945,18.2878142059945,-8.91984470579152));
#49216=CARTESIAN_POINT('Ctrl Pts',(16.3143664333072,18.3703452363826,-8.92422025954683));
#49217=CARTESIAN_POINT('Ctrl Pts',(16.2883841141658,18.4543211123896,-8.92859581330214));
#49218=CARTESIAN_POINT('Ctrl Pts',(16.2624439986578,18.5381605845957,-8.93296425975245));
#49219=CARTESIAN_POINT('Ctrl Pts',(16.2407868563187,18.6234398583863,-8.93733270620276));
#49220=CARTESIAN_POINT('Ctrl Pts',(16.2235607960525,18.7097066694205,-8.94170115265307));
#49221=CARTESIAN_POINT('Ctrl Pts',(16.2063704951607,18.7957944002037,-8.94606053069715));
#49222=CARTESIAN_POINT('Ctrl Pts',(16.193593030381,18.8828651985171,-8.95041990874122));
#49223=CARTESIAN_POINT('Ctrl Pts',(16.1853263642748,18.9704533339262,-8.9547792867853));
#49224=CARTESIAN_POINT('Ctrl Pts',(16.1777850503447,19.0503561166421,-8.9587561545997));
#49225=CARTESIAN_POINT('Ctrl Pts',(16.1739971536887,19.1306890276032,-8.96273302241411));
#49226=CARTESIAN_POINT('Ctrl Pts',(16.174000001606,19.21109067809,-8.96670989022851));
#49227=CARTESIAN_POINT('Origin',(18.734,19.211,1.76670989022852));
#49228=CARTESIAN_POINT('',(20.2947700725713,21.2427129721482,-7.6502134855505));
#49229=CARTESIAN_POINT('',(20.2923705327637,21.2395869487749,-7.71658757605019));
#49230=CARTESIAN_POINT('',(20.2935358855687,21.2411349269503,1.76670989022852));
#49231=CARTESIAN_POINT('',(16.1740010826189,19.2133543592346,-8.23329012251325));
#49232=CARTESIAN_POINT('Ctrl Pts',(20.2923705327634,21.239586948775,-7.71658757605017));
#49233=CARTESIAN_POINT('Ctrl Pts',(20.5052428186746,21.0789785260141,-7.72982826792657));
#49234=CARTESIAN_POINT('Ctrl Pts',(21.2942513389235,20.2707707462439,-7.78546089536344));
#49235=CARTESIAN_POINT('Ctrl Pts',(21.5288884363408,18.0482922871128,-7.88348545836079));
#49236=CARTESIAN_POINT('Ctrl Pts',(19.2691669172862,16.2315894932317,-8.01066126504223));
#49237=CARTESIAN_POINT('Ctrl Pts',(16.7471750875427,17.0720885005601,-8.12726281551246));
#49238=CARTESIAN_POINT('Ctrl Pts',(16.180230297531,18.573538664413,-8.20147243042223));
#49239=CARTESIAN_POINT('Ctrl Pts',(16.1744184457826,19.2133537191784,-8.23329010977151));
#49240=CARTESIAN_POINT('Ctrl Pts',(16.1740010826189,19.2133543592346,-8.23329012251325));
#49241=CARTESIAN_POINT('Ctrl Pts',(16.1741014808466,19.322521792358,-8.23871812867197));
#49242=CARTESIAN_POINT('Ctrl Pts',(16.1811885397039,19.4313771444072,-8.24414613483068));
#49243=CARTESIAN_POINT('Ctrl Pts',(16.1951208364047,19.5391654958424,-8.2495741409894));
#49244=CARTESIAN_POINT('Ctrl Pts',(16.2083299266963,19.6413587018203,-8.25472038679463));
#49245=CARTESIAN_POINT('Ctrl Pts',(16.2276915596972,19.7425933354954,-8.25986663259986));
#49246=CARTESIAN_POINT('Ctrl Pts',(16.253046772176,19.84224565848,-8.2650128784051));
#49247=CARTESIAN_POINT('Ctrl Pts',(16.2736641888712,19.9232772597465,-8.26919751279815));
#49248=CARTESIAN_POINT('Ctrl Pts',(16.2982940662942,20.0034485022604,-8.27338214719119));
#49249=CARTESIAN_POINT('Ctrl Pts',(16.3268482220627,20.0823324956487,-8.27756678158424));
#49250=CARTESIAN_POINT('Ctrl Pts',(16.3553617345248,20.1611042074361,-8.28174545966818));
#49251=CARTESIAN_POINT('Ctrl Pts',(16.3877882750863,20.2385918806365,-8.28592413775212));
#49252=CARTESIAN_POINT('Ctrl Pts',(16.4239892031399,20.314381220789,-8.29010281583606));
#49253=CARTESIAN_POINT('Ctrl Pts',(16.4608390068118,20.3915290303949,-8.2943563937215));
#49254=CARTESIAN_POINT('Ctrl Pts',(16.5015997218018,20.4669165555969,-8.29860997160693));
#49255=CARTESIAN_POINT('Ctrl Pts',(16.5460727818105,20.5401254598065,-8.30286354949237));
#49256=CARTESIAN_POINT('Ctrl Pts',(16.589683644769,20.6119150665525,-8.30703466347032));
#49257=CARTESIAN_POINT('Ctrl Pts',(16.6368639453122,20.6816093608382,-8.31120577744827));
#49258=CARTESIAN_POINT('Ctrl Pts',(16.6873797310322,20.7488379221005,-8.31537689142623));
#49259=CARTESIAN_POINT('Ctrl Pts',(16.7378785656925,20.8160439241698,-8.3195466057466));
#49260=CARTESIAN_POINT('Ctrl Pts',(16.7917103865529,20.880785468974,-8.32371632006697));
#49261=CARTESIAN_POINT('Ctrl Pts',(16.8485987415145,20.9427222913912,-8.32788603438734));
#49262=CARTESIAN_POINT('Ctrl Pts',(16.9054850721443,21.0046569098304,-8.33205560033138));
#49263=CARTESIAN_POINT('Ctrl Pts',(16.9654274088046,21.0637866660879,-8.33622516627543));
#49264=CARTESIAN_POINT('Ctrl Pts',(17.0281108772059,21.1198065121255,-8.34039473221947));
#49265=CARTESIAN_POINT('Ctrl Pts',(17.0929982190277,21.1777959468418,-8.34471089495839));
#49266=CARTESIAN_POINT('Ctrl Pts',(17.160822642128,21.2324523620817,-8.34902705769731));
#49267=CARTESIAN_POINT('Ctrl Pts',(17.2311971876102,21.2834824986169,-8.35334322043623));
#49268=CARTESIAN_POINT('Ctrl Pts',(17.2992792896755,21.3328503338219,-8.35751878462791));
#49269=CARTESIAN_POINT('Ctrl Pts',(17.3697475047295,21.3788242964685,-8.36169434881959));
#49270=CARTESIAN_POINT('Ctrl Pts',(17.4422231594135,21.4211838371783,-8.36586991301127));
#49271=CARTESIAN_POINT('Ctrl Pts',(17.5183593871211,21.4656828575892,-8.37025637502381));
#49272=CARTESIAN_POINT('Ctrl Pts',(17.5967106568092,21.5061924632349,-8.37464283703636));
#49273=CARTESIAN_POINT('Ctrl Pts',(17.6768123961765,21.5425133219267,-8.3790292990489));
#49274=CARTESIAN_POINT('Ctrl Pts',(17.7569141355438,21.5788341806186,-8.38341576106144));
#49275=CARTESIAN_POINT('Ctrl Pts',(17.8387657767031,21.6109661511407,-8.38780222307398));
#49276=CARTESIAN_POINT('Ctrl Pts',(17.921884774769,21.638770347654,-8.39218868508652));
#49277=CARTESIAN_POINT('Ctrl Pts',(18.0011804710188,21.6652956086952,-8.3963733789285));
#49278=CARTESIAN_POINT('Ctrl Pts',(18.0819246518068,21.6879812201688,-8.40055807277047));
#49279=CARTESIAN_POINT('Ctrl Pts',(18.1637106209527,21.7066702554917,-8.40474276661245));
#49280=CARTESIAN_POINT('Ctrl Pts',(18.2453798597931,21.7253326165961,-8.40892148778459));
#49281=CARTESIAN_POINT('Ctrl Pts',(18.3280874888049,21.7400096304256,-8.41310020895674));
#49282=CARTESIAN_POINT('Ctrl Pts',(18.4114100949888,21.7505936196929,-8.41727893012888));
#49283=CARTESIAN_POINT('Ctrl Pts',(18.4946347461077,21.7611651662942,-8.4214527387458));
#49284=CARTESIAN_POINT('Ctrl Pts',(18.5784724833061,21.7676531957144,-8.42562654736272));
#49285=CARTESIAN_POINT('Ctrl Pts',(18.6624895012298,21.7700010255109,-8.42980035597964));
#49286=CARTESIAN_POINT('Ctrl Pts',(18.7464521744715,21.7723473366619,-8.4339714648542));
#49287=CARTESIAN_POINT('Ctrl Pts',(18.8305934396791,21.7705587522909,-8.43814257372877));
#49288=CARTESIAN_POINT('Ctrl Pts',(18.9144752300251,21.764630492328,-8.44231368260333));
#49289=CARTESIAN_POINT('Ctrl Pts',(18.9983279261209,21.7587042885716,-8.44648334473617));
#49290=CARTESIAN_POINT('Ctrl Pts',(19.0819208676515,21.7486412935491,-8.45065300686901));
#49291=CARTESIAN_POINT('Ctrl Pts',(19.1648182224781,21.7344887872112,-8.45482266900186));
#49292=CARTESIAN_POINT('Ctrl Pts',(19.2477116915592,21.7203369442605,-8.4589921356852));
#49293=CARTESIAN_POINT('Ctrl Pts',(19.3299091855241,21.7020960496226,-8.46316160236854));
#49294=CARTESIAN_POINT('Ctrl Pts',(19.4109835709537,21.6798647684024,-8.46733106905189));
#49295=CARTESIAN_POINT('Ctrl Pts',(19.4921313337435,21.6576133664903,-8.47150430936184));
#49296=CARTESIAN_POINT('Ctrl Pts',(19.5721535125693,21.6313644844617,-8.4756775496718));
#49297=CARTESIAN_POINT('Ctrl Pts',(19.6506371967119,21.601266982913,-8.47985078998176));
#49298=CARTESIAN_POINT('Ctrl Pts',(19.7291549023672,21.5711564345439,-8.48402583932947));
#49299=CARTESIAN_POINT('Ctrl Pts',(19.8061323627767,21.537194127788,-8.48820088867719));
#49300=CARTESIAN_POINT('Ctrl Pts',(19.8811779671275,21.4995765689042,-8.4923759380249));
#49301=CARTESIAN_POINT('Ctrl Pts',(19.9563509512632,21.4618951592911,-8.49655807395541));
#49302=CARTESIAN_POINT('Ctrl Pts',(20.0295851250182,21.4205463259095,-8.50074020988591));
#49303=CARTESIAN_POINT('Ctrl Pts',(20.1005148649941,21.3757718410378,-8.50492234581642));
#49304=CARTESIAN_POINT('Ctrl Pts',(20.1669693717355,21.3338223526038,-8.50884061452122));
#49305=CARTESIAN_POINT('Ctrl Pts',(20.2314010883057,21.2888664569032,-8.51275888322602));
#49306=CARTESIAN_POINT('Ctrl Pts',(20.2935358855687,21.2411349269503,-8.51667715193082));
#49307=CARTESIAN_POINT('',(16.1740010575059,19.2086731074563,-8.16670989022852));
#49308=CARTESIAN_POINT('Ctrl Pts',(16.1740010575059,19.2086731074563,-8.16670989022852));
#49309=CARTESIAN_POINT('Ctrl Pts',(16.1739251952239,19.2921352174732,-8.17086478789788));
#49310=CARTESIAN_POINT('Ctrl Pts',(16.1779353066412,19.375721983002,-8.17501968556725));
#49311=CARTESIAN_POINT('Ctrl Pts',(16.1860403077383,19.458994771335,-8.17917458323661));
#49312=CARTESIAN_POINT('Ctrl Pts',(16.1940671586084,19.5414646248839,-8.18328941845664));
#49313=CARTESIAN_POINT('Ctrl Pts',(16.206110236511,19.6236260477268,-8.18740425367667));
#49314=CARTESIAN_POINT('Ctrl Pts',(16.2221259449782,19.7050533692914,-8.1915190888967));
#49315=CARTESIAN_POINT('Ctrl Pts',(16.238134689091,19.7864452825742,-8.19563213480029));
#49316=CARTESIAN_POINT('Ctrl Pts',(16.2581125446655,19.8671032636359,-8.19974518070388));
#49317=CARTESIAN_POINT('Ctrl Pts',(16.2819644394347,19.9466096857188,-8.20385822660747));
#49318=CARTESIAN_POINT('Ctrl Pts',(16.3058135810413,20.0261069305807,-8.20797079775279));
#49319=CARTESIAN_POINT('Ctrl Pts',(16.3335357367831,20.1044524267965,-8.21208336889812));
#49320=CARTESIAN_POINT('Ctrl Pts',(16.364985800536,20.1812431255815,-8.21619594004344));
#49321=CARTESIAN_POINT('Ctrl Pts',(16.3969970744394,20.2594041147404,-8.22038189789759));
#49322=CARTESIAN_POINT('Ctrl Pts',(16.4328704281986,20.3359537977656,-8.22456785575174));
#49323=CARTESIAN_POINT('Ctrl Pts',(16.4724022025115,20.4104896424709,-8.22875381360589));
#49324=CARTESIAN_POINT('Ctrl Pts',(16.5112918107484,20.4838147044136,-8.23287177349698));
#49325=CARTESIAN_POINT('Ctrl Pts',(16.5537215594669,20.555190490736,-8.23698973338807));
#49326=CARTESIAN_POINT('Ctrl Pts',(16.5994527799559,20.6242615346786,-8.24110769327916));
#49327=CARTESIAN_POINT('Ctrl Pts',(16.6463167081171,20.6950433858238,-8.24532765011484));
#49328=CARTESIAN_POINT('Ctrl Pts',(16.696647513794,20.7634043768934,-8.24954760695052));
#49329=CARTESIAN_POINT('Ctrl Pts',(16.7501447185242,20.828998214511,-8.2537675637862));
#49330=CARTESIAN_POINT('Ctrl Pts',(16.8036419232544,20.8945920521286,-8.25798752062187));
#49331=CARTESIAN_POINT('Ctrl Pts',(16.8603051182411,20.9574183953713,-8.26220747745755));
#49332=CARTESIAN_POINT('Ctrl Pts',(16.9197953580223,21.0171731691692,-8.26642743429323));
#49333=CARTESIAN_POINT('Ctrl Pts',(16.9787876447051,21.0764277756308,-8.27061206868628));
#49334=CARTESIAN_POINT('Ctrl Pts',(17.0407957809271,21.1328994502154,-8.27479670307933));
#49335=CARTESIAN_POINT('Ctrl Pts',(17.1055265727616,21.1862656268913,-8.27898133747238));
#49336=CARTESIAN_POINT('Ctrl Pts',(17.1701652283259,21.2395558434201,-8.28316001555632));
#49337=CARTESIAN_POINT('Ctrl Pts',(17.237518489892,21.2897490519968,-8.28733869364026));
#49338=CARTESIAN_POINT('Ctrl Pts',(17.3072561423604,21.3365592122281,-8.29151737172421));
#49339=CARTESIAN_POINT('Ctrl Pts',(17.3782437921299,21.3842084109397,-8.29577094960964));
#49340=CARTESIAN_POINT('Ctrl Pts',(17.4517018138302,21.4283517444167,-8.30002452749508));
#49341=CARTESIAN_POINT('Ctrl Pts',(17.5272463530812,21.4687301954946,-8.30427810538051));
#49342=CARTESIAN_POINT('Ctrl Pts',(17.6013263140258,21.5083258315063,-8.30844921935846));
#49343=CARTESIAN_POINT('Ctrl Pts',(17.6774121876524,21.5443010347691,-8.31262033333642));
#49344=CARTESIAN_POINT('Ctrl Pts',(17.75511405008,21.5764560442014,-8.31679144731437));
#49345=CARTESIAN_POINT('Ctrl Pts',(17.8327898388973,21.6086002637098,-8.32096116163474));
#49346=CARTESIAN_POINT('Ctrl Pts',(17.9120801148579,21.6369266595075,-8.32513087595512));
#49347=CARTESIAN_POINT('Ctrl Pts',(17.9925737212262,21.6612830598002,-8.32930059027549));
#49348=CARTESIAN_POINT('Ctrl Pts',(18.0730644632864,21.6856385933875,-8.33347015621953));
#49349=CARTESIAN_POINT('Ctrl Pts',(18.1547580100543,21.7060242799309,-8.33763972216357));
#49350=CARTESIAN_POINT('Ctrl Pts',(18.2372280581078,21.7223378183249,-8.34180928810762));
#49351=CARTESIAN_POINT('Ctrl Pts',(18.3225976513131,21.7392249206038,-8.34612545084654));
#49352=CARTESIAN_POINT('Ctrl Pts',(18.4087988479273,21.7517480910506,-8.35044161358546));
#49353=CARTESIAN_POINT('Ctrl Pts',(18.4953492973482,21.7598518674344,-8.35475777632438));
#49354=CARTESIAN_POINT('Ctrl Pts',(18.5790803749826,21.7676916641549,-8.35893334051605));
#49355=CARTESIAN_POINT('Ctrl Pts',(18.6631378283657,21.7713955951849,-8.36310890470773));
#49356=CARTESIAN_POINT('Ctrl Pts',(18.7470834485355,21.770966566847,-8.36728446889941));
#49357=CARTESIAN_POINT('Ctrl Pts',(18.8352689624184,21.7705158693077,-8.37167093091195));
#49358=CARTESIAN_POINT('Ctrl Pts',(18.9233304658568,21.7655037616187,-8.3760573929245));
#49359=CARTESIAN_POINT('Ctrl Pts',(19.0107666109435,21.7559951361578,-8.38044385493704));
#49360=CARTESIAN_POINT('Ctrl Pts',(19.0982027560302,21.7464865106969,-8.38483031694958));
#49361=CARTESIAN_POINT('Ctrl Pts',(19.1850129820694,21.7324815349687,-8.38921677896212));
#49362=CARTESIAN_POINT('Ctrl Pts',(19.2707112385803,21.7141062794819,-8.39360324097466));
#49363=CARTESIAN_POINT('Ctrl Pts',(19.3524727077245,21.6965751423775,-8.39778819867499));
#49364=CARTESIAN_POINT('Ctrl Pts',(19.4335264843041,21.67500117954,-8.40197315637533));
#49365=CARTESIAN_POINT('Ctrl Pts',(19.5134425416024,21.6494563404622,-8.40615811407565));
#49366=CARTESIAN_POINT('Ctrl Pts',(19.5932250321231,21.6239541954556,-8.41033607729536));
#49367=CARTESIAN_POINT('Ctrl Pts',(19.6718731494994,21.5944945081295,-8.41451404051505));
#49368=CARTESIAN_POINT('Ctrl Pts',(19.7489678548335,21.5612000454546,-8.41869200373476));
#49369=CARTESIAN_POINT('Ctrl Pts',(19.8259879712299,21.5279377950904,-8.42286592478533));
#49370=CARTESIAN_POINT('Ctrl Pts',(19.9014572393319,21.4908483161393,-8.4270398458359));
#49371=CARTESIAN_POINT('Ctrl Pts',(19.9749733693948,21.4501036368272,-8.43121376688647));
#49372=CARTESIAN_POINT('Ctrl Pts',(20.048437496638,21.4093877789209,-8.43538473544669));
#49373=CARTESIAN_POINT('Ctrl Pts',(20.1199508294576,21.3650220797911,-8.43955570400692));
#49374=CARTESIAN_POINT('Ctrl Pts',(20.1891338986603,21.3172253765848,-8.44372667256715));
#49375=CARTESIAN_POINT('Ctrl Pts',(20.2245612917467,21.2927495530598,-8.4458625498047));
#49376=CARTESIAN_POINT('Ctrl Pts',(20.2593780186155,21.2673747687365,-8.44799842704225));
#49377=CARTESIAN_POINT('Ctrl Pts',(20.2935358855687,21.2411349269503,-8.4501343042798));
#49378=CARTESIAN_POINT('Ctrl Pts',(20.2947700725713,21.2427129721481,-7.65021348555051));
#49379=CARTESIAN_POINT('Ctrl Pts',(20.8607342680588,20.7994053635694,-7.6860503928895));
#49380=CARTESIAN_POINT('Ctrl Pts',(21.6914150496944,19.288541779014,-7.76427923578897));
#49381=CARTESIAN_POINT('Ctrl Pts',(20.5479111384388,16.787568886273,-7.88490001424893));
#49382=CARTESIAN_POINT('Ctrl Pts',(17.6781136453352,16.37403049238,-8.01207582093036));
#49383=CARTESIAN_POINT('Ctrl Pts',(16.2739021846612,17.9910560858828,-8.10601244625689));
#49384=CARTESIAN_POINT('Ctrl Pts',(16.1718447049445,19.0247813383249,-8.15755713602294));
#49385=CARTESIAN_POINT('Ctrl Pts',(16.1735502234357,19.2086726976739,-8.16670989022852));
#49386=CARTESIAN_POINT('Origin',(18.734,19.211,1.76670989022852));
#49387=CARTESIAN_POINT('',(20.2935358855687,21.2411349269503,-6.85004462256371));
#49388=CARTESIAN_POINT('',(20.2935358855687,21.2411349269503,-6.91673142315837));
#49389=CARTESIAN_POINT('',(20.2935358855687,21.2411349269503,1.76670989022852));
#49390=CARTESIAN_POINT('',(16.1743644999821,19.2104398261047,-7.43329008494582));
#49391=CARTESIAN_POINT('Ctrl Pts',(20.2935358855687,21.2411349269503,-6.91673142315837));
#49392=CARTESIAN_POINT('Ctrl Pts',(20.3602014276152,21.1899229095753,-6.92090111997205));
#49393=CARTESIAN_POINT('Ctrl Pts',(20.4243665511424,21.1354046687238,-6.92507081678572));
#49394=CARTESIAN_POINT('Ctrl Pts',(20.4856940824214,21.0778604237087,-6.9292405135994));
#49395=CARTESIAN_POINT('Ctrl Pts',(20.5470198554989,21.0203178284319,-6.93341009087187));
#49396=CARTESIAN_POINT('Ctrl Pts',(20.6055078632375,20.9597497169416,-6.93757966814435));
#49397=CARTESIAN_POINT('Ctrl Pts',(20.6608565789692,20.8964743320748,-6.94174924541683));
#49398=CARTESIAN_POINT('Ctrl Pts',(20.7178321177842,20.8313391415135,-6.94604137593132));
#49399=CARTESIAN_POINT('Ctrl Pts',(20.7714805809141,20.7633354172175,-6.95033350644581));
#49400=CARTESIAN_POINT('Ctrl Pts',(20.8215177086802,20.6928467585909,-6.95462563696031));
#49401=CARTESIAN_POINT('Ctrl Pts',(20.8701964139745,20.6242717465336,-6.95880124346946));
#49402=CARTESIAN_POINT('Ctrl Pts',(20.9154571725214,20.5533454368994,-6.96297684997862));
#49403=CARTESIAN_POINT('Ctrl Pts',(20.9570834048037,20.4804487682795,-6.96715245648777));
#49404=CARTESIAN_POINT('Ctrl Pts',(21.0004520625165,20.404500730313,-6.97150284900493));
#49405=CARTESIAN_POINT('Ctrl Pts',(21.0398749854783,20.3264142577069,-6.9758532415221));
#49406=CARTESIAN_POINT('Ctrl Pts',(21.0751622346957,20.2466444326285,-6.98020363403926));
#49407=CARTESIAN_POINT('Ctrl Pts',(21.1104494839132,20.1668746075502,-6.98455402655642));
#49408=CARTESIAN_POINT('Ctrl Pts',(21.1416009291318,20.0854219761771,-6.98890441907358));
#49409=CARTESIAN_POINT('Ctrl Pts',(21.1684852750765,20.0027584514458,-6.99325481159075));
#49410=CARTESIAN_POINT('Ctrl Pts',(21.1943452769569,19.9232445622331,-6.99743944598379));
#49411=CARTESIAN_POINT('Ctrl Pts',(21.2163537449119,19.8423144298574,-7.00162408037684));
#49412=CARTESIAN_POINT('Ctrl Pts',(21.234357169427,19.7603760326907,-7.00580871476988));
#49413=CARTESIAN_POINT('Ctrl Pts',(21.2523349682956,19.6785542646905,-7.00998739285382));
#49414=CARTESIAN_POINT('Ctrl Pts',(21.2663189491972,19.5957275280113,-7.01416607093776));
#49415=CARTESIAN_POINT('Ctrl Pts',(21.2762049862094,19.5123201090075,-7.0183447490217));
#49416=CARTESIAN_POINT('Ctrl Pts',(21.28626822333,19.4274176719618,-7.02259832690713));
#49417=CARTESIAN_POINT('Ctrl Pts',(21.2920850111441,19.3419139888709,-7.02685190479257));
#49418=CARTESIAN_POINT('Ctrl Pts',(21.2935997221946,19.2562687766723,-7.031105482678));
#49419=CARTESIAN_POINT('Ctrl Pts',(21.2950850676157,19.1722839640351,-7.03527659665596));
#49420=CARTESIAN_POINT('Ctrl Pts',(21.2924336475013,19.088163542099,-7.03944771063391));
#49421=CARTESIAN_POINT('Ctrl Pts',(21.2856453456189,19.0043456262704,-7.04361882461186));
#49422=CARTESIAN_POINT('Ctrl Pts',(21.2788593216167,18.9205558363528,-7.04778853893223));
#49423=CARTESIAN_POINT('Ctrl Pts',(21.2679392098804,18.8370688090943,-7.05195825325261));
#49424=CARTESIAN_POINT('Ctrl Pts',(21.252936930744,18.7543198724117,-7.05612796757298));
#49425=CARTESIAN_POINT('Ctrl Pts',(21.2379351854531,18.6715738802915,-7.06029753351703));
#49426=CARTESIAN_POINT('Ctrl Pts',(21.2188516444825,18.5895663790285,-7.06446709946107));
#49427=CARTESIAN_POINT('Ctrl Pts',(21.1957895218785,18.5087234519298,-7.06863666540511));
#49428=CARTESIAN_POINT('Ctrl Pts',(21.1719165634939,18.4250381872448,-7.07295282814404));
#49429=CARTESIAN_POINT('Ctrl Pts',(21.1437801888442,18.3426014204637,-7.07726899088296));
#49430=CARTESIAN_POINT('Ctrl Pts',(21.1115508461405,18.261867778433,-7.08158515362188));
#49431=CARTESIAN_POINT('Ctrl Pts',(21.0803713708855,18.1837640263,-7.08576071781356));
#49432=CARTESIAN_POINT('Ctrl Pts',(21.0453617283798,18.1072545529914,-7.08993628200524));
#49433=CARTESIAN_POINT('Ctrl Pts',(21.006724205865,18.032728094167,-7.09411184619691));
#49434=CARTESIAN_POINT('Ctrl Pts',(20.9661351939398,17.9544374810769,-7.09849830820946));
#49435=CARTESIAN_POINT('Ctrl Pts',(20.9215424772638,17.8783359749763,-7.102884770222));
#49436=CARTESIAN_POINT('Ctrl Pts',(20.8732322919594,17.8048402647501,-7.10727123223455));
#49437=CARTESIAN_POINT('Ctrl Pts',(20.8249221066551,17.731344554524,-7.11165769424709));
#49438=CARTESIAN_POINT('Ctrl Pts',(20.7728948573422,17.6604550629257,-7.11604415625964));
#49439=CARTESIAN_POINT('Ctrl Pts',(20.7174842649081,17.5925469821889,-7.12043061827219));
#49440=CARTESIAN_POINT('Ctrl Pts',(20.6646231959702,17.5277634529108,-7.12461525266524));
#49441=CARTESIAN_POINT('Ctrl Pts',(20.6084865283937,17.4654518685825,-7.12879988705828));
#49442=CARTESIAN_POINT('Ctrl Pts',(20.549334215637,17.4059621373673,-7.13298452145133));
#49443=CARTESIAN_POINT('Ctrl Pts',(20.4902660988757,17.3465570824209,-7.13716319953529));
#49444=CARTESIAN_POINT('Ctrl Pts',(20.4281911845783,17.2899662258643,-7.14134187761925));
#49445=CARTESIAN_POINT('Ctrl Pts',(20.3634098690371,17.2365067792762,-7.1455205557032));
#49446=CARTESIAN_POINT('Ctrl Pts',(20.2974673949727,17.1820891105288,-7.14977413358864));
#49447=CARTESIAN_POINT('Ctrl Pts',(20.2287208456641,17.1309165905524,-7.15402771147407));
#49448=CARTESIAN_POINT('Ctrl Pts',(20.1575266602167,17.083284829294,-7.15828128935951));
#49449=CARTESIAN_POINT('Ctrl Pts',(20.0877127129782,17.0365765026734,-7.16245240333746));
#49450=CARTESIAN_POINT('Ctrl Pts',(20.0155455870556,16.9932731384694,-7.1666235173154));
#49451=CARTESIAN_POINT('Ctrl Pts',(19.9413936052579,16.9536119779749,-7.17079463129335));
#49452=CARTESIAN_POINT('Ctrl Pts',(19.8672665058736,16.9139641261658,-7.17496434561373));
#49453=CARTESIAN_POINT('Ctrl Pts',(19.7911562786912,16.8779562675926,-7.1791340599341));
#49454=CARTESIAN_POINT('Ctrl Pts',(19.7134570690884,16.8457803802157,-7.18330377425448));
#49455=CARTESIAN_POINT('Ctrl Pts',(19.6357606243572,16.8136056377949,-7.18747334019852));
#49456=CARTESIAN_POINT('Ctrl Pts',(19.5564757349841,16.7852627706771,-7.19164290614255));
#49457=CARTESIAN_POINT('Ctrl Pts',(19.476016537407,16.7608956229959,-7.19581247208659));
#49458=CARTESIAN_POINT('Ctrl Pts',(19.3927284937001,16.7356717564624,-7.20012863482551));
#49459=CARTESIAN_POINT('Ctrl Pts',(19.3081825327891,16.7147085365433,-7.20444479756443));
#49460=CARTESIAN_POINT('Ctrl Pts',(19.2228531842896,16.6981087241566,-7.20876096030335));
#49461=CARTESIAN_POINT('Ctrl Pts',(19.1403034303422,16.6820496489123,-7.21293652449504));
#49462=CARTESIAN_POINT('Ctrl Pts',(19.0570210156983,16.6700740910786,-7.21711208868672));
#49463=CARTESIAN_POINT('Ctrl Pts',(18.9734422997759,16.6622223743374,-7.2212876528784));
#49464=CARTESIAN_POINT('Ctrl Pts',(18.8856422216019,16.6539740860494,-7.22567411489094));
#49465=CARTESIAN_POINT('Ctrl Pts',(18.7975157065269,16.6502772019506,-7.23006057690348));
#49466=CARTESIAN_POINT('Ctrl Pts',(18.7095680581451,16.6511165885499,-7.23444703891601));
#49467=CARTESIAN_POINT('Ctrl Pts',(18.6216204097632,16.6519559751493,-7.23883350092855));
#49468=CARTESIAN_POINT('Ctrl Pts',(18.5338522025563,16.6573315210541,-7.24321996294108));
#49469=CARTESIAN_POINT('Ctrl Pts',(18.4467595506041,16.6671657042506,-7.24760642495362));
#49470=CARTESIAN_POINT('Ctrl Pts',(18.3636741606704,16.6765474021004,-7.25179105934667));
#49471=CARTESIAN_POINT('Ctrl Pts',(18.2808942658293,16.6900213769478,-7.25597569373972));
#49472=CARTESIAN_POINT('Ctrl Pts',(18.1988547913486,16.7075584477249,-7.26016032813276));
#49473=CARTESIAN_POINT('Ctrl Pts',(18.116932089905,16.7250705566525,-7.26433900621672));
#49474=CARTESIAN_POINT('Ctrl Pts',(18.0357481614728,16.7466341786849,-7.26851768430067));
#49475=CARTESIAN_POINT('Ctrl Pts',(17.9557323296054,16.77216842869,-7.27269636238463));
#49476=CARTESIAN_POINT('Ctrl Pts',(17.8742822714585,16.7981603617751,-7.27694994027006));
#49477=CARTESIAN_POINT('Ctrl Pts',(17.7940430771259,16.8282666158667,-7.2812035181555));
#49478=CARTESIAN_POINT('Ctrl Pts',(17.7154562415191,16.8623474901426,-7.28545709604093));
#49479=CARTESIAN_POINT('Ctrl Pts',(17.63839296507,16.8957676401673,-7.28962821001889));
#49480=CARTESIAN_POINT('Ctrl Pts',(17.5629189921761,16.9330094826425,-7.29379932399685));
#49481=CARTESIAN_POINT('Ctrl Pts',(17.4894331713713,16.9738917305867,-7.2979704379748));
#49482=CARTESIAN_POINT('Ctrl Pts',(17.4159720094435,17.0147602600978,-7.30214015229517));
#49483=CARTESIAN_POINT('Ctrl Pts',(17.3444980763215,17.059266545551,-7.30630986661554));
#49484=CARTESIAN_POINT('Ctrl Pts',(17.2753861385062,17.1071830870871,-7.31047958093591));
#49485=CARTESIAN_POINT('Ctrl Pts',(17.2062766599905,17.155097923547,-7.31464914687994));
#49486=CARTESIAN_POINT('Ctrl Pts',(17.1395293872397,17.2064225119979,-7.31881871282397));
#49487=CARTESIAN_POINT('Ctrl Pts',(17.0754894346056,17.2608864893358,-7.322988278768));
#49488=CARTESIAN_POINT('Ctrl Pts',(17.0091979162384,17.3172653529285,-7.32730444150692));
#49489=CARTESIAN_POINT('Ctrl Pts',(16.9458080406878,17.377008133023,-7.33162060424584));
#49490=CARTESIAN_POINT('Ctrl Pts',(16.885663067504,17.4397714478444,-7.33593676698476));
#49491=CARTESIAN_POINT('Ctrl Pts',(16.8274773104956,17.5004902542869,-7.34011233117644));
#49492=CARTESIAN_POINT('Ctrl Pts',(16.7723285700598,17.5640354429535,-7.34428789536812));
#49493=CARTESIAN_POINT('Ctrl Pts',(16.7204869451086,17.6300619310733,-7.3484634595598));
#49494=CARTESIAN_POINT('Ctrl Pts',(16.6660269229228,17.6994232601449,-7.35284992157234));
#49495=CARTESIAN_POINT('Ctrl Pts',(16.6152172172816,17.7715226597539,-7.35723638358488));
#49496=CARTESIAN_POINT('Ctrl Pts',(16.5683186145658,17.845927058072,-7.36162284559743));
#49497=CARTESIAN_POINT('Ctrl Pts',(16.52142001185,17.9203314563902,-7.36600930760997));
#49498=CARTESIAN_POINT('Ctrl Pts',(16.4784327293519,17.9970403100744,-7.37039576962251));
#49499=CARTESIAN_POINT('Ctrl Pts',(16.4395601204679,18.0755945044995,-7.37478223163505));
#49500=CARTESIAN_POINT('Ctrl Pts',(16.399796394139,18.1559494788318,-7.37926924910124));
#49501=CARTESIAN_POINT('Ctrl Pts',(16.3642056179145,18.2385006465143,-7.38375626656742));
#49502=CARTESIAN_POINT('Ctrl Pts',(16.3330179090159,18.3228080169392,-7.3882432840336));
#49503=CARTESIAN_POINT('Ctrl Pts',(16.3019356806123,18.4068302499339,-7.39271512587964));
#49504=CARTESIAN_POINT('Ctrl Pts',(16.2752269677052,18.4925965155752,-7.39718696772568));
#49505=CARTESIAN_POINT('Ctrl Pts',(16.2530742870064,18.5796462112197,-7.40165880957171));
#49506=CARTESIAN_POINT('Ctrl Pts',(16.2309688572624,18.6665102326658,-7.40612111312305));
#49507=CARTESIAN_POINT('Ctrl Pts',(16.2134002030055,18.7546518909164,-7.41058341667439));
#49508=CARTESIAN_POINT('Ctrl Pts',(16.2005019648759,18.8435932689479,-7.41504572022573));
#49509=CARTESIAN_POINT('Ctrl Pts',(16.1876417930138,18.9322721563783,-7.41949485428535));
#49510=CARTESIAN_POINT('Ctrl Pts',(16.1794246278368,19.0217457093711,-7.42394398834497));
#49511=CARTESIAN_POINT('Ctrl Pts',(16.1759333991831,19.1115250494595,-7.42839312240459));
#49512=CARTESIAN_POINT('Ctrl Pts',(16.1746525201579,19.1444637323753,-7.43002544244498));
#49513=CARTESIAN_POINT('Ctrl Pts',(16.1740072831437,19.177443453577,-7.43165776248538));
#49514=CARTESIAN_POINT('Ctrl Pts',(16.1740000613162,19.2104396974995,-7.43329008252577));
#49515=CARTESIAN_POINT('Ctrl Pts',(16.1781030359051,19.2104411453813,-7.4332901097715));
#49516=CARTESIAN_POINT('Ctrl Pts',(16.1790025448085,19.6723916862602,-7.4561794192865));
#49517=CARTESIAN_POINT('Ctrl Pts',(16.519742516428,20.9911304253782,-7.52146066436197));
#49518=CARTESIAN_POINT('Ctrl Pts',(18.3750628632639,22.0833380538217,-7.61589315312154));
#49519=CARTESIAN_POINT('Ctrl Pts',(19.8237022835423,21.5931889594048,-7.68743633236609));
#49520=CARTESIAN_POINT('Ctrl Pts',(20.2923705327634,21.239586948775,-7.71658757605017));
#49521=CARTESIAN_POINT('',(16.1738764730989,19.2121301833587,-7.36670989022851));
#49522=CARTESIAN_POINT('Ctrl Pts',(16.1703788196327,19.2121317274208,-7.36670989022851));
#49523=CARTESIAN_POINT('Ctrl Pts',(16.1700290407744,19.2754624167648,-7.36987218932674));
#49524=CARTESIAN_POINT('Ctrl Pts',(16.2008981366677,20.1874206696652,-7.41542642398544));
#49525=CARTESIAN_POINT('Ctrl Pts',(17.2895132664939,21.8712161675055,-7.50337259420461));
#49526=CARTESIAN_POINT('Ctrl Pts',(19.3719151151867,21.8671174429886,-7.59471149354706));
#49527=CARTESIAN_POINT('Ctrl Pts',(20.1912479901919,21.3237995976637,-7.64365845732902));
#49528=CARTESIAN_POINT('Ctrl Pts',(20.2947700725713,21.2427129721481,-7.65021348555051));
#49529=CARTESIAN_POINT('Ctrl Pts',(20.2935358855687,21.2411349269503,-6.8500446225637));
#49530=CARTESIAN_POINT('Ctrl Pts',(20.3601338969406,21.1899747861817,-6.85422899519217));
#49531=CARTESIAN_POINT('Ctrl Pts',(20.4241220194898,21.1356031650462,-6.85841336782063));
#49532=CARTESIAN_POINT('Ctrl Pts',(20.4851928134884,21.0783306429196,-6.86259774044909));
#49533=CARTESIAN_POINT('Ctrl Pts',(20.5090109309219,21.055993883097,-6.86422968056521));
#49534=CARTESIAN_POINT('Ctrl Pts',(20.5323857243709,21.0332162494999,-6.86586162068134));
#49535=CARTESIAN_POINT('Ctrl Pts',(20.5553006227462,21.0100175211999,-6.86749356079746));
#49536=CARTESIAN_POINT('Ctrl Pts',(20.6140591953844,20.9505311495128,-6.87167819519051));
#49537=CARTESIAN_POINT('Ctrl Pts',(20.6700096812721,20.8880523361676,-6.87586282958356));
#49538=CARTESIAN_POINT('Ctrl Pts',(20.7228319806689,20.8228769657355,-6.8800474639766));
#49539=CARTESIAN_POINT('Ctrl Pts',(20.7755790940605,20.7577943643761,-6.88422614206055));
#49540=CARTESIAN_POINT('Ctrl Pts',(20.8252065780214,20.6900231841701,-6.88840482014449));
#49541=CARTESIAN_POINT('Ctrl Pts',(20.8714311671561,20.6198960237255,-6.89258349822843));
#49542=CARTESIAN_POINT('Ctrl Pts',(20.9184842988301,20.5485118843294,-6.89683707611387));
#49543=CARTESIAN_POINT('Ctrl Pts',(20.9620110031542,20.4746868150558,-6.9010906539993));
#49544=CARTESIAN_POINT('Ctrl Pts',(21.0017554861493,20.3988068256412,-6.90534423188474));
#49545=CARTESIAN_POINT('Ctrl Pts',(21.0407294447865,20.324397917889,-6.90951534586269));
#49546=CARTESIAN_POINT('Ctrl Pts',(21.0760663016048,20.2480134825273,-6.91368645984064));
#49547=CARTESIAN_POINT('Ctrl Pts',(21.1075695674518,20.1700451024153,-6.91785757381859));
#49548=CARTESIAN_POINT('Ctrl Pts',(21.1390622620736,20.0921028853463,-6.92202728813896));
#49549=CARTESIAN_POINT('Ctrl Pts',(21.1667237483346,20.0125782052865,-6.92619700245933));
#49550=CARTESIAN_POINT('Ctrl Pts',(21.1904053024889,19.9318834787289,-6.9303667167797));
#49551=CARTESIAN_POINT('Ctrl Pts',(21.214086013952,19.8511916236359,-6.93453628272375));
#49552=CARTESIAN_POINT('Ctrl Pts',(21.2337869461661,19.7693302464837,-6.93870584866779));
#49553=CARTESIAN_POINT('Ctrl Pts',(21.2494093711531,19.6867264923413,-6.94287541461183));
#49554=CARTESIAN_POINT('Ctrl Pts',(21.2655810613302,19.601218492106,-6.94719157735075));
#49555=CARTESIAN_POINT('Ctrl Pts',(21.2773820094429,19.5149154578639,-6.95150774008968));
#49556=CARTESIAN_POINT('Ctrl Pts',(21.2847607940422,19.4283001877063,-6.9558239028286));
#49557=CARTESIAN_POINT('Ctrl Pts',(21.2918992155093,19.3445064008638,-6.95999946702028));
#49558=CARTESIAN_POINT('Ctrl Pts',(21.2948991834511,19.2604208803107,-6.96417503121195));
#49559=CARTESIAN_POINT('Ctrl Pts',(21.2937672733171,19.1764817953118,-6.96835059540363));
#49560=CARTESIAN_POINT('Ctrl Pts',(21.2925781930931,19.0883031466757,-6.97273705741617));
#49561=CARTESIAN_POINT('Ctrl Pts',(21.2868289009944,19.0002866979193,-6.97712351942871));
#49562=CARTESIAN_POINT('Ctrl Pts',(21.2765884850301,18.9129332360151,-6.98150998144125));
#49563=CARTESIAN_POINT('Ctrl Pts',(21.2663480690658,18.8255797741109,-6.9858964434538));
#49564=CARTESIAN_POINT('Ctrl Pts',(21.2516167014297,18.7388898583324,-6.99028290546634));
#49565=CARTESIAN_POINT('Ctrl Pts',(21.2325245180282,18.6533484665025,-6.99466936747888));
#49566=CARTESIAN_POINT('Ctrl Pts',(21.2143107942864,18.5717429609135,-6.99885400187193));
#49567=CARTESIAN_POINT('Ctrl Pts',(21.1920609365757,18.490878859979,-7.00303863626498));
#49568=CARTESIAN_POINT('Ctrl Pts',(21.1658504730776,18.4111854736302,-7.00722327065802));
#49569=CARTESIAN_POINT('Ctrl Pts',(21.1396773169301,18.3316055209528,-7.01140194874197));
#49570=CARTESIAN_POINT('Ctrl Pts',(21.109554895207,18.2531934061979,-7.01558062682591));
#49571=CARTESIAN_POINT('Ctrl Pts',(21.0756095445168,18.1763673400535,-7.01975930490986));
#49572=CARTESIAN_POINT('Ctrl Pts',(21.0410557478115,18.0981642218874,-7.02401288279529));
#49573=CARTESIAN_POINT('Ctrl Pts',(21.0025407271243,18.0216050420064,-7.02826646068073));
#49574=CARTESIAN_POINT('Ctrl Pts',(20.9602505991268,17.9471138224161,-7.03252003856616));
#49575=CARTESIAN_POINT('Ctrl Pts',(20.9187803477829,17.8740667604752,-7.03669115254411));
#49576=CARTESIAN_POINT('Ctrl Pts',(20.8736802961219,17.8030086099539,-7.04086226652207));
#49577=CARTESIAN_POINT('Ctrl Pts',(20.8251733475076,17.7343165435092,-7.04503338050002));
#49578=CARTESIAN_POINT('Ctrl Pts',(20.7766826758684,17.6656475273507,-7.04920309482039));
#49579=CARTESIAN_POINT('Ctrl Pts',(20.7247876428631,17.5993433939188,-7.05337280914077));
#49580=CARTESIAN_POINT('Ctrl Pts',(20.669754524153,17.5357524295731,-7.05754252346114));
#49581=CARTESIAN_POINT('Ctrl Pts',(20.6147233637575,17.4721637280668,-7.06171208940518));
#49582=CARTESIAN_POINT('Ctrl Pts',(20.556554641366,17.4112883509861,-7.06588165534923));
#49583=CARTESIAN_POINT('Ctrl Pts',(20.4955540788025,17.3534405184613,-7.07005122129327));
#49584=CARTESIAN_POINT('Ctrl Pts',(20.4324088117115,17.2935588275079,-7.07436738403219));
#49585=CARTESIAN_POINT('Ctrl Pts',(20.3662292470559,17.2369219021169,-7.07868354677111));
#49586=CARTESIAN_POINT('Ctrl Pts',(20.2973935081709,17.1838343090391,-7.08299970951003));
#49587=CARTESIAN_POINT('Ctrl Pts',(20.2308000862399,17.132476038722,-7.08717527370171));
#49588=CARTESIAN_POINT('Ctrl Pts',(20.1617212960249,17.0844396429708,-7.09135083789339));
#49589=CARTESIAN_POINT('Ctrl Pts',(20.0905291277018,17.0399567655856,-7.09552640208507));
#49590=CARTESIAN_POINT('Ctrl Pts',(20.0157412122,16.9932271638116,-7.09991286409762));
#49591=CARTESIAN_POINT('Ctrl Pts',(19.9386213249318,16.9504197742736,-7.10429932611015));
#49592=CARTESIAN_POINT('Ctrl Pts',(19.8596279445188,16.9117475713792,-7.10868578812269));
#49593=CARTESIAN_POINT('Ctrl Pts',(19.7806345641058,16.8730753684849,-7.11307225013523));
#49594=CARTESIAN_POINT('Ctrl Pts',(19.6997682540137,16.8385385101708,-7.11745871214778));
#49595=CARTESIAN_POINT('Ctrl Pts',(19.6175072439402,16.8082900820313,-7.12184517416032));
#49596=CARTESIAN_POINT('Ctrl Pts',(19.5390311848803,16.7794334289094,-7.12602980855336));
#49597=CARTESIAN_POINT('Ctrl Pts',(19.4589938470389,16.7543718340009,-7.13021444294641));
#49598=CARTESIAN_POINT('Ctrl Pts',(19.3777970941006,16.733274167381,-7.13439907733946));
#49599=CARTESIAN_POINT('Ctrl Pts',(19.2967159146901,16.7122065306782,-7.1385777554234));
#49600=CARTESIAN_POINT('Ctrl Pts',(19.2144790396056,16.6950917298573,-7.14275643350734));
#49601=CARTESIAN_POINT('Ctrl Pts',(19.1315065014626,16.6820499053372,-7.14693511159128));
#49602=CARTESIAN_POINT('Ctrl Pts',(19.0470467402047,16.6687743154856,-7.15118868947672));
#49603=CARTESIAN_POINT('Ctrl Pts',(18.9618251354749,16.6597193207395,-7.15544226736216));
#49604=CARTESIAN_POINT('Ctrl Pts',(18.8762989641012,16.654957941501,-7.15969584524759));
#49605=CARTESIAN_POINT('Ctrl Pts',(18.7924308844501,16.6502888708901,-7.16386695922554));
#49606=CARTESIAN_POINT('Ctrl Pts',(18.7082704224839,16.6497484479464,-7.1680380732035));
#49607=CARTESIAN_POINT('Ctrl Pts',(18.6242553740812,16.6533534026215,-7.17220918718145));
#49608=CARTESIAN_POINT('Ctrl Pts',(18.5402685177394,16.6569571476192,-7.17637890150182));
#49609=CARTESIAN_POINT('Ctrl Pts',(18.4564274372811,16.6647034879404,-7.18054861582219));
#49610=CARTESIAN_POINT('Ctrl Pts',(18.3731691163825,16.6765570486934,-7.18471833014257));
#49611=CARTESIAN_POINT('Ctrl Pts',(18.2899137581723,16.6884101876458,-7.18888789608661));
#49612=CARTESIAN_POINT('Ctrl Pts',(18.2072415736113,16.7043701907562,-7.19305746203065));
#49613=CARTESIAN_POINT('Ctrl Pts',(18.1255822535274,16.7243500757491,-7.1972270279747));
#49614=CARTESIAN_POINT('Ctrl Pts',(18.041051892487,16.7450324288504,-7.20154319071362));
#49615=CARTESIAN_POINT('Ctrl Pts',(17.9576074580676,16.7700224760727,-7.20585935345254));
#49616=CARTESIAN_POINT('Ctrl Pts',(17.8757097136975,16.7991671317359,-7.21017551619146));
#49617=CARTESIAN_POINT('Ctrl Pts',(17.7964797797362,16.8273624033065,-7.21435108038314));
#49618=CARTESIAN_POINT('Ctrl Pts',(17.7186977338734,16.8594455439839,-7.21852664457482));
#49619=CARTESIAN_POINT('Ctrl Pts',(17.6427597031133,16.8952291532946,-7.2227022087665));
#49620=CARTESIAN_POINT('Ctrl Pts',(17.5629862229451,16.9328201076441,-7.22708867077904));
#49621=CARTESIAN_POINT('Ctrl Pts',(17.4852484504759,16.9744949002993,-7.23147513279159));
#49622=CARTESIAN_POINT('Ctrl Pts',(17.409973629261,17.0199833023029,-7.23586159480413));
#49623=CARTESIAN_POINT('Ctrl Pts',(17.3346988080461,17.0654717043064,-7.24024805681667));
#49624=CARTESIAN_POINT('Ctrl Pts',(17.2618873758783,17.1147733273606,-7.24463451882921));
#49625=CARTESIAN_POINT('Ctrl Pts',(17.1919269101811,17.1675689183003,-7.24902098084175));
#49626=CARTESIAN_POINT('Ctrl Pts',(17.1258771580207,17.2174132934338,-7.25316224442401));
#49627=CARTESIAN_POINT('Ctrl Pts',(17.0621112325389,17.2705657001619,-7.25730350800627));
#49628=CARTESIAN_POINT('Ctrl Pts',(17.0009846311416,17.326787238314,-7.26144477158852));
#49629=CARTESIAN_POINT('Ctrl Pts',(16.9399453026366,17.3829285067285,-7.26558012252321));
#49630=CARTESIAN_POINT('Ctrl Pts',(16.8815381604268,17.4421298917806,-7.2697154734579));
#49631=CARTESIAN_POINT('Ctrl Pts',(16.8260879518441,17.5041105435613,-7.27385082439259));
#49632=CARTESIAN_POINT('Ctrl Pts',(16.7707013118209,17.5660201402305,-7.27798143452813));
#49633=CARTESIAN_POINT('Ctrl Pts',(16.7182651826551,17.6307023247235,-7.28211204466367));
#49634=CARTESIAN_POINT('Ctrl Pts',(16.6690684130045,17.6978385608177,-7.28624265479921));
#49635=CARTESIAN_POINT('Ctrl Pts',(16.6199019406792,17.7649334517505,-7.29037072114092));
#49636=CARTESIAN_POINT('Ctrl Pts',(16.5739711466916,17.8344790168686,-7.29449878748264));
#49637=CARTESIAN_POINT('Ctrl Pts',(16.5315246255303,17.9061236744984,-7.29862685382436));
#49638=CARTESIAN_POINT('Ctrl Pts',(16.4890908665707,17.977746791056,-7.3027536789992));
#49639=CARTESIAN_POINT('Ctrl Pts',(16.4501395400176,18.0514673424197,-7.30688050417405));
#49640=CARTESIAN_POINT('Ctrl Pts',(16.4148750854129,18.1269060785424,-7.3110073293489));
#49641=CARTESIAN_POINT('Ctrl Pts',(16.3796101195078,18.2023459084537,-7.31513421435872));
#49642=CARTESIAN_POINT('Ctrl Pts',(16.3480323287909,18.2795035453344,-7.31926109936854));
#49643=CARTESIAN_POINT('Ctrl Pts',(16.3202988339461,18.3579779129531,-7.32338798437835));
#49644=CARTESIAN_POINT('Ctrl Pts',(16.2925397363851,18.4365247257132,-7.32751867920247));
#49645=CARTESIAN_POINT('Ctrl Pts',(16.2686321752694,18.516390251046,-7.33164937402659));
#49646=CARTESIAN_POINT('Ctrl Pts',(16.2486837569799,18.5971570459957,-7.33578006885071));
#49647=CARTESIAN_POINT('Ctrl Pts',(16.2287250388403,18.6779655427923,-7.33991289645232));
#49648=CARTESIAN_POINT('Ctrl Pts',(16.2127296214478,18.7596757735077,-7.34404572405394));
#49649=CARTESIAN_POINT('Ctrl Pts',(16.2007537416511,18.8418612800569,-7.34817855165556));
#49650=CARTESIAN_POINT('Ctrl Pts',(16.1887593096482,18.9241741027186,-7.35231778154836));
#49651=CARTESIAN_POINT('Ctrl Pts',(16.180796886798,19.0069632027562,-7.35645701144116));
#49652=CARTESIAN_POINT('Ctrl Pts',(16.176870697397,19.0897988045885,-7.36059624133397));
#49653=CARTESIAN_POINT('Ctrl Pts',(16.1749377014765,19.1305815748691,-7.36263412429881));
#49654=CARTESIAN_POINT('Ctrl Pts',(16.1739822581149,19.1713756409971,-7.36467200726366));
#49655=CARTESIAN_POINT('Ctrl Pts',(16.1740002494514,19.2121301287168,-7.36670989022851));
#49656=CARTESIAN_POINT('Origin',(18.734,19.211,1.76670989022852));
#49657=CARTESIAN_POINT('',(20.2935358855687,21.2411349269503,-6.05008448348788));
#49658=CARTESIAN_POINT('',(20.2954006757859,21.2435252751206,-6.11677130154247));
#49659=CARTESIAN_POINT('',(20.2935358855687,21.2411349269503,1.76670989022852));
#49660=CARTESIAN_POINT('',(16.1740008768645,19.208881145288,-6.6332901097715));
#49661=CARTESIAN_POINT('Ctrl Pts',(20.2954006757859,21.2435252751206,-6.11677130154247));
#49662=CARTESIAN_POINT('Ctrl Pts',(20.8926533935168,20.777292913641,-6.1545808581957));
#49663=CARTESIAN_POINT('Ctrl Pts',(21.7124083704566,19.1915607510674,-6.23478235040939));
#49664=CARTESIAN_POINT('Ctrl Pts',(20.433793589474,16.7062061261689,-6.35737577818358));
#49665=CARTESIAN_POINT('Ctrl Pts',(17.5479307751794,16.4259451726882,-6.48455158486501));
#49666=CARTESIAN_POINT('Ctrl Pts',(16.2478508564243,18.0710820233979,-6.57652302872766));
#49667=CARTESIAN_POINT('Ctrl Pts',(16.1710772436132,19.0646440698247,-6.62610253702982));
#49668=CARTESIAN_POINT('Ctrl Pts',(16.172362658312,19.2088797893707,-6.6332901097715));
#49669=CARTESIAN_POINT('Ctrl Pts',(16.1740008768645,19.208881145288,-6.6332901097715));
#49670=CARTESIAN_POINT('Ctrl Pts',(16.1739325519701,19.291431245901,-6.63740642252224));
#49671=CARTESIAN_POINT('Ctrl Pts',(16.1778613169669,19.3741241408158,-6.64152273527298));
#49672=CARTESIAN_POINT('Ctrl Pts',(16.1858020059738,19.456534077555,-6.64563904802372));
#49673=CARTESIAN_POINT('Ctrl Pts',(16.1937337220434,19.5388508914938,-6.64975070936243));
#49674=CARTESIAN_POINT('Ctrl Pts',(16.2056683130375,19.6208849121504,-6.65386237070114));
#49675=CARTESIAN_POINT('Ctrl Pts',(16.2215685692311,19.7022110602219,-6.65797403203985));
#49676=CARTESIAN_POINT('Ctrl Pts',(16.2374592000151,19.7834879765409,-6.66208320433539));
#49677=CARTESIAN_POINT('Ctrl Pts',(16.2573106430752,19.8640574053625,-6.66619237663093));
#49678=CARTESIAN_POINT('Ctrl Pts',(16.2810340922892,19.9435013690146,-6.67030154892647));
#49679=CARTESIAN_POINT('Ctrl Pts',(16.3047507902537,20.0229227244023,-6.67440955182852));
#49680=CARTESIAN_POINT('Ctrl Pts',(16.3323371713261,20.1012187954775,-6.67851755473057));
#49681=CARTESIAN_POINT('Ctrl Pts',(16.3636541468012,20.1779852823199,-6.68262555763262));
#49682=CARTESIAN_POINT('Ctrl Pts',(16.3949722554066,20.2547545467753,-6.68673370917299));
#49683=CARTESIAN_POINT('Ctrl Pts',(16.4300210447236,20.3299936782016,-6.69084186071336));
#49684=CARTESIAN_POINT('Ctrl Pts',(16.4686133150906,20.4033184003592,-6.69495001225373));
#49685=CARTESIAN_POINT('Ctrl Pts',(16.5072438266208,20.4767157801408,-6.69906223457025));
#49686=CARTESIAN_POINT('Ctrl Pts',(16.5494246053548,20.5481945435127,-6.70317445688677));
#49687=CARTESIAN_POINT('Ctrl Pts',(16.5949228757402,20.6173957680782,-6.70728667920329));
#49688=CARTESIAN_POINT('Ctrl Pts',(16.6404458510681,20.6866345679682,-6.71140113440064));
#49689=CARTESIAN_POINT('Ctrl Pts',(16.6892896206456,20.7535929860938,-6.715515589598));
#49690=CARTESIAN_POINT('Ctrl Pts',(16.7411800554792,20.8179438909682,-6.71963004479535));
#49691=CARTESIAN_POINT('Ctrl Pts',(16.7931561866085,20.8824010704228,-6.7237512949554));
#49692=CARTESIAN_POINT('Ctrl Pts',(16.8481887081045,20.9442417891331,-6.72787254511546));
#49693=CARTESIAN_POINT('Ctrl Pts',(16.9059658904508,21.0031750177716,-6.73199379527552));
#49694=CARTESIAN_POINT('Ctrl Pts',(16.9382542996129,21.0361094760171,-6.73429692959297));
#49695=CARTESIAN_POINT('Ctrl Pts',(16.9713992632832,21.068136611825,-6.73660006391043));
#49696=CARTESIAN_POINT('Ctrl Pts',(17.0053421035809,21.0992112903877,-6.73890319822789));
#49697=CARTESIAN_POINT('Ctrl Pts',(17.067013876621,21.1556718136325,-6.74308783262094));
#49698=CARTESIAN_POINT('Ctrl Pts',(17.1315694533286,21.2092127933028,-6.74727246701399));
#49699=CARTESIAN_POINT('Ctrl Pts',(17.198701023428,21.259525580152,-6.75145710140704));
#49700=CARTESIAN_POINT('Ctrl Pts',(17.2657370400465,21.3097667529765,-6.75563577949099));
#49701=CARTESIAN_POINT('Ctrl Pts',(17.3353414020479,21.3567885864286,-6.75981445757493));
#49702=CARTESIAN_POINT('Ctrl Pts',(17.4071710083241,21.4003206313485,-6.76399313565888));
#49703=CARTESIAN_POINT('Ctrl Pts',(17.4802881086698,21.4446329568877,-6.76824671354431));
#49704=CARTESIAN_POINT('Ctrl Pts',(17.5557106573433,21.4853288288424,-6.77250029142975));
#49705=CARTESIAN_POINT('Ctrl Pts',(17.6330432222703,21.5221672751169,-6.77675386931518));
#49706=CARTESIAN_POINT('Ctrl Pts',(17.7088765445241,21.5582915362259,-6.78092498329313));
#49707=CARTESIAN_POINT('Ctrl Pts',(17.7865460506904,21.5907063974352,-6.78509609727109));
#49708=CARTESIAN_POINT('Ctrl Pts',(17.8656529884827,21.6192303601585,-6.78926721124904));
#49709=CARTESIAN_POINT('Ctrl Pts',(17.9447333811781,21.6477447513906,-6.79343692556941));
#49710=CARTESIAN_POINT('Ctrl Pts',(18.0252498151568,21.6723706812234,-6.79760663988978));
#49711=CARTESIAN_POINT('Ctrl Pts',(18.1067845307988,21.6929751721552,-6.80177635421016));
#49712=CARTESIAN_POINT('Ctrl Pts',(18.1883163450855,21.7135789298907,-6.80594592015419));
#49713=CARTESIAN_POINT('Ctrl Pts',(18.2708659227708,21.7301614213603,-6.81011548609823));
#49714=CARTESIAN_POINT('Ctrl Pts',(18.3540026821446,21.7426401873929,-6.81428505204227));
#49715=CARTESIAN_POINT('Ctrl Pts',(18.4400624274178,21.755557691445,-6.81860121478119));
#49716=CARTESIAN_POINT('Ctrl Pts',(18.5267508916658,21.7640774486062,-6.82291737752011));
#49717=CARTESIAN_POINT('Ctrl Pts',(18.6135836740995,21.7681663826307,-6.82723354025903));
#49718=CARTESIAN_POINT('Ctrl Pts',(18.6975878877785,21.7721221200595,-6.83140910445071));
#49719=CARTESIAN_POINT('Ctrl Pts',(18.7817266907697,21.7719313177434,-6.83558466864238));
#49720=CARTESIAN_POINT('Ctrl Pts',(18.8655624783152,21.7676171622477,-6.83976023283406));
#49721=CARTESIAN_POINT('Ctrl Pts',(18.953632612189,21.7630851090138,-6.8441466948466));
#49722=CARTESIAN_POINT('Ctrl Pts',(19.0413677347562,21.7540022746857,-6.84853315685915));
#49723=CARTESIAN_POINT('Ctrl Pts',(19.1282700391325,21.7404566879554,-6.85291961887169));
#49724=CARTESIAN_POINT('Ctrl Pts',(19.2151723435088,21.7269111012252,-6.85730608088423));
#49725=CARTESIAN_POINT('Ctrl Pts',(19.3012412773526,21.7089029553709,-6.86169254289678));
#49726=CARTESIAN_POINT('Ctrl Pts',(19.3859971465595,21.6865806835727,-6.86607900490932));
#49727=CARTESIAN_POINT('Ctrl Pts',(19.4675566076895,21.6651002542397,-6.87030003976341));
#49728=CARTESIAN_POINT('Ctrl Pts',(19.5482065108308,21.6395446517759,-6.87452107461749));
#49729=CARTESIAN_POINT('Ctrl Pts',(19.6275095396711,21.6100082747912,-6.87874210947158));
#49730=CARTESIAN_POINT('Ctrl Pts',(19.7060066089446,21.5807720770802,-6.8829202457949));
#49731=CARTESIAN_POINT('Ctrl Pts',(19.7831836018448,21.5476357741988,-6.88709838211823));
#49732=CARTESIAN_POINT('Ctrl Pts',(19.8586276861513,21.5107418480217,-6.89127651844155));
#49733=CARTESIAN_POINT('Ctrl Pts',(19.9352336905536,21.4732797156739,-6.89551900256102));
#49734=CARTESIAN_POINT('Ctrl Pts',(20.0100524876427,21.4319433469969,-6.89976148668049));
#49735=CARTESIAN_POINT('Ctrl Pts',(20.0826708300222,21.3869335909552,-6.90400397079996));
#49736=CARTESIAN_POINT('Ctrl Pts',(20.1552891724016,21.3419238349136,-6.90824645491943));
#49737=CARTESIAN_POINT('Ctrl Pts',(20.2257066125816,21.2932409145431,-6.9124889390389));
#49738=CARTESIAN_POINT('Ctrl Pts',(20.2935358855687,21.2411349269503,-6.91673142315837));
#49739=CARTESIAN_POINT('',(16.174000571626,19.2127107672549,-6.56670989025839));
#49740=CARTESIAN_POINT('Ctrl Pts',(16.174000571626,19.2127107672549,-6.56670989025838));
#49741=CARTESIAN_POINT('Ctrl Pts',(16.1740643617891,19.3081666398866,-6.57143929947811));
#49742=CARTESIAN_POINT('Ctrl Pts',(16.1794711562484,19.4034153336876,-6.57616870869783));
#49743=CARTESIAN_POINT('Ctrl Pts',(16.1901275024527,19.4979019278825,-6.58089811791755));
#49744=CARTESIAN_POINT('Ctrl Pts',(16.200836414009,19.5928546031322,-6.58565085624608));
#49745=CARTESIAN_POINT('Ctrl Pts',(16.2168466650982,19.6870374428256,-6.59040359457461));
#49746=CARTESIAN_POINT('Ctrl Pts',(16.2380139506883,19.7799056526714,-6.59515633290315));
#49747=CARTESIAN_POINT('Ctrl Pts',(16.2593038089226,19.8733116311407,-6.59993659274364));
#49748=CARTESIAN_POINT('Ctrl Pts',(16.2858104835354,19.9653875176628,-6.60471685258415));
#49749=CARTESIAN_POINT('Ctrl Pts',(16.3173390825683,20.0556005032904,-6.60949711242465));
#49750=CARTESIAN_POINT('Ctrl Pts',(16.3253523527952,20.0785289255476,-6.61071205742796));
#49751=CARTESIAN_POINT('Ctrl Pts',(16.3336897868424,20.101337126465,-6.61192700243127));
#49752=CARTESIAN_POINT('Ctrl Pts',(16.3423477078173,20.1240166007785,-6.61314194743458));
#49753=CARTESIAN_POINT('Ctrl Pts',(16.3721681801721,20.2021315014283,-6.61732658182763));
#49754=CARTESIAN_POINT('Ctrl Pts',(16.405875193857,20.2789292632221,-6.62151121622068));
#49755=CARTESIAN_POINT('Ctrl Pts',(16.4433319467771,20.3539960060927,-6.62569585061372));
#49756=CARTESIAN_POINT('Ctrl Pts',(16.4807353846457,20.4289559007464,-6.62987452869767));
#49757=CARTESIAN_POINT('Ctrl Pts',(16.5218777565726,20.5021892624269,-6.63405320678162));
#49758=CARTESIAN_POINT('Ctrl Pts',(16.5665735905077,20.5733005393214,-6.63823188486556));
#49759=CARTESIAN_POINT('Ctrl Pts',(16.6120705651437,20.6456864347474,-6.642485462751));
#49760=CARTESIAN_POINT('Ctrl Pts',(16.6612494744651,20.715872969927,-6.64673904063643));
#49761=CARTESIAN_POINT('Ctrl Pts',(16.7138648542456,20.7834674854787,-6.65099261852187));
#49762=CARTESIAN_POINT('Ctrl Pts',(16.7654601822185,20.8497515494465,-6.65516373249982));
#49763=CARTESIAN_POINT('Ctrl Pts',(16.8203596287513,20.9135428198972,-6.65933484647778));
#49764=CARTESIAN_POINT('Ctrl Pts',(16.8782881026494,20.9745003130228,-6.66350596045573));
#49765=CARTESIAN_POINT('Ctrl Pts',(16.9361971380886,21.0354373512729,-6.6676756747761));
#49766=CARTESIAN_POINT('Ctrl Pts',(16.9971328656302,21.0935421675084,-6.67184538909648));
#49767=CARTESIAN_POINT('Ctrl Pts',(17.0607814536892,21.1485086312792,-6.67601510341685));
#49768=CARTESIAN_POINT('Ctrl Pts',(17.1244277768583,21.2034731391074,-6.68018466936089));
#49769=CARTESIAN_POINT('Ctrl Pts',(17.1907864198801,21.2552992164785,-6.68435423530494));
#49770=CARTESIAN_POINT('Ctrl Pts',(17.2595094445544,21.3037201441907,-6.68852380124898));
#49771=CARTESIAN_POINT('Ctrl Pts',(17.3306486859971,21.3538434919877,-6.6928399639879));
#49772=CARTESIAN_POINT('Ctrl Pts',(17.404321234744,21.4003174810233,-6.69715612672682));
#49773=CARTESIAN_POINT('Ctrl Pts',(17.4801089073794,21.4428954114937,-6.70147228946574));
#49774=CARTESIAN_POINT('Ctrl Pts',(17.5534278045501,21.4840863703575,-6.70564785365742));
#49775=CARTESIAN_POINT('Ctrl Pts',(17.6287256988458,21.5216310329473,-6.7098234178491));
#49776=CARTESIAN_POINT('Ctrl Pts',(17.7056010183995,21.555353969571,-6.71399898204078));
#49777=CARTESIAN_POINT('Ctrl Pts',(17.7863591275902,21.5907801715548,-6.71838544405332));
#49778=CARTESIAN_POINT('Ctrl Pts',(17.8688576552588,21.6219882241026,-6.72277190606586));
#49779=CARTESIAN_POINT('Ctrl Pts',(17.9526121488768,21.6488336748263,-6.7271583680784));
#49780=CARTESIAN_POINT('Ctrl Pts',(18.0363666424948,21.67567912555,-6.73154483009094));
#49781=CARTESIAN_POINT('Ctrl Pts',(18.1213765216826,21.6981618996353,-6.73593129210348));
#49782=CARTESIAN_POINT('Ctrl Pts',(18.20714644876,21.7161996598167,-6.74031775411602));
#49783=CARTESIAN_POINT('Ctrl Pts',(18.2889778682176,21.7334091360257,-6.7445027922187));
#49784=CARTESIAN_POINT('Ctrl Pts',(18.3718056859211,21.7466369348047,-6.74868783032139));
#49785=CARTESIAN_POINT('Ctrl Pts',(18.4552077229433,21.7557740304894,-6.75287286842408));
#49786=CARTESIAN_POINT('Ctrl Pts',(18.5384664989634,21.76489543124,-6.75705071782042));
#49787=CARTESIAN_POINT('Ctrl Pts',(18.6222970795584,21.7699400516429,-6.76122856721677));
#49788=CARTESIAN_POINT('Ctrl Pts',(18.7062667332565,21.7708497740914,-6.76540641661311));
#49789=CARTESIAN_POINT('Ctrl Pts',(18.7901543122251,21.771758607347,-6.76958018244065));
#49790=CARTESIAN_POINT('Ctrl Pts',(18.8741802371502,21.7685405617463,-6.77375394826818));
#49791=CARTESIAN_POINT('Ctrl Pts',(18.9579070743406,21.7611893306302,-6.77792771409572));
#49792=CARTESIAN_POINT('Ctrl Pts',(19.0415771929613,21.7538430794146,-6.78209865251408));
#49793=CARTESIAN_POINT('Ctrl Pts',(19.1249481693622,21.7423692437104,-6.78626959093244));
#49794=CARTESIAN_POINT('Ctrl Pts',(19.2075843584856,21.7268135573603,-6.7904405293508));
#49795=CARTESIAN_POINT('Ctrl Pts',(19.2901893576106,21.7112637423098,-6.7946098935005));
#49796=CARTESIAN_POINT('Ctrl Pts',(19.3720596691157,21.691635223593,-6.79877925765021));
#49797=CARTESIAN_POINT('Ctrl Pts',(19.4527679051965,21.6680251725327,-6.80294862179992));
#49798=CARTESIAN_POINT('Ctrl Pts',(19.5335042821167,21.6444068892686,-6.80711943969725));
#49799=CARTESIAN_POINT('Ctrl Pts',(19.6130773298807,21.61680442152,-6.81129025759458));
#49800=CARTESIAN_POINT('Ctrl Pts',(19.6910737323164,21.585365151132,-6.81546107549191));
#49801=CARTESIAN_POINT('Ctrl Pts',(19.769082010496,21.5539210937959,-6.81963252843861));
#49802=CARTESIAN_POINT('Ctrl Pts',(19.8455127429604,21.5186392539808,-6.8238039813853));
#49803=CARTESIAN_POINT('Ctrl Pts',(19.9199734317163,21.4797148386836,-6.827975434332));
#49804=CARTESIAN_POINT('Ctrl Pts',(19.9945177108365,21.4407467264221,-6.83215157019631));
#49805=CARTESIAN_POINT('Ctrl Pts',(20.0670871265665,21.3981280958129,-6.83632770606063));
#49806=CARTESIAN_POINT('Ctrl Pts',(20.1373150369655,21.3520994621985,-6.84050384192494));
#49807=CARTESIAN_POINT('Ctrl Pts',(20.19079582316,21.3170471945292,-6.84368410213786));
#49808=CARTESIAN_POINT('Ctrl Pts',(20.2429192162059,21.2800183091488,-6.84686436235078));
#49809=CARTESIAN_POINT('Ctrl Pts',(20.2935358855687,21.2411349269503,-6.8500446225637));
#49810=CARTESIAN_POINT('Ctrl Pts',(20.2935358855687,21.2411349269503,-6.05008448348788));
#49811=CARTESIAN_POINT('Ctrl Pts',(20.3602243251599,21.1899053198368,-6.05425482437397));
#49812=CARTESIAN_POINT('Ctrl Pts',(20.4243678378452,21.1354001087936,-6.05842516526005));
#49813=CARTESIAN_POINT('Ctrl Pts',(20.4856397822034,21.0779113726695,-6.06259550614614));
#49814=CARTESIAN_POINT('Ctrl Pts',(20.5469803588776,21.0203582419002,-6.06677051834071));
#49815=CARTESIAN_POINT('Ctrl Pts',(20.6054426129598,20.9598152326617,-6.07094553053529));
#49816=CARTESIAN_POINT('Ctrl Pts',(20.6607367282526,20.8966113371719,-6.07512054272987));
#49817=CARTESIAN_POINT('Ctrl Pts',(20.7160670495591,20.8333660564264,-6.07929828867916));
#49818=CARTESIAN_POINT('Ctrl Pts',(20.768224818516,20.7674567823383,-6.08347603462846));
#49819=CARTESIAN_POINT('Ctrl Pts',(20.8169619650072,20.6992437476211,-6.08765378057776));
#49820=CARTESIAN_POINT('Ctrl Pts',(20.8657776938873,20.6309207281468,-6.0918382626058));
#49821=CARTESIAN_POINT('Ctrl Pts',(20.9111615468503,20.5602869221389,-6.09602274463385));
#49822=CARTESIAN_POINT('Ctrl Pts',(20.9529102907763,20.4877290712938,-6.1002072266619));
#49823=CARTESIAN_POINT('Ctrl Pts',(20.9669828856803,20.4632713955407,-6.10161772467755));
#49824=CARTESIAN_POINT('Ctrl Pts',(20.9806428526884,20.4385952862944,-6.1030282226932));
#49825=CARTESIAN_POINT('Ctrl Pts',(20.9938836431733,20.4137160593082,-6.10443872070885));
#49826=CARTESIAN_POINT('Ctrl Pts',(21.0331661282527,20.3399049175952,-6.1086233551019));
#49827=CARTESIAN_POINT('Ctrl Pts',(21.0689017421373,20.2640298565515,-6.11280798949495));
#49828=CARTESIAN_POINT('Ctrl Pts',(21.1008684225543,20.1864659759907,-6.116992623888));
#49829=CARTESIAN_POINT('Ctrl Pts',(21.1327896023584,20.1090124980134,-6.12117130197194));
#49830=CARTESIAN_POINT('Ctrl Pts',(21.1609523307067,20.0298753969622,-6.12534998005589));
#49831=CARTESIAN_POINT('Ctrl Pts',(21.1851803441784,19.9494544131587,-6.12952865813984));
#49832=CARTESIAN_POINT('Ctrl Pts',(21.2098426273792,19.867591941018,-6.13378223602527));
#49833=CARTESIAN_POINT('Ctrl Pts',(21.2304275222058,19.7843995318237,-6.13803581391071));
#49834=CARTESIAN_POINT('Ctrl Pts',(21.2468003698023,19.7003202443405,-6.14228939179614));
#49835=CARTESIAN_POINT('Ctrl Pts',(21.2628557977992,19.6178709979124,-6.14646050577409));
#49836=CARTESIAN_POINT('Ctrl Pts',(21.2748609466779,19.5345694264043,-6.15063161975204));
#49837=CARTESIAN_POINT('Ctrl Pts',(21.2827395777799,19.4508469609111,-6.15480273372999));
#49838=CARTESIAN_POINT('Ctrl Pts',(21.2906155651312,19.3671525892997,-6.15897244805036));
#49839=CARTESIAN_POINT('Ctrl Pts',(21.2943677416632,19.2830380618264,-6.16314216237074));
#49840=CARTESIAN_POINT('Ctrl Pts',(21.2939715980996,19.1989411060454,-6.16731187669111));
#49841=CARTESIAN_POINT('Ctrl Pts',(21.2935754686325,19.1148471427948,-6.17148144263515));
#49842=CARTESIAN_POINT('Ctrl Pts',(21.2890313155854,19.0307712100169,-6.1756510085792));
#49843=CARTESIAN_POINT('Ctrl Pts',(21.2803667494581,18.9471508437493,-6.17982057452325));
#49844=CARTESIAN_POINT('Ctrl Pts',(21.2713975478746,18.8605904885607,-6.18413673726217));
#49845=CARTESIAN_POINT('Ctrl Pts',(21.2580128490967,18.7745188559842,-6.18845290000109));
#49846=CARTESIAN_POINT('Ctrl Pts',(21.2403015155518,18.6894132736133,-6.19276906274001));
#49847=CARTESIAN_POINT('Ctrl Pts',(21.2231671268342,18.6070799966365,-6.19694462693169));
#49848=CARTESIAN_POINT('Ctrl Pts',(21.2019838191122,18.5256512422048,-6.20112019112337));
#49849=CARTESIAN_POINT('Ctrl Pts',(21.1768832583851,18.4455449811374,-6.20529575531505));
#49850=CARTESIAN_POINT('Ctrl Pts',(21.1505149280065,18.361392743258,-6.20968221732759));
#49851=CARTESIAN_POINT('Ctrl Pts',(21.1198234271564,18.278700655445,-6.21406867934013));
#49852=CARTESIAN_POINT('Ctrl Pts',(21.0850182368018,18.197928802983,-6.21845514135267));
#49853=CARTESIAN_POINT('Ctrl Pts',(21.0502130464472,18.117156950521,-6.2228416033652));
#49854=CARTESIAN_POINT('Ctrl Pts',(21.0112944915984,18.0383058200371,-6.22722806537774));
#49855=CARTESIAN_POINT('Ctrl Pts',(20.9685260259017,17.9618028820206,-6.23161452739028));
#49856=CARTESIAN_POINT('Ctrl Pts',(20.9277254007097,17.8888199575867,-6.23579916178333));
#49857=CARTESIAN_POINT('Ctrl Pts',(20.8832694918769,17.8177022301347,-6.23998379617638));
#49858=CARTESIAN_POINT('Ctrl Pts',(20.8353535008892,17.7488394533087,-6.24416843056942));
#49859=CARTESIAN_POINT('Ctrl Pts',(20.7875057123838,17.680074694122,-6.24834710865336));
#49860=CARTESIAN_POINT('Ctrl Pts',(20.7362078848241,17.6135588845842,-6.25252578673731));
#49861=CARTESIAN_POINT('Ctrl Pts',(20.6817007285136,17.5496566061926,-6.25670446482125));
#49862=CARTESIAN_POINT('Ctrl Pts',(20.6262165705999,17.4846089253865,-6.26095804270669));
#49863=CARTESIAN_POINT('Ctrl Pts',(20.5674071330978,17.4222698132395,-6.26521162059212));
#49864=CARTESIAN_POINT('Ctrl Pts',(20.5055720700286,17.3629923158453,-6.26946519847756));
#49865=CARTESIAN_POINT('Ctrl Pts',(20.4449358003181,17.3048640284086,-6.27363631245551));
#49866=CARTESIAN_POINT('Ctrl Pts',(20.3813905208317,17.2496800373396,-6.27780742643346));
#49867=CARTESIAN_POINT('Ctrl Pts',(20.3152577303047,17.1977379727538,-6.28197854041141));
#49868=CARTESIAN_POINT('Ctrl Pts',(20.2491471312743,17.1458133378293,-6.28614825473179));
#49869=CARTESIAN_POINT('Ctrl Pts',(20.1804511070728,17.0971287527976,-6.29031796905216));
#49870=CARTESIAN_POINT('Ctrl Pts',(20.1095244508951,17.0519417597041,-6.29448768337254));
#49871=CARTESIAN_POINT('Ctrl Pts',(20.0386003185924,17.0067563745578,-6.29865724931658));
#49872=CARTESIAN_POINT('Ctrl Pts',(19.9654461005736,16.9650685803562,-6.30282681526061));
#49873=CARTESIAN_POINT('Ctrl Pts',(19.8904446404444,16.9270919909971,-6.30699638120464));
#49874=CARTESIAN_POINT('Ctrl Pts',(19.8128062215012,16.8877801916052,-6.31131254394357));
#49875=CARTESIAN_POINT('Ctrl Pts',(19.7331887160479,16.8524456628669,-6.31562870668249));
#49876=CARTESIAN_POINT('Ctrl Pts',(19.6520415805985,16.8212720539165,-6.31994486942141));
#49877=CARTESIAN_POINT('Ctrl Pts',(19.5735378045512,16.7911139219988,-6.32412043361309));
#49878=CARTESIAN_POINT('Ctrl Pts',(19.4936029857573,16.7648498911065,-6.32829599780477));
#49879=CARTESIAN_POINT('Ctrl Pts',(19.4126598398385,16.7425954906478,-6.33247156199645));
#49880=CARTESIAN_POINT('Ctrl Pts',(19.3276284480433,16.7192170733266,-6.33685802400899));
#49881=CARTESIAN_POINT('Ctrl Pts',(19.2414847611992,16.7002641097526,-6.34124448602154));
#49882=CARTESIAN_POINT('Ctrl Pts',(19.154729026295,16.6858094950216,-6.34563094803408));
#49883=CARTESIAN_POINT('Ctrl Pts',(19.0679732913908,16.6713548802907,-6.35001741004663));
#49884=CARTESIAN_POINT('Ctrl Pts',(18.9806060935248,16.6613986045227,-6.35440387205917));
#49885=CARTESIAN_POINT('Ctrl Pts',(18.8931294701917,16.6559505265619,-6.35879033407172));
#49886=CARTESIAN_POINT('Ctrl Pts',(18.8096777759695,16.650753122744,-6.36297496846477));
#49887=CARTESIAN_POINT('Ctrl Pts',(18.7258158815285,16.6496388297568,-6.36715960285782));
#49888=CARTESIAN_POINT('Ctrl Pts',(18.6419771668654,16.6526544802975,-6.37134423725087));
#49889=CARTESIAN_POINT('Ctrl Pts',(18.5582577862359,16.6556658384328,-6.3755229153348));
#49890=CARTESIAN_POINT('Ctrl Pts',(18.4745619756522,16.6627954472227,-6.37970159341873));
#49891=CARTESIAN_POINT('Ctrl Pts',(18.391326582379,16.6740382484444,-6.38388027150266));
#49892=CARTESIAN_POINT('Ctrl Pts',(18.3065992545013,16.6854825687981,-6.3881338493881));
#49893=CARTESIAN_POINT('Ctrl Pts',(18.2223494934534,16.7011890198916,-6.39238742727354));
#49894=CARTESIAN_POINT('Ctrl Pts',(18.1390363521675,16.7210967372691,-6.39664100515897));
#49895=CARTESIAN_POINT('Ctrl Pts',(18.0573383986977,16.7406185046986,-6.40081211913692));
#49896=CARTESIAN_POINT('Ctrl Pts',(17.9765415407101,16.7641799807696,-6.40498323311487));
#49897=CARTESIAN_POINT('Ctrl Pts',(17.8970700591987,16.7916719374606,-6.40915434709282));
#49898=CARTESIAN_POINT('Ctrl Pts',(17.8176252451106,16.81915466896,-6.41332406141319));
#49899=CARTESIAN_POINT('Ctrl Pts',(17.7395053586247,16.8505651114303,-6.41749377573355));
#49900=CARTESIAN_POINT('Ctrl Pts',(17.6631189946713,16.8857443425666,-6.42166349005392));
#49901=CARTESIAN_POINT('Ctrl Pts',(17.5867353488726,16.9209223218748,-6.42583305599795));
#49902=CARTESIAN_POINT('Ctrl Pts',(17.5120855204514,16.9598686299929,-6.43000262194199));
#49903=CARTESIAN_POINT('Ctrl Pts',(17.4395563508731,17.002376981186,-6.43417218788603));
#49904=CARTESIAN_POINT('Ctrl Pts',(17.3644771451667,17.0463798735675,-6.43848835062496));
#49905=CARTESIAN_POINT('Ctrl Pts',(17.2916709526717,17.0941996856766,-6.44280451336388));
#49906=CARTESIAN_POINT('Ctrl Pts',(17.2215354755333,17.1455579015064,-6.44712067610281));
#49907=CARTESIAN_POINT('Ctrl Pts',(17.1536846541857,17.1952431288574,-6.45129624029449));
#49908=CARTESIAN_POINT('Ctrl Pts',(17.0883335592488,17.2482394397185,-6.45547180448617));
#49909=CARTESIAN_POINT('Ctrl Pts',(17.0258081406205,17.3042539310255,-6.45964736867785));
#49910=CARTESIAN_POINT('Ctrl Pts',(16.9601247117373,17.3630975811266,-6.4640338306904));
#49911=CARTESIAN_POINT('Ctrl Pts',(16.8975603248985,17.4252719095173,-6.46842029270295));
#49912=CARTESIAN_POINT('Ctrl Pts',(16.8384470475511,17.4903957443787,-6.4728067547155));
#49913=CARTESIAN_POINT('Ctrl Pts',(16.7793337702037,17.55551957924,-6.47719321672805));
#49914=CARTESIAN_POINT('Ctrl Pts',(16.7236719107427,17.6235924232491,-6.4815796787406));
#49915=CARTESIAN_POINT('Ctrl Pts',(16.6717415022697,17.6941974787273,-6.48596614075315));
#49916=CARTESIAN_POINT('Ctrl Pts',(16.6219091295866,17.7619500256717,-6.4901753857061));
#49917=CARTESIAN_POINT('Ctrl Pts',(16.5753265021954,17.8322867639503,-6.49438463065906));
#49918=CARTESIAN_POINT('Ctrl Pts',(16.5322706261132,17.9048653345982,-6.49859387561201));
#49919=CARTESIAN_POINT('Ctrl Pts',(16.4892771418592,17.9773387323843,-6.50279702099131));
#49920=CARTESIAN_POINT('Ctrl Pts',(16.4498004872777,18.0520471246589,-6.5070001663706));
#49921=CARTESIAN_POINT('Ctrl Pts',(16.4140760664827,18.128617007389,-6.5112033117499));
#49922=CARTESIAN_POINT('Ctrl Pts',(16.3783931208862,18.2050979943158,-6.51540157737789));
#49923=CARTESIAN_POINT('Ctrl Pts',(16.3464539443372,18.2834357700826,-6.51959984300588));
#49924=CARTESIAN_POINT('Ctrl Pts',(16.3184487740251,18.3632310015746,-6.52379810863387));
#49925=CARTESIAN_POINT('Ctrl Pts',(16.2904693914728,18.4429527559108,-6.52799250840908));
#49926=CARTESIAN_POINT('Ctrl Pts',(16.2664169618498,18.5241288717768,-6.53218690818429));
#49927=CARTESIAN_POINT('Ctrl Pts',(16.2464336691667,18.6063399717985,-6.5363813079595));
#49928=CARTESIAN_POINT('Ctrl Pts',(16.2264610773219,18.6885070486605,-6.54057346167876));
#49929=CARTESIAN_POINT('Ctrl Pts',(16.210553397436,18.7717075687093,-6.54476561539801));
#49930=CARTESIAN_POINT('Ctrl Pts',(16.1988026788696,18.8555080269072,-6.54895776911726));
#49931=CARTESIAN_POINT('Ctrl Pts',(16.1870533030452,18.9392989093172,-6.55314944380363));
#49932=CARTESIAN_POINT('Ctrl Pts',(16.1794600117858,19.0236891460433,-6.55734111849001));
#49933=CARTESIAN_POINT('Ctrl Pts',(16.1760633700115,19.1082371810286,-6.56153279317638));
#49934=CARTESIAN_POINT('Ctrl Pts',(16.1746649834927,19.1430453357189,-6.56325849219375));
#49935=CARTESIAN_POINT('Ctrl Pts',(16.173977295445,19.1778801783156,-6.56498419121113));
#49936=CARTESIAN_POINT('Ctrl Pts',(16.1740005716256,19.2127107666517,-6.5667098902285));
#49937=CARTESIAN_POINT('Origin',(18.734,19.211,1.76670989022852));
#49938=CARTESIAN_POINT('',(20.2935358855687,21.2411349269503,-5.2501823431226));
#49939=CARTESIAN_POINT('',(20.2935358855687,21.2411349269503,-5.31661775129949));
#49940=CARTESIAN_POINT('',(20.2935358855687,21.2411349269503,1.76670989022852));
#49941=CARTESIAN_POINT('',(16.1740005630998,19.2126979607665,-5.83329010977151));
#49942=CARTESIAN_POINT('Ctrl Pts',(20.2935358855687,21.2411349269503,-5.31661775129949));
#49943=CARTESIAN_POINT('Ctrl Pts',(20.3601996618573,21.1899242660186,-5.32080132208221));
#49944=CARTESIAN_POINT('Ctrl Pts',(20.4242600608059,21.1354868005558,-5.32498489286492));
#49945=CARTESIAN_POINT('Ctrl Pts',(20.4854058680557,21.0781308163436,-5.32916846364764));
#49946=CARTESIAN_POINT('Ctrl Pts',(20.5380265760828,21.0287715448812,-5.33276875067579));
#49947=CARTESIAN_POINT('Ctrl Pts',(20.5884892422948,20.9772515834067,-5.33636903770395));
#49948=CARTESIAN_POINT('Ctrl Pts',(20.6366195645772,20.923786849695,-5.3399693247321));
#49949=CARTESIAN_POINT('Ctrl Pts',(20.6925617159657,20.8616444811129,-5.34415395912515));
#49950=CARTESIAN_POINT('Ctrl Pts',(20.7455602793472,20.7966428559979,-5.34833859351819));
#49951=CARTESIAN_POINT('Ctrl Pts',(20.7953091936645,20.7290923582293,-5.35252322791124));
#49952=CARTESIAN_POINT('Ctrl Pts',(20.8449872965599,20.6616380102333,-5.35670190599519));
#49953=CARTESIAN_POINT('Ctrl Pts',(20.891424667568,20.5916423631925,-5.36088058407913));
#49954=CARTESIAN_POINT('Ctrl Pts',(20.934353739878,20.5194507707228,-5.36505926216307));
#49955=CARTESIAN_POINT('Ctrl Pts',(20.9780522849565,20.4459651958412,-5.36931284004851));
#49956=CARTESIAN_POINT('Ctrl Pts',(21.0181151991572,20.3702045348863,-5.37356641793395));
#49957=CARTESIAN_POINT('Ctrl Pts',(21.0543048298795,20.2925662237874,-5.37781999581938));
#49958=CARTESIAN_POINT('Ctrl Pts',(21.089792853992,20.2164330828479,-5.38199110979733));
#49959=CARTESIAN_POINT('Ctrl Pts',(21.1215562334332,20.1384948820617,-5.38616222377529));
#49960=CARTESIAN_POINT('Ctrl Pts',(21.1494168148283,20.0591518794676,-5.39033333775324));
#49961=CARTESIAN_POINT('Ctrl Pts',(21.1772680473363,19.9798355011844,-5.39450305207361));
#49962=CARTESIAN_POINT('Ctrl Pts',(21.2012189304412,19.8991156909809,-5.39867276639398));
#49963=CARTESIAN_POINT('Ctrl Pts',(21.2211399893044,19.817411307285,-5.40284248071436));
#49964=CARTESIAN_POINT('Ctrl Pts',(21.2410603392908,19.7357098309816,-5.4070120466584));
#49965=CARTESIAN_POINT('Ctrl Pts',(21.2569510420042,19.6530242979867,-5.41118161260244));
#49966=CARTESIAN_POINT('Ctrl Pts',(21.2687332465284,19.5697859653662,-5.41535117854649));
#49967=CARTESIAN_POINT('Ctrl Pts',(21.2809296988287,19.4836210756563,-5.41966734128541));
#49968=CARTESIAN_POINT('Ctrl Pts',(21.2887232939913,19.396864312403,-5.42398350402433));
#49969=CARTESIAN_POINT('Ctrl Pts',(21.2920850129342,19.3100003363693,-5.42829966676325));
#49970=CARTESIAN_POINT('Ctrl Pts',(21.2953372242362,19.2259659452184,-5.43247523095493));
#49971=CARTESIAN_POINT('Ctrl Pts',(21.2944419142066,19.1418316894466,-5.43665079514661));
#49972=CARTESIAN_POINT('Ctrl Pts',(21.2894259327675,19.0580349643243,-5.44082635933829));
#49973=CARTESIAN_POINT('Ctrl Pts',(21.2841566060303,18.9700058658239,-5.44521282135083));
#49974=CARTESIAN_POINT('Ctrl Pts',(21.2743394628619,18.8823498716687,-5.44959928336338));
#49975=CARTESIAN_POINT('Ctrl Pts',(21.2600666971253,18.7955640342066,-5.45398574537592));
#49976=CARTESIAN_POINT('Ctrl Pts',(21.2457939313886,18.7087781967444,-5.45837220738846));
#49977=CARTESIAN_POINT('Ctrl Pts',(21.2270657409798,18.6228630666792,-5.462758669401));
#49978=CARTESIAN_POINT('Ctrl Pts',(21.2040345704695,18.5382970784324,-5.46714513141354));
#49979=CARTESIAN_POINT('Ctrl Pts',(21.1820630982548,18.4576220966617,-5.47132976580659));
#49980=CARTESIAN_POINT('Ctrl Pts',(21.1560941354244,18.377874545241,-5.47551440019964));
#49981=CARTESIAN_POINT('Ctrl Pts',(21.1262230006562,18.2994797779909,-5.47969903459269));
#49982=CARTESIAN_POINT('Ctrl Pts',(21.0963943837511,18.2211965959888,-5.48387771267663));
#49983=CARTESIAN_POINT('Ctrl Pts',(21.0626747898134,18.1442627996735,-5.48805639076058));
#49984=CARTESIAN_POINT('Ctrl Pts',(21.0252097777407,18.0690903037518,-5.49223506884452));
#49985=CARTESIAN_POINT('Ctrl Pts',(20.9870732322522,17.9925703948663,-5.49648864672996));
#49986=CARTESIAN_POINT('Ctrl Pts',(20.9450558013772,17.9178760152568,-5.50074222461539));
#49987=CARTESIAN_POINT('Ctrl Pts',(20.8993630289915,17.8454221176818,-5.50499580250083));
#49988=CARTESIAN_POINT('Ctrl Pts',(20.8545561001606,17.7743728802934,-5.50916691647878));
#49989=CARTESIAN_POINT('Ctrl Pts',(20.8062153221384,17.7054784349764,-5.51333803045673));
#49990=CARTESIAN_POINT('Ctrl Pts',(20.7545808175507,17.6391052326106,-5.51750914443469));
#49991=CARTESIAN_POINT('Ctrl Pts',(20.7029636394196,17.5727543024138,-5.52167885875506));
#49992=CARTESIAN_POINT('Ctrl Pts',(20.6480552119857,17.5089232977413,-5.52584857307543));
#49993=CARTESIAN_POINT('Ctrl Pts',(20.5901376466263,17.4479478065648,-5.53001828739581));
#49994=CARTESIAN_POINT('Ctrl Pts',(20.5322221422224,17.3869744851579,-5.53418785333985));
#49995=CARTESIAN_POINT('Ctrl Pts',(20.4712980302308,17.3288568081792,-5.53835741928389));
#49996=CARTESIAN_POINT('Ctrl Pts',(20.4076852490904,17.2738945080411,-5.54252698522793));
#49997=CARTESIAN_POINT('Ctrl Pts',(20.3418359210399,17.2169998012334,-5.54684314796685));
#49998=CARTESIAN_POINT('Ctrl Pts',(20.2731057379437,17.163486830588,-5.55115931070577));
#49999=CARTESIAN_POINT('Ctrl Pts',(20.2018865153253,17.1136423342391,-5.55547547344469));
#50000=CARTESIAN_POINT('Ctrl Pts',(20.1329872513929,17.065421517116,-5.55965103763637));
#50001=CARTESIAN_POINT('Ctrl Pts',(20.0617590424853,17.0206340542481,-5.56382660182806));
#50002=CARTESIAN_POINT('Ctrl Pts',(19.9885842021593,16.979494122864,-5.56800216601974));
#50003=CARTESIAN_POINT('Ctrl Pts',(19.9117134746051,16.9362763113467,-5.57238862803228));
#50004=CARTESIAN_POINT('Ctrl Pts',(19.8326948219823,16.8970844480459,-5.57677509004481));
#50005=CARTESIAN_POINT('Ctrl Pts',(19.7519960894444,16.8621100575217,-5.58116155205735));
#50006=CARTESIAN_POINT('Ctrl Pts',(19.6712973569065,16.8271356669974,-5.58554801406989));
#50007=CARTESIAN_POINT('Ctrl Pts',(19.5889191146258,16.7963788809358,-5.58993447608243));
#50008=CARTESIAN_POINT('Ctrl Pts',(19.5053461655915,16.7699704850561,-5.59432093809497));
#50009=CARTESIAN_POINT('Ctrl Pts',(19.4256185318271,16.7447771786174,-5.59850557248802));
#50010=CARTESIAN_POINT('Ctrl Pts',(19.3445069543662,16.7234471296282,-5.60269020688107));
#50011=CARTESIAN_POINT('Ctrl Pts',(19.2624206826507,16.7061304261206,-5.60687484127411));
#50012=CARTESIAN_POINT('Ctrl Pts',(19.1804512505827,16.688838370797,-5.61105351935806));
#50013=CARTESIAN_POINT('Ctrl Pts',(19.097510326263,16.6755484082766,-5.615232197442));
#50014=CARTESIAN_POINT('Ctrl Pts',(19.0140230530434,16.6663611081797,-5.61941087552595));
#50015=CARTESIAN_POINT('Ctrl Pts',(18.9290393304527,16.6570091323315,-5.62366445341138));
#50016=CARTESIAN_POINT('Ctrl Pts',(18.8434899394339,16.651908491303,-5.62791803129682));
#50017=CARTESIAN_POINT('Ctrl Pts',(18.7578350465908,16.6511109612809,-5.63217160918225));
#50018=CARTESIAN_POINT('Ctrl Pts',(18.6738407409872,16.6503288929346,-5.6363427231602));
#50019=CARTESIAN_POINT('Ctrl Pts',(18.58974546897,16.6536845805936,-5.64051383713816));
#50020=CARTESIAN_POINT('Ctrl Pts',(18.5059873315598,16.6611744720411,-5.64468495111611));
#50021=CARTESIAN_POINT('Ctrl Pts',(18.4222573000016,16.6686618501832,-5.64885466543648));
#50022=CARTESIAN_POINT('Ctrl Pts',(18.3388646361981,16.6802806360296,-5.65302437975685));
#50023=CARTESIAN_POINT('Ctrl Pts',(18.2562442180638,16.6959752659613,-5.65719409407723));
#50024=CARTESIAN_POINT('Ctrl Pts',(18.1736267399186,16.7116693374106,-5.66136366002127));
#50025=CARTESIAN_POINT('Ctrl Pts',(18.0917819045974,16.7314388778862,-5.66553322596531));
#50026=CARTESIAN_POINT('Ctrl Pts',(18.0111349162343,16.7551771092621,-5.66970279190935));
#50027=CARTESIAN_POINT('Ctrl Pts',(17.9276524792492,16.7797499475689,-5.67401895464827));
#50028=CARTESIAN_POINT('Ctrl Pts',(17.8454541950085,16.8085755987089,-5.67833511738719));
#50029=CARTESIAN_POINT('Ctrl Pts',(17.7649932472177,16.8414798137466,-5.68265128012612));
#50030=CARTESIAN_POINT('Ctrl Pts',(17.6871533063383,16.8733121774403,-5.6868268443178));
#50031=CARTESIAN_POINT('Ctrl Pts',(17.6109396593041,16.9089612248341,-5.69100240850948));
#50032=CARTESIAN_POINT('Ctrl Pts',(17.5367393343476,16.9482214208011,-5.69517797270115));
#50033=CARTESIAN_POINT('Ctrl Pts',(17.458791327372,16.989464555934,-5.6995644347137));
#50034=CARTESIAN_POINT('Ctrl Pts',(17.3830658746254,17.0346929255447,-5.70395089672624));
#50035=CARTESIAN_POINT('Ctrl Pts',(17.3099772536615,17.0836168145088,-5.70833735873878));
#50036=CARTESIAN_POINT('Ctrl Pts',(17.2368886326976,17.1325407034729,-5.71272382075132));
#50037=CARTESIAN_POINT('Ctrl Pts',(17.1664372628671,17.185159703645,-5.71711028276386));
#50038=CARTESIAN_POINT('Ctrl Pts',(17.0989955289255,17.2411369642621,-5.72149674477641));
#50039=CARTESIAN_POINT('Ctrl Pts',(17.0355419517776,17.2938040179914,-5.72562381401755));
#50040=CARTESIAN_POINT('Ctrl Pts',(16.9745020021859,17.3496514870446,-5.72975088325869));
#50041=CARTESIAN_POINT('Ctrl Pts',(16.9162185170908,17.4084267059583,-5.73387795249983));
#50042=CARTESIAN_POINT('Ctrl Pts',(16.8577217299028,17.4674170265802,-5.73802012571948));
#50043=CARTESIAN_POINT('Ctrl Pts',(16.8020020379166,17.5293563204315,-5.74216229893914));
#50044=CARTESIAN_POINT('Ctrl Pts',(16.7493744028763,17.5939467419898,-5.74630447215879));
#50045=CARTESIAN_POINT('Ctrl Pts',(16.6970742796338,17.658135205051,-5.75042086784546));
#50046=CARTESIAN_POINT('Ctrl Pts',(16.6478281605157,17.7249415391099,-5.75453726353214));
#50047=CARTESIAN_POINT('Ctrl Pts',(16.6019085746493,17.7940362905332,-5.75865365921882));
#50048=CARTESIAN_POINT('Ctrl Pts',(16.5560170315912,17.8630888462173,-5.76276754104799));
#50049=CARTESIAN_POINT('Ctrl Pts',(16.5134482524876,17.9344266527044,-5.76688142287718));
#50050=CARTESIAN_POINT('Ctrl Pts',(16.4744330306067,18.0076891046671,-5.77099530470636));
#50051=CARTESIAN_POINT('Ctrl Pts',(16.4354291736145,18.0809302157386,-5.77510798818765));
#50052=CARTESIAN_POINT('Ctrl Pts',(16.3999770407451,18.1560944409467,-5.77922067166894));
#50053=CARTESIAN_POINT('Ctrl Pts',(16.3682620211174,18.2327956168202,-5.78333335515023));
#50054=CARTESIAN_POINT('Ctrl Pts',(16.3361584999703,18.3104363640294,-5.78749641803534));
#50055=CARTESIAN_POINT('Ctrl Pts',(16.3078844956125,18.3896515290332,-5.79165948092045));
#50056=CARTESIAN_POINT('Ctrl Pts',(16.2835818660733,18.4700202641616,-5.79582254380555));
#50057=CARTESIAN_POINT('Ctrl Pts',(16.2595524301163,18.5494855487963,-5.79993880837771));
#50058=CARTESIAN_POINT('Ctrl Pts',(16.2394055983611,18.6300781193828,-5.80405507294986));
#50059=CARTESIAN_POINT('Ctrl Pts',(16.2232275631063,18.7113783730311,-5.80817133752201));
#50060=CARTESIAN_POINT('Ctrl Pts',(16.2067736327736,18.7940650953989,-5.81235779956359));
#50061=CARTESIAN_POINT('Ctrl Pts',(16.1944252132088,18.877483359597,-5.81654426160518));
#50062=CARTESIAN_POINT('Ctrl Pts',(16.186218055036,18.9611857471735,-5.82073072364676));
#50063=CARTESIAN_POINT('Ctrl Pts',(16.1780108968631,19.04488813475,-5.82491718568835));
#50064=CARTESIAN_POINT('Ctrl Pts',(16.1739449655996,19.1288741338656,-5.82910364772993));
#50065=CARTESIAN_POINT('Ctrl Pts',(16.1740005630998,19.2126979607665,-5.83329010977151));
#50066=CARTESIAN_POINT('Ctrl Pts',(16.1712326816491,19.2126997966084,-5.83329010977151));
#50067=CARTESIAN_POINT('Ctrl Pts',(16.1704460797826,19.3154768238875,-5.83841759033362));
#50068=CARTESIAN_POINT('Ctrl Pts',(16.2227680075723,20.2671650151133,-5.88593700645621));
#50069=CARTESIAN_POINT('Ctrl Pts',(17.4141948907083,21.935225591005,-5.97584835813926));
#50070=CARTESIAN_POINT('Ctrl Pts',(19.4492535151759,21.8369133510816,-6.06521460816749));
#50071=CARTESIAN_POINT('Ctrl Pts',(20.2230158477614,21.3000309188846,-6.11218892263521));
#50072=CARTESIAN_POINT('Ctrl Pts',(20.2954006757859,21.2435252751206,-6.11677130154247));
#50073=CARTESIAN_POINT('',(16.1740007055014,19.2090994299067,-5.76670989019962));
#50074=CARTESIAN_POINT('Ctrl Pts',(16.174000705501,19.2090994304895,-5.76670989022851));
#50075=CARTESIAN_POINT('Ctrl Pts',(16.1739381768052,19.293323351932,-5.77088500205647));
#50076=CARTESIAN_POINT('Ctrl Pts',(16.1780364138872,19.3775880720651,-5.77506011388443));
#50077=CARTESIAN_POINT('Ctrl Pts',(16.1862808495761,19.4614538491682,-5.77923522571239));
#50078=CARTESIAN_POINT('Ctrl Pts',(16.1945245019763,19.5453116583386,-5.78340994087067));
#50079=CARTESIAN_POINT('Ctrl Pts',(16.2069135252696,19.6287701442273,-5.78758465602896));
#50080=CARTESIAN_POINT('Ctrl Pts',(16.223381442754,19.7113943045357,-5.79175937118724));
#50081=CARTESIAN_POINT('Ctrl Pts',(16.2398526754153,19.7940350980167,-5.79593492676263));
#50082=CARTESIAN_POINT('Ctrl Pts',(16.2604043427346,19.8758407835677,-5.80011048233803));
#50083=CARTESIAN_POINT('Ctrl Pts',(16.2849190524509,19.9563874914111,-5.80428603791342));
#50084=CARTESIAN_POINT('Ctrl Pts',(16.3094630809744,20.0370305305357,-5.80846658731946));
#50085=CARTESIAN_POINT('Ctrl Pts',(16.3379794801115,20.1164111473512,-5.8126471367255));
#50086=CARTESIAN_POINT('Ctrl Pts',(16.3703013760236,20.1941219736187,-5.81682768613154));
#50087=CARTESIAN_POINT('Ctrl Pts',(16.4026440716426,20.2718828081661,-5.82101092579446));
#50088=CARTESIAN_POINT('Ctrl Pts',(16.4387969424261,20.3479712998167,-5.82519416545737));
#50089=CARTESIAN_POINT('Ctrl Pts',(16.4785465454201,20.4220035979401,-5.82937740512028));
#50090=CARTESIAN_POINT('Ctrl Pts',(16.5183679957904,20.4961697093842,-5.83356820598561));
#50091=CARTESIAN_POINT('Ctrl Pts',(16.5617989238518,20.5682718138333,-5.83775900685093));
#50092=CARTESIAN_POINT('Ctrl Pts',(16.6085819963923,20.6379542073733,-5.84194980771626));
#50093=CARTESIAN_POINT('Ctrl Pts',(16.6388616407129,20.6830550948785,-5.84466224092616));
#50094=CARTESIAN_POINT('Ctrl Pts',(16.6705446814796,20.7271429654286,-5.84737467413607));
#50095=CARTESIAN_POINT('Ctrl Pts',(16.7035527014987,20.770129169764,-5.85008710734598));
#50096=CARTESIAN_POINT('Ctrl Pts',(16.754476165831,20.8364465811684,-5.85427174173903));
#50097=CARTESIAN_POINT('Ctrl Pts',(16.8087468503131,20.900389929485,-5.85845637613208));
#50098=CARTESIAN_POINT('Ctrl Pts',(16.8661152556941,20.9616017771011,-5.86264101052512));
#50099=CARTESIAN_POINT('Ctrl Pts',(16.9234020042509,21.0227264972286,-5.86681968860907));
#50100=CARTESIAN_POINT('Ctrl Pts',(16.9837774037105,21.0811271065654,-5.87099836669302));
#50101=CARTESIAN_POINT('Ctrl Pts',(17.0469505633859,21.1364776546146,-5.87517704477697));
#50102=CARTESIAN_POINT('Ctrl Pts',(17.1112560565466,21.1928203214578,-5.8794306226624));
#50103=CARTESIAN_POINT('Ctrl Pts',(17.1784603025303,21.2460021244014,-5.88368420054784));
#50104=CARTESIAN_POINT('Ctrl Pts',(17.2482157539324,21.2957170489391,-5.88793777843327));
#50105=CARTESIAN_POINT('Ctrl Pts',(17.3166188597925,21.344468152654,-5.89210889241122));
#50106=CARTESIAN_POINT('Ctrl Pts',(17.3874747417498,21.389885323497,-5.89628000638917));
#50107=CARTESIAN_POINT('Ctrl Pts',(17.4604222489457,21.4317205389286,-5.90045112036712));
#50108=CARTESIAN_POINT('Ctrl Pts',(17.5333452779011,21.4735417161497,-5.9046208346875));
#50109=CARTESIAN_POINT('Ctrl Pts',(17.6083581394478,21.5117830963987,-5.90879054900787));
#50110=CARTESIAN_POINT('Ctrl Pts',(17.6850725337914,21.5462411375773,-5.91296026332824));
#50111=CARTESIAN_POINT('Ctrl Pts',(17.7617841983077,21.5806979525909,-5.91712982927229));
#50112=CARTESIAN_POINT('Ctrl Pts',(17.8401968552433,21.6113715084928,-5.92129939521633));
#50113=CARTESIAN_POINT('Ctrl Pts',(17.9199007999998,21.6381057852016,-5.92546896116037));
#50114=CARTESIAN_POINT('Ctrl Pts',(18.0024070371285,21.6657800060992,-5.92978512389929));
#50115=CARTESIAN_POINT('Ctrl Pts',(18.0862965548757,21.6892326159303,-5.93410128663821));
#50116=CARTESIAN_POINT('Ctrl Pts',(18.1710980677304,21.7083468751151,-5.93841744937713));
#50117=CARTESIAN_POINT('Ctrl Pts',(18.2531371802234,21.7268384893174,-5.94259301356881));
#50118=CARTESIAN_POINT('Ctrl Pts',(18.3360293116301,21.7412700216399,-5.94676857776049));
#50119=CARTESIAN_POINT('Ctrl Pts',(18.4193394847882,21.751588270493,-5.95094414195217));
#50120=CARTESIAN_POINT('Ctrl Pts',(18.5068574567412,21.7624276695664,-5.95533060396471));
#50121=CARTESIAN_POINT('Ctrl Pts',(18.5948362284717,21.7687272994046,-5.95971706597725));
#50122=CARTESIAN_POINT('Ctrl Pts',(18.6827702698548,21.7704873538952,-5.96410352798979));
#50123=CARTESIAN_POINT('Ctrl Pts',(18.7707043112379,21.7722474083857,-5.96848999000233));
#50124=CARTESIAN_POINT('Ctrl Pts',(18.8585930447507,21.7694679818952,-5.97287645201487));
#50125=CARTESIAN_POINT('Ctrl Pts',(18.945938282031,21.7622119011579,-5.97726291402741));
#50126=CARTESIAN_POINT('Ctrl Pts',(19.0292570355293,21.7552903148054,-5.98144716675294));
#50127=CARTESIAN_POINT('Ctrl Pts',(19.1123913980882,21.744269959261,-5.98563141947847));
#50128=CARTESIAN_POINT('Ctrl Pts',(19.1949058912311,21.7291671428697,-5.989815672204));
#50129=CARTESIAN_POINT('Ctrl Pts',(19.2773086561187,21.7140847763564,-5.99399425926718));
#50130=CARTESIAN_POINT('Ctrl Pts',(19.3590927697212,21.6949310074223,-5.99817284633035));
#50131=CARTESIAN_POINT('Ctrl Pts',(19.4398267332542,21.6717739885296,-6.00235143339353));
#50132=CARTESIAN_POINT('Ctrl Pts',(19.5204679325005,21.6486435773276,-6.00652521921036));
#50133=CARTESIAN_POINT('Ctrl Pts',(19.6000609401169,21.6215191846142,-6.01069900502718));
#50134=CARTESIAN_POINT('Ctrl Pts',(19.6781847982248,21.5905199235983,-6.01487279084401));
#50135=CARTESIAN_POINT('Ctrl Pts',(19.7562551368422,21.5595418989204,-6.01904371736924));
#50136=CARTESIAN_POINT('Ctrl Pts',(19.8328578987203,21.5246944476579,-6.02321464389447));
#50137=CARTESIAN_POINT('Ctrl Pts',(19.9075887387111,21.4861460331967,-6.02738557041971));
#50138=CARTESIAN_POINT('Ctrl Pts',(19.9823054028883,21.4476049310463,-6.03155570575516));
#50139=CARTESIAN_POINT('Ctrl Pts',(20.0551504373937,21.4053644619575,-6.03572584109061));
#50140=CARTESIAN_POINT('Ctrl Pts',(20.1257419130185,21.3596401391456,-6.03989597642606));
#50141=CARTESIAN_POINT('Ctrl Pts',(20.1832317936462,21.3224021321912,-6.04329214544667));
#50142=CARTESIAN_POINT('Ctrl Pts',(20.2392273245281,21.2828543953029,-6.04668831446728));
#50143=CARTESIAN_POINT('Ctrl Pts',(20.2935358855687,21.2411349269503,-6.05008448348788));
#50144=CARTESIAN_POINT('Ctrl Pts',(20.2935358855687,21.2411349269503,-5.2501823431226));
#50145=CARTESIAN_POINT('Ctrl Pts',(20.3601377596623,21.1899718188651,-5.2543537748487));
#50146=CARTESIAN_POINT('Ctrl Pts',(20.4242723999887,21.1354869667526,-5.25852520657481));
#50147=CARTESIAN_POINT('Ctrl Pts',(20.4855962900899,21.0779521784297,-5.26269663830092));
#50148=CARTESIAN_POINT('Ctrl Pts',(20.5468968447462,21.020439283693,-5.2668664826813));
#50149=CARTESIAN_POINT('Ctrl Pts',(20.6053884380554,20.9598790719395,-5.27103632706169));
#50150=CARTESIAN_POINT('Ctrl Pts',(20.6607620024634,20.8965824470678,-5.27520617144207));
#50151=CARTESIAN_POINT('Ctrl Pts',(20.7161311064392,20.833290920844,-5.27937567993459));
#50152=CARTESIAN_POINT('Ctrl Pts',(20.7683823782338,20.7672637661809,-5.2835451884271));
#50153=CARTESIAN_POINT('Ctrl Pts',(20.8172458070711,20.6988463991019,-5.28771469691962));
#50154=CARTESIAN_POINT('Ctrl Pts',(20.866119957485,20.630414019936,-5.29188512028253));
#50155=CARTESIAN_POINT('Ctrl Pts',(20.9116045226243,20.5595907619903,-5.29605554364545));
#50156=CARTESIAN_POINT('Ctrl Pts',(20.9534725319694,20.4867514177274,-5.30022596700836));
#50157=CARTESIAN_POINT('Ctrl Pts',(20.9953878196887,20.4138298215057,-5.30440109971475));
#50158=CARTESIAN_POINT('Ctrl Pts',(21.0336781736472,20.3388879958581,-5.30857623242114));
#50159=CARTESIAN_POINT('Ctrl Pts',(21.0681626406287,20.2623252432493,-5.31275136512752));
#50160=CARTESIAN_POINT('Ctrl Pts',(21.1026701956664,20.1857112303112,-5.31692929317068));
#50161=CARTESIAN_POINT('Ctrl Pts',(21.1333666251999,20.1074745584388,-5.32110722121383));
#50162=CARTESIAN_POINT('Ctrl Pts',(21.1601200329157,20.0280321816703,-5.32528514925698));
#50163=CARTESIAN_POINT('Ctrl Pts',(21.1869161592313,19.9484629550019,-5.32946974842172));
#50164=CARTESIAN_POINT('Ctrl Pts',(21.2097565773899,19.8676846237838,-5.33365434758646));
#50165=CARTESIAN_POINT('Ctrl Pts',(21.228560023284,19.7861263254567,-5.3378389467512));
#50166=CARTESIAN_POINT('Ctrl Pts',(21.2338697291507,19.7630959416884,-5.33902059137422));
#50167=CARTESIAN_POINT('Ctrl Pts',(21.2388578511548,19.7400034037589,-5.34020223599723));
#50168=CARTESIAN_POINT('Ctrl Pts',(21.2435233083642,19.7168584434175,-5.34138388062024));
#50169=CARTESIAN_POINT('Ctrl Pts',(21.2600453931921,19.6348937010711,-5.34556851501328));
#50170=CARTESIAN_POINT('Ctrl Pts',(21.2725783676241,19.5519661209787,-5.34975314940633));
#50171=CARTESIAN_POINT('Ctrl Pts',(21.2810167729394,19.4684986570167,-5.35393778379938));
#50172=CARTESIAN_POINT('Ctrl Pts',(21.2894431672291,19.3851499986585,-5.35811646188331));
#50173=CARTESIAN_POINT('Ctrl Pts',(21.2937865229904,19.3012634366148,-5.36229513996725));
#50174=CARTESIAN_POINT('Ctrl Pts',(21.293992315731,19.2172724316081,-5.36647381805119));
#50175=CARTESIAN_POINT('Ctrl Pts',(21.2942017971586,19.1317759481998,-5.37072739593663));
#50176=CARTESIAN_POINT('Ctrl Pts',(21.2901238296771,19.0461717133525,-5.37498097382206));
#50177=CARTESIAN_POINT('Ctrl Pts',(21.2817561480521,18.9609227917973,-5.3792345517075));
#50178=CARTESIAN_POINT('Ctrl Pts',(21.2735506902637,18.877326586936,-5.38340566568545));
#50179=CARTESIAN_POINT('Ctrl Pts',(21.2612204100085,18.7940725203437,-5.38757677966341));
#50180=CARTESIAN_POINT('Ctrl Pts',(21.2448156932503,18.7115958004501,-5.39174789364136));
#50181=CARTESIAN_POINT('Ctrl Pts',(21.2284164812532,18.6291467564165,-5.39591760796173));
#50182=CARTESIAN_POINT('Ctrl Pts',(21.2079456377352,18.547474991856,-5.4000873222821));
#50183=CARTESIAN_POINT('Ctrl Pts',(21.18350491705,18.4670069480513,-5.40425703660247));
#50184=CARTESIAN_POINT('Ctrl Pts',(21.1590650660706,18.3865417676451,-5.4084266025465));
#50185=CARTESIAN_POINT('Ctrl Pts',(21.1306557533069,18.3072806627598,-5.41259616849054));
#50186=CARTESIAN_POINT('Ctrl Pts',(21.0984286192899,18.2296349790813,-5.41676573443457));
#50187=CARTESIAN_POINT('Ctrl Pts',(21.0650684189972,18.1492593689506,-5.4210818971735));
#50188=CARTESIAN_POINT('Ctrl Pts',(21.0276171353227,18.0706153771464,-5.42539805991242));
#50189=CARTESIAN_POINT('Ctrl Pts',(20.9862964849995,17.9941349525692,-5.42971422265135));
#50190=CARTESIAN_POINT('Ctrl Pts',(20.9463218505145,17.9201458697782,-5.43388978684303));
#50191=CARTESIAN_POINT('Ctrl Pts',(20.9027263517809,17.8481819408659,-5.43806535103471));
#50192=CARTESIAN_POINT('Ctrl Pts',(20.8557557370749,17.7786059926858,-5.44224091522639));
#50193=CARTESIAN_POINT('Ctrl Pts',(20.8064127482821,17.7055159287641,-5.44662737723894));
#50194=CARTESIAN_POINT('Ctrl Pts',(20.7533450801513,17.6350618855125,-5.45101383925148));
#50195=CARTESIAN_POINT('Ctrl Pts',(20.6968850924156,17.5676247799201,-5.45540030126403));
#50196=CARTESIAN_POINT('Ctrl Pts',(20.6404251046799,17.5001876743278,-5.45978676327658));
#50197=CARTESIAN_POINT('Ctrl Pts',(20.5805732479926,17.4357678796897,-5.46417322528913));
#50198=CARTESIAN_POINT('Ctrl Pts',(20.5177042670235,17.3746996193972,-5.46855968730167));
#50199=CARTESIAN_POINT('Ctrl Pts',(20.4577279810631,17.3164412002857,-5.47274432169472));
#50200=CARTESIAN_POINT('Ctrl Pts',(20.3947828711329,17.2610158259165,-5.47692895608776));
#50201=CARTESIAN_POINT('Ctrl Pts',(20.3291674917036,17.208741107296,-5.48111359048081));
#50202=CARTESIAN_POINT('Ctrl Pts',(20.2636455076451,17.156540795267,-5.48529226856476));
#50203=CARTESIAN_POINT('Ctrl Pts',(20.1954611603976,17.1074825154228,-5.48947094664871));
#50204=CARTESIAN_POINT('Ctrl Pts',(20.1249494087588,17.0618467383005,-5.49364962473266));
#50205=CARTESIAN_POINT('Ctrl Pts',(20.0531737846479,17.0153929726713,-5.4979032026181));
#50206=CARTESIAN_POINT('Ctrl Pts',(19.9789868438522,16.9724859492608,-5.50215678050353));
#50207=CARTESIAN_POINT('Ctrl Pts',(19.9027767244007,16.9333782209289,-5.50641035838897));
#50208=CARTESIAN_POINT('Ctrl Pts',(19.8280440868266,16.8950286722232,-5.51058147236691));
#50209=CARTESIAN_POINT('Ctrl Pts',(19.7513664452244,16.8603326394005,-5.51475258634486));
#50210=CARTESIAN_POINT('Ctrl Pts',(19.6731370139767,16.8294833259079,-5.51892370032281));
#50211=CARTESIAN_POINT('Ctrl Pts',(19.5949338333702,16.7986443642003,-5.52309341464318));
#50212=CARTESIAN_POINT('Ctrl Pts',(19.5151803248757,16.7716497268886,-5.52726312896355));
#50213=CARTESIAN_POINT('Ctrl Pts',(19.434290135828,16.7486446792427,-5.53143284328392));
#50214=CARTESIAN_POINT('Ctrl Pts',(19.3534028252003,16.725640450215,-5.53560240922796));
#50215=CARTESIAN_POINT('Ctrl Pts',(19.2713793571596,16.7066256536093,-5.53977197517201));
#50216=CARTESIAN_POINT('Ctrl Pts',(19.1886476884741,16.6916954373547,-5.54394154111605));
#50217=CARTESIAN_POINT('Ctrl Pts',(19.1030072763782,16.6762402931151,-5.54825770385497));
#50218=CARTESIAN_POINT('Ctrl Pts',(19.0166084554192,16.6651623947289,-5.5525738665939));
#50219=CARTESIAN_POINT('Ctrl Pts',(18.9299344373275,16.6585091192584,-5.55689002933282));
#50220=CARTESIAN_POINT('Ctrl Pts',(18.8460838162587,16.6520725735365,-5.5610655935245));
#50221=CARTESIAN_POINT('Ctrl Pts',(18.7619761239716,16.6497767790178,-5.56524115771618));
#50222=CARTESIAN_POINT('Ctrl Pts',(18.6780494593125,16.6516114915869,-5.56941672190786));
#50223=CARTESIAN_POINT('Ctrl Pts',(18.5898838583381,16.6535388711264,-5.5738031839204));
#50224=CARTESIAN_POINT('Ctrl Pts',(18.5019186353064,16.6600249445383,-5.57818964593294));
#50225=CARTESIAN_POINT('Ctrl Pts',(18.4146539811437,16.670996433026,-5.58257610794548));
#50226=CARTESIAN_POINT('Ctrl Pts',(18.3273893269809,16.6819679215137,-5.58696256995803));
#50227=CARTESIAN_POINT('Ctrl Pts',(18.2408257994993,16.6974246482065,-5.59134903197057));
#50228=CARTESIAN_POINT('Ctrl Pts',(18.1554472698611,16.7172324209243,-5.59573549398311));
#50229=CARTESIAN_POINT('Ctrl Pts',(18.073997132933,16.7361288086573,-5.59992012837615));
#50230=CARTESIAN_POINT('Ctrl Pts',(17.9933221701874,16.7590549809083,-5.6041047627692));
#50231=CARTESIAN_POINT('Ctrl Pts',(17.9138510440902,16.7859318174286,-5.60828939716224));
#50232=CARTESIAN_POINT('Ctrl Pts',(17.8344930353039,16.812770398099,-5.6124680752462));
#50233=CARTESIAN_POINT('Ctrl Pts',(17.7563358916492,16.8435483273115,-5.61664675333017));
#50234=CARTESIAN_POINT('Ctrl Pts',(17.6797967513065,16.878135771108,-5.62082543141413));
#50235=CARTESIAN_POINT('Ctrl Pts',(17.6018857018813,16.9133431699767,-5.62507900929956));
#50236=CARTESIAN_POINT('Ctrl Pts',(17.5256517013906,16.9524978888719,-5.629332587185));
#50237=CARTESIAN_POINT('Ctrl Pts',(17.4515171985758,16.9954102672085,-5.63358616507043));
#50238=CARTESIAN_POINT('Ctrl Pts',(17.3788199377597,17.0374907053544,-5.63775727904838));
#50239=CARTESIAN_POINT('Ctrl Pts',(17.3081419118292,17.0831841629374,-5.64192839302633));
#50240=CARTESIAN_POINT('Ctrl Pts',(17.2398584137958,17.1322645862508,-5.64609950700428));
#50241=CARTESIAN_POINT('Ctrl Pts',(17.1715978289495,17.1813285401541,-5.65026922132465));
#50242=CARTESIAN_POINT('Ctrl Pts',(17.1057305494612,17.2337769343487,-5.65443893564503));
#50243=CARTESIAN_POINT('Ctrl Pts',(17.0426026198909,17.2893405862224,-5.6586086499654));
#50244=CARTESIAN_POINT('Ctrl Pts',(16.9794769366833,17.3449022609028,-5.66277821590943));
#50245=CARTESIAN_POINT('Ctrl Pts',(16.9190907543426,17.4035786682712,-5.66694778185347));
#50246=CARTESIAN_POINT('Ctrl Pts',(16.8617557221014,17.4650614661805,-5.67111734779751));
#50247=CARTESIAN_POINT('Ctrl Pts',(16.8024048608568,17.5287059234172,-5.67543351053642));
#50248=CARTESIAN_POINT('Ctrl Pts',(16.7463240583277,17.5953574026463,-5.67974967327534));
#50249=CARTESIAN_POINT('Ctrl Pts',(16.6938147044704,17.6646352435778,-5.68406583601426));
#50250=CARTESIAN_POINT('Ctrl Pts',(16.643015837292,17.7316563661277,-5.68824140020594));
#50251=CARTESIAN_POINT('Ctrl Pts',(16.5955595388127,17.8011349549805,-5.69241696439763));
#50252=CARTESIAN_POINT('Ctrl Pts',(16.5516743299489,17.8726970933918,-5.69659252858931));
#50253=CARTESIAN_POINT('Ctrl Pts',(16.5055725835126,17.9478736652914,-5.70097899060185));
#50254=CARTESIAN_POINT('Ctrl Pts',(16.4634124379741,18.0253492855824,-5.70536545261439));
#50255=CARTESIAN_POINT('Ctrl Pts',(16.4254030213233,18.1046637084299,-5.70975191462692));
#50256=CARTESIAN_POINT('Ctrl Pts',(16.3873936046726,18.1839781312775,-5.71413837663946));
#50257=CARTESIAN_POINT('Ctrl Pts',(16.3535350701226,18.265130791913,-5.718524838652));
#50258=CARTESIAN_POINT('Ctrl Pts',(16.3239764935691,18.3476421955815,-5.72291130066454));
#50259=CARTESIAN_POINT('Ctrl Pts',(16.2911969765864,18.4391447059584,-5.72777574688621));
#50260=CARTESIAN_POINT('Ctrl Pts',(16.2636032939179,18.5325974942141,-5.73264019310788));
#50261=CARTESIAN_POINT('Ctrl Pts',(16.2413973788042,18.6274486545232,-5.73750463932955));
#50262=CARTESIAN_POINT('Ctrl Pts',(16.2191773325015,18.7223601753114,-5.74237218114123));
#50263=CARTESIAN_POINT('Ctrl Pts',(16.2023520711405,18.818671733483,-5.74723972295291));
#50264=CARTESIAN_POINT('Ctrl Pts',(16.191076093449,18.9158085274076,-5.75210726476459));
#50265=CARTESIAN_POINT('Ctrl Pts',(16.1798001157575,19.0129453213322,-5.75697480657626));
#50266=CARTESIAN_POINT('Ctrl Pts',(16.1740736044194,19.1109072194811,-5.76184234838794));
#50267=CARTESIAN_POINT('Ctrl Pts',(16.1740007055014,19.2090994299067,-5.76670989019962));
#50268=CARTESIAN_POINT('Origin',(18.734,19.211,1.76670989022852));
#50269=CARTESIAN_POINT('',(20.2961058327006,21.2444858570038,-4.45010593307017));
#50270=CARTESIAN_POINT('',(20.2910030748979,21.2378274151617,-4.51667470337929));
#50271=CARTESIAN_POINT('',(20.2935358855687,21.2411349269503,1.76670989022852));
#50272=CARTESIAN_POINT('',(16.1741505041835,19.2121967451321,-5.03329016024809));
#50273=CARTESIAN_POINT('Ctrl Pts',(20.2910030748979,21.2378274151617,-4.51667470337929));
#50274=CARTESIAN_POINT('Ctrl Pts',(20.6127492989713,20.9913952836578,-4.53675463046736));
#50275=CARTESIAN_POINT('Ctrl Pts',(21.4403820747963,20.0000799362034,-4.59922649311591));
#50276=CARTESIAN_POINT('Ctrl Pts',(21.3050299007693,17.61315900461,-4.70409029132493));
#50277=CARTESIAN_POINT('Ctrl Pts',(18.7821183085442,16.1842897024026,-4.83126609800637));
#50278=CARTESIAN_POINT('Ctrl Pts',(16.5671405518731,17.3473640177625,-4.94099937082189));
#50279=CARTESIAN_POINT('Ctrl Pts',(16.1797898343239,18.7088775035926,-5.00834070807693));
#50280=CARTESIAN_POINT('Ctrl Pts',(16.1776748250889,19.2121940791439,-5.0332901097715));
#50281=CARTESIAN_POINT('Ctrl Pts',(16.1740002797795,19.2121968587701,-5.03329016239966));
#50282=CARTESIAN_POINT('Ctrl Pts',(16.1740435234787,19.3046921980315,-5.03786858507908));
#50283=CARTESIAN_POINT('Ctrl Pts',(16.1791038614083,19.3970207371689,-5.0424470077585));
#50284=CARTESIAN_POINT('Ctrl Pts',(16.1891023385012,19.4886614710357,-5.04702543043792));
#50285=CARTESIAN_POINT('Ctrl Pts',(16.199131888135,19.5805869993194,-5.05161808160682));
#50286=CARTESIAN_POINT('Ctrl Pts',(16.2141301908471,19.6718201549905,-5.05621073277571));
#50287=CARTESIAN_POINT('Ctrl Pts',(16.2339673694789,19.7618510200861,-5.0608033839446));
#50288=CARTESIAN_POINT('Ctrl Pts',(16.2538962421947,19.8522980379953,-5.06541726388547));
#50289=CARTESIAN_POINT('Ctrl Pts',(16.2787086950664,19.9415313458139,-5.07003114382633));
#50290=CARTESIAN_POINT('Ctrl Pts',(16.3082244096461,20.0290542679085,-5.07464502376719));
#50291=CARTESIAN_POINT('Ctrl Pts',(16.331622411587,20.0984363421765,-5.07830258630121));
#50292=CARTESIAN_POINT('Ctrl Pts',(16.3579750606107,20.1667439285256,-5.08196014883522));
#50293=CARTESIAN_POINT('Ctrl Pts',(16.3871718743355,20.233740313369,-5.08561771136923));
#50294=CARTESIAN_POINT('Ctrl Pts',(16.4205760854035,20.310391190454,-5.08980234576228));
#50295=CARTESIAN_POINT('Ctrl Pts',(16.457801705802,20.385546444256,-5.09398698015532));
#50296=CARTESIAN_POINT('Ctrl Pts',(16.4986929228154,20.4587989704629,-5.09817161454837));
#50297=CARTESIAN_POINT('Ctrl Pts',(16.5395259362427,20.5319472307656,-5.10235029263232));
#50298=CARTESIAN_POINT('Ctrl Pts',(16.5840139603303,20.6031977447539,-5.10652897071627));
#50299=CARTESIAN_POINT('Ctrl Pts',(16.6319534129312,20.6721639695094,-5.11070764880021));
#50300=CARTESIAN_POINT('Ctrl Pts',(16.6807521457666,20.7423663642785,-5.11496122668565));
#50301=CARTESIAN_POINT('Ctrl Pts',(16.7331270652481,20.8102013305708,-5.11921480457108));
#50302=CARTESIAN_POINT('Ctrl Pts',(16.7888147952353,20.8752879916542,-5.12346838245652));
#50303=CARTESIAN_POINT('Ctrl Pts',(16.843422909911,20.9391128208063,-5.12763949643447));
#50304=CARTESIAN_POINT('Ctrl Pts',(16.9012162179244,21.0002945906744,-5.13181061041243));
#50305=CARTESIAN_POINT('Ctrl Pts',(16.9619041398262,21.0585054160556,-5.13598172439038));
#50306=CARTESIAN_POINT('Ctrl Pts',(17.0225716973097,21.1166967082321,-5.14015143871075));
#50307=CARTESIAN_POINT('Ctrl Pts',(17.0861316079122,21.1719187176575,-5.14432115303112));
#50308=CARTESIAN_POINT('Ctrl Pts',(17.1522562065727,21.2238801683047,-5.14849086735149));
#50309=CARTESIAN_POINT('Ctrl Pts',(17.2183784522363,21.2758397699405,-5.15266043329554));
#50310=CARTESIAN_POINT('Ctrl Pts',(17.2870648422625,21.3245387599152,-5.15682999923959));
#50311=CARTESIAN_POINT('Ctrl Pts',(17.3579554657573,21.3697268098999,-5.16099956518364));
#50312=CARTESIAN_POINT('Ctrl Pts',(17.4313385161211,21.4165036159766,-5.16531572792256));
#50313=CARTESIAN_POINT('Ctrl Pts',(17.5070832408528,21.4595177156541,-5.16963189066148));
#50314=CARTESIAN_POINT('Ctrl Pts',(17.5847604857698,21.4985420299815,-5.1739480534004));
#50315=CARTESIAN_POINT('Ctrl Pts',(17.6599074026039,21.5362951313744,-5.17812361759208));
#50316=CARTESIAN_POINT('Ctrl Pts',(17.7368624194981,21.5703142429023,-5.18229918178376));
#50317=CARTESIAN_POINT('Ctrl Pts',(17.8152162748905,21.6004427104398,-5.18647474597544));
#50318=CARTESIAN_POINT('Ctrl Pts',(17.8975275972502,21.632092895249,-5.19086120798798));
#50319=CARTESIAN_POINT('Ctrl Pts',(17.9813822273946,21.6594488930309,-5.19524767000052));
#50320=CARTESIAN_POINT('Ctrl Pts',(18.0662895457781,21.6823888300554,-5.19963413201305));
#50321=CARTESIAN_POINT('Ctrl Pts',(18.1511968641616,21.70532876708,-5.20402059402559));
#50322=CARTESIAN_POINT('Ctrl Pts',(18.2371562875637,21.723852595477,-5.20840705603813));
#50323=CARTESIAN_POINT('Ctrl Pts',(18.3236691980734,21.7379009939035,-5.21279351805067));
#50324=CARTESIAN_POINT('Ctrl Pts',(18.408989825629,21.7517557834699,-5.21711952776937));
#50325=CARTESIAN_POINT('Ctrl Pts',(18.4951771222118,21.7613111070864,-5.22144553748807));
#50326=CARTESIAN_POINT('Ctrl Pts',(18.5817594759544,21.7664691981783,-5.22577154720677));
#50327=CARTESIAN_POINT('Ctrl Pts',(18.6653746425121,21.7714505208975,-5.22994930407667));
#50328=CARTESIAN_POINT('Ctrl Pts',(18.7493577223217,21.7723310236273,-5.23412706094656));
#50329=CARTESIAN_POINT('Ctrl Pts',(18.8332735539207,21.7690744245412,-5.23830481781645));
#50330=CARTESIAN_POINT('Ctrl Pts',(18.9171071868207,21.7658210154159,-5.24247848241707));
#50331=CARTESIAN_POINT('Ctrl Pts',(19.0008732452765,21.7584385686514,-5.24665214701768));
#50332=CARTESIAN_POINT('Ctrl Pts',(19.0841345036665,21.7469427890515,-5.2508258116183));
#50333=CARTESIAN_POINT('Ctrl Pts',(19.167339184286,21.7354548210748,-5.25499664012632));
#50334=CARTESIAN_POINT('Ctrl Pts',(19.2500392918514,21.7198591351502,-5.25916746863435));
#50335=CARTESIAN_POINT('Ctrl Pts',(19.3318020308339,21.7002233190156,-5.26333829714237));
#50336=CARTESIAN_POINT('Ctrl Pts',(19.4135337382729,21.6805949552937,-5.26750754268916));
#50337=CARTESIAN_POINT('Ctrl Pts',(19.4943283376287,21.6569296169492,-5.27167678823594));
#50338=CARTESIAN_POINT('Ctrl Pts',(19.5737638923663,21.6293458406683,-5.27584603378273));
#50339=CARTESIAN_POINT('Ctrl Pts',(19.6532187793364,21.6017553513233,-5.28001629399888));
#50340=CARTESIAN_POINT('Ctrl Pts',(19.7313135243688,21.5702446646857,-5.28418655421504));
#50341=CARTESIAN_POINT('Ctrl Pts',(19.8076429172256,21.5349816880284,-5.28835681443119));
#50342=CARTESIAN_POINT('Ctrl Pts',(19.8839842507333,21.4997131949786,-5.29252772702541));
#50343=CARTESIAN_POINT('Ctrl Pts',(19.9585592699248,21.4606914475138,-5.29669863961962));
#50344=CARTESIAN_POINT('Ctrl Pts',(20.0309859635671,21.4181310360533,-5.30086955221384));
#50345=CARTESIAN_POINT('Ctrl Pts',(20.1034742979777,21.3755344023614,-5.30504401458015));
#50346=CARTESIAN_POINT('Ctrl Pts',(20.1738102692344,21.3293933401784,-5.30921847694646));
#50347=CARTESIAN_POINT('Ctrl Pts',(20.2416402519882,21.2799661356787,-5.31339293931278));
#50348=CARTESIAN_POINT('Ctrl Pts',(20.2591066881619,21.2672384734032,-5.31446787664168));
#50349=CARTESIAN_POINT('Ctrl Pts',(20.2764071251532,21.25429312456,-5.31554281397059));
#50350=CARTESIAN_POINT('Ctrl Pts',(20.2935358855687,21.2411349269503,-5.31661775129949));
#50351=CARTESIAN_POINT('',(16.1737368487789,19.2101644346317,-4.96670989022851));
#50352=CARTESIAN_POINT('Ctrl Pts',(16.1740001363332,19.210164520558,-4.96670989022851));
#50353=CARTESIAN_POINT('Ctrl Pts',(16.1739730621524,19.2931227545131,-4.97085977152528));
#50354=CARTESIAN_POINT('Ctrl Pts',(16.1779827035226,19.3762448671897,-4.97500965282206));
#50355=CARTESIAN_POINT('Ctrl Pts',(16.1860506816107,19.4591013319584,-4.97915953411883));
#50356=CARTESIAN_POINT('Ctrl Pts',(16.194107496698,19.5418431550195,-4.98330367356457));
#50357=CARTESIAN_POINT('Ctrl Pts',(16.2062114544436,19.6243195978693,-4.9874478130103));
#50358=CARTESIAN_POINT('Ctrl Pts',(16.2223321624273,19.7061006702712,-4.99159195245604));
#50359=CARTESIAN_POINT('Ctrl Pts',(16.2384354396281,19.7877933155319,-4.99573161098225));
#50360=CARTESIAN_POINT('Ctrl Pts',(16.2585467481878,19.8687916269891,-4.99987126950846));
#50361=CARTESIAN_POINT('Ctrl Pts',(16.2825840079949,19.9486717658564,-5.00401092803467));
#50362=CARTESIAN_POINT('Ctrl Pts',(16.3066073287287,20.0285055826754,-5.00814818599591));
#50363=CARTESIAN_POINT('Ctrl Pts',(16.3345519481597,20.1072220663068,-5.01228544395717));
#50364=CARTESIAN_POINT('Ctrl Pts',(16.3662852025772,20.1844097996554,-5.01642270191841));
#50365=CARTESIAN_POINT('Ctrl Pts',(16.398009961529,20.2615768686959,-5.02055885227397));
#50366=CARTESIAN_POINT('Ctrl Pts',(16.4335211635115,20.3372155671951,-5.02469500262952));
#50367=CARTESIAN_POINT('Ctrl Pts',(16.4726375176033,20.4109332161453,-5.02883115298508));
#50368=CARTESIAN_POINT('Ctrl Pts',(16.5117556109319,20.4846541428151,-5.03296748724695));
#50369=CARTESIAN_POINT('Ctrl Pts',(16.5544789534247,20.5564534375443,-5.03710382150882));
#50370=CARTESIAN_POINT('Ctrl Pts',(16.6005803897988,20.6259631680044,-5.04124015577069));
#50371=CARTESIAN_POINT('Ctrl Pts',(16.6467285005472,20.6955432720456,-5.04538067777221));
#50372=CARTESIAN_POINT('Ctrl Pts',(16.6962612737686,20.7628287929976,-5.04952119977374));
#50373=CARTESIAN_POINT('Ctrl Pts',(16.7489086678718,20.827481488638,-5.05366172177526));
#50374=CARTESIAN_POINT('Ctrl Pts',(16.8015842228015,20.8921687666805,-5.0578044585212));
#50375=CARTESIAN_POINT('Ctrl Pts',(16.8573774008546,20.9542200685977,-5.06194719526713));
#50376=CARTESIAN_POINT('Ctrl Pts',(16.9159800655225,21.0133327988588,-5.06608993201307));
#50377=CARTESIAN_POINT('Ctrl Pts',(16.9746826938387,21.0725463628314,-5.07023973538442));
#50378=CARTESIAN_POINT('Ctrl Pts',(17.0362040315226,21.1288110311767,-5.07438953875576));
#50379=CARTESIAN_POINT('Ctrl Pts',(17.1002018437174,21.1818636646221,-5.07853934212711));
#50380=CARTESIAN_POINT('Ctrl Pts',(17.1438608301668,21.2180559050325,-5.08137031717053));
#50381=CARTESIAN_POINT('Ctrl Pts',(17.1886716656524,21.2527541562677,-5.08420129221395));
#50382=CARTESIAN_POINT('Ctrl Pts',(17.2345184376715,21.2858867545572,-5.08703226725736));
#50383=CARTESIAN_POINT('Ctrl Pts',(17.302287307428,21.3348620398235,-5.09121690165041));
#50384=CARTESIAN_POINT('Ctrl Pts',(17.3725842232475,21.38060482739,-5.09540153604346));
#50385=CARTESIAN_POINT('Ctrl Pts',(17.4450678487465,21.4228440065848,-5.09958617043651));
#50386=CARTESIAN_POINT('Ctrl Pts',(17.5174483027762,21.4650230635361,-5.10376484852045));
#50387=CARTESIAN_POINT('Ctrl Pts',(17.5920088899903,21.5037081881329,-5.10794352660439));
#50388=CARTESIAN_POINT('Ctrl Pts',(17.6683776217253,21.53867028312,-5.11212220468833));
#50389=CARTESIAN_POINT('Ctrl Pts',(17.7461152080914,21.574259048533,-5.11637578257376));
#50390=CARTESIAN_POINT('Ctrl Pts',(17.8257260077701,21.6059897185084,-5.1206293604592));
#50391=CARTESIAN_POINT('Ctrl Pts',(17.9067894477688,21.6336685085412,-5.12488293834464));
#50392=CARTESIAN_POINT('Ctrl Pts',(17.9862813148009,21.6608106912186,-5.12905405232259));
#50393=CARTESIAN_POINT('Ctrl Pts',(18.0671695448449,21.6840565436589,-5.13322516630054));
#50394=CARTESIAN_POINT('Ctrl Pts',(18.1490371223203,21.7032717411504,-5.1373962802785));
#50395=CARTESIAN_POINT('Ctrl Pts',(18.2308772283394,21.7224804907968,-5.14156599459887));
#50396=CARTESIAN_POINT('Ctrl Pts',(18.3136955816371,21.7376611666003,-5.14573570891925));
#50397=CARTESIAN_POINT('Ctrl Pts',(18.3970618790071,21.7487298324727,-5.14990542323963));
#50398=CARTESIAN_POINT('Ctrl Pts',(18.4804252098465,21.7597981044744,-5.15407498918367));
#50399=CARTESIAN_POINT('Ctrl Pts',(18.5643359898477,21.7667545977695,-5.15824455512772));
#50400=CARTESIAN_POINT('Ctrl Pts',(18.6483570024155,21.7695670358552,-5.16241412107176));
#50401=CARTESIAN_POINT('Ctrl Pts',(18.735332090134,21.7724783557944,-5.16673028381068));
#50402=CARTESIAN_POINT('Ctrl Pts',(18.8224247790693,21.7709487709587,-5.1710464465496));
#50403=CARTESIAN_POINT('Ctrl Pts',(18.9091500846463,21.7650012623036,-5.17536260928853));
#50404=CARTESIAN_POINT('Ctrl Pts',(18.993050322516,21.7592474931173,-5.1795381734802));
#50405=CARTESIAN_POINT('Ctrl Pts',(19.0766062822591,21.7493593099811,-5.18371373767188));
#50406=CARTESIAN_POINT('Ctrl Pts',(19.1593859487962,21.735410187463,-5.18788930186356));
#50407=CARTESIAN_POINT('Ctrl Pts',(19.2463466195001,21.7207565279273,-5.1922757638761));
#50408=CARTESIAN_POINT('Ctrl Pts',(19.3324499449363,21.7016210383821,-5.19666222588864));
#50409=CARTESIAN_POINT('Ctrl Pts',(19.4172115835234,21.6781485427796,-5.20104868790118));
#50410=CARTESIAN_POINT('Ctrl Pts',(19.5019732221104,21.6546760471771,-5.20543514991372));
#50411=CARTESIAN_POINT('Ctrl Pts',(19.5853926474676,21.6268668011754,-5.20982161192626));
#50412=CARTESIAN_POINT('Ctrl Pts',(19.6670104728636,21.5949235427183,-5.2142080739388));
#50413=CARTESIAN_POINT('Ctrl Pts',(19.7448664736172,21.5644525721622,-5.21839236074254));
#50414=CARTESIAN_POINT('Ctrl Pts',(19.821373063145,21.5301068697127,-5.22257664754627));
#50415=CARTESIAN_POINT('Ctrl Pts',(19.8961176236051,21.4920266611564,-5.22676093435));
#50416=CARTESIAN_POINT('Ctrl Pts',(19.9707478771509,21.4540046886926,-5.23093882212068));
#50417=CARTESIAN_POINT('Ctrl Pts',(20.0436210503422,21.4122597663648,-5.23511670989136));
#50418=CARTESIAN_POINT('Ctrl Pts',(20.1143433780777,21.3669805561732,-5.23929459766204));
#50419=CARTESIAN_POINT('Ctrl Pts',(20.1757784656169,21.3276474016958,-5.24292384614889));
#50420=CARTESIAN_POINT('Ctrl Pts',(20.2355906124235,21.2856480928829,-5.24655309463575));
#50421=CARTESIAN_POINT('Ctrl Pts',(20.2935358855687,21.2411349269503,-5.2501823431226));
#50422=CARTESIAN_POINT('Ctrl Pts',(20.296105832701,21.2444858570035,-4.4501059330702));
#50423=CARTESIAN_POINT('Ctrl Pts',(20.3016500430467,21.2402338391459,-4.4504550333302));
#50424=CARTESIAN_POINT('Ctrl Pts',(20.9781025843879,20.7166175212097,-4.49319606915068));
#50425=CARTESIAN_POINT('Ctrl Pts',(21.748497275926,18.9351410603846,-4.57832904053163));
#50426=CARTESIAN_POINT('Ctrl Pts',(20.1337364884029,16.526967633547,-4.70550484721307));
#50427=CARTESIAN_POINT('Ctrl Pts',(17.2348043502142,16.5812273130942,-4.8326806538945));
#50428=CARTESIAN_POINT('Ctrl Pts',(16.1917618195022,18.2701494080764,-4.91974900156632));
#50429=CARTESIAN_POINT('Ctrl Pts',(16.169904976237,19.1644257529645,-4.96442541367765));
#50430=CARTESIAN_POINT('Ctrl Pts',(16.170099683962,19.2101632476096,-4.96670989022851));
#50431=CARTESIAN_POINT('Origin',(18.734,19.211,1.76670989022852));
#50432=CARTESIAN_POINT('',(20.2935358855687,21.2411349269503,-3.65004596059139));
#50433=CARTESIAN_POINT('',(20.2935358855687,21.2411349269503,-3.71676815338605));
#50434=CARTESIAN_POINT('',(20.2935358855687,21.2411349269503,1.76670989022852));
#50435=CARTESIAN_POINT('',(16.1740009581142,19.2087851537238,-4.23329008724976));
#50436=CARTESIAN_POINT('Ctrl Pts',(20.2935358855687,21.2411349269503,-3.71676815338605));
#50437=CARTESIAN_POINT('Ctrl Pts',(20.3601013017359,21.1899998255969,-3.72094076519367));
#50438=CARTESIAN_POINT('Ctrl Pts',(20.4242136531026,21.1355378040453,-3.72511337700128));
#50439=CARTESIAN_POINT('Ctrl Pts',(20.4855270181563,21.0780171677487,-3.7292859888089));
#50440=CARTESIAN_POINT('Ctrl Pts',(20.5468083990537,21.020526537129,-3.73345642397089));
#50441=CARTESIAN_POINT('Ctrl Pts',(20.6052933577953,20.9599807738333,-3.73762685913287));
#50442=CARTESIAN_POINT('Ctrl Pts',(20.6606699248329,20.8966876937156,-3.74179729429485));
#50443=CARTESIAN_POINT('Ctrl Pts',(20.7160342164331,20.8334086439051,-3.74596680498789));
#50444=CARTESIAN_POINT('Ctrl Pts',(20.76829118238,20.7673838332093,-3.75013631568094));
#50445=CARTESIAN_POINT('Ctrl Pts',(20.817167476553,20.6989560694563,-3.75430582637399));
#50446=CARTESIAN_POINT('Ctrl Pts',(20.8660475978043,20.6305229477191,-3.75847566354522));
#50447=CARTESIAN_POINT('Ctrl Pts',(20.911546255344,20.5596868744331,-3.76264550071646));
#50448=CARTESIAN_POINT('Ctrl Pts',(20.9534327818709,20.4868205699693,-3.76681533788769));
#50449=CARTESIAN_POINT('Ctrl Pts',(20.9953632065693,20.4138778997194,-3.77098954515696));
#50450=CARTESIAN_POINT('Ctrl Pts',(21.0336737113649,20.3389011492554,-3.77516375242623));
#50451=CARTESIAN_POINT('Ctrl Pts',(21.0681793245512,20.2622882006557,-3.7793379596955));
#50452=CARTESIAN_POINT('Ctrl Pts',(21.1027036734523,20.1856336530745,-3.78351443345854));
#50453=CARTESIAN_POINT('Ctrl Pts',(21.133418848782,20.1073415667467,-3.78769090722157));
#50454=CARTESIAN_POINT('Ctrl Pts',(21.160188745424,20.0278281162997,-3.79186738098461));
#50455=CARTESIAN_POINT('Ctrl Pts',(21.1870051409859,19.9481765521498,-3.79605110922162));
#50456=CARTESIAN_POINT('Ctrl Pts',(21.2098624449983,19.867299829612,-3.80023483745864));
#50457=CARTESIAN_POINT('Ctrl Pts',(21.2286750191276,19.7856273130829,-3.80441856569565));
#50458=CARTESIAN_POINT('Ctrl Pts',(21.2428259538791,19.7241927404161,-3.80756559198206));
#50459=CARTESIAN_POINT('Ctrl Pts',(21.2546893788146,19.6623081668811,-3.81071261826848));
#50460=CARTESIAN_POINT('Ctrl Pts',(21.2642482087236,19.6001580684646,-3.81385964455489));
#50461=CARTESIAN_POINT('Ctrl Pts',(21.2769586867287,19.517516420223,-3.818044278948));
#50462=CARTESIAN_POINT('Ctrl Pts',(21.285639763102,19.4340976099862,-3.82222891334111));
#50463=CARTESIAN_POINT('Ctrl Pts',(21.2902056694013,19.350329019665,-3.82641354773422));
#50464=CARTESIAN_POINT('Ctrl Pts',(21.2947650766981,19.2666796635636,-3.83059222581822));
#50465=CARTESIAN_POINT('Ctrl Pts',(21.2952209238071,19.1826819717237,-3.83477090390223));
#50466=CARTESIAN_POINT('Ctrl Pts',(21.2915388082527,19.0987714640506,-3.83894958198623));
#50467=CARTESIAN_POINT('Ctrl Pts',(21.2877906934233,19.0133569208345,-3.84320315987165));
#50468=CARTESIAN_POINT('Ctrl Pts',(21.2797547375529,18.9280331946162,-3.84745673775707));
#50469=CARTESIAN_POINT('Ctrl Pts',(21.2674501116906,18.8432629586579,-3.85171031564249));
#50470=CARTESIAN_POINT('Ctrl Pts',(21.2553840350109,18.7601361591377,-3.85588142962051));
#50471=CARTESIAN_POINT('Ctrl Pts',(21.2392133934507,18.6775420566421,-3.86005254359852));
#50472=CARTESIAN_POINT('Ctrl Pts',(21.2190086634415,18.5959130609251,-3.86422365757653));
#50473=CARTESIAN_POINT('Ctrl Pts',(21.1988107133246,18.514311456606,-3.86839337189697));
#50474=CARTESIAN_POINT('Ctrl Pts',(21.1745814736228,18.4336747620778,-3.8725630862174));
#50475=CARTESIAN_POINT('Ctrl Pts',(21.1464423282956,18.3544242516579,-3.87673280053783));
#50476=CARTESIAN_POINT('Ctrl Pts',(21.1183041842799,18.2751765613113,-3.88090236648194));
#50477=CARTESIAN_POINT('Ctrl Pts',(21.0862565659976,18.197315390231,-3.88507193242604));
#50478=CARTESIAN_POINT('Ctrl Pts',(21.0504699913874,18.1212446242381,-3.88924149837015));
#50479=CARTESIAN_POINT('Ctrl Pts',(21.0134252049625,18.0424993039588,-3.893557661109));
#50480=CARTESIAN_POINT('Ctrl Pts',(20.9723738713788,17.965673109816,-3.89787382384785));
#50481=CARTESIAN_POINT('Ctrl Pts',(20.9275574633285,17.8911872651486,-3.9021899865867));
#50482=CARTESIAN_POINT('Ctrl Pts',(20.8842009450552,17.8191277890344,-3.90636555077843));
#50483=CARTESIAN_POINT('Ctrl Pts',(20.8373211816343,17.7492588949819,-3.91054111497017));
#50484=CARTESIAN_POINT('Ctrl Pts',(20.7871804520949,17.6819316460225,-3.91471667916191));
#50485=CARTESIAN_POINT('Ctrl Pts',(20.734507233507,17.6112038577767,-3.91910314117432));
#50486=CARTESIAN_POINT('Ctrl Pts',(20.6782353411158,17.5432816689316,-3.92348960318672));
#50487=CARTESIAN_POINT('Ctrl Pts',(20.6187144099126,17.4785302042842,-3.92787606519912));
#50488=CARTESIAN_POINT('Ctrl Pts',(20.5591934787095,17.4137787396368,-3.93226252721153));
#50489=CARTESIAN_POINT('Ctrl Pts',(20.4964239761435,17.3521983512227,-3.93664898922393));
#50490=CARTESIAN_POINT('Ctrl Pts',(20.4307957154099,17.2941055584183,-3.94103545123633));
#50491=CARTESIAN_POINT('Ctrl Pts',(20.3681871082353,17.2386857011236,-3.94522008562936));
#50492=CARTESIAN_POINT('Ctrl Pts',(20.3027439921319,17.1862332698865,-3.94940472002238));
#50493=CARTESIAN_POINT('Ctrl Pts',(20.2347793028206,17.137051716116,-3.95358935441541));
#50494=CARTESIAN_POINT('Ctrl Pts',(20.1669113528323,17.0879401661999,-3.95776803249933));
#50495=CARTESIAN_POINT('Ctrl Pts',(20.0965293283138,17.0420905134705,-3.96194671058325));
#50496=CARTESIAN_POINT('Ctrl Pts',(20.0239808111754,16.9997674236301,-3.96612538866717));
#50497=CARTESIAN_POINT('Ctrl Pts',(19.9501319140064,16.9566857228211,-3.97037896655261));
#50498=CARTESIAN_POINT('Ctrl Pts',(19.8740384525303,16.9172585752805,-3.97463254443805));
#50499=CARTESIAN_POINT('Ctrl Pts',(19.7960998386662,16.8817202974513,-3.9788861223235));
#50500=CARTESIAN_POINT('Ctrl Pts',(19.7196722169169,16.8468709984853,-3.98305723630143));
#50501=CARTESIAN_POINT('Ctrl Pts',(19.6414707859437,16.8157613278183,-3.98722835027936));
#50502=CARTESIAN_POINT('Ctrl Pts',(19.561897281475,16.7885660811229,-3.9913994642573));
#50503=CARTESIAN_POINT('Ctrl Pts',(19.4823504786642,16.7613799600552,-3.99556917857765));
#50504=CARTESIAN_POINT('Ctrl Pts',(19.4014329516943,16.7381058029317,-3.99973889289801));
#50505=CARTESIAN_POINT('Ctrl Pts',(19.3195646284335,16.7188695728499,-4.00390860721836));
#50506=CARTESIAN_POINT('Ctrl Pts',(19.2376992183989,16.6996340272756,-4.00807817316238));
#50507=CARTESIAN_POINT('Ctrl Pts',(19.1548835273743,16.6844362274532,-4.01224773910641));
#50508=CARTESIAN_POINT('Ctrl Pts',(19.0715494575451,16.6733514105158,-4.01641730505043));
#50509=CARTESIAN_POINT('Ctrl Pts',(18.9852854646236,16.6618768650894,-4.02073346778937));
#50510=CARTESIAN_POINT('Ctrl Pts',(18.8984664850875,16.6548099783526,-4.02504963052832));
#50511=CARTESIAN_POINT('Ctrl Pts',(18.8115774056933,16.6521757101892,-4.02936579326726));
#50512=CARTESIAN_POINT('Ctrl Pts',(18.7275187289222,16.6496272530341,-4.03354135745892));
#50513=CARTESIAN_POINT('Ctrl Pts',(18.643394919223,16.6512270080047,-4.03771692165058));
#50514=CARTESIAN_POINT('Ctrl Pts',(18.559643131712,16.6569444637047,-4.04189248584225));
#50515=CARTESIAN_POINT('Ctrl Pts',(18.4716612405136,16.6629506945001,-4.04627894785483));
#50516=CARTESIAN_POINT('Ctrl Pts',(18.3840905205399,16.6735014582054,-4.05066540986742));
#50517=CARTESIAN_POINT('Ctrl Pts',(18.2974272347526,16.6885004022509,-4.05505187188));
#50518=CARTESIAN_POINT('Ctrl Pts',(18.2107639489653,16.7034993462965,-4.05943833389259));
#50519=CARTESIAN_POINT('Ctrl Pts',(18.125008646392,16.7229462681819,-4.06382479590517));
#50520=CARTESIAN_POINT('Ctrl Pts',(18.040638468227,16.7466847226344,-4.06821125791776));
#50521=CARTESIAN_POINT('Ctrl Pts',(17.960150287027,16.7693309356085,-4.07239589231081));
#50522=CARTESIAN_POINT('Ctrl Pts',(17.8806229756134,16.7959667334644,-4.07658052670385));
#50523=CARTESIAN_POINT('Ctrl Pts',(17.8024810747699,16.8264932392761,-4.08076516109689));
#50524=CARTESIAN_POINT('Ctrl Pts',(17.7244503992502,16.8569762943851,-4.08494383918083));
#50525=CARTESIAN_POINT('Ctrl Pts',(17.6478016421982,16.8913388913935,-4.08912251726477));
#50526=CARTESIAN_POINT('Ctrl Pts',(17.5729454850808,16.9294320274457,-4.0933011953487));
#50527=CARTESIAN_POINT('Ctrl Pts',(17.496747585145,16.9682079555846,-4.09755477323414));
#50528=CARTESIAN_POINT('Ctrl Pts',(17.4224076460745,17.0108493474659,-4.10180835111958));
#50529=CARTESIAN_POINT('Ctrl Pts',(17.3503388850128,17.0571471919204,-4.10606192900502));
#50530=CARTESIAN_POINT('Ctrl Pts',(17.279667317515,17.1025474623173,-4.11023304298296));
#50531=CARTESIAN_POINT('Ctrl Pts',(17.2111800563177,17.1514634154306,-4.1144041569609));
#50532=CARTESIAN_POINT('Ctrl Pts',(17.1452415288499,17.2036518686713,-4.11857527093885));
#50533=CARTESIAN_POINT('Ctrl Pts',(17.0793251276917,17.2558228095726,-4.12274498525921));
#50534=CARTESIAN_POINT('Ctrl Pts',(17.0159561221395,17.3112637844565,-4.12691469957958));
#50535=CARTESIAN_POINT('Ctrl Pts',(16.9554677262144,17.3696898818767,-4.13108441389994));
#50536=CARTESIAN_POINT('Ctrl Pts',(16.8949814827259,17.4281139002458,-4.13525397984399));
#50537=CARTESIAN_POINT('Ctrl Pts',(16.8373759753513,17.4895225097358,-4.13942354578803));
#50538=CARTESIAN_POINT('Ctrl Pts',(16.7829482470742,17.5535932733921,-4.14359311173208));
#50539=CARTESIAN_POINT('Ctrl Pts',(16.7266069070147,17.6199166860587,-4.147909274471));
#50540=CARTESIAN_POINT('Ctrl Pts',(16.6736713066578,17.6890925366905,-4.15222543720993));
#50541=CARTESIAN_POINT('Ctrl Pts',(16.6244248933202,17.7607266225718,-4.15654159994886));
#50542=CARTESIAN_POINT('Ctrl Pts',(16.5767826767175,17.8300272356399,-4.16071716414053));
#50543=CARTESIAN_POINT('Ctrl Pts',(16.5325931948251,17.9016279637396,-4.16489272833221));
#50544=CARTESIAN_POINT('Ctrl Pts',(16.4920674161604,17.9751447133591,-4.16906829252389));
#50545=CARTESIAN_POINT('Ctrl Pts',(16.449494776756,18.0523746192327,-4.17345475453644));
#50546=CARTESIAN_POINT('Ctrl Pts',(16.4109659295263,18.1317186646457,-4.17784121654899));
#50547=CARTESIAN_POINT('Ctrl Pts',(16.3766684749371,18.2127074171643,-4.18222767856154));
#50548=CARTESIAN_POINT('Ctrl Pts',(16.342371020348,18.293696169683,-4.18661414057409));
#50549=CARTESIAN_POINT('Ctrl Pts',(16.3123050853067,18.3763290580522,-4.19100060258664));
#50550=CARTESIAN_POINT('Ctrl Pts',(16.2865973915759,18.4601202011779,-4.1953870645992));
#50551=CARTESIAN_POINT('Ctrl Pts',(16.256634152739,18.557781782967,-4.20049964335899));
#50552=CARTESIAN_POINT('Ctrl Pts',(16.2324986213398,18.6573099274652,-4.20561222211878));
#50553=CARTESIAN_POINT('Ctrl Pts',(16.2143850329176,18.7580757042789,-4.21072480087858));
#50554=CARTESIAN_POINT('Ctrl Pts',(16.1965183144929,18.8574681448718,-4.21576770033044));
#50555=CARTESIAN_POINT('Ctrl Pts',(16.184510545625,18.9580647258724,-4.2208105997823));
#50556=CARTESIAN_POINT('Ctrl Pts',(16.1785021632639,19.0592409592912,-4.22585349923416));
#50557=CARTESIAN_POINT('Ctrl Pts',(16.1755487125961,19.1089746473601,-4.22833236190603));
#50558=CARTESIAN_POINT('Ctrl Pts',(16.1740441624119,19.1588480714529,-4.23081122457789));
#50559=CARTESIAN_POINT('Ctrl Pts',(16.1740009581142,19.2087851537238,-4.23329008724976));
#50560=CARTESIAN_POINT('Ctrl Pts',(16.1756127741342,19.2087870016449,-4.2332901097715));
#50561=CARTESIAN_POINT('Ctrl Pts',(16.1805387735992,19.8078855990186,-4.26304769694121));
#50562=CARTESIAN_POINT('Ctrl Pts',(16.6895187210545,21.2679843244803,-4.3351972196714));
#50563=CARTESIAN_POINT('Ctrl Pts',(18.6971963258685,22.0472231898468,-4.429658750874));
#50564=CARTESIAN_POINT('Ctrl Pts',(19.9334915936059,21.5116529017718,-4.49436269490689));
#50565=CARTESIAN_POINT('Ctrl Pts',(20.2910030748979,21.2378274151617,-4.51667470337929));
#50566=CARTESIAN_POINT('',(16.1740010840393,19.2133559031925,-4.16670989022851));
#50567=CARTESIAN_POINT('Ctrl Pts',(16.1740881651155,19.2133565881468,-4.16670992828903));
#50568=CARTESIAN_POINT('Ctrl Pts',(16.1722334682522,19.4149927583358,-4.17674049235513));
#50569=CARTESIAN_POINT('Ctrl Pts',(16.2862272813843,20.4667260563269,-4.22916299198171));
#50570=CARTESIAN_POINT('Ctrl Pts',(17.7316712378677,22.0633000666069,-4.32362832690876));
#50571=CARTESIAN_POINT('Ctrl Pts',(19.628405606888,21.7565647837825,-4.40806309776972));
#50572=CARTESIAN_POINT('Ctrl Pts',(20.296105832701,21.2444858570035,-4.4501059330702));
#50573=CARTESIAN_POINT('Ctrl Pts',(20.2935358855687,21.2411349269503,-3.65004596059139));
#50574=CARTESIAN_POINT('Ctrl Pts',(20.3602232230616,21.1899061664612,-3.65422168157886));
#50575=CARTESIAN_POINT('Ctrl Pts',(20.4243341316756,21.1354261893531,-3.65839740256633));
#50576=CARTESIAN_POINT('Ctrl Pts',(20.4855499160717,21.077995685991,-3.6625731235538));
#50577=CARTESIAN_POINT('Ctrl Pts',(20.5479163689702,21.01948566577,-3.6668273352551));
#50578=CARTESIAN_POINT('Ctrl Pts',(20.6072773982079,20.9579134254356,-3.6710815469564));
#50579=CARTESIAN_POINT('Ctrl Pts',(20.6633380126266,20.8936333031989,-3.6753357586577));
#50580=CARTESIAN_POINT('Ctrl Pts',(20.7193986270453,20.8293531809622,-3.679589970359));
#50581=CARTESIAN_POINT('Ctrl Pts',(20.7721585712015,20.7623656090433,-3.6838441820603));
#50582=CARTESIAN_POINT('Ctrl Pts',(20.8213695361432,20.6930554711554,-3.6880983937616));
#50583=CARTESIAN_POINT('Ctrl Pts',(20.8697756595073,20.6248788952852,-3.69228302815506));
#50584=CARTESIAN_POINT('Ctrl Pts',(20.914928230553,20.5542014284548,-3.69646766254852));
#50585=CARTESIAN_POINT('Ctrl Pts',(20.956559006204,20.4813666651568,-3.70065229694198));
#50586=CARTESIAN_POINT('Ctrl Pts',(20.9981305255987,20.4086355731292,-3.70483097502633));
#50587=CARTESIAN_POINT('Ctrl Pts',(21.0361899803432,20.3337536798788,-3.70900965311069));
#50588=CARTESIAN_POINT('Ctrl Pts',(21.0705113959642,20.2570948793151,-3.71318833119504));
#50589=CARTESIAN_POINT('Ctrl Pts',(21.1054479982896,20.1790620248547,-3.71744190908037));
#50590=CARTESIAN_POINT('Ctrl Pts',(21.1365109555625,20.0991883275092,-3.72169548696571));
#50591=CARTESIAN_POINT('Ctrl Pts',(21.1635100116304,20.017895968132,-3.72594906485104));
#50592=CARTESIAN_POINT('Ctrl Pts',(21.1899856383154,19.9381796197602,-3.73012017882942));
#50593=CARTESIAN_POINT('Ctrl Pts',(21.2125533792702,19.8570995822363,-3.7342912928078));
#50594=CARTESIAN_POINT('Ctrl Pts',(21.2310824062636,19.7750739812551,-3.73846240678618));
#50595=CARTESIAN_POINT('Ctrl Pts',(21.249605215663,19.6930759047563,-3.74263212110698));
#50596=CARTESIAN_POINT('Ctrl Pts',(21.2640919013283,19.6101333433023,-3.74680183542779));
#50597=CARTESIAN_POINT('Ctrl Pts',(21.2744621331457,19.5266772878315,-3.7509715497486));
#50598=CARTESIAN_POINT('Ctrl Pts',(21.2848319959458,19.4432242020852,-3.75514111569308));
#50599=CARTESIAN_POINT('Ctrl Pts',(21.2910856402585,19.3592581152793,-3.75931068163755));
#50600=CARTESIAN_POINT('Ctrl Pts',(21.293194451632,19.2752164989407,-3.76348024758203));
#50601=CARTESIAN_POINT('Ctrl Pts',(21.2953774062114,19.1882200830675,-3.76779641032045));
#50602=CARTESIAN_POINT('Ctrl Pts',(21.2931186269949,19.1011432548625,-3.77211257305887));
#50603=CARTESIAN_POINT('Ctrl Pts',(21.2864451550249,19.0144707894738,-3.77642873579728));
#50604=CARTESIAN_POINT('Ctrl Pts',(21.2799890707009,18.9306216705101,-3.7806042999894));
#50605=CARTESIAN_POINT('Ctrl Pts',(21.2694016000863,18.847151436045,-3.78477986418152));
#50606=CARTESIAN_POINT('Ctrl Pts',(21.2547598325397,18.7644914707929,-3.78895542837365));
#50607=CARTESIAN_POINT('Ctrl Pts',(21.2393785441268,18.6776565472299,-3.79334189038521));
#50608=CARTESIAN_POINT('Ctrl Pts',(21.21952276158,18.5917164663179,-3.79772835239678));
#50609=CARTESIAN_POINT('Ctrl Pts',(21.1953413592831,18.5071543400131,-3.80211481440834));
#50610=CARTESIAN_POINT('Ctrl Pts',(21.1711599569862,18.4225922137084,-3.80650127641991));
#50611=CARTESIAN_POINT('Ctrl Pts',(21.1426531949957,18.3394085662324,-3.81088773843147));
#50612=CARTESIAN_POINT('Ctrl Pts',(21.1100276507034,18.2580610706384,-3.81527420044303));
#50613=CARTESIAN_POINT('Ctrl Pts',(21.0789032560606,18.1804564938874,-3.81945883483597));
#50614=CARTESIAN_POINT('Ctrl Pts',(21.0439149217344,18.104233954906,-3.82364346922891));
#50615=CARTESIAN_POINT('Ctrl Pts',(21.0052063614281,18.0298049848529,-3.82782810362184));
#50616=CARTESIAN_POINT('Ctrl Pts',(20.9665528979663,17.9554819552262,-3.83200678170567));
#50617=CARTESIAN_POINT('Ctrl Pts',(20.924189937065,17.8829478282645,-3.8361854597895));
#50618=CARTESIAN_POINT('Ctrl Pts',(20.8783095486356,17.8125949944204,-3.84036413787333));
#50619=CARTESIAN_POINT('Ctrl Pts',(20.8316067872157,17.7409811365889,-3.8446177157588));
#50620=CARTESIAN_POINT('Ctrl Pts',(20.7812594376514,17.6716279878893,-3.84887129364426));
#50621=CARTESIAN_POINT('Ctrl Pts',(20.7275195051817,17.6049240421262,-3.85312487152973));
#50622=CARTESIAN_POINT('Ctrl Pts',(20.6748214261695,17.5395132825159,-3.85729598550756));
#50623=CARTESIAN_POINT('Ctrl Pts',(20.6188614359627,17.476650297294,-3.8614670994854));
#50624=CARTESIAN_POINT('Ctrl Pts',(20.5599202972605,17.4166714158069,-3.86563821346324));
#50625=CARTESIAN_POINT('Ctrl Pts',(20.5009989368265,17.3567126608129,-3.8698079277835));
#50626=CARTESIAN_POINT('Ctrl Pts',(20.4390987367876,17.2996364153551,-3.87397764210375));
#50627=CARTESIAN_POINT('Ctrl Pts',(20.3745386111499,17.2457435115675,-3.87814735642401));
#50628=CARTESIAN_POINT('Ctrl Pts',(20.3099807828387,17.1918525255206,-3.88231692236793));
#50629=CARTESIAN_POINT('Ctrl Pts',(20.2427635708238,17.1411449500712,-3.88648648831186));
#50630=CARTESIAN_POINT('Ctrl Pts',(20.1732393309682,17.0938816404853,-3.89065605425579));
#50631=CARTESIAN_POINT('Ctrl Pts',(20.1012707046023,17.0449566112369,-3.89497221699484));
#50632=CARTESIAN_POINT('Ctrl Pts',(20.0268302379304,16.9997228515222,-3.8992883797339));
#50633=CARTESIAN_POINT('Ctrl Pts',(19.9503401869381,16.9584200236974,-3.90360454247296));
#50634=CARTESIAN_POINT('Ctrl Pts',(19.8763417913159,16.9184626311471,-3.90778010666452));
#50635=CARTESIAN_POINT('Ctrl Pts',(19.8004257365565,16.882184163653,-3.91195567085608));
#50636=CARTESIAN_POINT('Ctrl Pts',(19.7229964759442,16.8497533016286,-3.91613123504764));
#50637=CARTESIAN_POINT('Ctrl Pts',(19.6416564474417,16.8156844338573,-3.92051769706044));
#50638=CARTESIAN_POINT('Ctrl Pts',(19.5586468811865,16.7858622689059,-3.92490415907325));
#50639=CARTESIAN_POINT('Ctrl Pts',(19.4744545807604,16.7604231263168,-3.92929062108606));
#50640=CARTESIAN_POINT('Ctrl Pts',(19.3902622803344,16.7349839837277,-3.93367708309886));
#50641=CARTESIAN_POINT('Ctrl Pts',(19.3048878272885,16.7139279285856,-3.93806354511167));
#50642=CARTESIAN_POINT('Ctrl Pts',(19.2188278686569,16.6973289917387,-3.94245000712447));
#50643=CARTESIAN_POINT('Ctrl Pts',(19.1367276562993,16.6814937965827,-3.94663464151747));
#50644=CARTESIAN_POINT('Ctrl Pts',(19.0536980417284,16.6696556340513,-3.95081927591047));
#50645=CARTESIAN_POINT('Ctrl Pts',(18.9701628470245,16.6619164176737,-3.95500391030348));
#50646=CARTESIAN_POINT('Ctrl Pts',(18.8867465543309,16.6541882171128,-3.95918258838736));
#50647=CARTESIAN_POINT('Ctrl Pts',(18.8028265650706,16.6505474159413,-3.96336126647125));
#50648=CARTESIAN_POINT('Ctrl Pts',(18.7188367813175,16.651044907269,-3.96753994455514));
#50649=CARTESIAN_POINT('Ctrl Pts',(18.6333415410517,16.6515513157713,-3.97179352244059));
#50650=CARTESIAN_POINT('Ctrl Pts',(18.5477744529634,16.6563459251098,-3.97604710032604));
#50651=CARTESIAN_POINT('Ctrl Pts',(18.4625985845179,16.6654271230872,-3.98030067821149));
#50652=CARTESIAN_POINT('Ctrl Pts',(18.3790740164904,16.6743322643211,-3.98447179218939));
#50653=CARTESIAN_POINT('Ctrl Pts',(18.2959261128669,16.6873592186152,-3.98864290616729));
#50654=CARTESIAN_POINT('Ctrl Pts',(18.2135896449265,16.7044539576676,-3.9928140201452));
#50655=CARTESIAN_POINT('Ctrl Pts',(18.1312808057832,16.7215429604151,-3.99698373446551));
#50656=CARTESIAN_POINT('Ctrl Pts',(18.049783311613,16.7426969435999,-4.00115344878583));
#50657=CARTESIAN_POINT('Ctrl Pts',(17.9695227367355,16.7678105857401,-4.00532316310615));
#50658=CARTESIAN_POINT('Ctrl Pts',(17.8892650178734,16.7929233342292,-4.00949272905015));
#50659=CARTESIAN_POINT('Ctrl Pts',(17.8102445695787,16.8219953233349,-4.01366229499415));
#50660=CARTESIAN_POINT('Ctrl Pts',(17.7328714533942,16.8548714735458,-4.01783186093816));
#50661=CARTESIAN_POINT('Ctrl Pts',(17.652777993893,16.8889035086419,-4.02214802367714));
#50662=CARTESIAN_POINT('Ctrl Pts',(17.5744503476379,16.9270119844461,-4.02646418641611));
#50663=CARTESIAN_POINT('Ctrl Pts',(17.4983185918994,16.9689715751859,-4.03078034915509));
#50664=CARTESIAN_POINT('Ctrl Pts',(17.4246668200984,17.0095643366696,-4.03495591334672));
#50665=CARTESIAN_POINT('Ctrl Pts',(17.3530704495475,17.0537608783684,-4.03913147753835));
#50666=CARTESIAN_POINT('Ctrl Pts',(17.2838902366718,17.1013124225847,-4.04330704172998));
#50667=CARTESIAN_POINT('Ctrl Pts',(17.2112158957014,17.1512656822582,-4.04769350374263));
#50668=CARTESIAN_POINT('Ctrl Pts',(17.1412086706269,17.2049214186627,-4.05207996575528));
#50669=CARTESIAN_POINT('Ctrl Pts',(17.0742466821561,17.2619440942071,-4.05646642776794));
#50670=CARTESIAN_POINT('Ctrl Pts',(17.0072846936854,17.3189667697514,-4.06085288978059));
#50671=CARTESIAN_POINT('Ctrl Pts',(16.9433683113269,17.3793559306723,-4.06523935179324));
#50672=CARTESIAN_POINT('Ctrl Pts',(16.8828286089282,17.4427340469043,-4.06962581380589));
#50673=CARTESIAN_POINT('Ctrl Pts',(16.8258191500137,17.5024164036099,-4.07375648865202));
#50674=CARTESIAN_POINT('Ctrl Pts',(16.7715797255597,17.5649836670307,-4.07788716349815));
#50675=CARTESIAN_POINT('Ctrl Pts',(16.720421868205,17.6301448177784,-4.08201783834428));
#50676=CARTESIAN_POINT('Ctrl Pts',(16.6693300782615,17.6952218166721,-4.08614317866297));
#50677=CARTESIAN_POINT('Ctrl Pts',(16.6213122506322,17.7628856907896,-4.09026851898165));
#50678=CARTESIAN_POINT('Ctrl Pts',(16.5766430483354,17.8328088002369,-4.09439385930034));
#50679=CARTESIAN_POINT('Ctrl Pts',(16.5320173182039,17.9026638603613,-4.09851518482882));
#50680=CARTESIAN_POINT('Ctrl Pts',(16.4907340001792,17.9747733973529,-4.10263651035731));
#50681=CARTESIAN_POINT('Ctrl Pts',(16.4530264539488,18.0487781269419,-4.10675783588579));
#50682=CARTESIAN_POINT('Ctrl Pts',(16.4153436115609,18.1227343728356,-4.11087646135587));
#50683=CARTESIAN_POINT('Ctrl Pts',(16.3812321043788,18.1985829265154,-4.11499508682596));
#50684=CARTESIAN_POINT('Ctrl Pts',(16.350880245421,18.2759383788566,-4.11911371229604));
#50685=CARTESIAN_POINT('Ctrl Pts',(16.3205285952524,18.3532932990729,-4.12323230943428));
#50686=CARTESIAN_POINT('Ctrl Pts',(16.293936732308,18.4321546644583,-4.12735090657251));
#50687=CARTESIAN_POINT('Ctrl Pts',(16.271245067881,18.5121165016089,-4.13146950371074));
#50688=CARTESIAN_POINT('Ctrl Pts',(16.2485547151171,18.592073716666,-4.13558786277865));
#50689=CARTESIAN_POINT('Ctrl Pts',(16.2297642345969,18.6731308198829,-4.13970622184656));
#50690=CARTESIAN_POINT('Ctrl Pts',(16.2149637529306,18.7548680169618,-4.14382458091447));
#50691=CARTESIAN_POINT('Ctrl Pts',(16.2001500672814,18.8366781344071,-4.14794661410215));
#50692=CARTESIAN_POINT('Ctrl Pts',(16.1893335672673,18.9191690901925,-4.15206864728983));
#50693=CARTESIAN_POINT('Ctrl Pts',(16.1825528364003,19.0019130052847,-4.15619068047751));
#50694=CARTESIAN_POINT('Ctrl Pts',(16.1767848147302,19.0722990307275,-4.15969708372784));
#50695=CARTESIAN_POINT('Ctrl Pts',(16.1739362156169,19.1428678239494,-4.16320348697818));
#50696=CARTESIAN_POINT('Ctrl Pts',(16.1740010840393,19.2133559031925,-4.16670989022851));
#50697=CARTESIAN_POINT('Origin',(18.734,19.211,1.76670989022852));
#50698=CARTESIAN_POINT('',(20.2912843055177,21.2382340775644,-2.85017128750281));
#50699=CARTESIAN_POINT('',(20.2935358855687,21.2411349269503,-2.91665631135199));
#50700=CARTESIAN_POINT('',(20.2935358855687,21.2411349269503,1.76670989022852));
#50701=CARTESIAN_POINT('',(16.1740000028035,19.2108801919503,-3.43329010980363));
#50702=CARTESIAN_POINT('Ctrl Pts',(20.2935358855687,21.2411349269503,-2.91665631135199));
#50703=CARTESIAN_POINT('Ctrl Pts',(20.3304359409714,21.2127885545905,-2.91898054016294));
#50704=CARTESIAN_POINT('Ctrl Pts',(20.3665290680521,21.1834618031319,-2.9213047689739));
#50705=CARTESIAN_POINT('Ctrl Pts',(20.401762322946,21.1532072068041,-2.92362899778486));
#50706=CARTESIAN_POINT('Ctrl Pts',(20.4651976823984,21.0987356230994,-2.92781363217407));
#50707=CARTESIAN_POINT('Ctrl Pts',(20.5260796023552,21.0410515629438,-2.93199826656328));
#50708=CARTESIAN_POINT('Ctrl Pts',(20.5840648143939,20.9804236865549,-2.93618290095248));
#50709=CARTESIAN_POINT('Ctrl Pts',(20.6419674916593,20.919882106445,-2.94036157903251));
#50710=CARTESIAN_POINT('Ctrl Pts',(20.6969813355446,20.8564053626881,-2.94454025711254));
#50711=CARTESIAN_POINT('Ctrl Pts',(20.7487967797138,20.7903017243246,-2.94871893519257));
#50712=CARTESIAN_POINT('Ctrl Pts',(20.8015409785421,20.723013225673,-2.95297251307897));
#50713=CARTESIAN_POINT('Ctrl Pts',(20.8509706214137,20.6530030460431,-2.95722609096538));
#50714=CARTESIAN_POINT('Ctrl Pts',(20.8967991444563,20.5806349370322,-2.96147966885178));
#50715=CARTESIAN_POINT('Ctrl Pts',(20.9417391920986,20.5096698251147,-2.96565078282566));
#50716=CARTESIAN_POINT('Ctrl Pts',(20.9832162459024,20.4364378006298,-2.96982189679954));
#50717=CARTESIAN_POINT('Ctrl Pts',(21.021002390723,20.361313029061,-2.97399301077341));
#50718=CARTESIAN_POINT('Ctrl Pts',(21.0587758560373,20.2862134663357,-2.97816272508966));
#50719=CARTESIAN_POINT('Ctrl Pts',(21.0928606655495,20.2092228285369,-2.98233243940591));
#50720=CARTESIAN_POINT('Ctrl Pts',(21.1230748017628,20.1307399586743,-2.98650215372216));
#50721=CARTESIAN_POINT('Ctrl Pts',(21.153287862827,20.0522598815699,-2.99067171966203));
#50722=CARTESIAN_POINT('Ctrl Pts',(21.1796303599629,19.9722881076019,-2.9948412856019));
#50723=CARTESIAN_POINT('Ctrl Pts',(21.2019688964371,19.8912422555377,-2.99901085154177));
#50724=CARTESIAN_POINT('Ctrl Pts',(21.2250928283449,19.8073469311187,-3.00332701428548));
#50725=CARTESIAN_POINT('Ctrl Pts',(21.2439258622492,19.7223011025982,-3.00764317702919));
#50726=CARTESIAN_POINT('Ctrl Pts',(21.2583771885885,19.6365817309687,-3.0119593397729));
#50727=CARTESIAN_POINT('Ctrl Pts',(21.2723577644625,19.5536546590301,-3.01613490396034));
#50728=CARTESIAN_POINT('Ctrl Pts',(21.2822377087348,19.4700977247691,-3.02031046814778));
#50729=CARTESIAN_POINT('Ctrl Pts',(21.2879876706469,19.3863481627602,-3.02448603233522));
#50730=CARTESIAN_POINT('Ctrl Pts',(21.294028049485,19.2983686091941,-3.02887249435706));
#50731=CARTESIAN_POINT('Ctrl Pts',(21.295510260803,19.2101770410252,-3.03325895637891));
#50732=CARTESIAN_POINT('Ctrl Pts',(21.2924621252161,19.1222782223196,-3.03764541840075));
#50733=CARTESIAN_POINT('Ctrl Pts',(21.2894139896292,19.034379403614,-3.0420318804226));
#50734=CARTESIAN_POINT('Ctrl Pts',(21.2818356329245,18.9467739058741,-3.04641834244444));
#50735=CARTESIAN_POINT('Ctrl Pts',(21.2698170137414,18.859955739515,-3.05080480446629));
#50736=CARTESIAN_POINT('Ctrl Pts',(21.2583513890591,18.7771322058033,-3.05498943886226));
#50737=CARTESIAN_POINT('Ctrl Pts',(21.2428024516836,18.6947168580505,-3.05917407325823));
#50738=CARTESIAN_POINT('Ctrl Pts',(21.2232102976567,18.6131437513584,-3.0633587076542));
#50739=CARTESIAN_POINT('Ctrl Pts',(21.2036460306358,18.531686753886,-3.06753738574111));
#50740=CARTESIAN_POINT('Ctrl Pts',(21.1800500847572,18.4510700597147,-3.07171606382802));
#50741=CARTESIAN_POINT('Ctrl Pts',(21.1525141031145,18.371720825329,-3.07589474191492));
#50742=CARTESIAN_POINT('Ctrl Pts',(21.1244845588153,18.2909493130154,-3.08014831979962));
#50743=CARTESIAN_POINT('Ctrl Pts',(21.09237240526,18.2114916234332,-3.08440189768432));
#50744=CARTESIAN_POINT('Ctrl Pts',(21.0563283883888,18.133785603288,-3.08865547556902));
#50745=CARTESIAN_POINT('Ctrl Pts',(21.0209831550868,18.0575860659054,-3.09282658955002));
#50746=CARTESIAN_POINT('Ctrl Pts',(20.9818573541681,17.9830713215426,-3.09699770353101));
#50747=CARTESIAN_POINT('Ctrl Pts',(20.9391422334475,17.9106355394482,-3.10116881751201));
#50748=CARTESIAN_POINT('Ctrl Pts',(20.896441446198,17.8382240638797,-3.10533853183544));
#50749=CARTESIAN_POINT('Ctrl Pts',(20.8501539646469,17.7678905610384,-3.10950824615888));
#50750=CARTESIAN_POINT('Ctrl Pts',(20.8005166300296,17.7000039649916,-3.11367796048232));
#50751=CARTESIAN_POINT('Ctrl Pts',(20.7508810617214,17.6321197846409,-3.11784752642945));
#50752=CARTESIAN_POINT('Ctrl Pts',(20.697896149566,17.5666827088149,-3.12201709237658));
#50753=CARTESIAN_POINT('Ctrl Pts',(20.6418408397364,17.5040309521746,-3.1261866583237));
#50754=CARTESIAN_POINT('Ctrl Pts',(20.583814694456,17.4391764371619,-3.13050282105904));
#50755=CARTESIAN_POINT('Ctrl Pts',(20.5224985756088,17.3773071422623,-3.13481898379437));
#50756=CARTESIAN_POINT('Ctrl Pts',(20.4582443784125,17.3187575938816,-3.13913514652971));
#50757=CARTESIAN_POINT('Ctrl Pts',(20.3960832548338,17.262115290792,-3.14331071072449));
#50758=CARTESIAN_POINT('Ctrl Pts',(20.3311729226017,17.2085800374226,-3.14748627491927));
#50759=CARTESIAN_POINT('Ctrl Pts',(20.2638651397918,17.1584131798996,-3.15166183911405));
#50760=CARTESIAN_POINT('Ctrl Pts',(20.1931578010453,17.1057125137858,-3.15604830111966));
#50761=CARTESIAN_POINT('Ctrl Pts',(20.1198049419668,17.0567297856998,-3.16043476312527));
#50762=CARTESIAN_POINT('Ctrl Pts',(20.0442460480199,17.0117148221187,-3.16482122513089));
#50763=CARTESIAN_POINT('Ctrl Pts',(19.9686871540731,16.9666998585377,-3.1692076871365));
#50764=CARTESIAN_POINT('Ctrl Pts',(19.8909227738875,16.9256528630382,-3.17359414914211));
#50765=CARTESIAN_POINT('Ctrl Pts',(19.8114169849418,16.8887655931067,-3.17798061114772));
#50766=CARTESIAN_POINT('Ctrl Pts',(19.7355693750926,16.8535755610944,-3.18216524554016));
#50767=CARTESIAN_POINT('Ctrl Pts',(19.6578547653245,16.8220398921686,-3.1863498799326));
#50768=CARTESIAN_POINT('Ctrl Pts',(19.5786598305131,16.7943598176978,-3.19053451432504));
#50769=CARTESIAN_POINT('Ctrl Pts',(19.499577619889,16.7667191423869,-3.19471319240838));
#50770=CARTESIAN_POINT('Ctrl Pts',(19.4190197000616,16.7429233111999,-3.19889187049171));
#50771=CARTESIAN_POINT('Ctrl Pts',(19.3373948467028,16.7231264785017,-3.20307054857505));
#50772=CARTESIAN_POINT('Ctrl Pts',(19.2543069264952,16.7029748018014,-3.20732412646064));
#50773=CARTESIAN_POINT('Ctrl Pts',(19.1701138843273,16.6869671007256,-3.21157770434623));
#50774=CARTESIAN_POINT('Ctrl Pts',(19.0852654759065,16.6752136199127,-3.21583128223181));
#50775=CARTESIAN_POINT('Ctrl Pts',(19.0020620194662,16.6636880032626,-3.22000239620915));
#50776=CARTESIAN_POINT('Ctrl Pts',(18.9182288577836,16.6562531921902,-3.22417351018649));
#50777=CARTESIAN_POINT('Ctrl Pts',(18.8342009436322,16.6529617338876,-3.22834462416383));
#50778=CARTESIAN_POINT('Ctrl Pts',(18.7502012258589,16.6496713800656,-3.23251433848359));
#50779=CARTESIAN_POINT('Ctrl Pts',(18.666007344703,16.6505216357631,-3.23668405280335));
#50780=CARTESIAN_POINT('Ctrl Pts',(18.5820577129978,16.6555130519957,-3.24085376712311));
#50781=CARTESIAN_POINT('Ctrl Pts',(18.4981110685807,16.6605042906122,-3.24502333306655));
#50782=CARTESIAN_POINT('Ctrl Pts',(18.4144091155048,16.6696363686189,-3.24919289900998));
#50783=CARTESIAN_POINT('Ctrl Pts',(18.3313872270485,16.6828578056098,-3.25336246495341));
#50784=CARTESIAN_POINT('Ctrl Pts',(18.2454463913857,16.6965440920191,-3.25767862769306));
#50785=CARTESIAN_POINT('Ctrl Pts',(18.1602348531238,16.7146125685865,-3.2619947904327));
#50786=CARTESIAN_POINT('Ctrl Pts',(18.0762243702396,16.7369484199206,-3.26631095317235));
#50787=CARTESIAN_POINT('Ctrl Pts',(17.9949505200243,16.7585566832401,-3.27048651736343));
#50788=CARTESIAN_POINT('Ctrl Pts',(17.9148011124186,16.784158383043,-3.27466208155451));
#50789=CARTESIAN_POINT('Ctrl Pts',(17.8361862981298,16.813599208156,-3.27883764574559));
#50790=CARTESIAN_POINT('Ctrl Pts',(17.7536008364222,16.8445270193708,-3.28322410775951));
#50791=CARTESIAN_POINT('Ctrl Pts',(17.6727096022458,16.8796917438774,-3.28761056977344));
#50792=CARTESIAN_POINT('Ctrl Pts',(17.5939605452813,16.9188590702828,-3.29199703178737));
#50793=CARTESIAN_POINT('Ctrl Pts',(17.5152114883168,16.9580263966883,-3.2963834938013));
#50794=CARTESIAN_POINT('Ctrl Pts',(17.4386050767024,17.001195973874,-3.30076995581523));
#50795=CARTESIAN_POINT('Ctrl Pts',(17.364553744478,17.0480813808105,-3.30515641782915));
#50796=CARTESIAN_POINT('Ctrl Pts',(17.2939096238495,17.092809520654,-3.30934105222176));
#50797=CARTESIAN_POINT('Ctrl Pts',(17.2253276726157,17.1410855493988,-3.31352568661436));
#50798=CARTESIAN_POINT('Ctrl Pts',(17.1591863942882,17.19269325739,-3.31771032100696));
#50799=CARTESIAN_POINT('Ctrl Pts',(17.0931392598839,17.2442275081965,-3.32188899909045));
#50800=CARTESIAN_POINT('Ctrl Pts',(17.0295262575255,17.2990837381083,-3.32606767717394));
#50801=CARTESIAN_POINT('Ctrl Pts',(16.9686982691563,17.3570016723092,-3.33024635525743));
#50802=CARTESIAN_POINT('Ctrl Pts',(16.9067799828036,17.4159577438638,-3.33449993314298));
#50803=CARTESIAN_POINT('Ctrl Pts',(16.8477479425957,17.4780861035064,-3.33875351102853));
#50804=CARTESIAN_POINT('Ctrl Pts',(16.7919382910611,17.5430682511945,-3.34300708891407));
#50805=CARTESIAN_POINT('Ctrl Pts',(16.7372106185328,17.6067905931384,-3.34717820289155));
#50806=CARTESIAN_POINT('Ctrl Pts',(16.6855818186072,17.6732566930094,-3.35134931686903));
#50807=CARTESIAN_POINT('Ctrl Pts',(16.6373315068437,17.742129267156,-3.35552043084651));
#50808=CARTESIAN_POINT('Ctrl Pts',(16.5890973859384,17.810978730445,-3.3596901451664));
#50809=CARTESIAN_POINT('Ctrl Pts',(16.5442397654171,17.8822326878121,-3.36385985948629));
#50810=CARTESIAN_POINT('Ctrl Pts',(16.5029964131481,17.9555228016989,-3.36802957380618));
#50811=CARTESIAN_POINT('Ctrl Pts',(16.4617545284947,18.0288103076089,-3.37219913974973));
#50812=CARTESIAN_POINT('Ctrl Pts',(16.4241268812486,18.1041334246491,-3.37636870569329));
#50813=CARTESIAN_POINT('Ctrl Pts',(16.3903058438335,18.1810982074242,-3.38053827163684));
#50814=CARTESIAN_POINT('Ctrl Pts',(16.3552957004569,18.2607689770351,-3.38485443437632));
#50815=CARTESIAN_POINT('Ctrl Pts',(16.3243650403573,18.3421985193633,-3.3891705971158));
#50816=CARTESIAN_POINT('Ctrl Pts',(16.2976726756056,18.4249280132142,-3.39348675985528));
#50817=CARTESIAN_POINT('Ctrl Pts',(16.2718498118346,18.5049626024846,-3.39766232404646));
#50818=CARTESIAN_POINT('Ctrl Pts',(16.2499934356292,18.5862132848944,-3.40183788823764));
#50819=CARTESIAN_POINT('Ctrl Pts',(16.2321958025117,18.6682516628952,-3.40601345242882));
#50820=CARTESIAN_POINT('Ctrl Pts',(16.2134992532484,18.7544336043728,-3.41039991444245));
#50821=CARTESIAN_POINT('Ctrl Pts',(16.1992823307861,18.8414843294194,-3.41478637645608));
#50822=CARTESIAN_POINT('Ctrl Pts',(16.1895904829899,18.9289003549305,-3.41917283846971));
#50823=CARTESIAN_POINT('Ctrl Pts',(16.1798986351937,19.0163163804415,-3.42355930048334));
#50824=CARTESIAN_POINT('Ctrl Pts',(16.174731820223,19.1040971227329,-3.42794576249697));
#50825=CARTESIAN_POINT('Ctrl Pts',(16.1740724460423,19.1917407557755,-3.43233222451059));
#50826=CARTESIAN_POINT('Ctrl Pts',(16.1740244495167,19.1981204260764,-3.43265151959756));
#50827=CARTESIAN_POINT('Ctrl Pts',(16.1740003013853,19.204500276023,-3.43297081468453));
#50828=CARTESIAN_POINT('Ctrl Pts',(16.1740000028035,19.2108801913083,-3.4332901097715));
#50829=CARTESIAN_POINT('Ctrl Pts',(16.1740000028035,19.2108801919503,-3.43329010980363));
#50830=CARTESIAN_POINT('Ctrl Pts',(16.173996094898,19.2943824116246,-3.43746913841142));
#50831=CARTESIAN_POINT('Ctrl Pts',(16.1780820066338,19.3780422026732,-3.4416481670192));
#50832=CARTESIAN_POINT('Ctrl Pts',(16.1862780259001,19.4614251239166,-3.44582719562699));
#50833=CARTESIAN_POINT('Ctrl Pts',(16.1944623792895,19.5446893613378,-3.45000027597725));
#50834=CARTESIAN_POINT('Ctrl Pts',(16.2067451760218,19.6276770564327,-3.45417335632751));
#50835=CARTESIAN_POINT('Ctrl Pts',(16.2230946976723,19.7099534675123,-3.45834643667778));
#50836=CARTESIAN_POINT('Ctrl Pts',(16.2396087147061,19.7930576758859,-3.46256150311587));
#50837=CARTESIAN_POINT('Ctrl Pts',(16.2602717621694,19.8754357285734,-3.46677656955397));
#50838=CARTESIAN_POINT('Ctrl Pts',(16.2849973159137,19.9566445891563,-3.47099163599206));
#50839=CARTESIAN_POINT('Ctrl Pts',(16.3094325809408,20.0369000225196,-3.47515721572334));
#50840=CARTESIAN_POINT('Ctrl Pts',(16.3378353258574,20.1160131199902,-3.47932279545462));
#50841=CARTESIAN_POINT('Ctrl Pts',(16.3700710228283,20.1935679573893,-3.4834883751859));
#50842=CARTESIAN_POINT('Ctrl Pts',(16.4022960455082,20.2710971138511,-3.48765257555782));
#50843=CARTESIAN_POINT('Ctrl Pts',(16.4383513227395,20.3470686092118,-3.49181677592973));
#50844=CARTESIAN_POINT('Ctrl Pts',(16.4780536821042,20.4210852080628,-3.49598097630165));
#50845=CARTESIAN_POINT('Ctrl Pts',(16.5177548909312,20.495099661981,-3.50014505599888));
#50846=CARTESIAN_POINT('Ctrl Pts',(16.561102752779,20.5671589258651,-3.50430913569611));
#50847=CARTESIAN_POINT('Ctrl Pts',(16.6078681568273,20.636890383391,-3.50847321539335));
#50848=CARTESIAN_POINT('Ctrl Pts',(16.6556310871523,20.7081092430383,-3.5127261167099));
#50849=CARTESIAN_POINT('Ctrl Pts',(16.7069587733461,20.7768994173764,-3.51697901802646));
#50850=CARTESIAN_POINT('Ctrl Pts',(16.761561649075,20.8428967344168,-3.52123191934301));
#50851=CARTESIAN_POINT('Ctrl Pts',(16.8151012611779,20.9076089076679,-3.52540200532769));
#50852=CARTESIAN_POINT('Ctrl Pts',(16.8717892886061,20.9696357146529,-3.52957209131237));
#50853=CARTESIAN_POINT('Ctrl Pts',(16.9313144499797,21.028670159228,-3.53374217729704));
#50854=CARTESIAN_POINT('Ctrl Pts',(16.9926128107595,21.0894631852106,-3.53803648627954));
#50855=CARTESIAN_POINT('Ctrl Pts',(17.0569196193486,21.1470823903912,-3.54233079526204));
#50856=CARTESIAN_POINT('Ctrl Pts',(17.1238587796064,21.2012374859271,-3.54662510424453));
#50857=CARTESIAN_POINT('Ctrl Pts',(17.1907979398641,21.255392581463,-3.55091941322703));
#50858=CARTESIAN_POINT('Ctrl Pts',(17.2603689845985,21.3060833143331,-3.55521372220952));
#50859=CARTESIAN_POINT('Ctrl Pts',(17.3321657913456,21.3530692919339,-3.55950803119202));
#50860=CARTESIAN_POINT('Ctrl Pts',(17.4021289421207,21.3988552702266,-3.56369266558496));
#50861=CARTESIAN_POINT('Ctrl Pts',(17.4744678068902,21.4412951999105,-3.5678772999779));
#50862=CARTESIAN_POINT('Ctrl Pts',(17.5488288662329,21.4801340603158,-3.57206193437084));
#50863=CARTESIAN_POINT('Ctrl Pts',(17.6230840818118,21.5189176384105,-3.57624061245467));
#50864=CARTESIAN_POINT('Ctrl Pts',(17.6993553703912,21.5541101172787,-3.58041929053851));
#50865=CARTESIAN_POINT('Ctrl Pts',(17.7772605377966,21.5854998634371,-3.58459796862235));
#50866=CARTESIAN_POINT('Ctrl Pts',(17.8565620993408,21.6174522482369,-3.58885154650781));
#50867=CARTESIAN_POINT('Ctrl Pts',(17.9375562869758,21.6454639674282,-3.59310512439327));
#50868=CARTESIAN_POINT('Ctrl Pts',(18.0198140087909,21.6693609112497,-3.59735870227874));
#50869=CARTESIAN_POINT('Ctrl Pts',(18.1004770041531,21.6927945661834,-3.60152981625657));
#50870=CARTESIAN_POINT('Ctrl Pts',(18.1823545166283,21.7122714336376,-3.60570093023441));
#50871=CARTESIAN_POINT('Ctrl Pts',(18.265023760118,21.7276766352526,-3.60987204421225));
#50872=CARTESIAN_POINT('Ctrl Pts',(18.3476652631446,21.7430766675033,-3.6140417585325));
#50873=CARTESIAN_POINT('Ctrl Pts',(18.4310975176837,21.754407663177,-3.61821147285276));
#50874=CARTESIAN_POINT('Ctrl Pts',(18.5148867965887,21.7616056935737,-3.62238118717302));
#50875=CARTESIAN_POINT('Ctrl Pts',(18.5986730939115,21.7688034678337,-3.62655075311694));
#50876=CARTESIAN_POINT('Ctrl Pts',(18.6828159319229,21.7718685307012,-3.63072031906087));
#50877=CARTESIAN_POINT('Ctrl Pts',(18.7668770686622,21.7707888776921,-3.63488988500479));
#50878=CARTESIAN_POINT('Ctrl Pts',(18.8538936912738,21.7696712654151,-3.63920604774385));
#50879=CARTESIAN_POINT('Ctrl Pts',(18.9408222331037,21.764112064791,-3.6435222104829));
#50880=CARTESIAN_POINT('Ctrl Pts',(19.0271792931092,21.7541566806023,-3.64783837322196));
#50881=CARTESIAN_POINT('Ctrl Pts',(19.1107232809632,21.744525592007,-3.65201393741352));
#50882=CARTESIAN_POINT('Ctrl Pts',(19.193731990268,21.7307804563761,-3.65618950160509));
#50883=CARTESIAN_POINT('Ctrl Pts',(19.2757772698984,21.7130146661883,-3.66036506579665));
#50884=CARTESIAN_POINT('Ctrl Pts',(19.3619664615664,21.6943515681707,-3.66475152780945));
#50885=CARTESIAN_POINT('Ctrl Pts',(19.4470917766263,21.6712511277377,-3.66913798982225));
#50886=CARTESIAN_POINT('Ctrl Pts',(19.5306760960808,21.6438804323134,-3.67352445183505));
#50887=CARTESIAN_POINT('Ctrl Pts',(19.6142604155353,21.6165097368891,-3.67791091384786));
#50888=CARTESIAN_POINT('Ctrl Pts',(19.6963032254016,21.584869066222,-3.68229737586066));
#50889=CARTESIAN_POINT('Ctrl Pts',(19.7763550154477,21.5491822045707,-3.68668383787346));
#50890=CARTESIAN_POINT('Ctrl Pts',(19.8527263004245,21.5151361016724,-3.6908686254994));
#50891=CARTESIAN_POINT('Ctrl Pts',(19.9275699049942,21.4772809673763,-3.69505341312535));
#50892=CARTESIAN_POINT('Ctrl Pts',(20.0004799995006,21.4357760361135,-3.69923820075129));
#50893=CARTESIAN_POINT('Ctrl Pts',(20.0732773467754,21.3943352875421,-3.70341651707552));
#50894=CARTESIAN_POINT('Ctrl Pts',(20.1441467296573,21.3492561841679,-3.70759483339976));
#50895=CARTESIAN_POINT('Ctrl Pts',(20.212703423182,21.3007454836103,-3.71177314972399));
#50896=CARTESIAN_POINT('Ctrl Pts',(20.2400223166183,21.2814146409031,-3.71343815094468));
#50897=CARTESIAN_POINT('Ctrl Pts',(20.2669742248431,21.2615394146186,-3.71510315216536));
#50898=CARTESIAN_POINT('Ctrl Pts',(20.2935358855687,21.2411349269503,-3.71676815338605));
#50899=CARTESIAN_POINT('',(16.174394460606,19.210617605254,-3.3667098651142));
#50900=CARTESIAN_POINT('Ctrl Pts',(16.1740000284928,19.2106180532904,-3.36670989022851));
#50901=CARTESIAN_POINT('Ctrl Pts',(16.1739869935966,19.297984518944,-3.37103154303559));
#50902=CARTESIAN_POINT('Ctrl Pts',(16.1784506871913,19.3852864628672,-3.37535319584266));
#50903=CARTESIAN_POINT('Ctrl Pts',(16.1873453738308,19.472055961455,-3.37967484864974));
#50904=CARTESIAN_POINT('Ctrl Pts',(16.1966194662204,19.5625266412114,-3.38418084296216));
#50905=CARTESIAN_POINT('Ctrl Pts',(16.2107109130556,19.6524179424094,-3.38868683727458));
#50906=CARTESIAN_POINT('Ctrl Pts',(16.2295088315793,19.7412112666689,-3.39319283158699));
#50907=CARTESIAN_POINT('Ctrl Pts',(16.2475982064586,19.8266577339084,-3.39752898296558));
#50908=CARTESIAN_POINT('Ctrl Pts',(16.2700454505064,19.9110871351913,-3.40186513434416));
#50909=CARTESIAN_POINT('Ctrl Pts',(16.2967009964589,19.9940540002691,-3.40620128572275));
#50910=CARTESIAN_POINT('Ctrl Pts',(16.3233900671467,20.0771252129449,-3.41054289068791));
#50911=CARTESIAN_POINT('Ctrl Pts',(16.354297844581,20.1587298407162,-3.41488449565307));
#50912=CARTESIAN_POINT('Ctrl Pts',(16.3892268388774,20.2384428562597,-3.41922610061823));
#50913=CARTESIAN_POINT('Ctrl Pts',(16.4242296046623,20.318324229007,-3.42357687523362));
#50914=CARTESIAN_POINT('Ctrl Pts',(16.4632703651621,20.3963056454692,-3.42792764984902));
#50915=CARTESIAN_POINT('Ctrl Pts',(16.5061059491326,20.4719869539808,-3.43227842446442));
#50916=CARTESIAN_POINT('Ctrl Pts',(16.5109248522386,20.4805009243496,-3.43276787644252));
#50917=CARTESIAN_POINT('Ctrl Pts',(16.5157917376009,20.4889858169829,-3.43325732842063));
#50918=CARTESIAN_POINT('Ctrl Pts',(16.5207062260026,20.4974410868688,-3.43374678039873));
#50919=CARTESIAN_POINT('Ctrl Pts',(16.5627232942887,20.5697305345463,-3.43793141479118));
#50920=CARTESIAN_POINT('Ctrl Pts',(16.608363899273,20.6400938357955,-3.44211604918362));
#50921=CARTESIAN_POINT('Ctrl Pts',(16.6574263400684,20.7081445604478,-3.44630068357607));
#50922=CARTESIAN_POINT('Ctrl Pts',(16.7064189465521,20.7760984233165,-3.4504793616594));
#50923=CARTESIAN_POINT('Ctrl Pts',(16.7588234476462,20.8417458779045,-3.45465803974274));
#50924=CARTESIAN_POINT('Ctrl Pts',(16.8143930615575,20.9047264247462,-3.45883671782608));
#50925=CARTESIAN_POINT('Ctrl Pts',(16.8709587208712,20.9688358526383,-3.46309029571167));
#50926=CARTESIAN_POINT('Ctrl Pts',(16.9308038360938,21.0301814068962,-3.46734387359725));
#50927=CARTESIAN_POINT('Ctrl Pts',(16.9936228831502,21.0884151089052,-3.47159745148284));
#50928=CARTESIAN_POINT('Ctrl Pts',(17.055224060387,21.1455198369568,-3.47576856546018));
#50929=CARTESIAN_POINT('Ctrl Pts',(17.1196845346186,21.1996319675306,-3.47993967943753));
#50930=CARTESIAN_POINT('Ctrl Pts',(17.1866778681087,21.250459296029,-3.48411079341487));
#50931=CARTESIAN_POINT('Ctrl Pts',(17.2536487213387,21.3012695689265,-3.48828050773464));
#50932=CARTESIAN_POINT('Ctrl Pts',(17.3231503796755,21.3487969510058,-3.4924502220544));
#50933=CARTESIAN_POINT('Ctrl Pts',(17.3948237869028,21.3927898776634,-3.49661993637417));
#50934=CARTESIAN_POINT('Ctrl Pts',(17.4664946436827,21.436781238864,-3.50078950231762));
#50935=CARTESIAN_POINT('Ctrl Pts',(17.5403367031862,21.477238154784,-3.50495906826106));
#50936=CARTESIAN_POINT('Ctrl Pts',(17.6159635983352,21.5139534525371,-3.5091286342045));
#50937=CARTESIAN_POINT('Ctrl Pts',(17.6942494418461,21.5519596148778,-3.51344479694414));
#50938=CARTESIAN_POINT('Ctrl Pts',(17.7744474914063,21.5859559226943,-3.51776095968378));
#50939=CARTESIAN_POINT('Ctrl Pts',(17.8561052781564,21.6157662791546,-3.52207712242342));
#50940=CARTESIAN_POINT('Ctrl Pts',(17.9351030710677,21.6446055663799,-3.5262526866145));
#50941=CARTESIAN_POINT('Ctrl Pts',(18.0154664958613,21.6695273345316,-3.53042825080559));
#50942=CARTESIAN_POINT('Ctrl Pts',(18.0967709615466,21.6904231491522,-3.53460381499668));
#50943=CARTESIAN_POINT('Ctrl Pts',(18.1821819225495,21.7123743617041,-3.53899027701059));
#50944=CARTESIAN_POINT('Ctrl Pts',(18.2686309144575,21.7298821146794,-3.5433767390245));
#50945=CARTESIAN_POINT('Ctrl Pts',(18.3556165397336,21.7428819002862,-3.54776320103842));
#50946=CARTESIAN_POINT('Ctrl Pts',(18.4426021650097,21.755881685893,-3.55214966305233));
#50947=CARTESIAN_POINT('Ctrl Pts',(18.5301238388031,21.7643735238079,-3.55653612506624));
#50948=CARTESIAN_POINT('Ctrl Pts',(18.6176794289204,21.7683559636358,-3.56092258708016));
#50949=CARTESIAN_POINT('Ctrl Pts',(18.7011876748678,21.7721543112247,-3.56510628052802));
#50950=CARTESIAN_POINT('Ctrl Pts',(18.7850375342269,21.7718650921499,-3.56928997397588));
#50951=CARTESIAN_POINT('Ctrl Pts',(18.8687951970932,21.7674487585009,-3.57347366742374));
#50952=CARTESIAN_POINT('Ctrl Pts',(18.9524422754805,21.7630382556969,-3.57765183717927));
#50953=CARTESIAN_POINT('Ctrl Pts',(19.0359969440171,21.7545114802047,-3.5818300069348));
#50954=CARTESIAN_POINT('Ctrl Pts',(19.1190226609998,21.7418807855205,-3.58600817669033));
#50955=CARTESIAN_POINT('Ctrl Pts',(19.2019636761051,21.729262976525,-3.59018208392535));
#50956=CARTESIAN_POINT('Ctrl Pts',(19.2843763591294,21.712549632003,-3.59435599116036));
#50957=CARTESIAN_POINT('Ctrl Pts',(19.3658279303823,21.6918050037012,-3.59852989839538));
#50958=CARTESIAN_POINT('Ctrl Pts',(19.4496036345041,21.670468449771,-3.60282290357838));
#50959=CARTESIAN_POINT('Ctrl Pts',(19.532362045609,21.6448670908952,-3.60711590876138));
#50960=CARTESIAN_POINT('Ctrl Pts',(19.613642591816,21.6151274738797,-3.61140891394438));
#50961=CARTESIAN_POINT('Ctrl Pts',(19.692588988533,21.5862418953165,-3.61557863605011));
#50962=CARTESIAN_POINT('Ctrl Pts',(19.770140803741,21.5534527148571,-3.61974835815585));
#50963=CARTESIAN_POINT('Ctrl Pts',(19.845892348409,21.5169261491968,-3.62391808026158));
#50964=CARTESIAN_POINT('Ctrl Pts',(19.9250034275847,21.4787796527704,-3.62827272698321));
#50965=CARTESIAN_POINT('Ctrl Pts',(20.0021503442013,21.4365567646314,-3.63262737370485));
#50966=CARTESIAN_POINT('Ctrl Pts',(20.0768973698964,21.3905014691267,-3.63698202042648));
#50967=CARTESIAN_POINT('Ctrl Pts',(20.1516443955915,21.344446173622,-3.64133666714812));
#50968=CARTESIAN_POINT('Ctrl Pts',(20.2239910581103,21.2945587918557,-3.64569131386975));
#50969=CARTESIAN_POINT('Ctrl Pts',(20.2935358855687,21.2411349269503,-3.65004596059139));
#50970=CARTESIAN_POINT('Ctrl Pts',(20.2912843055177,21.2382340775644,-2.85017128750281));
#50971=CARTESIAN_POINT('Ctrl Pts',(20.6891190168232,20.9296543890738,-2.87512870955954));
#50972=CARTESIAN_POINT('Ctrl Pts',(21.5323502710954,19.7924126903705,-2.94247806717674));
#50973=CARTESIAN_POINT('Ctrl Pts',(21.1037095810087,17.3274479097959,-3.05221936035442));
#50974=CARTESIAN_POINT('Ctrl Pts',(18.4329096216685,16.1989182335261,-3.17939516703586));
#50975=CARTESIAN_POINT('Ctrl Pts',(16.4590845281242,17.5465283070756,-3.28422525531049));
#50976=CARTESIAN_POINT('Ctrl Pts',(16.1776267405031,18.8060181972744,-3.34666340802465));
#50977=CARTESIAN_POINT('Ctrl Pts',(16.1781627672566,19.2106133248248,-3.36670962517832));
#50978=CARTESIAN_POINT('Origin',(18.734,19.211,1.76670989022852));
#50979=CARTESIAN_POINT('',(20.2935358855687,21.2411349269503,-2.05017637612677));
#50980=CARTESIAN_POINT('',(20.2935358855687,21.2411349269503,-2.11663751762489));
#50981=CARTESIAN_POINT('',(20.2935358855687,21.2411349269503,1.76670989022852));
#50982=CARTESIAN_POINT('',(16.1740010149448,19.2132795868243,-2.63329010980609));
#50983=CARTESIAN_POINT('Ctrl Pts',(20.2935358855687,21.2411349269503,-2.11663751762489));
#50984=CARTESIAN_POINT('Ctrl Pts',(20.3602472229086,21.1898877299415,-2.12081218256376));
#50985=CARTESIAN_POINT('Ctrl Pts',(20.424391713608,21.1353781809648,-2.12498684750263));
#50986=CARTESIAN_POINT('Ctrl Pts',(20.485647461214,21.0779041677661,-2.12916151244151));
#50987=CARTESIAN_POINT('Ctrl Pts',(20.5469405618567,21.0203951075881,-2.13333872304211));
#50988=CARTESIAN_POINT('Ctrl Pts',(20.6053410936532,20.9599183157007,-2.13751593364272));
#50989=CARTESIAN_POINT('Ctrl Pts',(20.6605654824905,20.8968070594455,-2.14169314424333));
#50990=CARTESIAN_POINT('Ctrl Pts',(20.7158816120992,20.8335909604667,-2.14587729417872));
#50991=CARTESIAN_POINT('Ctrl Pts',(20.7680107808068,20.7677320210624,-2.15006144411412));
#50992=CARTESIAN_POINT('Ctrl Pts',(20.8167112376172,20.6995946058962,-2.15424559404952));
#50993=CARTESIAN_POINT('Ctrl Pts',(20.8412645276369,20.6652417922813,-2.1563551152651));
#50994=CARTESIAN_POINT('Ctrl Pts',(20.8649469909646,20.6303102486314,-2.15846463648067));
#50995=CARTESIAN_POINT('Ctrl Pts',(20.887732090256,20.5948490103337,-2.16057415769625));
#50996=CARTESIAN_POINT('Ctrl Pts',(20.9329306422986,20.5245049401061,-2.16475879183929));
#50997=CARTESIAN_POINT('Ctrl Pts',(20.9747633711854,20.4518132565708,-2.16894342598234));
#50998=CARTESIAN_POINT('Ctrl Pts',(21.0129782252718,20.3771296020327,-2.17312806012539));
#50999=CARTESIAN_POINT('Ctrl Pts',(21.0511386852002,20.3025522505174,-2.17730673795494));
#51000=CARTESIAN_POINT('Ctrl Pts',(21.0856912912948,20.2259889658803,-2.1814854157845));
#51001=CARTESIAN_POINT('Ctrl Pts',(21.1164276176732,20.1478237008892,-2.18566409361405));
#51002=CARTESIAN_POINT('Ctrl Pts',(21.1477148729807,20.0682573736764,-2.18991767156253));
#51003=CARTESIAN_POINT('Ctrl Pts',(21.1750474280242,19.9870314755984,-2.19417124951102));
#51004=CARTESIAN_POINT('Ctrl Pts',(21.1982547719723,19.9045765414226,-2.1984248274595));
#51005=CARTESIAN_POINT('Ctrl Pts',(21.2210121944984,19.8237201633468,-2.20259594117411));
#51006=CARTESIAN_POINT('Ctrl Pts',(21.2398027993352,19.7416824418443,-2.20676705488871));
#51007=CARTESIAN_POINT('Ctrl Pts',(21.2545152522168,19.658887110043,-2.21093816860331));
#51008=CARTESIAN_POINT('Ctrl Pts',(21.2692227681826,19.5761195610716,-2.21510788265757));
#51009=CARTESIAN_POINT('Ctrl Pts',(21.2798547695701,19.4925953592547,-2.21927759671182));
#51010=CARTESIAN_POINT('Ctrl Pts',(21.2863509615982,19.4087487517752,-2.22344731076607));
#51011=CARTESIAN_POINT('Ctrl Pts',(21.2928469224601,19.3249051279668,-2.22761687644157));
#51012=CARTESIAN_POINT('Ctrl Pts',(21.295207331893,19.2407395800309,-2.23178644211707));
#51013=CARTESIAN_POINT('Ctrl Pts',(21.2934238553146,19.1566904350363,-2.23595600779257));
#51014=CARTESIAN_POINT('Ctrl Pts',(21.2915776736484,19.0696862139404,-2.24027217084133));
#51015=CARTESIAN_POINT('Ctrl Pts',(21.2852907961475,18.9828072608784,-2.24458833389009));
#51016=CARTESIAN_POINT('Ctrl Pts',(21.2746126736334,18.8965365799125,-2.24890449693885));
#51017=CARTESIAN_POINT('Ctrl Pts',(21.2642823912514,18.8130761687308,-2.25308006085863));
#51018=CARTESIAN_POINT('Ctrl Pts',(21.2498426885277,18.730185465086,-2.25725562477842));
#51019=CARTESIAN_POINT('Ctrl Pts',(21.231390539663,18.6482918230543,-2.26143118869821));
#51020=CARTESIAN_POINT('Ctrl Pts',(21.2120064127083,18.562261910464,-2.26581765131146));
#51021=CARTESIAN_POINT('Ctrl Pts',(21.1881940056825,18.4773329923524,-2.2702041139247));
#51022=CARTESIAN_POINT('Ctrl Pts',(21.1601243952751,18.3939807721657,-2.27459057653795));
#51023=CARTESIAN_POINT('Ctrl Pts',(21.1320547848677,18.3106285519789,-2.27897703915119));
#51024=CARTESIAN_POINT('Ctrl Pts',(21.0997282551214,18.2288535413399,-2.28336350176443));
#51025=CARTESIAN_POINT('Ctrl Pts',(21.0633723464423,18.1491033611364,-2.28774996437768));
#51026=CARTESIAN_POINT('Ctrl Pts',(21.0286892306356,18.0730226128866,-2.29193459890683));
#51027=CARTESIAN_POINT('Ctrl Pts',(20.9902102866642,17.9985012713197,-2.29611923343598));
#51028=CARTESIAN_POINT('Ctrl Pts',(20.9480981227546,17.925943774454,-2.30030386796514));
#51029=CARTESIAN_POINT('Ctrl Pts',(20.9060459002788,17.8534895541713,-2.30448254618689));
#51030=CARTESIAN_POINT('Ctrl Pts',(20.8603709589165,17.7829940207375,-2.30866122440865));
#51031=CARTESIAN_POINT('Ctrl Pts',(20.8112833253067,17.7148402537152,-2.3128399026304));
#51032=CARTESIAN_POINT('Ctrl Pts',(20.7613158331932,17.6454648822467,-2.3170934804816));
#51033=CARTESIAN_POINT('Ctrl Pts',(20.7078123007188,17.5785164937711,-2.32134705833279));
#51034=CARTESIAN_POINT('Ctrl Pts',(20.6510424452123,17.5143715011074,-2.32560063618399));
#51035=CARTESIAN_POINT('Ctrl Pts',(20.5953731818021,17.4514700816625,-2.32977175030294));
#51036=CARTESIAN_POINT('Ctrl Pts',(20.5365634319281,17.3912646900244,-2.33394286442189));
#51037=CARTESIAN_POINT('Ctrl Pts',(20.4749092250524,17.3340782994148,-2.33811397854084));
#51038=CARTESIAN_POINT('Ctrl Pts',(20.4132757068275,17.2769110982382,-2.34228369300309));
#51039=CARTESIAN_POINT('Ctrl Pts',(20.3487999642247,17.2227611987298,-2.34645340746534));
#51040=CARTESIAN_POINT('Ctrl Pts',(20.281814494063,17.1719143490357,-2.35062312192759));
#51041=CARTESIAN_POINT('Ctrl Pts',(20.2148314075206,17.1210693086822,-2.35479268801421));
#51042=CARTESIAN_POINT('Ctrl Pts',(20.1453391379229,17.073527361915,-2.35896225410082));
#51043=CARTESIAN_POINT('Ctrl Pts',(20.0737017376934,17.0295327749376,-2.36313182018743));
#51044=CARTESIAN_POINT('Ctrl Pts',(19.9995456602385,16.983991395867,-2.36744798276007));
#51045=CARTESIAN_POINT('Ctrl Pts',(19.9230912497119,16.942251743645,-2.37176414533271));
#51046=CARTESIAN_POINT('Ctrl Pts',(19.8447714026906,16.9045336787708,-2.37608030790535));
#51047=CARTESIAN_POINT('Ctrl Pts',(19.769002810937,16.8680442732384,-2.38025587223989));
#51048=CARTESIAN_POINT('Ctrl Pts',(19.6914889015773,16.8353186124795,-2.38443143657442));
#51049=CARTESIAN_POINT('Ctrl Pts',(19.6126415021214,16.8065064752115,-2.38860700090896));
#51050=CARTESIAN_POINT('Ctrl Pts',(19.5298117168534,16.7762391086339,-2.39299346260065));
#51051=CARTESIAN_POINT('Ctrl Pts',(19.4455107504595,16.7502911703632,-2.39737992429234));
#51052=CARTESIAN_POINT('Ctrl Pts',(19.3602311944416,16.7287763011549,-2.40176638598403));
#51053=CARTESIAN_POINT('Ctrl Pts',(19.2749516384237,16.7072614319465,-2.40615284767573));
#51054=CARTESIAN_POINT('Ctrl Pts',(19.1886940767219,16.6901796698973,-2.41053930936742));
#51055=CARTESIAN_POINT('Ctrl Pts',(19.1019580505852,16.6775819782338,-2.41492577105911));
#51056=CARTESIAN_POINT('Ctrl Pts',(19.0192128717126,16.6655639241852,-2.41911040544303));
#51057=CARTESIAN_POINT('Ctrl Pts',(18.9357242972398,16.6575816378624,-2.42329503982696));
#51058=CARTESIAN_POINT('Ctrl Pts',(18.8519204122534,16.6537173061286,-2.42747967421088));
#51059=CARTESIAN_POINT('Ctrl Pts',(18.7682358117204,16.6498584747926,-2.43165835228591));
#51060=CARTESIAN_POINT('Ctrl Pts',(18.6842372477567,16.6501059764731,-2.43583703036094));
#51061=CARTESIAN_POINT('Ctrl Pts',(18.6003605130588,16.6544905657264,-2.44001570843598));
#51062=CARTESIAN_POINT('Ctrl Pts',(18.5149803479453,16.6589537456027,-2.44426928632367));
#51063=CARTESIAN_POINT('Ctrl Pts',(18.4297268997696,16.6677038557791,-2.44852286421136));
#51064=CARTESIAN_POINT('Ctrl Pts',(18.3450626650525,16.6807178518031,-2.45277644209905));
#51065=CARTESIAN_POINT('Ctrl Pts',(18.2620398119428,16.6934795460874,-2.45694755606873));
#51066=CARTESIAN_POINT('Ctrl Pts',(18.1795840056908,16.7103412009465,-2.4611186700384));
#51067=CARTESIAN_POINT('Ctrl Pts',(18.0981270507742,16.7312287217481,-2.46528978400808));
#51068=CARTESIAN_POINT('Ctrl Pts',(18.0166974295208,16.7521092335416,-2.46945949832043));
#51069=CARTESIAN_POINT('Ctrl Pts',(17.9362664391865,16.7770128141616,-2.47362921263277));
#51070=CARTESIAN_POINT('Ctrl Pts',(17.8572543229417,16.8058145564719,-2.47779892694511));
#51071=CARTESIAN_POINT('Ctrl Pts',(17.7782450182819,16.8346152738944,-2.4819684928814));
#51072=CARTESIAN_POINT('Ctrl Pts',(17.7006549192462,16.8673137188579,-2.48613805881768));
#51073=CARTESIAN_POINT('Ctrl Pts',(17.6248864697071,16.9037359975674,-2.49030762475396));
#51074=CARTESIAN_POINT('Ctrl Pts',(17.5464540946258,16.9414388388218,-2.49462378750285));
#51075=CARTESIAN_POINT('Ctrl Pts',(17.4699743261962,16.9831320174928,-2.49893995025173));
#51076=CARTESIAN_POINT('Ctrl Pts',(17.3958663510844,17.0285705423451,-2.50325611300061));
#51077=CARTESIAN_POINT('Ctrl Pts',(17.3241724357532,17.0725289118542,-2.50743167718527));
#51078=CARTESIAN_POINT('Ctrl Pts',(17.2546985266629,17.1199920607128,-2.51160724136992));
#51079=CARTESIAN_POINT('Ctrl Pts',(17.1877934784099,17.1706947795508,-2.51578280555458));
#51080=CARTESIAN_POINT('Ctrl Pts',(17.1175092148074,17.2239583724966,-2.52016926758558));
#51081=CARTESIAN_POINT('Ctrl Pts',(17.0500605848372,17.2807970211557,-2.52455572961657));
#51082=CARTESIAN_POINT('Ctrl Pts',(16.9858097729217,17.3408580455089,-2.52894219164757));
#51083=CARTESIAN_POINT('Ctrl Pts',(16.9215589610061,17.4009190698621,-2.53332865367856));
#51084=CARTESIAN_POINT('Ctrl Pts',(16.8605063152544,17.4642019995291,-2.53771511570956));
#51085=CARTESIAN_POINT('Ctrl Pts',(16.802965079949,17.53031438468,-2.54210157774055));
#51086=CARTESIAN_POINT('Ctrl Pts',(16.7485317522924,17.5928559186595,-2.54625111891253));
#51087=CARTESIAN_POINT('Ctrl Pts',(16.6970294692197,17.6581717364498,-2.55040066008451));
#51088=CARTESIAN_POINT('Ctrl Pts',(16.6487573722079,17.7259534743858,-2.55455020125649));
#51089=CARTESIAN_POINT('Ctrl Pts',(16.600549374283,17.7936452069609,-2.55869423237573));
#51090=CARTESIAN_POINT('Ctrl Pts',(16.5555633203294,17.8637959851695,-2.56283826349497));
#51091=CARTESIAN_POINT('Ctrl Pts',(16.5140597201748,17.9360626862432,-2.56698229461421));
#51092=CARTESIAN_POINT('Ctrl Pts',(16.4725982721945,18.0082559913085,-2.57112211694382));
#51093=CARTESIAN_POINT('Ctrl Pts',(16.4346124893249,18.0825605501313,-2.57526193927342));
#51094=CARTESIAN_POINT('Ctrl Pts',(16.4003201033264,18.1586036203684,-2.57940176160303));
#51095=CARTESIAN_POINT('Ctrl Pts',(16.3660518421391,18.2345931940449,-2.58353867155343));
#51096=CARTESIAN_POINT('Ctrl Pts',(16.3354720095434,18.3123184246929,-2.58767558150382));
#51097=CARTESIAN_POINT('Ctrl Pts',(16.3087521158413,18.3913825890187,-2.59181249145422));
#51098=CARTESIAN_POINT('Ctrl Pts',(16.2820372325134,18.4704319276473,-2.59594862567298));
#51099=CARTESIAN_POINT('Ctrl Pts',(16.2591810094474,18.5508192612106,-2.60008475989173));
#51100=CARTESIAN_POINT('Ctrl Pts',(16.2403061251843,18.6321296702138,-2.60422089411049));
#51101=CARTESIAN_POINT('Ctrl Pts',(16.2214331728159,18.7134317568803,-2.6083566049849));
#51102=CARTESIAN_POINT('Ctrl Pts',(16.2065408484307,18.7956562735366,-2.61249231585931));
#51103=CARTESIAN_POINT('Ctrl Pts',(16.1957010120579,18.878376717874,-2.61662802673372));
#51104=CARTESIAN_POINT('Ctrl Pts',(16.1848552750843,18.9611421905962,-2.62076598885789));
#51105=CARTESIAN_POINT('Ctrl Pts',(16.1780664813585,19.0444036643639,-2.62490395098206));
#51106=CARTESIAN_POINT('Ctrl Pts',(16.175354661978,19.1277291514511,-2.62904191310623));
#51107=CARTESIAN_POINT('Ctrl Pts',(16.1744266413965,19.1562442389712,-2.63045797866132));
#51108=CARTESIAN_POINT('Ctrl Pts',(16.1739756253558,19.1847668138065,-2.63187404421641));
#51109=CARTESIAN_POINT('Ctrl Pts',(16.1740010149441,19.213279586128,-2.6332901097715));
#51110=CARTESIAN_POINT('Ctrl Pts',(16.1740010149447,19.2132795868243,-2.63329010980609));
#51111=CARTESIAN_POINT('Ctrl Pts',(16.1740928743929,19.3164386732002,-2.6384134288319));
#51112=CARTESIAN_POINT('Ctrl Pts',(16.1804238944875,19.4193213099348,-2.64353674785771));
#51113=CARTESIAN_POINT('Ctrl Pts',(16.1928719236876,19.5212710102101,-2.64866006688352));
#51114=CARTESIAN_POINT('Ctrl Pts',(16.2055250386105,19.6249003681759,-2.65386779441843));
#51115=CARTESIAN_POINT('Ctrl Pts',(16.2244983314989,19.7275658814857,-2.65907552195333));
#51116=CARTESIAN_POINT('Ctrl Pts',(16.2496149571641,19.8286009706384,-2.66428324948824));
#51117=CARTESIAN_POINT('Ctrl Pts',(16.2576437833531,19.8608980307853,-2.66594796113282));
#51118=CARTESIAN_POINT('Ctrl Pts',(16.2662999939973,19.8930286552691,-2.6676126727774));
#51119=CARTESIAN_POINT('Ctrl Pts',(16.2755767948953,19.9249715292663,-2.66927738442198));
#51120=CARTESIAN_POINT('Ctrl Pts',(16.2988961609903,20.0052672671023,-2.67346201883521));
#51121=CARTESIAN_POINT('Ctrl Pts',(16.3261969265522,20.084568763058,-2.67764665324844));
#51122=CARTESIAN_POINT('Ctrl Pts',(16.3573766633344,20.1624523191503,-2.68183128766167));
#51123=CARTESIAN_POINT('Ctrl Pts',(16.3885120196228,20.240225017646,-2.68600996576606));
#51124=CARTESIAN_POINT('Ctrl Pts',(16.4235152107072,20.3165833617541,-2.69018864387045));
#51125=CARTESIAN_POINT('Ctrl Pts',(16.4622338002162,20.391117932039,-2.69436732197484));
#51126=CARTESIAN_POINT('Ctrl Pts',(16.5016463923758,20.4669884804673,-2.6986208998552));
#51127=CARTESIAN_POINT('Ctrl Pts',(16.5449087556001,20.5409687666981,-2.70287447773556));
#51128=CARTESIAN_POINT('Ctrl Pts',(16.5918084260801,20.6126473381798,-2.70712805561591));
#51129=CARTESIAN_POINT('Ctrl Pts',(16.6377988552166,20.6829362811212,-2.71129916961482));
#51130=CARTESIAN_POINT('Ctrl Pts',(16.6872865541289,20.7510115566489,-2.71547028361373));
#51131=CARTESIAN_POINT('Ctrl Pts',(16.7400252973105,20.8165107863339,-2.71964139761264));
#51132=CARTESIAN_POINT('Ctrl Pts',(16.7927463434994,20.8819880371221,-2.72381111195412));
#51133=CARTESIAN_POINT('Ctrl Pts',(16.848715979104,20.9448906007935,-2.7279808262956));
#51134=CARTESIAN_POINT('Ctrl Pts',(16.907646512581,21.0048876606389,-2.73215054063707));
#51135=CARTESIAN_POINT('Ctrl Pts',(16.9665749490584,21.0648825855331,-2.73632010660234));
#51136=CARTESIAN_POINT('Ctrl Pts',(17.0284637509525,21.1219718845682,-2.74048967256761));
#51137=CARTESIAN_POINT('Ctrl Pts',(17.0929880053961,21.1758612250147,-2.74465923853288));
#51138=CARTESIAN_POINT('Ctrl Pts',(17.1597808523044,21.2316452475883,-2.74897540124709));
#51139=CARTESIAN_POINT('Ctrl Pts',(17.2293975200615,21.2839997657393,-2.7532915639613));
#51140=CARTESIAN_POINT('Ctrl Pts',(17.3014414464079,21.3326446428491,-2.75760772667551));
#51141=CARTESIAN_POINT('Ctrl Pts',(17.3711385501858,21.3797049187129,-2.76178329088849));
#51142=CARTESIAN_POINT('Ctrl Pts',(17.4431067778014,21.4232933214559,-2.76595885510147));
#51143=CARTESIAN_POINT('Ctrl Pts',(17.5169602827148,21.4632021060621,-2.77013441931445));
#51144=CARTESIAN_POINT('Ctrl Pts',(17.5945439513518,21.5051265878347,-2.77452088127928));
#51145=CARTESIAN_POINT('Ctrl Pts',(17.6742078257196,21.5429897170844,-2.77890734324411));
#51146=CARTESIAN_POINT('Ctrl Pts',(17.7554809190361,21.5766078305986,-2.78329380520893));
#51147=CARTESIAN_POINT('Ctrl Pts',(17.8367540123527,21.6102259441129,-2.78768026717376));
#51148=CARTESIAN_POINT('Ctrl Pts',(17.9196357523206,21.639598919772,-2.79206672913859));
#51149=CARTESIAN_POINT('Ctrl Pts',(18.0036392138267,21.6646041086574,-2.79645319110342));
#51150=CARTESIAN_POINT('Ctrl Pts',(18.0837805456624,21.6884596629898,-2.80063798179663));
#51151=CARTESIAN_POINT('Ctrl Pts',(18.1652410320985,21.7084290356245,-2.80482277248983));
#51152=CARTESIAN_POINT('Ctrl Pts',(18.2476089212223,21.7243689976773,-2.80900756318304));
#51153=CARTESIAN_POINT('Ctrl Pts',(18.329858738654,21.7402861103125,-2.81318635511479));
#51154=CARTESIAN_POINT('Ctrl Pts',(18.4130129271253,21.7521851992249,-2.81736514704654));
#51155=CARTESIAN_POINT('Ctrl Pts',(18.4966446832044,21.7599728232347,-2.82154393897828));
#51156=CARTESIAN_POINT('Ctrl Pts',(18.5801762046835,21.7677511135963,-2.82571772253095));
#51157=CARTESIAN_POINT('Ctrl Pts',(18.6641837002169,21.7714276931344,-2.82989150608361));
#51158=CARTESIAN_POINT('Ctrl Pts',(18.7482317172097,21.770960440754,-2.83406528963627));
#51159=CARTESIAN_POINT('Ctrl Pts',(18.8322246249339,21.7704934947452,-2.83823633648952));
#51160=CARTESIAN_POINT('Ctrl Pts',(18.9162575426888,21.7658881143946,-2.84240738334278));
#51161=CARTESIAN_POINT('Ctrl Pts',(18.9998925087996,21.7571541928493,-2.84657843019603));
#51162=CARTESIAN_POINT('Ctrl Pts',(19.0834977254746,21.7484233780099,-2.85074799338406));
#51163=CARTESIAN_POINT('Ctrl Pts',(19.1667048146448,21.7355669871508,-2.85491755657209));
#51164=CARTESIAN_POINT('Ctrl Pts',(19.2490798028149,21.7186468644393,-2.85908711976013));
#51165=CARTESIAN_POINT('Ctrl Pts',(19.3314501999326,21.7017276847466,-2.86325645056351));
#51166=CARTESIAN_POINT('Ctrl Pts',(19.4129881380694,21.6807453176226,-2.8674257813669));
#51167=CARTESIAN_POINT('Ctrl Pts',(19.4932700684876,21.6558126642135,-2.87159511217028));
#51168=CARTESIAN_POINT('Ctrl Pts',(19.5736163334739,21.6308600308229,-2.87576778410031));
#51169=CARTESIAN_POINT('Ctrl Pts',(19.6527041405867,21.6019509257347,-2.87994045603033));
#51170=CARTESIAN_POINT('Ctrl Pts',(19.7301259599786,21.5692478817666,-2.88411312796035));
#51171=CARTESIAN_POINT('Ctrl Pts',(19.8075810658885,21.5365307775443,-2.88828759387715));
#51172=CARTESIAN_POINT('Ctrl Pts',(19.8833683419578,21.5000166836297,-2.89246205979394));
#51173=CARTESIAN_POINT('Ctrl Pts',(19.9571031322698,21.4599150112514,-2.89663652571074));
#51174=CARTESIAN_POINT('Ctrl Pts',(20.0309449059695,21.4197551544971,-2.9008170484496));
#51175=CARTESIAN_POINT('Ctrl Pts',(20.1027278532631,21.3759975629064,-2.90499757118846));
#51176=CARTESIAN_POINT('Ctrl Pts',(20.1720950490314,21.3288958024302,-2.90917809392733));
#51177=CARTESIAN_POINT('Ctrl Pts',(20.2134569395969,21.3008102233509,-2.91167083306888));
#51178=CARTESIAN_POINT('Ctrl Pts',(20.2539605167435,21.2715364569413,-2.91416357221043));
#51179=CARTESIAN_POINT('Ctrl Pts',(20.2935358855687,21.2411349269503,-2.91665631135199));
#51180=CARTESIAN_POINT('',(16.1740009418753,19.2088040034395,-2.56670989022851));
#51181=CARTESIAN_POINT('Ctrl Pts',(16.17268506744,19.2088155460777,-2.56671052147119));
#51182=CARTESIAN_POINT('Ctrl Pts',(16.1790130470455,19.904586810716,-2.60137099441749));
#51183=CARTESIAN_POINT('Ctrl Pts',(16.8320815026504,21.4617759084344,-2.67842340292429));
#51184=CARTESIAN_POINT('Ctrl Pts',(18.916759365406,22.004542103009,-2.77291032493482));
#51185=CARTESIAN_POINT('Ctrl Pts',(20.0133687968266,21.4537986792987,-2.83273677399906));
#51186=CARTESIAN_POINT('Ctrl Pts',(20.2912843055177,21.2382340775644,-2.85017128750281));
#51187=CARTESIAN_POINT('Ctrl Pts',(20.2935358855687,21.2411349269503,-2.05017637612677));
#51188=CARTESIAN_POINT('Ctrl Pts',(20.359994771256,21.1900816615893,-2.05435390919074));
#51189=CARTESIAN_POINT('Ctrl Pts',(20.4240373077701,21.1356899351298,-2.05853144225471));
#51190=CARTESIAN_POINT('Ctrl Pts',(20.4853117216981,21.0782191230391,-2.06270897531868));
#51191=CARTESIAN_POINT('Ctrl Pts',(20.5465213891913,21.0208090382561,-2.06688209413607));
#51192=CARTESIAN_POINT('Ctrl Pts',(20.6049684136104,20.9603266476494,-2.07105521295346));
#51193=CARTESIAN_POINT('Ctrl Pts',(20.6603338871675,20.8970716933601,-2.07522833177086));
#51194=CARTESIAN_POINT('Ctrl Pts',(20.7156675768893,20.8338530520456,-2.07939905491252));
#51195=CARTESIAN_POINT('Ctrl Pts',(20.7679229256929,20.7678653524743,-2.08356977805419));
#51196=CARTESIAN_POINT('Ctrl Pts',(20.816818521466,20.6994444922933,-2.08774050119586));
#51197=CARTESIAN_POINT('Ctrl Pts',(20.8657007153038,20.6310423857838,-2.09191008117196));
#51198=CARTESIAN_POINT('Ctrl Pts',(20.9112247179256,20.5602088174111,-2.09607966114805));
#51199=CARTESIAN_POINT('Ctrl Pts',(20.9531508438531,20.4873109073522,-2.10024924112415));
#51200=CARTESIAN_POINT('Ctrl Pts',(20.9950780549202,20.4144111105363,-2.10441892901808));
#51201=CARTESIAN_POINT('Ctrl Pts',(21.0334069761503,20.3394472653802,-2.10858861691201));
#51202=CARTESIAN_POINT('Ctrl Pts',(21.0679432142698,20.2628122800976,-2.11275830480594));
#51203=CARTESIAN_POINT('Ctrl Pts',(21.1025145449794,20.1860994252995,-2.11693222955821));
#51204=CARTESIAN_POINT('Ctrl Pts',(21.1332853054147,20.1077124589645,-2.12110615431048));
#51205=CARTESIAN_POINT('Ctrl Pts',(21.1601089494097,20.0280650926297,-2.12528007906274));
#51206=CARTESIAN_POINT('Ctrl Pts',(21.1869458971437,19.9483782235423,-2.129456073959));
#51207=CARTESIAN_POINT('Ctrl Pts',(21.2098317036757,19.8674301524326,-2.13363206885525));
#51208=CARTESIAN_POINT('Ctrl Pts',(21.2286701984997,19.7856482408549,-2.13780806375151));
#51209=CARTESIAN_POINT('Ctrl Pts',(21.2475424627081,19.7037197291988,-2.14199154442509));
#51210=CARTESIAN_POINT('Ctrl Pts',(21.2623528375578,19.6209548443099,-2.14617502509867));
#51211=CARTESIAN_POINT('Ctrl Pts',(21.273056640058,19.537789501939,-2.15035850577225));
#51212=CARTESIAN_POINT('Ctrl Pts',(21.2829756092266,19.4607220796968,-2.15423524170963));
#51213=CARTESIAN_POINT('Ctrl Pts',(21.2893686863835,19.3833111209002,-2.158111977647));
#51214=CARTESIAN_POINT('Ctrl Pts',(21.292240293453,19.3059031135093,-2.16198871358438));
#51215=CARTESIAN_POINT('Ctrl Pts',(21.2953399702058,19.2223471829115,-2.16617334886756));
#51216=CARTESIAN_POINT('Ctrl Pts',(21.2943475192288,19.1384837390471,-2.17035798415075));
#51217=CARTESIAN_POINT('Ctrl Pts',(21.2892270081185,19.0547472016827,-2.17454261943394));
#51218=CARTESIAN_POINT('Ctrl Pts',(21.2841137854076,18.9711298526819,-2.17872129841839));
#51219=CARTESIAN_POINT('Ctrl Pts',(21.2748842015326,18.88763950663,-2.18289997740284));
#51220=CARTESIAN_POINT('Ctrl Pts',(21.2615542857283,18.8047127460814,-2.18707865638728));
#51221=CARTESIAN_POINT('Ctrl Pts',(21.2479854444013,18.7202996055814,-2.19133223404889));
#51222=CARTESIAN_POINT('Ctrl Pts',(21.2301678127982,18.6364709353496,-2.19558581171049));
#51223=CARTESIAN_POINT('Ctrl Pts',(21.2081737664701,18.5536841145149,-2.1998393893721));
#51224=CARTESIAN_POINT('Ctrl Pts',(21.1866061117593,18.4725022555819,-2.20401050426942));
#51225=CARTESIAN_POINT('Ctrl Pts',(21.1610226544981,18.3923226756034,-2.20818161916673));
#51226=CARTESIAN_POINT('Ctrl Pts',(21.1315432452061,18.3135667783247,-2.21235273406405));
#51227=CARTESIAN_POINT('Ctrl Pts',(21.1020737279769,18.2348373082472,-2.21652244930882));
#51228=CARTESIAN_POINT('Ctrl Pts',(21.0687110162085,18.1575310025734,-2.22069216455359));
#51229=CARTESIAN_POINT('Ctrl Pts',(21.0316242450291,18.0820523357327,-2.22486187979835));
#51230=CARTESIAN_POINT('Ctrl Pts',(20.9945387935218,18.0065763546772,-2.2290314466706));
#51231=CARTESIAN_POINT('Ctrl Pts',(20.9537297497136,17.9329282956594,-2.23320101354286));
#51232=CARTESIAN_POINT('Ctrl Pts',(20.9094130508257,17.861489696854,-2.23737058041511));
#51233=CARTESIAN_POINT('Ctrl Pts',(20.8635382532167,17.7875394400905,-2.24168674206933));
#51234=CARTESIAN_POINT('Ctrl Pts',(20.8139048345105,17.7159573495152,-2.24600290372356));
#51235=CARTESIAN_POINT('Ctrl Pts',(20.7608012117929,17.6471340057809,-2.25031906537778));
#51236=CARTESIAN_POINT('Ctrl Pts',(20.7094274096687,17.5805525436961,-2.25449463049769));
#51237=CARTESIAN_POINT('Ctrl Pts',(20.6548063540235,17.5165531862989,-2.25867019561761));
#51238=CARTESIAN_POINT('Ctrl Pts',(20.5972390426215,17.4554544238184,-2.26284576073752));
#51239=CARTESIAN_POINT('Ctrl Pts',(20.5367641854478,17.3912697529606,-2.2672322206589));
#51240=CARTESIAN_POINT('Ctrl Pts',(20.4730380462776,17.3302867949802,-2.27161868058029));
#51241=CARTESIAN_POINT('Ctrl Pts',(20.4064500166287,17.27282793801,-2.27600514050167));
#51242=CARTESIAN_POINT('Ctrl Pts',(20.3398619869799,17.2153690810398,-2.28039160042305));
#51243=CARTESIAN_POINT('Ctrl Pts',(20.2704125717623,17.161434620885,-2.28477806034443));
#51244=CARTESIAN_POINT('Ctrl Pts',(20.1985254700647,17.1112940330771,-2.28916452026581));
#51245=CARTESIAN_POINT('Ctrl Pts',(20.1299459675149,17.0634604650486,-2.29334915467531));
#51246=CARTESIAN_POINT('Ctrl Pts',(20.0588929044646,17.0189012759396,-2.2975337890848));
#51247=CARTESIAN_POINT('Ctrl Pts',(19.9857121094414,16.9778818224111,-2.3017184234943));
#51248=CARTESIAN_POINT('Ctrl Pts',(19.9126354781723,16.9369207549698,-2.30589710159751));
#51249=CARTESIAN_POINT('Ctrl Pts',(19.8374375284665,16.8994896383239,-2.31007577970071));
#51250=CARTESIAN_POINT('Ctrl Pts',(19.7604940332793,16.8658113083076,-2.31425445780392));
#51251=CARTESIAN_POINT('Ctrl Pts',(19.6821713816824,16.8315293186239,-2.31850803568489));
#51252=CARTESIAN_POINT('Ctrl Pts',(19.6020403867561,16.8011362520523,-2.32276161356587));
#51253=CARTESIAN_POINT('Ctrl Pts',(19.5205248076185,16.7748188230346,-2.32701519144684));
#51254=CARTESIAN_POINT('Ctrl Pts',(19.4405895664632,16.7490116085441,-2.33118630545089));
#51255=CARTESIAN_POINT('Ctrl Pts',(19.3593234056723,16.7271235613564,-2.33535741945493));
#51256=CARTESIAN_POINT('Ctrl Pts',(19.2771455317487,16.7092820040337,-2.33952853345898));
#51257=CARTESIAN_POINT('Ctrl Pts',(19.1949952333547,16.6914464336072,-2.34369824780796));
#51258=CARTESIAN_POINT('Ctrl Pts',(19.1119342786025,16.6776547538833,-2.34786796215693));
#51259=CARTESIAN_POINT('Ctrl Pts',(19.0283943159519,16.6679836833525,-2.3520376765059));
#51260=CARTESIAN_POINT('Ctrl Pts',(18.9448573259619,16.6583129569542,-2.35620724248102));
#51261=CARTESIAN_POINT('Ctrl Pts',(18.8608418190422,16.6527626002741,-2.36037680845614));
#51262=CARTESIAN_POINT('Ctrl Pts',(18.7767854909837,16.6513575636896,-2.36454637443126));
#51263=CARTESIAN_POINT('Ctrl Pts',(18.6897738473637,16.6499031277727,-2.36886253714093));
#51264=CARTESIAN_POINT('Ctrl Pts',(18.602718986005,16.6528909431625,-2.3731786998506));
#51265=CARTESIAN_POINT('Ctrl Pts',(18.516105438621,16.6602899106089,-2.37749486256026));
#51266=CARTESIAN_POINT('Ctrl Pts',(18.4323133171228,16.6674478575809,-2.38167042678893));
#51267=CARTESIAN_POINT('Ctrl Pts',(18.3489346599913,16.6787338735485,-2.3858459910176));
#51268=CARTESIAN_POINT('Ctrl Pts',(18.2664001913304,16.694067259752,-2.39002155524626));
#51269=CARTESIAN_POINT('Ctrl Pts',(18.1796971048655,16.7101750984693,-2.39440801719643));
#51270=CARTESIAN_POINT('Ctrl Pts',(18.0939262957202,16.7307497815375,-2.39879447914659));
#51271=CARTESIAN_POINT('Ctrl Pts',(18.0095696123178,16.7556383945735,-2.40318094109676));
#51272=CARTESIAN_POINT('Ctrl Pts',(17.9252129289154,16.7805270076095,-2.40756740304692));
#51273=CARTESIAN_POINT('Ctrl Pts',(17.8422708932813,16.8097292861762,-2.41195386499709));
#51274=CARTESIAN_POINT('Ctrl Pts',(17.7611994326656,16.8430348279179,-2.41634032694725));
#51275=CARTESIAN_POINT('Ctrl Pts',(17.6838581936306,16.8748079308751,-2.42052496109137));
#51276=CARTESIAN_POINT('Ctrl Pts',(17.6079312972171,16.9104332654877,-2.42470959523549));
#51277=CARTESIAN_POINT('Ctrl Pts',(17.5338290567806,16.9497636773101,-2.4288942293796));
#51278=CARTESIAN_POINT('Ctrl Pts',(17.4598322917951,16.9890381071151,-2.43307290721024));
#51279=CARTESIAN_POINT('Ctrl Pts',(17.3876554268513,17.0320069250301,-2.43725158504088));
#51280=CARTESIAN_POINT('Ctrl Pts',(17.3176892303787,17.0784747823637,-2.44143026287152));
#51281=CARTESIAN_POINT('Ctrl Pts',(17.2464689347497,17.1257755462096,-2.44568384081973));
#51282=CARTESIAN_POINT('Ctrl Pts',(17.1775397858983,17.1767018411992,-2.44993741876795));
#51283=CARTESIAN_POINT('Ctrl Pts',(17.1112881539821,17.2309984179822,-2.45419099671616));
#51284=CARTESIAN_POINT('Ctrl Pts',(17.046320944273,17.2842423455401,-2.45836211043189));
#51285=CARTESIAN_POINT('Ctrl Pts',(16.9839287319629,17.3407267365349,-2.46253322414762));
#51286=CARTESIAN_POINT('Ctrl Pts',(16.9244454837024,17.4001680220001,-2.46670433786335));
#51287=CARTESIAN_POINT('Ctrl Pts',(16.864982195661,17.4595893613273,-2.47087405191874));
#51288=CARTESIAN_POINT('Ctrl Pts',(16.80842625819,17.5219652996602,-2.47504376597413));
#51289=CARTESIAN_POINT('Ctrl Pts',(16.7550758225251,17.5869744152861,-2.47921348002952));
#51290=CARTESIAN_POINT('Ctrl Pts',(16.7017272853287,17.6519812175709,-2.48338304570617));
#51291=CARTESIAN_POINT('Ctrl Pts',(16.6515843143223,17.7196206546924,-2.48755261138281));
#51292=CARTESIAN_POINT('Ctrl Pts',(16.6049048052609,17.789538198987,-2.49172217705945));
#51293=CARTESIAN_POINT('Ctrl Pts',(16.5565840956936,17.8619139677013,-2.49603834010689));
#51294=CARTESIAN_POINT('Ctrl Pts',(16.5119752240704,17.9367305827085,-2.50035450315433));
#51295=CARTESIAN_POINT('Ctrl Pts',(16.4713143087829,18.0135637959534,-2.50467066620176));
#51296=CARTESIAN_POINT('Ctrl Pts',(16.4319779238963,18.087894165226,-2.50884623012272));
#51297=CARTESIAN_POINT('Ctrl Pts',(16.3963363916594,18.1641113217507,-2.51302179404367));
#51298=CARTESIAN_POINT('Ctrl Pts',(16.3645549999772,18.241809414064,-2.51719735796462));
#51299=CARTESIAN_POINT('Ctrl Pts',(16.331168399037,18.3234318687324,-2.5215838205753));
#51300=CARTESIAN_POINT('Ctrl Pts',(16.3020423326827,18.4066882445185,-2.52597028318598));
#51301=CARTESIAN_POINT('Ctrl Pts',(16.2773090396161,18.491090613224,-2.53035674579666));
#51302=CARTESIAN_POINT('Ctrl Pts',(16.2525757465496,18.5754929819294,-2.53474320840733));
#51303=CARTESIAN_POINT('Ctrl Pts',(16.2322352869838,18.6610407614778,-2.53912967101801));
#51304=CARTESIAN_POINT('Ctrl Pts',(16.2163575306379,18.7472367021162,-2.54351613362869));
#51305=CARTESIAN_POINT('Ctrl Pts',(16.1935441105101,18.8710844400618,-2.54981867488401));
#51306=CARTESIAN_POINT('Ctrl Pts',(16.179864182312,18.9966631544576,-2.55612121613934));
#51307=CARTESIAN_POINT('Ctrl Pts',(16.1755170133968,19.1228818562274,-2.56242375739466));
#51308=CARTESIAN_POINT('Ctrl Pts',(16.1745315620438,19.1514941307573,-2.56385246833928));
#51309=CARTESIAN_POINT('Ctrl Pts',(16.1740255308992,19.180139168944,-2.56528117928389));
#51310=CARTESIAN_POINT('Ctrl Pts',(16.1740009418753,19.2088040034395,-2.56670989022851));
#51311=CARTESIAN_POINT('Origin',(18.734,19.211,1.76670989022852));
#51312=CARTESIAN_POINT('',(20.2935358855687,21.2411349269503,-1.25003886315632));
#51313=CARTESIAN_POINT('',(20.2916962525237,21.2387762312159,-1.31677679826697));
#51314=CARTESIAN_POINT('',(20.2935358855687,21.2411349269503,1.76670989022852));
#51315=CARTESIAN_POINT('',(16.1742339456424,19.2099923322427,-1.83329006740172));
#51316=CARTESIAN_POINT('Ctrl Pts',(20.2916962525238,21.2387762312158,-1.31677679826698));
#51317=CARTESIAN_POINT('Ctrl Pts',(20.71974029023,20.9053211442369,-1.34369097138053));
#51318=CARTESIAN_POINT('Ctrl Pts',(21.5659317303477,19.7058144822129,-1.41299708005456));
#51319=CARTESIAN_POINT('Ctrl Pts',(21.0139855967169,17.219779463867,-1.52469512428907));
#51320=CARTESIAN_POINT('Ctrl Pts',(18.2938122975693,16.2160838163956,-1.65187093097051));
#51321=CARTESIAN_POINT('Ctrl Pts',(16.4202753011031,17.6266608733541,-1.75473569408333));
#51322=CARTESIAN_POINT('Ctrl Pts',(16.1765569575323,18.8451666316293,-1.81520852163568));
#51323=CARTESIAN_POINT('Ctrl Pts',(16.1778407186761,19.2099805598359,-1.83328941362754));
#51324=CARTESIAN_POINT('Ctrl Pts',(16.174000198019,19.2099930951884,-1.8332901097715));
#51325=CARTESIAN_POINT('Ctrl Pts',(16.1739663681253,19.2960037291259,-1.83754657623673));
#51326=CARTESIAN_POINT('Ctrl Pts',(16.1782715498352,19.3819895204514,-1.84180304270196));
#51327=CARTESIAN_POINT('Ctrl Pts',(16.1868819594924,19.4674950052547,-1.84605950916719));
#51328=CARTESIAN_POINT('Ctrl Pts',(16.1954973714593,19.5530501653856,-1.85031844847222));
#51329=CARTESIAN_POINT('Ctrl Pts',(16.2084229438551,19.6381240334814,-1.85457738777724));
#51330=CARTESIAN_POINT('Ctrl Pts',(16.2255732751461,19.7222683894382,-1.85883632708227));
#51331=CARTESIAN_POINT('Ctrl Pts',(16.2427520342423,19.8065522202146,-1.86310232586009));
#51332=CARTESIAN_POINT('Ctrl Pts',(16.2641694501953,19.8899030371078,-1.86736832463791));
#51333=CARTESIAN_POINT('Ctrl Pts',(16.2896893999656,19.9718848076808,-1.87163432341573));
#51334=CARTESIAN_POINT('Ctrl Pts',(16.3152317962993,20.0539386868993,-1.87590407443496));
#51335=CARTESIAN_POINT('Ctrl Pts',(16.3448837660451,20.1346207148683,-1.88017382545418));
#51336=CARTESIAN_POINT('Ctrl Pts',(16.378460747601,20.2135142544661,-1.8844435764734));
#51337=CARTESIAN_POINT('Ctrl Pts',(16.4121081360956,20.2925732244374,-1.88872228065292));
#51338=CARTESIAN_POINT('Ctrl Pts',(16.4496967908718,20.3698358236637,-1.89300098483243));
#51339=CARTESIAN_POINT('Ctrl Pts',(16.4909957509127,20.4449092100217,-1.89727968901195));
#51340=CARTESIAN_POINT('Ctrl Pts',(16.5197685295451,20.4972124623244,-1.90026064078576));
#51341=CARTESIAN_POINT('Ctrl Pts',(16.5503412786202,20.5484536572702,-1.90324159255957));
#51342=CARTESIAN_POINT('Ctrl Pts',(16.5826239200438,20.5985089054101,-1.90622254433338));
#51343=CARTESIAN_POINT('Ctrl Pts',(16.6279420233601,20.668776046099,-1.9104071796206));
#51344=CARTESIAN_POINT('Ctrl Pts',(16.6767906254528,20.7369513808156,-1.91459181490782));
#51345=CARTESIAN_POINT('Ctrl Pts',(16.728950354716,20.8026582296292,-1.91877645019504));
#51346=CARTESIAN_POINT('Ctrl Pts',(16.7810358412062,20.8682715530599,-1.92295512918357));
#51347=CARTESIAN_POINT('Ctrl Pts',(16.8364228098493,20.9314230124315,-1.9271338081721));
#51348=CARTESIAN_POINT('Ctrl Pts',(16.8948480567163,20.9917639174006,-1.93131248716063));
#51349=CARTESIAN_POINT('Ctrl Pts',(16.9543205181259,21.0531863731818,-1.93556606482122));
#51350=CARTESIAN_POINT('Ctrl Pts',(17.016940988373,21.1116961215207,-1.93981964248181));
#51351=CARTESIAN_POINT('Ctrl Pts',(17.0823881640281,21.1669596987866,-1.9440732201424));
#51352=CARTESIAN_POINT('Ctrl Pts',(17.1465665360758,21.2211518986326,-1.94824433504389));
#51353=CARTESIAN_POINT('Ctrl Pts',(17.2134626230229,21.2722223587369,-1.95241544994537));
#51354=CARTESIAN_POINT('Ctrl Pts',(17.2827368115688,21.3198942974707,-1.95658656484686));
#51355=CARTESIAN_POINT('Ctrl Pts',(17.3519877545808,21.3675502394864,-1.96075628009582));
#51356=CARTESIAN_POINT('Ctrl Pts',(17.4236148357134,21.4118096644133,-1.96492599534479));
#51357=CARTESIAN_POINT('Ctrl Pts',(17.497247739258,21.4524378968754,-1.96909571059375));
#51358=CARTESIAN_POINT('Ctrl Pts',(17.5708780226959,21.4930646836483,-1.97326527747021));
#51359=CARTESIAN_POINT('Ctrl Pts',(17.6465135834374,21.5300603133606,-1.97743484434667));
#51360=CARTESIAN_POINT('Ctrl Pts',(17.7237588789492,21.5632357189146,-1.98160441122312));
#51361=CARTESIAN_POINT('Ctrl Pts',(17.8037199856914,21.5975775144525,-1.98592057287243));
#51362=CARTESIAN_POINT('Ctrl Pts',(17.8854056436194,21.6278252451695,-1.99023673452174));
#51363=CARTESIAN_POINT('Ctrl Pts',(17.9683557183338,21.6538239465733,-1.99455289617105));
#51364=CARTESIAN_POINT('Ctrl Pts',(18.0486037412681,21.6789757549796,-1.99872846129518));
#51365=CARTESIAN_POINT('Ctrl Pts',(18.1300346026431,21.7001510305579,-2.00290402641931));
#51366=CARTESIAN_POINT('Ctrl Pts',(18.2122191472962,21.7172611080555,-2.00707959154345));
#51367=CARTESIAN_POINT('Ctrl Pts',(18.2985545772993,21.7352353622706,-2.01146605145534));
#51368=CARTESIAN_POINT('Ctrl Pts',(18.3857212504014,21.7487228766122,-2.01585251136724));
#51369=CARTESIAN_POINT('Ctrl Pts',(18.4732153214809,21.7576824206111,-2.02023897127913));
#51370=CARTESIAN_POINT('Ctrl Pts',(18.5607093925604,21.7666419646101,-2.02462543119103));
#51371=CARTESIAN_POINT('Ctrl Pts',(18.6485302783063,21.7710735849926,-2.02901189110292));
#51372=CARTESIAN_POINT('Ctrl Pts',(18.7361763184418,21.7709990749291,-2.03339835101482));
#51373=CARTESIAN_POINT('Ctrl Pts',(18.8197745701698,21.7709280059906,-2.03758222948032));
#51374=CARTESIAN_POINT('Ctrl Pts',(18.903524881571,21.7667575762853,-2.04176610794582));
#51375=CARTESIAN_POINT('Ctrl Pts',(18.9869920193077,21.7584683586193,-2.04594998641132));
#51376=CARTESIAN_POINT('Ctrl Pts',(19.0703479391422,21.7501901861314,-2.05012828996198));
#51377=CARTESIAN_POINT('Ctrl Pts',(19.1534209809432,21.7378041671254,-2.05430659351263));
#51378=CARTESIAN_POINT('Ctrl Pts',(19.2357756009639,21.7213428543283,-2.05848489706328));
#51379=CARTESIAN_POINT('Ctrl Pts',(19.3180452017791,21.7048985354502,-2.06265888712128));
#51380=CARTESIAN_POINT('Ctrl Pts',(19.3995974052585,21.6843873684876,-2.06683287717928));
#51381=CARTESIAN_POINT('Ctrl Pts',(19.4800028447563,21.659893577846,-2.07100686723728));
#51382=CARTESIAN_POINT('Ctrl Pts',(19.5603542148008,21.6354162583024,-2.07517805045333));
#51383=CARTESIAN_POINT('Ctrl Pts',(19.6395599135012,21.6069617675492,-2.07934923366938));
#51384=CARTESIAN_POINT('Ctrl Pts',(19.7172030732739,21.574664890949,-2.08352041688543));
#51385=CARTESIAN_POINT('Ctrl Pts',(19.7948145897919,21.5423811768513,-2.08768990014732));
#51386=CARTESIAN_POINT('Ctrl Pts',(19.8708644093505,21.5062583672899,-2.0918593834092));
#51387=CARTESIAN_POINT('Ctrl Pts',(19.9449544117907,21.4664798630368,-2.09602886667109));
#51388=CARTESIAN_POINT('Ctrl Pts',(20.0190582144985,21.4266939494979,-2.10019912655578));
#51389=CARTESIAN_POINT('Ctrl Pts',(20.0912010629143,21.3832511941884,-2.10436938644046));
#51390=CARTESIAN_POINT('Ctrl Pts',(20.1610091624564,21.3363811070642,-2.10853964632514));
#51391=CARTESIAN_POINT('Ctrl Pts',(20.206193956802,21.306043434766,-2.11123893675839));
#51392=CARTESIAN_POINT('Ctrl Pts',(20.2504011005482,21.2742707763279,-2.11393822719164));
#51393=CARTESIAN_POINT('Ctrl Pts',(20.2935358855687,21.2411349269503,-2.11663751762489));
#51394=CARTESIAN_POINT('',(16.1740004726294,19.2125555906437,-1.76670989019937));
#51395=CARTESIAN_POINT('Ctrl Pts',(16.1740004726297,19.2125555912267,-1.7667098902285));
#51396=CARTESIAN_POINT('Ctrl Pts',(16.1740562220857,19.3043011464569,-1.77129369133236));
#51397=CARTESIAN_POINT('Ctrl Pts',(16.1790436176611,19.3958958077681,-1.77587749243622));
#51398=CARTESIAN_POINT('Ctrl Pts',(16.188916332748,19.4869513121681,-1.78046129354008));
#51399=CARTESIAN_POINT('Ctrl Pts',(16.1979293239672,19.5700776309547,-1.78464593360467));
#51400=CARTESIAN_POINT('Ctrl Pts',(16.2110359189468,19.6529166093026,-1.78883057366926));
#51401=CARTESIAN_POINT('Ctrl Pts',(16.2282088654964,19.7350331957452,-1.79301521373385));
#51402=CARTESIAN_POINT('Ctrl Pts',(16.2453573687607,19.8170329007231,-1.79719389754915));
#51403=CARTESIAN_POINT('Ctrl Pts',(16.2665606336754,19.898311809733,-1.80137258136445));
#51404=CARTESIAN_POINT('Ctrl Pts',(16.2917396796525,19.9784402437038,-1.80555126517975));
#51405=CARTESIAN_POINT('Ctrl Pts',(16.3173699981905,20.0600047830626,-1.80980484163982));
#51406=CARTESIAN_POINT('Ctrl Pts',(16.3471199654275,20.1403767219199,-1.8140584180999));
#51407=CARTESIAN_POINT('Ctrl Pts',(16.3808518403883,20.2191139513548,-1.81831199455997));
#51408=CARTESIAN_POINT('Ctrl Pts',(16.4139298144973,20.2963248398595,-1.82248311437409));
#51409=CARTESIAN_POINT('Ctrl Pts',(16.450836503808,20.3719633895875,-1.82665423418821));
#51410=CARTESIAN_POINT('Ctrl Pts',(16.4913923918018,20.4456299508969,-1.83082535400233));
#51411=CARTESIAN_POINT('Ctrl Pts',(16.5319346711508,20.5192717931798,-1.8349950741852));
#51412=CARTESIAN_POINT('Ctrl Pts',(16.5761234956298,20.5909425585429,-1.83916479436806));
#51413=CARTESIAN_POINT('Ctrl Pts',(16.6237330294819,20.6602664741656,-1.84333451455093));
#51414=CARTESIAN_POINT('Ctrl Pts',(16.671340869397,20.7295879232582,-1.84750408637604));
#51415=CARTESIAN_POINT('Ctrl Pts',(16.7223689155627,20.7965623098985,-1.85167365820116));
#51416=CARTESIAN_POINT('Ctrl Pts',(16.7765483378666,20.8608433229889,-1.85584323002627));
#51417=CARTESIAN_POINT('Ctrl Pts',(16.8326324731959,20.9273841771355,-1.86015938587588));
#51418=CARTESIAN_POINT('Ctrl Pts',(16.8920933523659,20.9910383498724,-1.86447554172548));
#51419=CARTESIAN_POINT('Ctrl Pts',(16.9545891221584,21.0514610639237,-1.86879169757509));
#51420=CARTESIAN_POINT('Ctrl Pts',(17.0150492802823,21.1099156898598,-1.872967267634));
#51421=CARTESIAN_POINT('Ctrl Pts',(17.0783492738879,21.1653458606137,-1.87714283769291));
#51422=CARTESIAN_POINT('Ctrl Pts',(17.1441452212348,21.2174799481773,-1.88131840775181));
#51423=CARTESIAN_POINT('Ctrl Pts',(17.2132640592835,21.2722469619589,-1.88570485649677));
#51424=CARTESIAN_POINT('Ctrl Pts',(17.2851371185139,21.323375865423,-1.89009130524172));
#51425=CARTESIAN_POINT('Ctrl Pts',(17.3593324933327,21.3706039558477,-1.89447775398667));
#51426=CARTESIAN_POINT('Ctrl Pts',(17.4335278681516,21.4178320462725,-1.89886420273162));
#51427=CARTESIAN_POINT('Ctrl Pts',(17.5100450161993,21.4611591039616,-1.90325065147657));
#51428=CARTESIAN_POINT('Ctrl Pts',(17.5884257348941,21.5003797420103,-1.90763710022152));
#51429=CARTESIAN_POINT('Ctrl Pts',(17.6632002791351,21.5377958997562,-1.91182173531038));
#51430=CARTESIAN_POINT('Ctrl Pts',(17.7399490034729,21.5716144630813,-1.91600637039924));
#51431=CARTESIAN_POINT('Ctrl Pts',(17.818291348554,21.6016228614457,-1.9201910054881));
#51432=CARTESIAN_POINT('Ctrl Pts',(17.8965221835546,21.6315885467804,-1.92436968429629));
#51433=CARTESIAN_POINT('Ctrl Pts',(17.9763417077984,21.6577546763325,-1.92854836310447));
#51434=CARTESIAN_POINT('Ctrl Pts',(18.0573458795764,21.679955082887,-1.93272704191266));
#51435=CARTESIAN_POINT('Ctrl Pts',(18.1398019751846,21.7025534109142,-1.93698061962059));
#51436=CARTESIAN_POINT('Ctrl Pts',(18.22348517397,21.7210422324029,-1.94123419732852));
#51437=CARTESIAN_POINT('Ctrl Pts',(18.3079491747639,21.7352980597219,-1.94548777503645));
#51438=CARTESIAN_POINT('Ctrl Pts',(18.3907756952125,21.7492775132387,-1.94965888980362));
#51439=CARTESIAN_POINT('Ctrl Pts',(18.4743525389348,21.759186555656,-1.95383000457078));
#51440=CARTESIAN_POINT('Ctrl Pts',(18.5582464958671,21.7649598089604,-1.95800111933795));
#51441=CARTESIAN_POINT('Ctrl Pts',(18.6421123018319,21.7707311250256,-1.96217083447015));
#51442=CARTESIAN_POINT('Ctrl Pts',(18.7262945511122,21.772369376577,-1.96634054960234));
#51443=CARTESIAN_POINT('Ctrl Pts',(18.8103550385056,21.769861056817,-1.97051026473454));
#51444=CARTESIAN_POINT('Ctrl Pts',(18.8944125351025,21.7673528263009,-1.97467983151203));
#51445=CARTESIAN_POINT('Ctrl Pts',(18.9783478186234,21.7606983323763,-1.97884939828952));
#51446=CARTESIAN_POINT('Ctrl Pts',(19.0617241844592,21.7499361667676,-1.983018965067));
#51447=CARTESIAN_POINT('Ctrl Pts',(19.1480319248283,21.7387956212922,-1.98733512688666));
#51448=CARTESIAN_POINT('Ctrl Pts',(19.2337401905612,21.7232532494629,-1.99165128870633));
#51449=CARTESIAN_POINT('Ctrl Pts',(19.3183740371403,21.7034098749436,-1.99596745052599));
#51450=CARTESIAN_POINT('Ctrl Pts',(19.4002509797481,21.6842128881312,-2.00014301559692));
#51451=CARTESIAN_POINT('Ctrl Pts',(19.481121986091,21.6609909777928,-2.00431858066785));
#51452=CARTESIAN_POINT('Ctrl Pts',(19.5605725242401,21.6338862668667,-2.00849414573879));
#51453=CARTESIAN_POINT('Ctrl Pts',(19.6440358680186,21.6054125792273,-2.01288060593281));
#51454=CARTESIAN_POINT('Ctrl Pts',(19.725930936615,21.572653764432,-2.01726706612684));
#51455=CARTESIAN_POINT('Ctrl Pts',(19.8058030522818,21.5358307932233,-2.02165352632086));
#51456=CARTESIAN_POINT('Ctrl Pts',(19.8856751679486,21.4990078220147,-2.02603998651489));
#51457=CARTESIAN_POINT('Ctrl Pts',(19.9635238523773,21.4581210315221,-2.03042644670891));
#51458=CARTESIAN_POINT('Ctrl Pts',(20.0389283879064,21.4134445287989,-2.03481290690294));
#51459=CARTESIAN_POINT('Ctrl Pts',(20.1108650768746,21.3708226936792,-2.03899763425965));
#51460=CARTESIAN_POINT('Ctrl Pts',(20.1808452608424,21.3245934161189,-2.04318236161637));
#51461=CARTESIAN_POINT('Ctrl Pts',(20.2484841862935,21.2749616395337,-2.04736708897308));
#51462=CARTESIAN_POINT('Ctrl Pts',(20.2636199524707,21.2638553873226,-2.04830351802431));
#51463=CARTESIAN_POINT('Ctrl Pts',(20.2786385693017,21.2525789442955,-2.04923994707554));
#51464=CARTESIAN_POINT('Ctrl Pts',(20.2935358855687,21.2411349269503,-2.05017637612677));
#51465=CARTESIAN_POINT('Ctrl Pts',(20.2935358855687,21.2411349269503,-1.25003886315632));
#51466=CARTESIAN_POINT('Ctrl Pts',(20.3601834809874,21.1899366960531,-1.25422273027566));
#51467=CARTESIAN_POINT('Ctrl Pts',(20.4242257520562,21.1355156975242,-1.258406597395));
#51468=CARTESIAN_POINT('Ctrl Pts',(20.4853525076874,21.0781808679978,-1.26259046451434));
#51469=CARTESIAN_POINT('Ctrl Pts',(20.5299990646909,21.0363039074377,-1.26564633194767));
#51470=CARTESIAN_POINT('Ctrl Pts',(20.5730910160661,20.9928733025549,-1.26870219938101));
#51471=CARTESIAN_POINT('Ctrl Pts',(20.6145211583455,20.948020487218,-1.27175806681434));
#51472=CARTESIAN_POINT('Ctrl Pts',(20.6712532036771,20.8866016309711,-1.27594259528124));
#51473=CARTESIAN_POINT('Ctrl Pts',(20.7250787538107,20.8222861461377,-1.28012712374813));
#51474=CARTESIAN_POINT('Ctrl Pts',(20.7756877958407,20.7553804402786,-1.28431165221502));
#51475=CARTESIAN_POINT('Ctrl Pts',(20.8262247807555,20.6885699947122,-1.2884902227535));
#51476=CARTESIAN_POINT('Ctrl Pts',(20.8735540790342,20.6191770173187,-1.29266879329197));
#51477=CARTESIAN_POINT('Ctrl Pts',(20.9174037187929,20.5475433778076,-1.29684736383044));
#51478=CARTESIAN_POINT('Ctrl Pts',(20.9620407606536,20.4746234226361,-1.30110096839983));
#51479=CARTESIAN_POINT('Ctrl Pts',(21.0030716129383,20.399381892885,-1.30535457296922));
#51480=CARTESIAN_POINT('Ctrl Pts',(21.0402535236503,20.3222131589622,-1.30960817753861));
#51481=CARTESIAN_POINT('Ctrl Pts',(21.0767133936984,20.2465429753506,-1.31377918077288));
#51482=CARTESIAN_POINT('Ctrl Pts',(21.1094722631679,20.1690202013163,-1.31795018400715));
#51483=CARTESIAN_POINT('Ctrl Pts',(21.1383468618206,20.0900427566697,-1.32212118724142));
#51484=CARTESIAN_POINT('Ctrl Pts',(21.1672117644678,20.0110918324171,-1.32629078986506));
#51485=CARTESIAN_POINT('Ctrl Pts',(21.1921948288651,19.9306876393951,-1.3304603924887));
#51486=CARTESIAN_POINT('Ctrl Pts',(21.2131612203808,19.8492473214673,-1.33462999511234));
#51487=CARTESIAN_POINT('Ctrl Pts',(21.2341268617413,19.7678099173871,-1.33879944855205));
#51488=CARTESIAN_POINT('Ctrl Pts',(21.2510760020805,19.6853369078528,-1.34296890199176));
#51489=CARTESIAN_POINT('Ctrl Pts',(21.2639242673564,19.6022584841778,-1.34713835543148));
#51490=CARTESIAN_POINT('Ctrl Pts',(21.2772250225956,19.5162542061506,-1.3514546486035));
#51491=CARTESIAN_POINT('Ctrl Pts',(21.2861305797708,19.4296015962165,-1.35577094177553));
#51492=CARTESIAN_POINT('Ctrl Pts',(21.290605703432,19.342784965678,-1.36008723494755));
#51493=CARTESIAN_POINT('Ctrl Pts',(21.2949348020335,19.2588011962232,-1.36426268576165));
#51494=CARTESIAN_POINT('Ctrl Pts',(21.2951181996998,19.1746644168246,-1.36843813657575));
#51495=CARTESIAN_POINT('Ctrl Pts',(21.2911771388899,19.0908123120325,-1.37261358738984));
#51496=CARTESIAN_POINT('Ctrl Pts',(21.287036673876,19.0027175773967,-1.37700030174083));
#51497=CARTESIAN_POINT('Ctrl Pts',(21.2783434334409,18.9149376655593,-1.38138701609182));
#51498=CARTESIAN_POINT('Ctrl Pts',(21.2651832584911,18.8279708732557,-1.38577373044281));
#51499=CARTESIAN_POINT('Ctrl Pts',(21.2520230835413,18.7410040809521,-1.3901604447938));
#51500=CARTESIAN_POINT('Ctrl Pts',(21.2343961650043,18.6548509616386,-1.39454715914479));
#51501=CARTESIAN_POINT('Ctrl Pts',(21.2124488481584,18.5699919602204,-1.39893387349578));
#51502=CARTESIAN_POINT('Ctrl Pts',(21.1915123905031,18.489041432083,-1.40311854262417));
#51503=CARTESIAN_POINT('Ctrl Pts',(21.1665668243994,18.4089670901725,-1.40730321175256));
#51504=CARTESIAN_POINT('Ctrl Pts',(21.1377020191448,18.3301954795987,-1.41148788088095));
#51505=CARTESIAN_POINT('Ctrl Pts',(21.1088782968446,18.251535983777,-1.41566659401657));
#51506=CARTESIAN_POINT('Ctrl Pts',(21.0761465724026,18.1741759645832,-1.4198453071522));
#51507=CARTESIAN_POINT('Ctrl Pts',(21.0396471231834,18.0985291719078,-1.42402402028782));
#51508=CARTESIAN_POINT('Ctrl Pts',(21.0024938354146,18.0215272686688,-1.42827758944988));
#51509=CARTESIAN_POINT('Ctrl Pts',(20.9614366236921,17.9463010448911,-1.43253115861194));
#51510=CARTESIAN_POINT('Ctrl Pts',(20.9166757000861,17.8732680431963,-1.436784727774));
#51511=CARTESIAN_POINT('Ctrl Pts',(20.8727820900014,17.8016501711454,-1.44095587732199));
#51512=CARTESIAN_POINT('Ctrl Pts',(20.825327269893,17.7321416952153,-1.44512702686999));
#51513=CARTESIAN_POINT('Ctrl Pts',(20.7745466544998,17.6651121157052,-1.44929817641799));
#51514=CARTESIAN_POINT('Ctrl Pts',(20.7237830774839,17.5981050265737,-1.45346792642368));
#51515=CARTESIAN_POINT('Ctrl Pts',(20.6696961989423,17.5335755483831,-1.45763767642937));
#51516=CARTESIAN_POINT('Ctrl Pts',(20.6125638140492,17.4718628586149,-1.46180742643506));
#51517=CARTESIAN_POINT('Ctrl Pts',(20.5554334612232,17.4101523638248,-1.46597702813235));
#51518=CARTESIAN_POINT('Ctrl Pts',(20.4952581305601,17.3512587952533,-1.47014662982965));
#51519=CARTESIAN_POINT('Ctrl Pts',(20.4323539003177,17.2954859621303,-1.47431623152694));
#51520=CARTESIAN_POINT('Ctrl Pts',(20.3672392271932,17.2377532820859,-1.47863235224779));
#51521=CARTESIAN_POINT('Ctrl Pts',(20.2992006896764,17.1833650979518,-1.48294847296865));
#51522=CARTESIAN_POINT('Ctrl Pts',(20.2286263825151,17.1326131311303,-1.48726459368951));
#51523=CARTESIAN_POINT('Ctrl Pts',(20.1603497799314,17.0835135082167,-1.49144019343698));
#51524=CARTESIAN_POINT('Ctrl Pts',(20.0897004104967,17.0378171816056,-1.49561579318445));
#51525=CARTESIAN_POINT('Ctrl Pts',(20.0170578177754,16.9957432121207,-1.49979139293192));
#51526=CARTESIAN_POINT('Ctrl Pts',(19.9407482759489,16.9515453770223,-1.50417777413947));
#51527=CARTESIAN_POINT('Ctrl Pts',(19.8622395019827,16.9113454968475,-1.50856415534702));
#51528=CARTESIAN_POINT('Ctrl Pts',(19.7819968173662,16.8753410628282,-1.51295053655457));
#51529=CARTESIAN_POINT('Ctrl Pts',(19.7017541327497,16.8393366288089,-1.51733691776211));
#51530=CARTESIAN_POINT('Ctrl Pts',(19.6197781058327,16.8075277799099,-1.52172329896966));
#51531=CARTESIAN_POINT('Ctrl Pts',(19.5365517913736,16.7800514974268,-1.52610968017721));
#51532=CARTESIAN_POINT('Ctrl Pts',(19.4571532093841,16.7538389001049,-1.53029432358246));
#51533=CARTESIAN_POINT('Ctrl Pts',(19.3763213117682,16.7314715386277,-1.53447896698771));
#51534=CARTESIAN_POINT('Ctrl Pts',(19.2944633944869,16.713104729289,-1.53866361039296));
#51535=CARTESIAN_POINT('Ctrl Pts',(19.2127219865111,16.6947640616392,-1.54284229774762));
#51536=CARTESIAN_POINT('Ctrl Pts',(19.1299579046074,16.6804127358414,-1.54702098510227));
#51537=CARTESIAN_POINT('Ctrl Pts',(19.0465949713152,16.6701567573129,-1.55119967245693));
#51538=CARTESIAN_POINT('Ctrl Pts',(18.9617380512092,16.6597169765107,-1.555453248057));
#51539=CARTESIAN_POINT('Ctrl Pts',(18.8762610609814,16.6535209330019,-1.55970682365707));
#51540=CARTESIAN_POINT('Ctrl Pts',(18.7906234644726,16.6516262908143,-1.56396039925714));
#51541=CARTESIAN_POINT('Ctrl Pts',(18.7066458766308,16.6497683745809,-1.5681315230761));
#51542=CARTESIAN_POINT('Ctrl Pts',(18.622514334468,16.6520466005142,-1.57230264689506));
#51543=CARTESIAN_POINT('Ctrl Pts',(18.5386669502935,16.6584630267727,-1.57647377071402));
#51544=CARTESIAN_POINT('Ctrl Pts',(18.4548476979935,16.6648773002377,-1.58064349506736));
#51545=CARTESIAN_POINT('Ctrl Pts',(18.3713128726456,16.6754269815325,-1.5848132194207));
#51546=CARTESIAN_POINT('Ctrl Pts',(18.2884980297119,16.6900620804015,-1.58898294377403));
#51547=CARTESIAN_POINT('Ctrl Pts',(18.2056861301165,16.7046966591217,-1.5931525199304));
#51548=CARTESIAN_POINT('Ctrl Pts',(18.1235946149204,16.7234162858241,-1.59732209608677));
#51549=CARTESIAN_POINT('Ctrl Pts',(18.0426500224206,16.7461196360673,-1.60149167224313));
#51550=CARTESIAN_POINT('Ctrl Pts',(17.9588599467863,16.7696210878046,-1.60580782346109));
#51551=CARTESIAN_POINT('Ctrl Pts',(17.8762994412694,16.7973914245208,-1.61012397467905));
#51552=CARTESIAN_POINT('Ctrl Pts',(17.7954238786636,16.8292622175275,-1.61444012589701));
#51553=CARTESIAN_POINT('Ctrl Pts',(17.7171824223145,16.8600949830688,-1.6186157006471));
#51554=CARTESIAN_POINT('Ctrl Pts',(17.6405182467689,16.8947649654851,-1.62279127539719));
#51555=CARTESIAN_POINT('Ctrl Pts',(17.5658209824087,16.9330716027804,-1.62696685014728));
#51556=CARTESIAN_POINT('Ctrl Pts',(17.4873515388115,16.9733127085343,-1.63135328959917));
#51557=CARTESIAN_POINT('Ctrl Pts',(17.4110533973333,17.0175671442341,-1.63573972905107));
#51558=CARTESIAN_POINT('Ctrl Pts',(17.3373445043261,17.0655505304473,-1.64012616850296));
#51559=CARTESIAN_POINT('Ctrl Pts',(17.2636356113189,17.1135339166605,-1.64451260795486));
#51560=CARTESIAN_POINT('Ctrl Pts',(17.1925163913081,17.1652458506637,-1.64889904740675));
#51561=CARTESIAN_POINT('Ctrl Pts',(17.1243635063082,17.2203542861233,-1.65328548685865));
#51562=CARTESIAN_POINT('Ctrl Pts',(17.0601943716838,17.27224146029,-1.65741552513525));
#51563=CARTESIAN_POINT('Ctrl Pts',(16.9984022161797,17.3273436089106,-1.66154556341186));
#51564=CARTESIAN_POINT('Ctrl Pts',(16.9393333495131,17.3854119814071,-1.66567560168847));
#51565=CARTESIAN_POINT('Ctrl Pts',(16.8791242534032,17.4446012704164,-1.66988536370976));
#51566=CARTESIAN_POINT('Ctrl Pts',(16.8217451257373,17.5068722664466,-1.67409512573104));
#51567=CARTESIAN_POINT('Ctrl Pts',(16.7675298311078,17.5719163917429,-1.67830488775233));
#51568=CARTESIAN_POINT('Ctrl Pts',(16.7144792339723,17.6355631857096,-1.6824242122078));
#51569=CARTESIAN_POINT('Ctrl Pts',(16.6644582224381,17.701864774228,-1.68654353666328));
#51570=CARTESIAN_POINT('Ctrl Pts',(16.6177431433907,17.7704942149182,-1.69066286111875));
#51571=CARTESIAN_POINT('Ctrl Pts',(16.5710563616802,17.8390820837981,-1.69477969032184));
#51572=CARTESIAN_POINT('Ctrl Pts',(16.5276718045391,17.9099946168291,-1.69889651952493));
#51573=CARTESIAN_POINT('Ctrl Pts',(16.4878244173549,17.9828732752973,-1.70301334872802));
#51574=CARTESIAN_POINT('Ctrl Pts',(16.4479884744815,18.0557310027567,-1.70712899556318));
#51575=CARTESIAN_POINT('Ctrl Pts',(16.4116879110196,18.1305533194009,-1.71124464239834));
#51576=CARTESIAN_POINT('Ctrl Pts',(16.3791125474012,18.206955635645,-1.7153602892335));
#51577=CARTESIAN_POINT('Ctrl Pts',(16.3452431867613,18.2863928948241,-1.71963942264732));
#51578=CARTESIAN_POINT('Ctrl Pts',(16.3154014151592,18.367537815818,-1.72391855606114));
#51579=CARTESIAN_POINT('Ctrl Pts',(16.2897454150196,18.4499352696373,-1.72819768947497));
#51580=CARTESIAN_POINT('Ctrl Pts',(16.265047031356,18.529257218353,-1.73231710318821));
#51581=CARTESIAN_POINT('Ctrl Pts',(16.2442275674438,18.6097393677812,-1.73643651690145));
#51582=CARTESIAN_POINT('Ctrl Pts',(16.2273766224859,18.690962267427,-1.74055593061469));
#51583=CARTESIAN_POINT('Ctrl Pts',(16.2105163819041,18.7722299727216,-1.74467761675363));
#51584=CARTESIAN_POINT('Ctrl Pts',(16.1976290874525,18.8542387741595,-1.74879930289257));
#51585=CARTESIAN_POINT('Ctrl Pts',(16.1887526583662,18.9365624480759,-1.75292098903151));
#51586=CARTESIAN_POINT('Ctrl Pts',(16.1798641545679,19.018998107865,-1.75704828194913));
#51587=CARTESIAN_POINT('Ctrl Pts',(16.1749974202386,19.1017490235124,-1.76117557486675));
#51588=CARTESIAN_POINT('Ctrl Pts',(16.1741383212113,19.1843882456639,-1.76530286778437));
#51589=CARTESIAN_POINT('Ctrl Pts',(16.1740406969644,19.1937790045501,-1.76577187525603));
#51590=CARTESIAN_POINT('Ctrl Pts',(16.173994768433,19.2031683266851,-1.7662408827277));
#51591=CARTESIAN_POINT('Ctrl Pts',(16.1740004726294,19.2125555906437,-1.76670989019937));
#51592=CARTESIAN_POINT('Origin',(18.734,19.211,1.76670989022852));
#51593=CARTESIAN_POINT('',(20.2910039445873,21.2378222631174,-0.450077510930245));
#51594=CARTESIAN_POINT('',(20.2957383200499,21.2439676837843,-0.516748669299169));
#51595=CARTESIAN_POINT('',(20.2935358855687,21.2411349269503,1.76670989022852));
#51596=CARTESIAN_POINT('',(16.1765334933267,19.2078568329122,-0.166709890228504));
#51597=CARTESIAN_POINT('Ctrl Pts',(16.1765334933267,19.2078568329122,-0.166709890228504));
#51598=CARTESIAN_POINT('Ctrl Pts',(16.1810511662408,19.7963216342631,-0.195923797939959));
#51599=CARTESIAN_POINT('Ctrl Pts',(16.6739009423912,21.2477390833877,-0.267529641211891));
#51600=CARTESIAN_POINT('Ctrl Pts',(18.6725570476074,22.0506151623629,-0.361985514779138));
#51601=CARTESIAN_POINT('Ctrl Pts',(19.9247548523317,21.5178475229395,-0.427227480634931));
#51602=CARTESIAN_POINT('Ctrl Pts',(20.2910039445873,21.2378222631174,-0.450077510930245));
#51603=CARTESIAN_POINT('',(18.0722627314315,16.7380050975816,0.));
#51604=CARTESIAN_POINT('Ctrl Pts',(18.0722627314315,16.7380050975816,1.38777878078145E-15));
#51605=CARTESIAN_POINT('Ctrl Pts',(17.2488902483963,16.9583275322964,-0.0423919355604767));
#51606=CARTESIAN_POINT('Ctrl Pts',(16.3345567825823,17.8262089039162,-0.0979618989699788));
#51607=CARTESIAN_POINT('Ctrl Pts',(16.1744956276614,18.942407731855,-0.153531862379481));
#51608=CARTESIAN_POINT('Ctrl Pts',(16.1765334933267,19.2078568329122,-0.166709890228504));
#51609=CARTESIAN_POINT('',(19.395767528315,16.7380131948456,-1.73172587381032E-11));
#51610=CARTESIAN_POINT('Origin',(18.734,19.211,0.));
#51611=CARTESIAN_POINT('',(16.1740007446525,19.2129525932361,-0.233290109771496));
#51612=CARTESIAN_POINT('Ctrl Pts',(19.395767528315,16.7380131948456,-1.73172587381032E-11));
#51613=CARTESIAN_POINT('Ctrl Pts',(19.3150528289901,16.7164140633987,-0.0041815967549353));
#51614=CARTESIAN_POINT('Ctrl Pts',(19.2331283959629,16.6987302550736,-0.00836319349255328));
#51615=CARTESIAN_POINT('Ctrl Pts',(19.1504091887632,16.685093551314,-0.0125447902301714));
#51616=CARTESIAN_POINT('Ctrl Pts',(19.0678077744006,16.6714762663337,-0.0167204323393492));
#51617=CARTESIAN_POINT('Ctrl Pts',(18.9844142845817,16.6618947132319,-0.0208960744485263));
#51618=CARTESIAN_POINT('Ctrl Pts',(18.9006573782918,16.6564305023623,-0.0250717165577041));
#51619=CARTESIAN_POINT('Ctrl Pts',(18.8165042143108,16.6509404400653,-0.0292671138175207));
#51620=CARTESIAN_POINT('Ctrl Pts',(18.7319846403618,16.6496069070114,-0.0334625110773381));
#51621=CARTESIAN_POINT('Ctrl Pts',(18.6475423744123,16.6524603620468,-0.0376579083371547));
#51622=CARTESIAN_POINT('Ctrl Pts',(18.5636493738553,16.6552952564233,-0.0418260161051873));
#51623=CARTESIAN_POINT('Ctrl Pts',(18.4798331446954,16.6622628172183,-0.0459941238732202));
#51624=CARTESIAN_POINT('Ctrl Pts',(18.3965307038144,16.6733407490106,-0.0501622316412529));
#51625=CARTESIAN_POINT('Ctrl Pts',(18.3132563453466,16.6844149462778,-0.0543289342820943));
#51626=CARTESIAN_POINT('Ctrl Pts',(18.2304958875343,16.6995967018794,-0.0584956369229356));
#51627=CARTESIAN_POINT('Ctrl Pts',(18.1486808927462,16.718811896609,-0.0626623395637771));
#51628=CARTESIAN_POINT('Ctrl Pts',(18.0668688404716,16.7380264002553,-0.0668288923472635));
#51629=CARTESIAN_POINT('Ctrl Pts',(17.9860026319441,16.7612739482847,-0.0709954451307501));
#51630=CARTESIAN_POINT('Ctrl Pts',(17.9065019549449,16.7884296737907,-0.0751619979142366));
#51631=CARTESIAN_POINT('Ctrl Pts',(17.8260462587421,16.8159116133658,-0.0793786023208257));
#51632=CARTESIAN_POINT('Ctrl Pts',(17.7469895837595,16.8473961156675,-0.0835952067274143));
#51633=CARTESIAN_POINT('Ctrl Pts',(17.6697476948766,16.8827029761992,-0.0878118111340034));
#51634=CARTESIAN_POINT('Ctrl Pts',(17.5933154552392,16.9176397503257,-0.0919842171059645));
#51635=CARTESIAN_POINT('Ctrl Pts',(17.5186605203447,16.9563188567597,-0.0961566230779257));
#51636=CARTESIAN_POINT('Ctrl Pts',(17.4461607527195,16.9985194750769,-0.100329029049887));
#51637=CARTESIAN_POINT('Ctrl Pts',(17.3725089964354,17.041390642215,-0.10456773267379));
#51638=CARTESIAN_POINT('Ctrl Pts',(17.3010819091514,17.0878959373098,-0.108806436297694));
#51639=CARTESIAN_POINT('Ctrl Pts',(17.2322432877688,17.1377593537487,-0.113045139921597));
#51640=CARTESIAN_POINT('Ctrl Pts',(17.1634046663863,17.1876227701875,-0.1172838435455));
#51641=CARTESIAN_POINT('Ctrl Pts',(17.0971548535428,17.2408439496524,-0.121522547169403));
#51642=CARTESIAN_POINT('Ctrl Pts',(17.0338195264424,17.2971070151826,-0.125761250793306));
#51643=CARTESIAN_POINT('Ctrl Pts',(16.9721381147478,17.3519008477408,-0.129889266471862));
#51644=CARTESIAN_POINT('Ctrl Pts',(16.9129812130569,17.4097927309776,-0.134017282150418));
#51645=CARTESIAN_POINT('Ctrl Pts',(16.8566825236081,17.4705175689386,-0.138145297828974));
#51646=CARTESIAN_POINT('Ctrl Pts',(16.8004749046566,17.5311441765279,-0.142266635901988));
#51647=CARTESIAN_POINT('Ctrl Pts',(16.7471166302611,17.5945942890769,-0.146387973975001));
#51648=CARTESIAN_POINT('Ctrl Pts',(16.6969071786038,17.6605636623788,-0.150509312048014));
#51649=CARTESIAN_POINT('Ctrl Pts',(16.6467433533799,17.7264730878598,-0.154626904970446));
#51650=CARTESIAN_POINT('Ctrl Pts',(16.5997229600923,17.7948968581842,-0.158744497892878));
#51651=CARTESIAN_POINT('Ctrl Pts',(16.5561068210809,17.8654958932736,-0.16286209081531));
#51652=CARTESIAN_POINT('Ctrl Pts',(16.5125163943093,17.9360533093806,-0.16697725636706));
#51653=CARTESIAN_POINT('Ctrl Pts',(16.4723264875143,18.0087830434683,-0.171092421918811));
#51654=CARTESIAN_POINT('Ctrl Pts',(16.4357550862559,18.0833163934643,-0.175207587470561));
#51655=CARTESIAN_POINT('Ctrl Pts',(16.3991935732988,18.1578295908767,-0.179321640349689));
#51656=CARTESIAN_POINT('Ctrl Pts',(16.3662488306646,18.2341450104433,-0.183435693228817));
#51657=CARTESIAN_POINT('Ctrl Pts',(16.3370925482536,18.3118700495687,-0.187549746107944));
#51658=CARTESIAN_POINT('Ctrl Pts',(16.3079200305285,18.3896383689178,-0.191666089846375));
#51659=CARTESIAN_POINT('Ctrl Pts',(16.2825403575632,18.4688174331029,-0.195782433584806));
#51660=CARTESIAN_POINT('Ctrl Pts',(16.2610764229501,18.5489962371172,-0.199898777323237));
#51661=CARTESIAN_POINT('Ctrl Pts',(16.239606571517,18.6291971434892,-0.204016255786767));
#51662=CARTESIAN_POINT('Ctrl Pts',(16.2220547120702,18.7103978759457,-0.208133734250297));
#51663=CARTESIAN_POINT('Ctrl Pts',(16.2084928021298,18.7921761784404,-0.212251212713827));
#51664=CARTESIAN_POINT('Ctrl Pts',(16.1949128183452,18.874063466196,-0.21637417850653));
#51665=CARTESIAN_POINT('Ctrl Pts',(16.1853334600005,18.9565293904166,-0.220497144299234));
#51666=CARTESIAN_POINT('Ctrl Pts',(16.1797748247972,19.0391461249782,-0.224620110091938));
#51667=CARTESIAN_POINT('Ctrl Pts',(16.1758784899859,19.0970564657531,-0.227510109985124));
#51668=CARTESIAN_POINT('Ctrl Pts',(16.1739565734894,19.1550408159346,-0.230400109878309));
#51669=CARTESIAN_POINT('Ctrl Pts',(16.1740007446525,19.2129525932361,-0.233290109771496));
#51670=CARTESIAN_POINT('Ctrl Pts',(16.1719919784605,19.2129541253863,-0.233290109771496));
#51671=CARTESIAN_POINT('Ctrl Pts',(16.1708576353774,19.3442909950989,-0.239839092339242));
#51672=CARTESIAN_POINT('Ctrl Pts',(16.2398215309513,20.3246257991586,-0.288780010467465));
#51673=CARTESIAN_POINT('Ctrl Pts',(17.5061738855977,21.978179087,-0.380112864156167));
#51674=CARTESIAN_POINT('Ctrl Pts',(19.5043144350046,21.8141354816799,-0.468050068097647));
#51675=CARTESIAN_POINT('Ctrl Pts',(20.2458873728542,21.2827381199421,-0.513595336478648));
#51676=CARTESIAN_POINT('Ctrl Pts',(20.2957383200499,21.2439676837843,-0.516748669299169));
#51677=CARTESIAN_POINT('Origin',(18.734,-18.952,1.76670989022851));
#51678=CARTESIAN_POINT('',(20.2955778924961,-16.9192440454753,-21.2501821980133));
#51679=CARTESIAN_POINT('',(20.2916907304467,-16.9243022127158,-21.3166133950378));
#51680=CARTESIAN_POINT('',(20.293535888361,-16.9218650751948,1.76670989022851));
#51681=CARTESIAN_POINT('',(16.1765333501007,-18.9488555363839,-21.8332901097715));
#51682=CARTESIAN_POINT('Ctrl Pts',(20.2916907304466,-16.9243022127157,-21.3166133950378));
#51683=CARTESIAN_POINT('Ctrl Pts',(20.5461545344098,-17.1171758877203,-21.3324492522228));
#51684=CARTESIAN_POINT('Ctrl Pts',(21.3518775433702,-17.9919927123694,-21.3906770449683));
#51685=CARTESIAN_POINT('Ctrl Pts',(21.4520480948179,-20.2843429650063,-21.4912967732743));
#51686=CARTESIAN_POINT('Ctrl Pts',(19.0860574215255,-21.9577201113934,-21.6184725799557));
#51687=CARTESIAN_POINT('Ctrl Pts',(16.6739013977444,-20.9887406839414,-21.7324703587881));
#51688=CARTESIAN_POINT('Ctrl Pts',(16.1810511496244,-19.5373209132916,-21.80407620206));
#51689=CARTESIAN_POINT('Ctrl Pts',(16.1765333501007,-18.9488555363839,-21.8332901097715));
#51690=CARTESIAN_POINT('',(18.0722627314314,-16.4790050975816,-22.));
#51691=CARTESIAN_POINT('Ctrl Pts',(16.1765333501007,-18.9488555363839,-21.8332901097715));
#51692=CARTESIAN_POINT('Ctrl Pts',(16.1744954273233,-18.6834061757001,-21.8464681376205));
#51693=CARTESIAN_POINT('Ctrl Pts',(16.3345563979949,-17.5672065717878,-21.90203810103));
#51694=CARTESIAN_POINT('Ctrl Pts',(17.2488902483963,-16.6993275322964,-21.9576080644395));
#51695=CARTESIAN_POINT('Ctrl Pts',(18.0722627314314,-16.4790050975816,-22.));
#51696=CARTESIAN_POINT('',(19.3957679668415,-16.4790133121946,-21.9999999999819));
#51697=CARTESIAN_POINT('Origin',(18.734,-18.952,-22.));
#51698=CARTESIAN_POINT('',(16.1740007447319,-18.9539526972956,-21.7667098902285));
#51699=CARTESIAN_POINT('Ctrl Pts',(16.1740007447319,-18.9539526972956,-21.7667098902285));
#51700=CARTESIAN_POINT('Ctrl Pts',(16.1739377135638,-18.8713184130896,-21.770833628584));
#51701=CARTESIAN_POINT('Ctrl Pts',(16.1778799218946,-18.788536175973,-21.7749573669396));
#51702=CARTESIAN_POINT('Ctrl Pts',(16.1858438033836,-18.7060325272615,-21.7790811052951));
#51703=CARTESIAN_POINT('Ctrl Pts',(16.1937978807278,-18.6236304468261,-21.7831997670146));
#51704=CARTESIAN_POINT('Ctrl Pts',(16.2057637513171,-18.5415067419993,-21.787318428734));
#51705=CARTESIAN_POINT('Ctrl Pts',(16.2217058130157,-18.4600874894405,-21.7914370904535));
#51706=CARTESIAN_POINT('Ctrl Pts',(16.2376371830466,-18.3787228413373,-21.7955529899605));
#51707=CARTESIAN_POINT('Ctrl Pts',(16.2575393635618,-18.2980621716067,-21.7996688894674));
#51708=CARTESIAN_POINT('Ctrl Pts',(16.2813251279379,-18.2185247298273,-21.8037847889744));
#51709=CARTESIAN_POINT('Ctrl Pts',(16.3051025309066,-18.1390152478366,-21.8078992416196));
#51710=CARTESIAN_POINT('Ctrl Pts',(16.3327606725193,-18.060628663487,-21.8120136942648));
#51711=CARTESIAN_POINT('Ctrl Pts',(16.3641619710533,-17.9837708346893,-21.81612814691));
#51712=CARTESIAN_POINT('Ctrl Pts',(16.3955622513427,-17.9069154981478,-21.8202424661365));
#51713=CARTESIAN_POINT('Ctrl Pts',(16.4307052665747,-17.8315892564416,-21.824356785363));
#51714=CARTESIAN_POINT('Ctrl Pts',(16.4694052036476,-17.7581782342687,-21.8284711045895));
#51715=CARTESIAN_POINT('Ctrl Pts',(16.5081407912399,-17.6846995856017,-21.8325892139415));
#51716=CARTESIAN_POINT('Ctrl Pts',(16.5504396217143,-17.6131400990191,-21.8367073232935));
#51717=CARTESIAN_POINT('Ctrl Pts',(16.5960701372503,-17.543860837146,-21.8408254326455));
#51718=CARTESIAN_POINT('Ctrl Pts',(16.6417225438979,-17.4745483387418,-21.8449455176489));
#51719=CARTESIAN_POINT('Ctrl Pts',(16.6907095365088,-17.407518624288,-21.8490656026523));
#51720=CARTESIAN_POINT('Ctrl Pts',(16.7427579736743,-17.343101248495,-21.8531856876557));
#51721=CARTESIAN_POINT('Ctrl Pts',(16.794892440757,-17.2785773983907,-21.8573125826728));
#51722=CARTESIAN_POINT('Ctrl Pts',(16.8500981395581,-17.2166748608617,-21.8614394776899));
#51723=CARTESIAN_POINT('Ctrl Pts',(16.9080639839603,-17.1576874114779,-21.865566372707));
#51724=CARTESIAN_POINT('Ctrl Pts',(16.9486676843771,-17.1163681009799,-21.8684571648736));
#51725=CARTESIAN_POINT('Ctrl Pts',(16.9906249225133,-17.0764783454379,-21.8713479570401));
#51726=CARTESIAN_POINT('Ctrl Pts',(17.0338195571032,-17.0381069879455,-21.8742387492067));
#51727=CARTESIAN_POINT('Ctrl Pts',(17.0962945700832,-16.9826081724059,-21.8784198767899));
#51728=CARTESIAN_POINT('Ctrl Pts',(17.1616053466634,-16.9300690778322,-21.8826010043731));
#51729=CARTESIAN_POINT('Ctrl Pts',(17.2294395634032,-16.8807931313779,-21.8867821319562));
#51730=CARTESIAN_POINT('Ctrl Pts',(17.2971787572344,-16.8315862112052,-21.8909574025704));
#51731=CARTESIAN_POINT('Ctrl Pts',(17.3674340003121,-16.7856336283223,-21.8951326731846));
#51732=CARTESIAN_POINT('Ctrl Pts',(17.4398582963668,-16.7432000428021,-21.8993079437988));
#51733=CARTESIAN_POINT('Ctrl Pts',(17.5126335322061,-16.7005608407393,-21.9035034461398));
#51734=CARTESIAN_POINT('Ctrl Pts',(17.5875985480893,-16.6614751468356,-21.9076989484807));
#51735=CARTESIAN_POINT('Ctrl Pts',(17.6643699161775,-16.6261686467455,-21.9118944508217));
#51736=CARTESIAN_POINT('Ctrl Pts',(17.7406375998075,-16.5910937868593,-21.9160624271542));
#51737=CARTESIAN_POINT('Ctrl Pts',(17.8186875806148,-16.5597488751243,-21.9202304034868));
#51738=CARTESIAN_POINT('Ctrl Pts',(17.8981189457525,-16.5323093455671,-21.9243983798194));
#51739=CARTESIAN_POINT('Ctrl Pts',(17.9775252548951,-16.5048784715922,-21.9285650413968));
#51740=CARTESIAN_POINT('Ctrl Pts',(18.0583116477557,-16.4813506834989,-21.9327317029742));
#51741=CARTESIAN_POINT('Ctrl Pts',(18.140058939298,-16.4618526115083,-21.9368983645517));
#51742=CARTESIAN_POINT('Ctrl Pts',(18.221805062827,-16.442354818108,-21.9410649665954));
#51743=CARTESIAN_POINT('Ctrl Pts',(18.3045116092593,-16.4268867321271,-21.9452315686392));
#51744=CARTESIAN_POINT('Ctrl Pts',(18.3877473464946,-16.4155242757045,-21.949398170683));
#51745=CARTESIAN_POINT('Ctrl Pts',(18.4719862643407,-16.4040248757484,-21.9536149897912));
#51746=CARTESIAN_POINT('Ctrl Pts',(18.5567667383604,-16.3967308160666,-21.9578318088995));
#51747=CARTESIAN_POINT('Ctrl Pts',(18.6416363028402,-16.3936667637997,-21.9620486280077));
#51748=CARTESIAN_POINT('Ctrl Pts',(18.7256174343068,-16.3906347866968,-21.9662213045387));
#51749=CARTESIAN_POINT('Ctrl Pts',(18.8096853344826,-16.3917446006535,-21.9703939810697));
#51750=CARTESIAN_POINT('Ctrl Pts',(18.8934033137616,-16.3969675963773,-21.9745666576007));
#51751=CARTESIAN_POINT('Ctrl Pts',(18.9784497667458,-16.4022734728939,-21.9788055479976));
#51752=CARTESIAN_POINT('Ctrl Pts',(19.0631346044502,-16.4118241506696,-21.9830444383944));
#51753=CARTESIAN_POINT('Ctrl Pts',(19.1470091266727,-16.4255353829343,-21.9872833287913));
#51754=CARTESIAN_POINT('Ctrl Pts',(19.2308836488952,-16.439246615199,-21.9915222191882));
#51755=CARTESIAN_POINT('Ctrl Pts',(19.3139473893182,-16.4571182338667,-21.9957611095851));
#51756=CARTESIAN_POINT('Ctrl Pts',(19.3957679668415,-16.4790133121946,-21.9999999999819));
#51757=CARTESIAN_POINT('Ctrl Pts',(20.2955778924961,-16.9192440454753,-21.2501821980133));
#51758=CARTESIAN_POINT('Ctrl Pts',(20.9031379978352,-17.3928060279424,-21.2886333061692));
#51759=CARTESIAN_POINT('Ctrl Pts',(21.7186680704123,-19.0034153201252,-21.3694763498856));
#51760=CARTESIAN_POINT('Ctrl Pts',(20.3959081902549,-21.4819377002129,-21.4927113291624));
#51761=CARTESIAN_POINT('Ctrl Pts',(17.5061736134544,-21.7191789276414,-21.6198871358439));
#51762=CARTESIAN_POINT('Ctrl Pts',(16.2398215663958,-20.0656261776283,-21.7112199895325));
#51763=CARTESIAN_POINT('Ctrl Pts',(16.1708575232621,-19.0852911366623,-21.7601609076608));
#51764=CARTESIAN_POINT('Ctrl Pts',(16.1719918438157,-18.9539542296302,-21.7667098902285));
#51765=CARTESIAN_POINT('Origin',(18.734,-18.952,1.76670989022851));
#51766=CARTESIAN_POINT('',(20.2940725979672,-16.9211546778498,-20.4499991793503));
#51767=CARTESIAN_POINT('',(20.293535888361,-16.9218650751948,-20.5167505018104));
#51768=CARTESIAN_POINT('',(20.293535888361,-16.9218650751948,1.76670989022851));
#51769=CARTESIAN_POINT('',(16.1740711621187,-18.953341697584,-21.0332900817674));
#51770=CARTESIAN_POINT('Ctrl Pts',(20.293535888361,-16.9218650751948,-20.5167505018104));
#51771=CARTESIAN_POINT('Ctrl Pts',(20.3601729838807,-16.9730552402864,-20.5209209411032));
#51772=CARTESIAN_POINT('Ctrl Pts',(20.4243268584381,-17.0275603845044,-20.525091380396));
#51773=CARTESIAN_POINT('Ctrl Pts',(20.4856569049576,-17.0851046929958,-20.5292618196889));
#51774=CARTESIAN_POINT('Ctrl Pts',(20.5469737360019,-17.1426366017675,-20.5334313603302));
#51775=CARTESIAN_POINT('Ctrl Pts',(20.6054676124936,-17.2032060591384,-20.5376009009716));
#51776=CARTESIAN_POINT('Ctrl Pts',(20.660832945591,-17.2664986503164,-20.5417704416129));
#51777=CARTESIAN_POINT('Ctrl Pts',(20.7162029558448,-17.3297965883304,-20.545940334489));
#51778=CARTESIAN_POINT('Ctrl Pts',(20.7684435960241,-17.3958177698225,-20.5501102273651));
#51779=CARTESIAN_POINT('Ctrl Pts',(20.8172888275803,-17.4642138389946,-20.5542801202412));
#51780=CARTESIAN_POINT('Ctrl Pts',(20.8661854276987,-17.5326818375574,-20.5584543984257));
#51781=CARTESIAN_POINT('Ctrl Pts',(20.9116792213078,-17.6035293356889,-20.5626286766101));
#51782=CARTESIAN_POINT('Ctrl Pts',(20.9535471879616,-17.6763784728957,-20.5668029547945));
#51783=CARTESIAN_POINT('Ctrl Pts',(20.9954381188789,-17.7492675673043,-20.5709795225391));
#51784=CARTESIAN_POINT('Ctrl Pts',(21.0336990535097,-17.8241600770645,-20.5751560902836));
#51785=CARTESIAN_POINT('Ctrl Pts',(21.0681538146031,-17.9006551613416,-20.5793326580281));
#51786=CARTESIAN_POINT('Ctrl Pts',(21.102668197055,-17.9772826145772,-20.5835164530072));
#51787=CARTESIAN_POINT('Ctrl Pts',(21.1333630832728,-18.0555177524356,-20.5877002479864));
#51788=CARTESIAN_POINT('Ctrl Pts',(21.1601112339645,-18.1349416909233,-20.5918840429655));
#51789=CARTESIAN_POINT('Ctrl Pts',(21.1796790948325,-18.1930450191058,-20.5949447374784));
#51790=CARTESIAN_POINT('Ctrl Pts',(21.1971357843348,-18.251784208033,-20.5980054319913));
#51791=CARTESIAN_POINT('Ctrl Pts',(21.2124488472332,-18.310991956643,-20.6010661265042));
#51792=CARTESIAN_POINT('Ctrl Pts',(21.2333845648802,-18.3919396230659,-20.6052506476905));
#51793=CARTESIAN_POINT('Ctrl Pts',(21.2503893834069,-18.4740647142243,-20.6094351688768));
#51794=CARTESIAN_POINT('Ctrl Pts',(21.26333508953,-18.556950629829,-20.6136196900631));
#51795=CARTESIAN_POINT('Ctrl Pts',(21.2762623681317,-18.6397185617596,-20.617798254807));
#51796=CARTESIAN_POINT('Ctrl Pts',(21.2851419407115,-18.7232447163151,-20.6219768195509));
#51797=CARTESIAN_POINT('Ctrl Pts',(21.2898958840996,-18.8070992420912,-20.6261553842948));
#51798=CARTESIAN_POINT('Ctrl Pts',(21.2947352019821,-18.8924596835152,-20.6304089904986));
#51799=CARTESIAN_POINT('Ctrl Pts',(21.2952991221814,-18.9781599402378,-20.6346625967024));
#51800=CARTESIAN_POINT('Ctrl Pts',(21.291560298641,-19.0637377233315,-20.6389162029062));
#51801=CARTESIAN_POINT('Ctrl Pts',(21.2878940830978,-19.1476535848685,-20.6430872040273));
#51802=CARTESIAN_POINT('Ctrl Pts',(21.2800907694637,-19.2314512062992,-20.6472582051485));
#51803=CARTESIAN_POINT('Ctrl Pts',(21.2681770980697,-19.3146933079329,-20.6514292062697));
#51804=CARTESIAN_POINT('Ctrl Pts',(21.2562674233252,-19.3979074845465,-20.6555988081555));
#51805=CARTESIAN_POINT('Ctrl Pts',(21.2402501944417,-19.4805660564334,-20.6597684100413));
#51806=CARTESIAN_POINT('Ctrl Pts',(21.2202039195676,-19.5622377162439,-20.6639380119271));
#51807=CARTESIAN_POINT('Ctrl Pts',(21.2001583553192,-19.6439064808543,-20.6681074660036));
#51808=CARTESIAN_POINT('Ctrl Pts',(21.1760841395508,-19.7245879563529,-20.6722769200801));
#51809=CARTESIAN_POINT('Ctrl Pts',(21.1481104108274,-19.803863207525,-20.6764463741567));
#51810=CARTESIAN_POINT('Ctrl Pts',(21.1191514853748,-19.8859304253645,-20.6807626707424));
#51811=CARTESIAN_POINT('Ctrl Pts',(21.0860134227951,-19.9664900212761,-20.6850789673282));
#51812=CARTESIAN_POINT('Ctrl Pts',(21.0488942544675,-20.0450986188966,-20.6893952639139));
#51813=CARTESIAN_POINT('Ctrl Pts',(21.012986292885,-20.1211422004361,-20.6935707187789));
#51814=CARTESIAN_POINT('Ctrl Pts',(20.973353301723,-20.1953597550486,-20.697746173644));
#51815=CARTESIAN_POINT('Ctrl Pts',(20.9302210187628,-20.2673757017462,-20.701921628509));
#51816=CARTESIAN_POINT('Ctrl Pts',(20.8849064017287,-20.3430353891309,-20.7063083459551));
#51817=CARTESIAN_POINT('Ctrl Pts',(20.8357293771903,-20.416264321532,-20.7106950634012));
#51818=CARTESIAN_POINT('Ctrl Pts',(20.7830012667822,-20.486664070318,-20.7150817808473));
#51819=CARTESIAN_POINT('Ctrl Pts',(20.730273156374,-20.5570638191041,-20.7194684982935));
#51820=CARTESIAN_POINT('Ctrl Pts',(20.6739943901059,-20.6246339869631,-20.7238552157396));
#51821=CARTESIAN_POINT('Ctrl Pts',(20.6145211534102,-20.689020492561,-20.7282419331857));
#51822=CARTESIAN_POINT('Ctrl Pts',(20.5577862400574,-20.7504424534151,-20.7324266732139));
#51823=CARTESIAN_POINT('Ctrl Pts',(20.4979333332223,-20.809196146077,-20.7366114132421));
#51824=CARTESIAN_POINT('Ctrl Pts',(20.4352433664353,-20.8649482502566,-20.7407961532704));
#51825=CARTESIAN_POINT('Ctrl Pts',(20.3726426387416,-20.9206209913821,-20.7449749363261));
#51826=CARTESIAN_POINT('Ctrl Pts',(20.3072132137399,-20.9733003279932,-20.7491537193819));
#51827=CARTESIAN_POINT('Ctrl Pts',(20.2392743864999,-21.022688055055,-20.7533325024377));
#51828=CARTESIAN_POINT('Ctrl Pts',(20.1701199698419,-21.0729594476264,-20.7575860539972));
#51829=CARTESIAN_POINT('Ctrl Pts',(20.0983657941174,-21.1198199254428,-20.7618396055568));
#51830=CARTESIAN_POINT('Ctrl Pts',(20.0243857323821,-21.1629963052128,-20.7660931571163));
#51831=CARTESIAN_POINT('Ctrl Pts',(19.9518376847091,-21.2053369303006,-20.7702643737129));
#51832=CARTESIAN_POINT('Ctrl Pts',(19.8771495707328,-21.2441345685215,-20.7744355903094));
#51833=CARTESIAN_POINT('Ctrl Pts',(19.8007035796531,-21.2791749983951,-20.7786068069059));
#51834=CARTESIAN_POINT('Ctrl Pts',(19.7242832601421,-21.3142036612317,-20.7827766227531));
#51835=CARTESIAN_POINT('Ctrl Pts',(19.6461066537349,-21.3454774300037,-20.7869464386003));
#51836=CARTESIAN_POINT('Ctrl Pts',(19.5665789487914,-21.372828844431,-20.7911162544474));
#51837=CARTESIAN_POINT('Ctrl Pts',(19.4870540969431,-21.4001792776131,-20.7952859207004));
#51838=CARTESIAN_POINT('Ctrl Pts',(19.4061786782093,-21.4236074874285,-20.7994555869534));
#51839=CARTESIAN_POINT('Ctrl Pts',(19.3243748839096,-21.4429952823016,-20.8036252532064));
#51840=CARTESIAN_POINT('Ctrl Pts',(19.2396994033476,-21.4630636771966,-20.8079412937615));
#51841=CARTESIAN_POINT('Ctrl Pts',(19.1540296665579,-21.4788025811522,-20.8122573343165));
#51842=CARTESIAN_POINT('Ctrl Pts',(19.0678455531895,-21.4901385199818,-20.8165733748716));
#51843=CARTESIAN_POINT('Ctrl Pts',(18.9844645952716,-21.5011057551435,-20.8207490353481));
#51844=CARTESIAN_POINT('Ctrl Pts',(18.9006026815546,-21.5079520580807,-20.8249246958246));
#51845=CARTESIAN_POINT('Ctrl Pts',(18.816697839618,-21.5106639223084,-20.8291003563011));
#51846=CARTESIAN_POINT('Ctrl Pts',(18.7285618460937,-21.5135125403678,-20.8334865868954));
#51847=CARTESIAN_POINT('Ctrl Pts',(18.6403790644727,-21.511798786369,-20.8378728174898));
#51848=CARTESIAN_POINT('Ctrl Pts',(18.5526528282173,-21.5055687191236,-20.8422590480841));
#51849=CARTESIAN_POINT('Ctrl Pts',(18.4649265919619,-21.4993386518781,-20.8466452786785));
#51850=CARTESIAN_POINT('Ctrl Pts',(18.3776574674128,-21.4885924176826,-20.8510315092728));
#51851=CARTESIAN_POINT('Ctrl Pts',(18.2913357986938,-21.4734377654192,-20.8554177398671));
#51852=CARTESIAN_POINT('Ctrl Pts',(18.208977638002,-21.458978947548,-20.8596025742139));
#51853=CARTESIAN_POINT('Ctrl Pts',(18.1271754851468,-21.4404538825132,-20.8637874085605));
#51854=CARTESIAN_POINT('Ctrl Pts',(18.0463616913993,-21.4179184002202,-20.8679722429073));
#51855=CARTESIAN_POINT('Ctrl Pts',(17.9656628842856,-21.3954149827411,-20.8721511228247));
#51856=CARTESIAN_POINT('Ctrl Pts',(17.8859500822175,-21.3689126049628,-20.8763300027422));
#51857=CARTESIAN_POINT('Ctrl Pts',(17.8076468707951,-21.3385183594543,-20.8805088826597));
#51858=CARTESIAN_POINT('Ctrl Pts',(17.7279449213762,-21.3075811785374,-20.8847624103218));
#51859=CARTESIAN_POINT('Ctrl Pts',(17.6497038924681,-21.2726118027868,-20.8890159379838));
#51860=CARTESIAN_POINT('Ctrl Pts',(17.5733558319313,-21.2337767452422,-20.8932694656458));
#51861=CARTESIAN_POINT('Ctrl Pts',(17.4984833648361,-21.1956922602179,-20.8974407845723));
#51862=CARTESIAN_POINT('Ctrl Pts',(17.4254317742295,-21.1538904079626,-20.9016121034987));
#51863=CARTESIAN_POINT('Ctrl Pts',(17.3545880671759,-21.108576620383,-20.9057834224251));
#51864=CARTESIAN_POINT('Ctrl Pts',(17.2837681192032,-21.0632780298334,-20.909953342403));
#51865=CARTESIAN_POINT('Ctrl Pts',(17.2151549713756,-21.0144700907621,-20.9141232623808));
#51866=CARTESIAN_POINT('Ctrl Pts',(17.149108758861,-20.9624028834442,-20.9182931823587));
#51867=CARTESIAN_POINT('Ctrl Pts',(17.083064889567,-20.9103375233928,-20.922462954394));
#51868=CARTESIAN_POINT('Ctrl Pts',(17.0195881352145,-20.8550134104492,-20.9266327264293));
#51869=CARTESIAN_POINT('Ctrl Pts',(16.959006405508,-20.7967215886177,-20.9308024984647));
#51870=CARTESIAN_POINT('Ctrl Pts',(16.8963013133661,-20.7363866645942,-20.9351184191383));
#51871=CARTESIAN_POINT('Ctrl Pts',(16.8366983362716,-20.6728724968332,-20.939434339812));
#51872=CARTESIAN_POINT('Ctrl Pts',(16.780518958098,-20.6065427824416,-20.9437502604856));
#51873=CARTESIAN_POINT('Ctrl Pts',(16.7261638999388,-20.5423670012093,-20.9479260297243));
#51874=CARTESIAN_POINT('Ctrl Pts',(16.6750137422498,-20.4755561368783,-20.952101798963));
#51875=CARTESIAN_POINT('Ctrl Pts',(16.6273169433958,-20.4064712094149,-20.9562775682017));
#51876=CARTESIAN_POINT('Ctrl Pts',(16.5772188714759,-20.3339082335381,-20.9606635645928));
#51877=CARTESIAN_POINT('Ctrl Pts',(16.530931306338,-20.2588367080558,-20.965049560984));
#51878=CARTESIAN_POINT('Ctrl Pts',(16.4886879171311,-20.1817047005371,-20.9694355573751));
#51879=CARTESIAN_POINT('Ctrl Pts',(16.4464445279242,-20.1045726930183,-20.9738215537662));
#51880=CARTESIAN_POINT('Ctrl Pts',(16.408245498097,-20.0253807586023,-20.9782075501573));
#51881=CARTESIAN_POINT('Ctrl Pts',(16.374265613089,-19.9445994273774,-20.9825935465485));
#51882=CARTESIAN_POINT('Ctrl Pts',(16.3382155102257,-19.8588965093302,-20.9872467589128));
#51883=CARTESIAN_POINT('Ctrl Pts',(16.30679887472,-19.7711342279521,-20.9918999712772));
#51884=CARTESIAN_POINT('Ctrl Pts',(16.2802296059439,-19.6818019274115,-20.9965531836415));
#51885=CARTESIAN_POINT('Ctrl Pts',(16.2537435506638,-19.5927494107485,-21.0011918223993));
#51886=CARTESIAN_POINT('Ctrl Pts',(16.2320746955043,-19.5021369352023,-21.0058304611572));
#51887=CARTESIAN_POINT('Ctrl Pts',(16.2153886011344,-19.4104720509521,-21.010469099915));
#51888=CARTESIAN_POINT('Ctrl Pts',(16.1987928068799,-19.3193032294376,-21.0150826357574));
#51889=CARTESIAN_POINT('Ctrl Pts',(16.1871261077823,-19.2270936177058,-21.0196961715999));
#51890=CARTESIAN_POINT('Ctrl Pts',(16.1805035115345,-19.1343614087313,-21.0243097074423));
#51891=CARTESIAN_POINT('Ctrl Pts',(16.1762064899349,-19.0741928147187,-21.0273031653588));
#51892=CARTESIAN_POINT('Ctrl Pts',(16.1740320413834,-19.0138045835855,-21.0302966232753));
#51893=CARTESIAN_POINT('Ctrl Pts',(16.1740003516178,-18.9533417463077,-21.0332900811918));
#51894=CARTESIAN_POINT('Ctrl Pts',(16.1775161375017,-18.9533393271451,-21.0332901097715));
#51895=CARTESIAN_POINT('Ctrl Pts',(16.179969922226,-18.4391275102653,-21.0587831909243));
#51896=CARTESIAN_POINT('Ctrl Pts',(16.5801691895444,-17.06634175119,-21.1266682076376));
#51897=CARTESIAN_POINT('Ctrl Pts',(18.4990491880931,-16.0899931954376,-21.2211093027264));
#51898=CARTESIAN_POINT('Ctrl Pts',(19.8649654422083,-16.6008610266685,-21.2900573166623));
#51899=CARTESIAN_POINT('Ctrl Pts',(20.2916907304466,-16.9243022127157,-21.3166133950378));
#51900=CARTESIAN_POINT('',(16.1715628046961,-18.9501455684938,-20.9667098902285));
#51901=CARTESIAN_POINT('Ctrl Pts',(16.1715628046961,-18.9501455684938,-20.9667098902285));
#51902=CARTESIAN_POINT('Ctrl Pts',(16.1706210062014,-18.8345295298074,-20.9724759609646));
#51903=CARTESIAN_POINT('Ctrl Pts',(16.2303035994096,-17.8698877850362,-21.0206339672611));
#51904=CARTESIAN_POINT('Ctrl Pts',(17.4553333973082,-16.2082456258976,-21.1111839091181));
#51905=CARTESIAN_POINT('Ctrl Pts',(19.4740835894722,-16.3361983067415,-21.1999086076436));
#51906=CARTESIAN_POINT('Ctrl Pts',(20.2333094787133,-16.8707090063625,-21.2462413706087));
#51907=CARTESIAN_POINT('Ctrl Pts',(20.2955778924961,-16.9192440454753,-21.2501821980133));
#51908=CARTESIAN_POINT('Ctrl Pts',(20.2940725979671,-16.9211546778497,-20.4499991793503));
#51909=CARTESIAN_POINT('Ctrl Pts',(20.4294543463688,-17.0229918862778,-20.4584344114705));
#51910=CARTESIAN_POINT('Ctrl Pts',(21.1817798484721,-17.716545109861,-20.5092615791512));
#51911=CARTESIAN_POINT('Ctrl Pts',(21.6424139385631,-19.7912991649835,-20.6024806823924));
#51912=CARTESIAN_POINT('Ctrl Pts',(19.6025526266728,-21.851808827879,-20.7296564890738));
#51913=CARTESIAN_POINT('Ctrl Pts',(16.8944629917136,-21.2791319918735,-20.8510662250192));
#51914=CARTESIAN_POINT('Ctrl Pts',(16.1775450733739,-19.6845343053476,-20.9300840254041));
#51915=CARTESIAN_POINT('Ctrl Pts',(16.1715628046961,-18.9501455684938,-20.9667098902285));
#51916=CARTESIAN_POINT('Origin',(18.734,-18.952,1.76670989022851));
#51917=CARTESIAN_POINT('',(20.293535888361,-16.9218650751947,-19.6501081160065));
#51918=CARTESIAN_POINT('',(20.293535888361,-16.9218650751948,-19.716724552643));
#51919=CARTESIAN_POINT('',(20.293535888361,-16.9218650751948,1.76670989022851));
#51920=CARTESIAN_POINT('',(16.1740004726297,-18.9535555911146,-20.2332901098006));
#51921=CARTESIAN_POINT('Ctrl Pts',(20.293535888361,-16.9218650751948,-19.716724552643));
#51922=CARTESIAN_POINT('Ctrl Pts',(20.3599060643816,-16.9728501945365,-19.720906221147));
#51923=CARTESIAN_POINT('Ctrl Pts',(20.4238851560338,-17.0271793245034,-19.725087889651));
#51924=CARTESIAN_POINT('Ctrl Pts',(20.4851178704728,-17.0845990779399,-19.729269558155));
#51925=CARTESIAN_POINT('Ctrl Pts',(20.5462729423841,-17.1419460236487,-19.7334459243412));
#51926=CARTESIAN_POINT('Ctrl Pts',(20.6046882218323,-17.2023754951433,-19.7376222905273));
#51927=CARTESIAN_POINT('Ctrl Pts',(20.6600404295884,-17.2655930907427,-19.7417986567135));
#51928=CARTESIAN_POINT('Ctrl Pts',(20.7153403235321,-17.3287509388888,-19.7459710757827));
#51929=CARTESIAN_POINT('Ctrl Pts',(20.767582597195,-17.3946913295733,-19.7501434948519));
#51930=CARTESIAN_POINT('Ctrl Pts',(20.8164808501031,-17.4630831087821,-19.7543159139211));
#51931=CARTESIAN_POINT('Ctrl Pts',(20.8653546247269,-17.5314406513197,-19.7584862442928));
#51932=CARTESIAN_POINT('Ctrl Pts',(20.9108874353274,-17.6022467722473,-19.7626565746645));
#51933=CARTESIAN_POINT('Ctrl Pts',(20.9528339582812,-17.6751382746835,-19.7668269050362));
#51934=CARTESIAN_POINT('Ctrl Pts',(20.994772065989,-17.7480151537402,-19.7709963987627));
#51935=CARTESIAN_POINT('Ctrl Pts',(21.0331250860997,-17.8229761845117,-19.7751658924892));
#51936=CARTESIAN_POINT('Ctrl Pts',(21.0676924595754,-17.8996314789386,-19.7793353862157));
#51937=CARTESIAN_POINT('Ctrl Pts',(21.1022632674651,-17.9762943893915,-19.7835052941989));
#51938=CARTESIAN_POINT('Ctrl Pts',(21.1330474939752,-18.0546514778417,-19.7876752021822));
#51939=CARTESIAN_POINT('Ctrl Pts',(21.1598923176434,-18.134291945008,-19.7918451101654));
#51940=CARTESIAN_POINT('Ctrl Pts',(21.1867656122562,-18.21401687685,-19.7960194406482));
#51941=CARTESIAN_POINT('Ctrl Pts',(21.2096910150703,-18.2950274681917,-19.8001937711309));
#51942=CARTESIAN_POINT('Ctrl Pts',(21.2285654637021,-18.3768972723899,-19.8043681016137));
#51943=CARTESIAN_POINT('Ctrl Pts',(21.2474505170233,-18.4588130754865,-19.8085447774618));
#51944=CARTESIAN_POINT('Ctrl Pts',(21.2622800033412,-18.5415885996961,-19.8127214533099));
#51945=CARTESIAN_POINT('Ctrl Pts',(21.2730023687634,-18.624789102544,-19.816898129158));
#51946=CARTESIAN_POINT('Ctrl Pts',(21.2837431250598,-18.7081323099092,-19.821081968791));
#51947=CARTESIAN_POINT('Ctrl Pts',(21.290362656088,-18.7919014928153,-19.8252658084241));
#51948=CARTESIAN_POINT('Ctrl Pts',(21.2928614752057,-18.8756589841044,-19.8294496480571));
#51949=CARTESIAN_POINT('Ctrl Pts',(21.2945659689631,-18.9327916192854,-19.83230352751));
#51950=CARTESIAN_POINT('Ctrl Pts',(21.2943542420303,-18.9899188035593,-19.8351574069628));
#51951=CARTESIAN_POINT('Ctrl Pts',(21.2922402934573,-19.0469031133929,-19.8380112864157));
#51952=CARTESIAN_POINT('Ctrl Pts',(21.2891406189066,-19.1304589847303,-19.8421959187306));
#51953=CARTESIAN_POINT('Ctrl Pts',(21.2819372856921,-19.2140183312952,-19.8463805510455));
#51954=CARTESIAN_POINT('Ctrl Pts',(21.2706266468765,-19.2971452655857,-19.8505651833604));
#51955=CARTESIAN_POINT('Ctrl Pts',(21.2593321073624,-19.380153878921,-19.8547438593665));
#51956=CARTESIAN_POINT('Ctrl Pts',(21.243941936219,-19.4627308505955,-19.8589225353726));
#51957=CARTESIAN_POINT('Ctrl Pts',(21.2245044655718,-19.5444419861614,-19.8631012113787));
#51958=CARTESIAN_POINT('Ctrl Pts',(21.2047185799778,-19.6276177866251,-19.8673547897837));
#51959=CARTESIAN_POINT('Ctrl Pts',(21.1807388847111,-19.7098959225239,-19.8716083681886));
#51960=CARTESIAN_POINT('Ctrl Pts',(21.1526714444945,-19.7908256336015,-19.8758619465935));
#51961=CARTESIAN_POINT('Ctrl Pts',(21.125148163346,-19.8701863153761,-19.8800330585091));
#51962=CARTESIAN_POINT('Ctrl Pts',(21.0936943831976,-19.9482499363987,-19.8842041704246));
#51963=CARTESIAN_POINT('Ctrl Pts',(21.0584608475263,-20.0246051315918,-19.8883752823401));
#51964=CARTESIAN_POINT('Ctrl Pts',(21.0232391347282,-20.1009347052351,-19.8925449946083));
#51965=CARTESIAN_POINT('Ctrl Pts',(20.9842403779078,-20.1755565742226,-19.8967147068764));
#51966=CARTESIAN_POINT('Ctrl Pts',(20.9416632153647,-20.2480799078473,-19.9008844191445));
#51967=CARTESIAN_POINT('Ctrl Pts',(20.89908756777,-20.3206006610016,-19.9050539830491));
#51968=CARTESIAN_POINT('Ctrl Pts',(20.8529340012468,-20.3910226309664,-19.9092235469537));
#51969=CARTESIAN_POINT('Ctrl Pts',(20.8034461281557,-20.4589813279074,-19.9133931108583));
#51970=CARTESIAN_POINT('Ctrl Pts',(20.7522182683888,-20.5293294430996,-19.9177092760448));
#51971=CARTESIAN_POINT('Ctrl Pts',(20.6974175740299,-20.5970374130935,-19.9220254412314));
#51972=CARTESIAN_POINT('Ctrl Pts',(20.6393606095101,-20.6617370990089,-19.926341606418));
#51973=CARTESIAN_POINT('Ctrl Pts',(20.5831949030825,-20.7243291341788,-19.9305171686225));
#51974=CARTESIAN_POINT('Ctrl Pts',(20.523982186015,-20.784105569659,-19.9346927308271));
#51975=CARTESIAN_POINT('Ctrl Pts',(20.4620462261043,-20.8407710926543,-19.9388682930317));
#51976=CARTESIAN_POINT('Ctrl Pts',(20.396981927938,-20.900298748143,-19.9432547597093));
#51977=CARTESIAN_POINT('Ctrl Pts',(20.3289124964612,-20.9563925858392,-19.9476412263868));
#51978=CARTESIAN_POINT('Ctrl Pts',(20.2582501417943,-21.0087599532371,-19.9520276930644));
#51979=CARTESIAN_POINT('Ctrl Pts',(20.1875877871275,-21.061127320635,-19.9564141597419));
#51980=CARTESIAN_POINT('Ctrl Pts',(20.1143330347169,-21.1097679601497,-19.9608006264195));
#51981=CARTESIAN_POINT('Ctrl Pts',(20.0389283877474,-21.1544445288931,-19.965187093097));
#51982=CARTESIAN_POINT('Ctrl Pts',(19.9669932812531,-21.1970654264043,-19.9693717283982));
#51983=CARTESIAN_POINT('Ctrl Pts',(19.8928340180601,-21.2362376726233,-19.9735563636995));
#51984=CARTESIAN_POINT('Ctrl Pts',(19.8168151370649,-21.2717222633201,-19.9777409990007));
#51985=CARTESIAN_POINT('Ctrl Pts',(19.7409044598143,-21.3071563459651,-19.9819196779762));
#51986=CARTESIAN_POINT('Ctrl Pts',(19.6631398357117,-21.3389130062059,-19.9860983569518));
#51987=CARTESIAN_POINT('Ctrl Pts',(19.5839125153236,-21.3667978624093,-19.9902770359274));
#51988=CARTESIAN_POINT('Ctrl Pts',(19.5032651236309,-21.3951825270617,-19.9945306135879));
#51989=CARTESIAN_POINT('Ctrl Pts',(19.4211024978227,-21.4195549746049,-19.9987841912483));
#51990=CARTESIAN_POINT('Ctrl Pts',(19.3378610660991,-21.4397604010133,-20.0030377689088));
#51991=CARTESIAN_POINT('Ctrl Pts',(19.2562334111026,-21.4595741108662,-20.007208883732));
#51992=CARTESIAN_POINT('Ctrl Pts',(19.1735688735353,-21.4753808138571,-20.0113799985552));
#51993=CARTESIAN_POINT('Ctrl Pts',(19.0902949413619,-21.4870845971604,-20.0155511133785));
#51994=CARTESIAN_POINT('Ctrl Pts',(19.0070489529337,-21.4987844530938,-20.0197208285252));
#51995=CARTESIAN_POINT('Ctrl Pts',(18.9231944311979,-21.5063840596987,-20.0238905436719));
#51996=CARTESIAN_POINT('Ctrl Pts',(18.8391675225314,-21.509838890979,-20.0280602588185));
#51997=CARTESIAN_POINT('Ctrl Pts',(18.7551436043038,-21.513293599305,-20.032229825569));
#51998=CARTESIAN_POINT('Ctrl Pts',(18.670947771023,-21.5126038075443,-20.0363993923194));
#51999=CARTESIAN_POINT('Ctrl Pts',(18.5870183641846,-21.5077770635822,-20.0405689590698));
#52000=CARTESIAN_POINT('Ctrl Pts',(18.5001381401371,-21.5027806193961,-20.0448851207956));
#52001=CARTESIAN_POINT('Ctrl Pts',(18.4135439525319,-21.4933509339464,-20.0492012825213));
#52002=CARTESIAN_POINT('Ctrl Pts',(18.3277166966688,-21.4795549207553,-20.053517444247));
#52003=CARTESIAN_POINT('Ctrl Pts',(18.2446852202507,-21.4662083057154,-20.0576930091878));
#52004=CARTESIAN_POINT('Ctrl Pts',(18.1623719289166,-21.4487756010914,-20.0618685741286));
#52005=CARTESIAN_POINT('Ctrl Pts',(18.0812003839157,-21.4273691969563,-20.0660441390694));
#52006=CARTESIAN_POINT('Ctrl Pts',(17.9959291092672,-21.4048816199831,-20.0704305991875));
#52007=CARTESIAN_POINT('Ctrl Pts',(17.9119185059158,-21.3780085540391,-20.0748170593057));
#52008=CARTESIAN_POINT('Ctrl Pts',(17.8296377675495,-21.3469381938825,-20.0792035194239));
#52009=CARTESIAN_POINT('Ctrl Pts',(17.7473570291832,-21.315867833726,-20.0835899795421));
#52010=CARTESIAN_POINT('Ctrl Pts',(17.6668066567987,-21.2806004817434,-20.0879764396603));
#52011=CARTESIAN_POINT('Ctrl Pts',(17.5884257348681,-21.2413797419973,-20.0923628997785));
#52012=CARTESIAN_POINT('Ctrl Pts',(17.5136510990602,-21.2039635384314,-20.0965475399912));
#52013=CARTESIAN_POINT('Ctrl Pts',(17.4405723466444,-21.1628104733658,-20.100732180204));
#52014=CARTESIAN_POINT('Ctrl Pts',(17.3695877608619,-21.1180976990178,-20.1049168204167));
#52015=CARTESIAN_POINT('Ctrl Pts',(17.2987042121431,-21.0734485673238,-20.1090955043538));
#52016=CARTESIAN_POINT('Ctrl Pts',(17.2299092952355,-21.0252500336355,-20.1132741882909));
#52017=CARTESIAN_POINT('Ctrl Pts',(17.1635782312554,-20.9737258637741,-20.117452872228));
#52018=CARTESIAN_POINT('Ctrl Pts',(17.0960583483627,-20.9212782516533,-20.1217064486544));
#52019=CARTESIAN_POINT('Ctrl Pts',(17.0310919385808,-20.8653848344035,-20.1259600250807));
#52020=CARTESIAN_POINT('Ctrl Pts',(16.9690453966424,-20.8063287864041,-20.130213601507));
#52021=CARTESIAN_POINT('Ctrl Pts',(16.9082016411681,-20.748417553457,-20.1343847213775));
#52022=CARTESIAN_POINT('Ctrl Pts',(16.8501659076099,-20.6874655440672,-20.138555841248));
#52023=CARTESIAN_POINT('Ctrl Pts',(16.7952502349276,-20.6237802931102,-20.1427269611185));
#52024=CARTESIAN_POINT('Ctrl Pts',(16.7403529896792,-20.5601164122958,-20.1468966813333));
#52025=CARTESIAN_POINT('Ctrl Pts',(16.6885740261885,-20.4937214595179,-20.151066401548));
#52026=CARTESIAN_POINT('Ctrl Pts',(16.6401868618211,-20.4249380646821,-20.1552361217628));
#52027=CARTESIAN_POINT('Ctrl Pts',(16.5918014193429,-20.3561571175489,-20.1594056935953));
#52028=CARTESIAN_POINT('Ctrl Pts',(16.5468077999962,-20.2849882740964,-20.1635752654278));
#52029=CARTESIAN_POINT('Ctrl Pts',(16.5054369234077,-20.2118041965518,-20.1677448372603));
#52030=CARTESIAN_POINT('Ctrl Pts',(16.4626116274946,-20.136047286488,-20.1720609930269));
#52031=CARTESIAN_POINT('Ctrl Pts',(16.4236688015119,-20.0581312666225,-20.1763771487935));
#52032=CARTESIAN_POINT('Ctrl Pts',(16.3888124800457,-19.978496710297,-20.1806933045602));
#52033=CARTESIAN_POINT('Ctrl Pts',(16.3550914981633,-19.9014560095544,-20.1848688745654));
#52034=CARTESIAN_POINT('Ctrl Pts',(16.3251950198264,-19.8228074630063,-20.1890444445707));
#52035=CARTESIAN_POINT('Ctrl Pts',(16.2992578088289,-19.7429680540524,-20.193220014576));
#52036=CARTESIAN_POINT('Ctrl Pts',(16.2720106919199,-19.6590965186773,-20.1976064632233));
#52037=CARTESIAN_POINT('Ctrl Pts',(16.2491334314107,-19.5739112339791,-20.2019929118706));
#52038=CARTESIAN_POINT('Ctrl Pts',(16.2307217504163,-19.4879085791077,-20.2063793605179));
#52039=CARTESIAN_POINT('Ctrl Pts',(16.2123100694219,-19.4019059242363,-20.2107658091652));
#52040=CARTESIAN_POINT('Ctrl Pts',(16.1983639848637,-19.3150864841139,-20.2151522578125));
#52041=CARTESIAN_POINT('Ctrl Pts',(16.1889163328206,-19.2279513128369,-20.2195387064599));
#52042=CARTESIAN_POINT('Ctrl Pts',(16.1790436177049,-19.1368958083959,-20.2241225075637));
#52043=CARTESIAN_POINT('Ctrl Pts',(16.1740562221029,-19.0453011470167,-20.2287063086676));
#52044=CARTESIAN_POINT('Ctrl Pts',(16.17400047263,-18.9535555916975,-20.2332901097715));
#52045=CARTESIAN_POINT('Ctrl Pts',(16.1740004726297,-18.9535555911146,-20.2332901098006));
#52046=CARTESIAN_POINT('Ctrl Pts',(16.173950276098,-18.8709483454626,-20.2374173417138));
#52047=CARTESIAN_POINT('Ctrl Pts',(16.1779027082632,-18.7881812209217,-20.2415445736269));
#52048=CARTESIAN_POINT('Ctrl Pts',(16.1858778001745,-18.7056805838826,-20.24567180554));
#52049=CARTESIAN_POINT('Ctrl Pts',(16.1940130436929,-18.6215232123815,-20.2498819183568));
#52050=CARTESIAN_POINT('Ctrl Pts',(16.2063343518257,-18.5376436404924,-20.2540920311735));
#52051=CARTESIAN_POINT('Ctrl Pts',(16.2228070334153,-18.4544963471735,-20.2583021439902));
#52052=CARTESIAN_POINT('Ctrl Pts',(16.2389199317137,-18.3731650913156,-20.2624203028504));
#52053=CARTESIAN_POINT('Ctrl Pts',(16.2590046102178,-18.2925349422861,-20.2665384617107));
#52054=CARTESIAN_POINT('Ctrl Pts',(16.2829763019886,-18.2130258246822,-20.270656620571));
#52055=CARTESIAN_POINT('Ctrl Pts',(16.306937024594,-18.1335530895192,-20.27477289501));
#52056=CARTESIAN_POINT('Ctrl Pts',(16.3347810947711,-18.0552008202622,-20.2788891694489));
#52057=CARTESIAN_POINT('Ctrl Pts',(16.3663732871523,-17.9783759716349,-20.2830054438879));
#52058=CARTESIAN_POINT('Ctrl Pts',(16.3979610860963,-17.9015618068228,-20.2871211458883));
#52059=CARTESIAN_POINT('Ctrl Pts',(16.4332957915605,-17.8262750781318,-20.2912368478886));
#52060=CARTESIAN_POINT('Ctrl Pts',(16.4721937794553,-17.7529034147721,-20.2953525498889));
#52061=CARTESIAN_POINT('Ctrl Pts',(16.5126461134818,-17.6765998526872,-20.2996327134933));
#52062=CARTESIAN_POINT('Ctrl Pts',(16.5569522564909,-17.6023681227906,-20.3039128770976));
#52063=CARTESIAN_POINT('Ctrl Pts',(16.6048536565105,-17.5306148136394,-20.308193040702));
#52064=CARTESIAN_POINT('Ctrl Pts',(16.6509736167644,-17.4615299901315,-20.3123140262104));
#52065=CARTESIAN_POINT('Ctrl Pts',(16.7004258077716,-17.3947428571309,-20.3164350117188));
#52066=CARTESIAN_POINT('Ctrl Pts',(16.752937145384,-17.3305839626854,-20.3205559972272));
#52067=CARTESIAN_POINT('Ctrl Pts',(16.8054841274566,-17.2663815174707,-20.3246797800421));
#52068=CARTESIAN_POINT('Ctrl Pts',(16.8610940674614,-17.2048112072835,-20.3288035628569));
#52069=CARTESIAN_POINT('Ctrl Pts',(16.9194565997149,-17.1461671593191,-20.3329273456718));
#52070=CARTESIAN_POINT('Ctrl Pts',(16.9779086863938,-17.0874331249574,-20.3370574562278));
#52071=CARTESIAN_POINT('Ctrl Pts',(17.0391214358428,-17.0316346193019,-20.3411875667839));
#52072=CARTESIAN_POINT('Ctrl Pts',(17.1027516837168,-16.9790253598631,-20.34531767734));
#52073=CARTESIAN_POINT('Ctrl Pts',(17.1099251001079,-16.9730944050642,-20.3457832892737));
#52074=CARTESIAN_POINT('Ctrl Pts',(17.117129212341,-16.9672039375623,-20.3462489012075));
#52075=CARTESIAN_POINT('Ctrl Pts',(17.1243635072392,-16.9613542853705,-20.3467145131413));
#52076=CARTESIAN_POINT('Ctrl Pts',(17.1893810782662,-16.9087810654215,-20.3508991582797));
#52077=CARTESIAN_POINT('Ctrl Pts',(17.2570980357154,-16.8592987213468,-20.3550838034181));
#52078=CARTESIAN_POINT('Ctrl Pts',(17.3271882231892,-16.8131964502025,-20.3592684485566));
#52079=CARTESIAN_POINT('Ctrl Pts',(17.3971786444276,-16.7671598009406,-20.3634471372793));
#52080=CARTESIAN_POINT('Ctrl Pts',(17.4695352047632,-16.7244939187135,-20.367625826002));
#52081=CARTESIAN_POINT('Ctrl Pts',(17.5438988654958,-16.6854477085997,-20.3718045147248));
#52082=CARTESIAN_POINT('Ctrl Pts',(17.6195952011134,-16.6457017494008,-20.3760580899372));
#52083=CARTESIAN_POINT('Ctrl Pts',(17.6973709112956,-16.6097067832357,-20.3803116651496));
#52084=CARTESIAN_POINT('Ctrl Pts',(17.7768165359456,-16.5776790831607,-20.384565240362));
#52085=CARTESIAN_POINT('Ctrl Pts',(17.8547221935641,-16.5462722052193,-20.388736364645));
#52086=CARTESIAN_POINT('Ctrl Pts',(17.9342331580126,-16.5186803432953,-20.392907488928));
#52087=CARTESIAN_POINT('Ctrl Pts',(18.0149402978771,-16.4950602073346,-20.3970786132109));
#52088=CARTESIAN_POINT('Ctrl Pts',(18.0956203529298,-16.4714479981438,-20.4012483376907));
#52089=CARTESIAN_POINT('Ctrl Pts',(18.1774953450108,-16.4518049968894,-20.4054180621704));
#52090=CARTESIAN_POINT('Ctrl Pts',(18.2601401459595,-16.4362383183758,-20.4095877866501));
#52091=CARTESIAN_POINT('Ctrl Pts',(18.3427820029266,-16.42067219438,-20.4137573625955));
#52092=CARTESIAN_POINT('Ctrl Pts',(18.4261931620005,-16.4091821887308,-20.4179269385409));
#52093=CARTESIAN_POINT('Ctrl Pts',(18.5099387943012,-16.401824206824,-20.4220965144863));
#52094=CARTESIAN_POINT('Ctrl Pts',(18.5966283648554,-16.3942075673155,-20.426412664931));
#52095=CARTESIAN_POINT('Ctrl Pts',(18.683675837258,-16.3910189213194,-20.4307288153757));
#52096=CARTESIAN_POINT('Ctrl Pts',(18.7705956997936,-16.3922615847012,-20.4350449658204));
#52097=CARTESIAN_POINT('Ctrl Pts',(18.8546845879849,-16.3934637746163,-20.4392205395221));
#52098=CARTESIAN_POINT('Ctrl Pts',(18.9386535841084,-16.3988129731103,-20.4433961132239));
#52099=CARTESIAN_POINT('Ctrl Pts',(19.0220673264253,-16.4082592082828,-20.4475716869256));
#52100=CARTESIAN_POINT('Ctrl Pts',(19.1096934356116,-16.4181824752605,-20.4519581257418));
#52101=CARTESIAN_POINT('Ctrl Pts',(19.1967061584436,-16.432627374484,-20.456344564558));
#52102=CARTESIAN_POINT('Ctrl Pts',(19.2826140303201,-16.4514755258674,-20.4607310033742));
#52103=CARTESIAN_POINT('Ctrl Pts',(19.3685219021966,-16.4703236772509,-20.4651174421904));
#52104=CARTESIAN_POINT('Ctrl Pts',(19.4533243836861,-16.4935748540295,-20.4695038810066));
#52105=CARTESIAN_POINT('Ctrl Pts',(19.5365517912807,-16.5210514973961,-20.4738903198228));
#52106=CARTESIAN_POINT('Ctrl Pts',(19.6159350029072,-16.5472590203528,-20.4780741531404));
#52107=CARTESIAN_POINT('Ctrl Pts',(19.6941808259681,-16.57740780265,-20.482257986458));
#52108=CARTESIAN_POINT('Ctrl Pts',(19.7708697962533,-16.6113802048138,-20.4864418197756));
#52109=CARTESIAN_POINT('Ctrl Pts',(19.8474630716383,-16.6453102151496,-20.4906204323749));
#52110=CARTESIAN_POINT('Ctrl Pts',(19.9225029327703,-16.6830541923724,-20.4947990449742));
#52111=CARTESIAN_POINT('Ctrl Pts',(19.9955857717825,-16.7244449859911,-20.4989776575735));
#52112=CARTESIAN_POINT('Ctrl Pts',(20.0685856282316,-16.7657887820631,-20.5031515255298));
#52113=CARTESIAN_POINT('Ctrl Pts',(20.1396324806856,-16.8107709395873,-20.507325393486));
#52114=CARTESIAN_POINT('Ctrl Pts',(20.2083448692775,-16.859177215712,-20.5114992614423));
#52115=CARTESIAN_POINT('Ctrl Pts',(20.2371610874347,-16.8794775697176,-20.5132496748983));
#52116=CARTESIAN_POINT('Ctrl Pts',(20.2655670197412,-16.9003795799026,-20.5150000883544));
#52117=CARTESIAN_POINT('Ctrl Pts',(20.293535888361,-16.9218650751948,-20.5167505018104));
#52118=CARTESIAN_POINT('',(16.1742339566945,-18.9509923323772,-20.1667099326003));
#52119=CARTESIAN_POINT('Ctrl Pts',(16.1778405451444,-18.9509805605723,-20.166710586341));
#52120=CARTESIAN_POINT('Ctrl Pts',(16.17655678384,-18.5861666074448,-20.1847914783433));
#52121=CARTESIAN_POINT('Ctrl Pts',(16.4202751438729,-17.3676607662538,-20.2452643059062));
#52122=CARTESIAN_POINT('Ctrl Pts',(18.1401763667744,-16.0727553476898,-20.3396938369093));
#52123=CARTESIAN_POINT('Ctrl Pts',(19.749082511602,-16.5112008275589,-20.41604247591));
#52124=CARTESIAN_POINT('Ctrl Pts',(20.2940725979671,-16.9211546778497,-20.4499991793503));
#52125=CARTESIAN_POINT('Ctrl Pts',(20.293535888361,-16.9218650751947,-19.6501081160065));
#52126=CARTESIAN_POINT('Ctrl Pts',(20.3602263211758,-16.973096213635,-19.6542777831496));
#52127=CARTESIAN_POINT('Ctrl Pts',(20.4243867046238,-17.0276147056197,-19.6584474502926));
#52128=CARTESIAN_POINT('Ctrl Pts',(20.4856865660341,-17.0851325236172,-19.6626171174357));
#52129=CARTESIAN_POINT('Ctrl Pts',(20.5470483483268,-17.1427084421384,-19.6667909964883));
#52130=CARTESIAN_POINT('Ctrl Pts',(20.6055435003501,-17.2032894232085,-19.6709648755409));
#52131=CARTESIAN_POINT('Ctrl Pts',(20.6608777171633,-17.2665498336944,-19.6751387545935));
#52132=CARTESIAN_POINT('Ctrl Pts',(20.7162388992875,-17.3298410720612,-19.6793146676488));
#52133=CARTESIAN_POINT('Ctrl Pts',(20.7684357919223,-17.3958139797163,-19.6834905807041));
#52134=CARTESIAN_POINT('Ctrl Pts',(20.817215346003,-17.4641109509854,-19.6876664937594));
#52135=CARTESIAN_POINT('Ctrl Pts',(20.8660828502715,-17.5325310626062,-19.6918499360417));
#52136=CARTESIAN_POINT('Ctrl Pts',(20.9115204546417,-17.6032832230595,-19.696033378324));
#52137=CARTESIAN_POINT('Ctrl Pts',(20.9533193413648,-17.6759821078668,-19.7002168206063));
#52138=CARTESIAN_POINT('Ctrl Pts',(20.9933959861807,-17.745685576388,-19.7042278922783));
#52139=CARTESIAN_POINT('Ctrl Pts',(21.0301277554738,-17.8171781553883,-19.7082389639503));
#52140=CARTESIAN_POINT('Ctrl Pts',(21.0633723464495,-17.8901033611523,-19.7122500356223));
#52141=CARTESIAN_POINT('Ctrl Pts',(21.0980554588832,-17.9661841020042,-19.7164346697446));
#52142=CARTESIAN_POINT('Ctrl Pts',(21.1290718315276,-18.0441074153776,-19.7206193038669));
#52143=CARTESIAN_POINT('Ctrl Pts',(21.1562228177885,-18.1234852922339,-19.7248039379892));
#52144=CARTESIAN_POINT('Ctrl Pts',(21.1833351579802,-18.2027501845047,-19.7289826158026));
#52145=CARTESIAN_POINT('Ctrl Pts',(21.2065928926805,-18.2834650962588,-19.733161293616));
#52146=CARTESIAN_POINT('Ctrl Pts',(21.2258445987289,-18.3652202322969,-19.7373399714295));
#52147=CARTESIAN_POINT('Ctrl Pts',(21.2454413793526,-18.4484407771033,-19.7415935493826));
#52148=CARTESIAN_POINT('Ctrl Pts',(21.2608869019323,-18.5327387665071,-19.7458471273357));
#52149=CARTESIAN_POINT('Ctrl Pts',(21.2720739254928,-18.6176637190888,-19.7501007052888));
#52150=CARTESIAN_POINT('Ctrl Pts',(21.2830440658925,-18.7009422290717,-19.7542718189987));
#52151=CARTESIAN_POINT('Ctrl Pts',(21.2899192902196,-18.7848231321654,-19.7584429327087));
#52152=CARTESIAN_POINT('Ctrl Pts',(21.2926499549078,-18.8688711346757,-19.7626140464186));
#52153=CARTESIAN_POINT('Ctrl Pts',(21.2953797032961,-18.9528909340954,-19.7667837604725));
#52154=CARTESIAN_POINT('Ctrl Pts',(21.2939676391625,-19.0370772621645,-19.7709534745263));
#52155=CARTESIAN_POINT('Ctrl Pts',(21.2884161370488,-19.1209917121782,-19.7751231885802));
#52156=CARTESIAN_POINT('Ctrl Pts',(21.2828648324788,-19.2049031761925,-19.7792927542596));
#52157=CARTESIAN_POINT('Ctrl Pts',(21.2731744140114,-19.2885423224134,-19.783462319939));
#52158=CARTESIAN_POINT('Ctrl Pts',(21.2593992661682,-19.3714741308316,-19.7876318856184));
#52159=CARTESIAN_POINT('Ctrl Pts',(21.2451397991641,-19.4573217311042,-19.7919480486755));
#52160=CARTESIAN_POINT('Ctrl Pts',(21.2265031054957,-19.5424108076161,-19.7962642117326));
#52161=CARTESIAN_POINT('Ctrl Pts',(21.2036071461083,-19.6262703789215,-19.8005803747897));
#52162=CARTESIAN_POINT('Ctrl Pts',(21.1814570231881,-19.7073982225299,-19.804755938724));
#52163=CARTESIAN_POINT('Ctrl Pts',(21.1553210566129,-19.7873750003197,-19.8089315026582));
#52164=CARTESIAN_POINT('Ctrl Pts',(21.1253562910769,-19.8657916004906,-19.8131070665925));
#52165=CARTESIAN_POINT('Ctrl Pts',(21.0938780701788,-19.9481688531772,-19.817493529211));
#52166=CARTESIAN_POINT('Ctrl Pts',(21.0581743348026,-20.0288236424593,-19.8218799918296));
#52167=CARTESIAN_POINT('Ctrl Pts',(21.0184823804606,-20.1073095919991,-19.8262664544481));
#52168=CARTESIAN_POINT('Ctrl Pts',(20.9787904261185,-20.1857955415389,-19.8306529170666));
#52169=CARTESIAN_POINT('Ctrl Pts',(20.9351106070456,-20.262112185551,-19.8350393796852));
#52170=CARTESIAN_POINT('Ctrl Pts',(20.887732090269,-20.3358490103134,-19.8394258423037));
#52171=CARTESIAN_POINT('Ctrl Pts',(20.8425335350788,-20.4061930854412,-19.8436104767381));
#52172=CARTESIAN_POINT('Ctrl Pts',(20.7938009308873,-20.4744513619087,-19.8477951111725));
#52173=CARTESIAN_POINT('Ctrl Pts',(20.7417530082945,-20.5402467873993,-19.8519797456069));
#52174=CARTESIAN_POINT('Ctrl Pts',(20.6897791695075,-20.6059485612075,-19.8561584237297));
#52175=CARTESIAN_POINT('Ctrl Pts',(20.6344996686009,-20.669194089486,-19.8603371018525));
#52176=CARTESIAN_POINT('Ctrl Pts',(20.5761771160362,-20.729634234918,-19.8645157799753));
#52177=CARTESIAN_POINT('Ctrl Pts',(20.5168091743247,-20.7911577258021,-19.8687693578507));
#52178=CARTESIAN_POINT('Ctrl Pts',(20.4542882752172,-20.849773866077,-19.8730229357261));
#52179=CARTESIAN_POINT('Ctrl Pts',(20.3889351547385,-20.9051486460612,-19.8772765136015));
#52180=CARTESIAN_POINT('Ctrl Pts',(20.3248490313748,-20.9594498784325,-19.8814476276121));
#52181=CARTESIAN_POINT('Ctrl Pts',(20.2580398900243,-21.0106339980016,-19.8856187416226));
#52182=CARTESIAN_POINT('Ctrl Pts',(20.1888468727078,-21.0584236461292,-19.8897898556332));
#52183=CARTESIAN_POINT('Ctrl Pts',(20.119677073816,-21.1061972579516,-19.8939595699837));
#52184=CARTESIAN_POINT('Ctrl Pts',(20.0481253658498,-21.1505783992841,-19.8981292843343));
#52185=CARTESIAN_POINT('Ctrl Pts',(19.9745616647957,-21.1913317654692,-19.9022989986849));
#52186=CARTESIAN_POINT('Ctrl Pts',(19.9010005814965,-21.232083681451,-19.9064685646567));
#52187=CARTESIAN_POINT('Ctrl Pts',(19.8254280502834,-21.2692078567734,-19.9106381306285));
#52188=CARTESIAN_POINT('Ctrl Pts',(19.748239291486,-21.3025145520941,-19.9148076966003));
#52189=CARTESIAN_POINT('Ctrl Pts',(19.6683366724282,-21.3369922691832,-19.9191238592991));
#52190=CARTESIAN_POINT('Ctrl Pts',(19.5867025423585,-21.3673788575717,-19.9234400219978));
#52191=CARTESIAN_POINT('Ctrl Pts',(19.5037967719923,-21.3935185704455,-19.9277561846965));
#52192=CARTESIAN_POINT('Ctrl Pts',(19.423591647215,-21.4188067852878,-19.9319317489098));
#52193=CARTESIAN_POINT('Ctrl Pts',(19.3421969248401,-21.4401204858129,-19.936107313123));
#52194=CARTESIAN_POINT('Ctrl Pts',(19.2600416085035,-21.4573702772491,-19.9402828773363));
#52195=CARTESIAN_POINT('Ctrl Pts',(19.1737368242881,-21.4754913142561,-19.9446693392777));
#52196=CARTESIAN_POINT('Ctrl Pts',(19.0865931685419,-21.4891270269191,-19.9490558012192));
#52197=CARTESIAN_POINT('Ctrl Pts',(18.9991144164072,-21.4982353281292,-19.9534422631607));
#52198=CARTESIAN_POINT('Ctrl Pts',(18.9116356642725,-21.5073436293392,-19.9578287251022));
#52199=CARTESIAN_POINT('Ctrl Pts',(18.823822399141,-21.5119245648308,-19.9622151870437));
#52200=CARTESIAN_POINT('Ctrl Pts',(18.7361763184532,-21.5119990749291,-19.9666016489852));
#52201=CARTESIAN_POINT('Ctrl Pts',(18.6525629441398,-21.5120701567241,-19.9707862842974));
#52202=CARTESIAN_POINT('Ctrl Pts',(18.56879048318,-21.5080406575016,-19.9749709196097));
#52203=CARTESIAN_POINT('Ctrl Pts',(18.4852943717973,-21.4998904039421,-19.9791555549219));
#52204=CARTESIAN_POINT('Ctrl Pts',(18.401917106683,-21.4917517512489,-19.9833342339293));
#52205=CARTESIAN_POINT('Ctrl Pts',(18.3188158637713,-21.479504039016,-19.9875129129367));
#52206=CARTESIAN_POINT('Ctrl Pts',(18.2364263585066,-21.4631790998037,-19.9916915919441));
#52207=CARTESIAN_POINT('Ctrl Pts',(18.1525601036476,-21.4465615523608,-19.9959451695992));
#52208=CARTESIAN_POINT('Ctrl Pts',(18.0694318349348,-21.4257191735617,-20.0001987472543));
#52209=CARTESIAN_POINT('Ctrl Pts',(17.9874960097629,-21.4007408585965,-20.0044523249094));
#52210=CARTESIAN_POINT('Ctrl Pts',(17.9071486482338,-21.3762467902365,-20.0086234398147));
#52211=CARTESIAN_POINT('Ctrl Pts',(17.8279483680941,-21.3477758591386,-20.0127945547199));
#52212=CARTESIAN_POINT('Ctrl Pts',(17.750311955338,-21.3154631012117,-20.0169656696251));
#52213=CARTESIAN_POINT('Ctrl Pts',(17.6727015942353,-21.283161186145,-20.0211353848722));
#52214=CARTESIAN_POINT('Ctrl Pts',(17.5966544826743,-21.2470201811681,-20.0253051001192));
#52215=CARTESIAN_POINT('Ctrl Pts',(17.5225687032624,-21.2072237612451,-20.0294748153663));
#52216=CARTESIAN_POINT('Ctrl Pts',(17.4484855601721,-21.1674287574665,-20.0336443822352));
#52217=CARTESIAN_POINT('Ctrl Pts',(17.3763640153245,-21.1239788158134,-20.0378139491041));
#52218=CARTESIAN_POINT('Ctrl Pts',(17.3065775348649,-21.0771035518364,-20.041983515973));
#52219=CARTESIAN_POINT('Ctrl Pts',(17.2343374822407,-21.0285802345094,-20.0462996776141));
#52220=CARTESIAN_POINT('Ctrl Pts',(17.1646001862986,-20.9763865421865,-20.0506158392553));
#52221=CARTESIAN_POINT('Ctrl Pts',(17.0977455243703,-20.920824850255,-20.0549320008964));
#52222=CARTESIAN_POINT('Ctrl Pts',(17.0330686154625,-20.8670730491964,-20.059107565999));
#52223=CARTESIAN_POINT('Ctrl Pts',(16.9710897386263,-20.810169654399,-20.0632831311016));
#52224=CARTESIAN_POINT('Ctrl Pts',(16.9121162723823,-20.7504270024224,-20.0674586962043));
#52225=CARTESIAN_POINT('Ctrl Pts',(16.8501642397595,-20.6876669348876,-20.0718451561147));
#52226=CARTESIAN_POINT('Ctrl Pts',(16.7915295867437,-20.6217736911657,-20.0762316160251));
#52227=CARTESIAN_POINT('Ctrl Pts',(16.7365203854165,-20.5531480847578,-20.0806180759355));
#52228=CARTESIAN_POINT('Ctrl Pts',(16.6815111840894,-20.4845224783498,-20.0850045358459));
#52229=CARTESIAN_POINT('Ctrl Pts',(16.6301277117734,-20.4131650245491,-20.0893909957563));
#52230=CARTESIAN_POINT('Ctrl Pts',(16.5826239199876,-20.339508905323,-20.0937774556667));
#52231=CARTESIAN_POINT('Ctrl Pts',(16.5362791661252,-20.2676499107529,-20.0980568909966));
#52232=CARTESIAN_POINT('Ctrl Pts',(16.4934601213991,-20.1933453656254,-20.1023363263266));
#52233=CARTESIAN_POINT('Ctrl Pts',(16.4544271376053,-20.1169667656347,-20.1066157616565));
#52234=CARTESIAN_POINT('Ctrl Pts',(16.4154575008855,-20.0407121213442,-20.1108882518421));
#52235=CARTESIAN_POINT('Ctrl Pts',(16.3802619051423,-19.9623904954392,-20.1151607420277));
#52236=CARTESIAN_POINT('Ctrl Pts',(16.3490570393213,-19.882401566158,-20.1194332322133));
#52237=CARTESIAN_POINT('Ctrl Pts',(16.3179055660145,-19.8025495004692,-20.1236984120328));
#52238=CARTESIAN_POINT('Ctrl Pts',(16.2907313869642,-19.7210362103122,-20.1279635918524));
#52239=CARTESIAN_POINT('Ctrl Pts',(16.2677042874668,-19.6382838030585,-20.1322287716719));
#52240=CARTESIAN_POINT('Ctrl Pts',(16.2447004012897,-19.5556148174328,-20.136489651819));
#52241=CARTESIAN_POINT('Ctrl Pts',(16.2258353999309,-19.4717096122622,-20.1407505319661));
#52242=CARTESIAN_POINT('Ctrl Pts',(16.2112300227482,-19.3870076342743,-20.1450114121132));
#52243=CARTESIAN_POINT('Ctrl Pts',(16.1966372356338,-19.3023786707434,-20.1492686193135));
#52244=CARTESIAN_POINT('Ctrl Pts',(16.1862968405519,-19.2169547258213,-20.1535258265139));
#52245=CARTESIAN_POINT('Ctrl Pts',(16.1802787590759,-19.1311865610278,-20.1577830337143));
#52246=CARTESIAN_POINT('Ctrl Pts',(16.1760723590192,-19.0712380185088,-20.1607586525524));
#52247=CARTESIAN_POINT('Ctrl Pts',(16.1739765481552,-19.0111215762638,-20.1637342713904));
#52248=CARTESIAN_POINT('Ctrl Pts',(16.1740001980189,-18.950993095359,-20.1667098902285));
#52249=CARTESIAN_POINT('Origin',(18.734,-18.952,1.76670989022851));
#52250=CARTESIAN_POINT('',(20.293535888361,-16.9218650751948,-18.8501886412182));
#52251=CARTESIAN_POINT('',(20.2933494025377,-16.9221164381228,-18.9165759009586));
#52252=CARTESIAN_POINT('',(20.293535888361,-16.9218650751948,1.76670989022851));
#52253=CARTESIAN_POINT('',(16.1740009418753,-18.9498040034616,-19.4332901097715));
#52254=CARTESIAN_POINT('Ctrl Pts',(20.2933494025375,-16.9221164381226,-18.9165759009586));
#52255=CARTESIAN_POINT('Ctrl Pts',(20.460481259063,-17.0478571352914,-18.9269774805209));
#52256=CARTESIAN_POINT('Ctrl Pts',(21.2286611541766,-17.7870025066956,-18.9797709956437));
#52257=CARTESIAN_POINT('Ctrl Pts',(21.6004478622574,-19.9250196443109,-19.074956446327));
#52258=CARTESIAN_POINT('Ctrl Pts',(19.4673983198524,-21.8889061091152,-19.2021322530084));
#52259=CARTESIAN_POINT('Ctrl Pts',(16.8320816481898,-21.2027757351818,-19.3215765971073));
#52260=CARTESIAN_POINT('Ctrl Pts',(16.1790132429278,-19.6455867561426,-19.3986290056455));
#52261=CARTESIAN_POINT('Ctrl Pts',(16.1726852643248,-18.9498155443718,-19.4332894786233));
#52262=CARTESIAN_POINT('Ctrl Pts',(16.1740009418753,-18.9498040034616,-19.4332901097715));
#52263=CARTESIAN_POINT('Ctrl Pts',(16.1741094126172,-18.8233534412475,-19.4395926510339));
#52264=CARTESIAN_POINT('Ctrl Pts',(16.1835900621658,-18.6972910723228,-19.4458951922963));
#52265=CARTESIAN_POINT('Ctrl Pts',(16.2022529884095,-18.572715055265,-19.4521977335588));
#52266=CARTESIAN_POINT('Ctrl Pts',(16.2064836512073,-18.5444751579424,-19.4536264444963));
#52267=CARTESIAN_POINT('Ctrl Pts',(16.2111860003678,-18.5163115073012,-19.4550551554338));
#52268=CARTESIAN_POINT('Ctrl Pts',(16.2163575306343,-18.4882367021355,-19.4564838663713));
#52269=CARTESIAN_POINT('Ctrl Pts',(16.2315047248245,-18.4060067810516,-19.4606685004925));
#52270=CARTESIAN_POINT('Ctrl Pts',(16.25071296974,-18.3243667083971,-19.4648531346137));
#52271=CARTESIAN_POINT('Ctrl Pts',(16.2739228554016,-18.2437483197165,-19.469037768735));
#52272=CARTESIAN_POINT('Ctrl Pts',(16.2970997046629,-18.1632446813365,-19.4732164465473));
#52273=CARTESIAN_POINT('Ctrl Pts',(16.3242667547544,-18.0837602766464,-19.4773951243597));
#52274=CARTESIAN_POINT('Ctrl Pts',(16.3553134075097,-18.0057177510347,-19.4815738021721));
#52275=CARTESIAN_POINT('Ctrl Pts',(16.3869165517615,-17.9262763628078,-19.4858273801254));
#52276=CARTESIAN_POINT('Ctrl Pts',(16.4225396637624,-17.8483295278622,-19.4900809580788));
#52277=CARTESIAN_POINT('Ctrl Pts',(16.4620126245779,-17.7723079359755,-19.4943345360321));
#52278=CARTESIAN_POINT('Ctrl Pts',(16.5007203219077,-17.6977601769908,-19.498505649741));
#52279=CARTESIAN_POINT('Ctrl Pts',(16.5431297041304,-17.6250641048156,-19.5026767634499));
#52280=CARTESIAN_POINT('Ctrl Pts',(16.5890321382659,-17.5546049691916,-19.5068478771588));
#52281=CARTESIAN_POINT('Ctrl Pts',(16.634919169412,-17.484169476787,-19.5110175912116));
#52282=CARTESIAN_POINT('Ctrl Pts',(16.6842966737064,-17.4159698153114,-19.5151873052644));
#52283=CARTESIAN_POINT('Ctrl Pts',(16.7369115952916,-17.3503639914827,-19.5193570193173));
#52284=CARTESIAN_POINT('Ctrl Pts',(16.7895246446353,-17.2847605021618,-19.5235265849956));
#52285=CARTESIAN_POINT('Ctrl Pts',(16.8453745937438,-17.2217510253186,-19.527696150674));
#52286=CARTESIAN_POINT('Ctrl Pts',(16.9041676934287,-17.1616610014224,-19.5318657163523));
#52287=CARTESIAN_POINT('Ctrl Pts',(16.9650278943521,-17.0994582778473,-19.5361818794107));
#52288=CARTESIAN_POINT('Ctrl Pts',(17.0290416909462,-17.0403845007301,-19.540498042469));
#52289=CARTESIAN_POINT('Ctrl Pts',(17.0958426218327,-16.984758173392,-19.5448142055274));
#52290=CARTESIAN_POINT('Ctrl Pts',(17.1604675106391,-16.9309438751296,-19.5489897694607));
#52291=CARTESIAN_POINT('Ctrl Pts',(17.2277003349621,-16.8803561190544,-19.5531653333939));
#52292=CARTESIAN_POINT('Ctrl Pts',(17.2971780335747,-16.8332403069725,-19.5573408973272));
#52293=CARTESIAN_POINT('Ctrl Pts',(17.370164900217,-16.7837447773015,-19.5617273599481));
#52294=CARTESIAN_POINT('Ctrl Pts',(17.4456288796107,-16.7380814487272,-19.5661138225691));
#52295=CARTESIAN_POINT('Ctrl Pts',(17.523119783767,-16.696480303359,-19.57050028519));
#52296=CARTESIAN_POINT('Ctrl Pts',(17.6006106879233,-16.6548791579908,-19.5748867478109));
#52297=CARTESIAN_POINT('Ctrl Pts',(17.6801279596806,-16.6173403747401,-19.5792732104318));
#52298=CARTESIAN_POINT('Ctrl Pts',(17.7611994326909,-16.5840348279075,-19.5836596730528));
#52299=CARTESIAN_POINT('Ctrl Pts',(17.8385406770861,-16.5522617227492,-19.587844307487));
#52300=CARTESIAN_POINT('Ctrl Pts',(17.9175841221718,-16.5242225928453,-19.5920289419213));
#52301=CARTESIAN_POINT('Ctrl Pts',(17.9979345050501,-16.5001012282021,-19.5962135763556));
#52302=CARTESIAN_POINT('Ctrl Pts',(18.078170519057,-16.4760141973499,-19.6003922544782));
#52303=CARTESIAN_POINT('Ctrl Pts',(18.1597093389465,-16.4558339863015,-19.6045709326009));
#52304=CARTESIAN_POINT('Ctrl Pts',(18.2421357220942,-16.4396963694409,-19.6087496107236));
#52305=CARTESIAN_POINT('Ctrl Pts',(18.3260395379465,-16.4232694975869,-19.613003188599));
#52306=CARTESIAN_POINT('Ctrl Pts',(18.4108626031779,-16.411031755533,-19.6172567664745));
#52307=CARTESIAN_POINT('Ctrl Pts',(18.4961506937665,-16.4030732243699,-19.6215103443499));
#52308=CARTESIAN_POINT('Ctrl Pts',(18.5797853091396,-16.3952689847841,-19.6256814583603));
#52309=CARTESIAN_POINT('Ctrl Pts',(18.6638666007976,-16.3915795598322,-19.6298525723707));
#52310=CARTESIAN_POINT('Ctrl Pts',(18.7479577055537,-16.3920380505844,-19.634023686381));
#52311=CARTESIAN_POINT('Ctrl Pts',(18.8320205926793,-16.3924963874854,-19.6381934007314));
#52312=CARTESIAN_POINT('Ctrl Pts',(18.9160928267199,-16.3970998732974,-19.6423631150818));
#52313=CARTESIAN_POINT('Ctrl Pts',(18.9997364062972,-16.4058295103493,-19.6465328294322));
#52314=CARTESIAN_POINT('Ctrl Pts',(19.0833770094284,-16.4145588367581,-19.6507023954039));
#52315=CARTESIAN_POINT('Ctrl Pts',(19.1665885309651,-16.4274139738732,-19.6548719613755));
#52316=CARTESIAN_POINT('Ctrl Pts',(19.2489383260598,-16.444324079879,-19.6590415273471));
#52317=CARTESIAN_POINT('Ctrl Pts',(19.3341834370064,-16.461828724073,-19.6633576900461));
#52318=CARTESIAN_POINT('Ctrl Pts',(19.4185045808358,-16.4836786817424,-19.667673852745));
#52319=CARTESIAN_POINT('Ctrl Pts',(19.5014355882166,-16.5097382167469,-19.6719900154439));
#52320=CARTESIAN_POINT('Ctrl Pts',(19.5816651279086,-16.5349488655021,-19.6761655796569));
#52321=CARTESIAN_POINT('Ctrl Pts',(19.6605932821672,-16.5640988419222,-19.68034114387));
#52322=CARTESIAN_POINT('Ctrl Pts',(19.7378171886915,-16.597015700331,-19.684516708083));
#52323=CARTESIAN_POINT('Ctrl Pts',(19.81894148943,-16.6315951102716,-19.6889031700249));
#52324=CARTESIAN_POINT('Ctrl Pts',(19.8981843303164,-16.6703316765417,-19.6932896319667));
#52325=CARTESIAN_POINT('Ctrl Pts',(19.9751086547792,-16.7129713474294,-19.6976760939086));
#52326=CARTESIAN_POINT('Ctrl Pts',(20.0520329792421,-16.7556110183172,-19.7020625558505));
#52327=CARTESIAN_POINT('Ctrl Pts',(20.1266383352645,-16.8021534221799,-19.7064490177923));
#52328=CARTESIAN_POINT('Ctrl Pts',(20.1985254700754,-16.8522940330845,-19.7108354797342));
#52329=CARTESIAN_POINT('Ctrl Pts',(20.230696316323,-16.8747329004621,-19.7127985040371));
#52330=CARTESIAN_POINT('Ctrl Pts',(20.2623793611531,-16.8979308421821,-19.7147615283401));
#52331=CARTESIAN_POINT('Ctrl Pts',(20.293535888361,-16.9218650751948,-19.716724552643));
#52332=CARTESIAN_POINT('',(16.1740010149448,-18.9542795868247,-19.3667098901939));
#52333=CARTESIAN_POINT('Ctrl Pts',(16.1740010149441,-18.9542795861284,-19.3667098902285));
#52334=CARTESIAN_POINT('Ctrl Pts',(16.173926819566,-18.8709574030249,-19.3708480242598));
#52335=CARTESIAN_POINT('Ctrl Pts',(16.1779248169782,-18.7875513930795,-19.374986158291));
#52336=CARTESIAN_POINT('Ctrl Pts',(16.1859928190662,-18.7044936245066,-19.3791242923222));
#52337=CARTESIAN_POINT('Ctrl Pts',(16.1940571655296,-18.6214734895413,-19.3832605513584));
#52338=CARTESIAN_POINT('Ctrl Pts',(16.2061878113244,-18.5388017480886,-19.3873968103945));
#52339=CARTESIAN_POINT('Ctrl Pts',(16.2223305526747,-18.456907496146,-19.3915330694306));
#52340=CARTESIAN_POINT('Ctrl Pts',(16.238471016352,-18.3750247991377,-19.3956687448579));
#52341=CARTESIAN_POINT('Ctrl Pts',(16.2586223602409,-18.2939198329686,-19.3998044202853));
#52342=CARTESIAN_POINT('Ctrl Pts',(16.2826791433887,-18.2140121559657,-19.4039400957127));
#52343=CARTESIAN_POINT('Ctrl Pts',(16.3067400382202,-18.1340908214803,-19.4080764779922));
#52344=CARTESIAN_POINT('Ctrl Pts',(16.3347075604887,-18.0553676300741,-19.4122128602717));
#52345=CARTESIAN_POINT('Ctrl Pts',(16.3664266589084,-17.9782461940757,-19.4163492425513));
#52346=CARTESIAN_POINT('Ctrl Pts',(16.3981808282496,-17.9010394870584,-19.4204901983132));
#52347=CARTESIAN_POINT('Ctrl Pts',(16.4336946710468,-17.8254385023485,-19.4246311540751));
#52348=CARTESIAN_POINT('Ctrl Pts',(16.4727655806441,-17.7518254707252,-19.4287721098371));
#52349=CARTESIAN_POINT('Ctrl Pts',(16.511861777281,-17.6781647960941,-19.4329157456624));
#52350=CARTESIAN_POINT('Ctrl Pts',(16.5545193804023,-17.6064950352306,-19.4370593814876));
#52351=CARTESIAN_POINT('Ctrl Pts',(16.6004918491533,-17.5371703387789,-19.4412030173129));
#52352=CARTESIAN_POINT('Ctrl Pts',(16.6465392454185,-17.4677326545476,-19.4453534065787));
#52353=CARTESIAN_POINT('Ctrl Pts',(16.6959120078393,-17.4006480348314,-19.4495037958445));
#52354=CARTESIAN_POINT('Ctrl Pts',(16.7483230702929,-17.3362379102018,-19.4536541851102));
#52355=CARTESIAN_POINT('Ctrl Pts',(16.7661884610673,-17.3142823917967,-19.4550689308266));
#52356=CARTESIAN_POINT('Ctrl Pts',(16.7844065661398,-17.292637312599,-19.4564836765431));
#52357=CARTESIAN_POINT('Ctrl Pts',(16.8029650799467,-17.2713143846827,-19.4578984222595));
#52358=CARTESIAN_POINT('Ctrl Pts',(16.857858757406,-17.2082439287342,-19.4620830566462));
#52359=CARTESIAN_POINT('Ctrl Pts',(16.9159478005841,-17.1477482923964,-19.466267691033));
#52360=CARTESIAN_POINT('Ctrl Pts',(16.9769612646036,-17.0901689436695,-19.4704523254198));
#52361=CARTESIAN_POINT('Ctrl Pts',(17.0378878835037,-17.0326715520237,-19.4746310034971));
#52362=CARTESIAN_POINT('Ctrl Pts',(17.1017303233984,-16.9780825158866,-19.4788096815744));
#52363=CARTESIAN_POINT('Ctrl Pts',(17.1681782563647,-16.9267093376113,-19.4829883596517));
#52364=CARTESIAN_POINT('Ctrl Pts',(17.2358172209073,-16.8744153319337,-19.4872419375387));
#52365=CARTESIAN_POINT('Ctrl Pts',(17.306155687672,-16.8254539702902,-19.4914955154258));
#52366=CARTESIAN_POINT('Ctrl Pts',(17.3788280009098,-16.780109382846,-19.4957490933128));
#52367=CARTESIAN_POINT('Ctrl Pts',(17.4500914193922,-16.7356438888086,-19.4999202072833));
#52368=CARTESIAN_POINT('Ctrl Pts',(17.5235985912761,-16.6946564386902,-19.5040913212538));
#52369=CARTESIAN_POINT('Ctrl Pts',(17.5989738385239,-16.657372445741,-19.5082624352243));
#52370=CARTESIAN_POINT('Ctrl Pts',(17.6743237928742,-16.6201009637983,-19.5124321495369));
#52371=CARTESIAN_POINT('Ctrl Pts',(17.7515401656506,-16.5865306747361,-19.5166018638495));
#52372=CARTESIAN_POINT('Ctrl Pts',(17.8302229081151,-16.556840930505,-19.5207715781621));
#52373=CARTESIAN_POINT('Ctrl Pts',(17.9089028507045,-16.5271522427645,-19.5249411440981));
#52374=CARTESIAN_POINT('Ctrl Pts',(17.9890486285235,-16.5013439869149,-19.5291107100341));
#52375=CARTESIAN_POINT('Ctrl Pts',(18.0702417419427,-16.4795467699346,-19.53328027597));
#52376=CARTESIAN_POINT('Ctrl Pts',(18.1542895053979,-16.4569831896063,-19.5375964387176));
#52377=CARTESIAN_POINT('Ctrl Pts',(18.2394591140171,-16.4387180891091,-19.5419126014652));
#52378=CARTESIAN_POINT('Ctrl Pts',(18.3252730114503,-16.4248390932054,-19.5462287642128));
#52379=CARTESIAN_POINT('Ctrl Pts',(18.408291529862,-16.4114122041881,-19.5504043283958));
#52380=CARTESIAN_POINT('Ctrl Pts',(18.4919125329016,-16.402090058559,-19.5545798925788));
#52381=CARTESIAN_POINT('Ctrl Pts',(18.5756985998716,-16.3968990887408,-19.5587554567618));
#52382=CARTESIAN_POINT('Ctrl Pts',(18.6637165024314,-16.3914459353448,-19.5631419187917));
#52383=CARTESIAN_POINT('Ctrl Pts',(18.75191599805,-16.3905522627807,-19.5675283808215));
#52384=CARTESIAN_POINT('Ctrl Pts',(18.8397925195445,-16.3941868827437,-19.5719148428514));
#52385=CARTESIAN_POINT('Ctrl Pts',(18.927669041039,-16.3978215027067,-19.5763013048812));
#52386=CARTESIAN_POINT('Ctrl Pts',(19.0152220177589,-16.4059842855989,-19.580687766911));
#52387=CARTESIAN_POINT('Ctrl Pts',(19.1019580505821,-16.4185819782334,-19.5850742289409));
#52388=CARTESIAN_POINT('Ctrl Pts',(19.1847019893314,-16.4305998521642,-19.5892588006086));
#52389=CARTESIAN_POINT('Ctrl Pts',(19.267010516095,-16.4466981015606,-19.5934433722764));
#52390=CARTESIAN_POINT('Ctrl Pts',(19.3484498725052,-16.4668337371157,-19.5976279439441));
#52391=CARTESIAN_POINT('Ctrl Pts',(19.433563152438,-16.4878777391949,-19.602001291616));
#52392=CARTESIAN_POINT('Ctrl Pts',(19.5177264872397,-16.5133320197713,-19.6063746392878));
#52393=CARTESIAN_POINT('Ctrl Pts',(19.6004511653704,-16.5430868886512,-19.6107479869597));
#52394=CARTESIAN_POINT('Ctrl Pts',(19.6793978237086,-16.571482858517,-19.6149216047029));
#52395=CARTESIAN_POINT('Ctrl Pts',(19.7570338500724,-16.6037950595409,-19.619095222446));
#52396=CARTESIAN_POINT('Ctrl Pts',(19.8329471640918,-16.6398764889101,-19.6232688401892));
#52397=CARTESIAN_POINT('Ctrl Pts',(19.9088089339765,-16.6759334194668,-19.6274396241012));
#52398=CARTESIAN_POINT('Ctrl Pts',(19.9829499008247,-16.7157542975669,-19.6316104080133));
#52399=CARTESIAN_POINT('Ctrl Pts',(20.0549778822146,-16.7591440004643,-19.6357811919253));
#52400=CARTESIAN_POINT('Ctrl Pts',(20.1269801310666,-16.8025182020641,-19.6399504857934));
#52401=CARTESIAN_POINT('Ctrl Pts',(20.1968705010822,-16.849458457535,-19.6441197796615));
#52402=CARTESIAN_POINT('Ctrl Pts',(20.2642825299598,-16.8997243414931,-19.6482890735296));
#52403=CARTESIAN_POINT('Ctrl Pts',(20.2740863758758,-16.9070345944162,-19.6488954210219));
#52404=CARTESIAN_POINT('Ctrl Pts',(20.2838378536473,-16.9144151106639,-19.6495017685142));
#52405=CARTESIAN_POINT('Ctrl Pts',(20.293535888361,-16.9218650751947,-19.6501081160065));
#52406=CARTESIAN_POINT('Ctrl Pts',(20.293535888361,-16.9218650751948,-18.8501886412182));
#52407=CARTESIAN_POINT('Ctrl Pts',(20.3600880992579,-16.9729900324945,-18.8543616964033));
#52408=CARTESIAN_POINT('Ctrl Pts',(20.4241919589121,-17.0274434638868,-18.8585347515884));
#52409=CARTESIAN_POINT('Ctrl Pts',(20.4855007810524,-17.0849582184716,-18.8627078067735));
#52410=CARTESIAN_POINT('Ctrl Pts',(20.5467748089402,-17.1424403320298,-18.866878493648));
#52411=CARTESIAN_POINT('Ctrl Pts',(20.6052566139188,-17.2029800053482,-18.8710491805225));
#52412=CARTESIAN_POINT('Ctrl Pts',(20.6606332981064,-17.2662704443987,-18.8752198673969));
#52413=CARTESIAN_POINT('Ctrl Pts',(20.7159951665402,-17.3295439504101,-18.8793894384251));
#52414=CARTESIAN_POINT('Ctrl Pts',(20.7682532615728,-17.3955664142886,-18.8835590094532));
#52415=CARTESIAN_POINT('Ctrl Pts',(20.8171331656151,-17.4639958957334,-18.8877285804813));
#52416=CARTESIAN_POINT('Ctrl Pts',(20.8660146547938,-17.5324275962917,-18.8918982867253));
#52417=CARTESIAN_POINT('Ctrl Pts',(20.9115174691059,-17.6032660943068,-18.8960679929693));
#52418=CARTESIAN_POINT('Ctrl Pts',(20.9534097498297,-17.6761393640524,-18.9002376992133));
#52419=CARTESIAN_POINT('Ctrl Pts',(20.995344766866,-17.7490869752939,-18.9044116591734));
#52420=CARTESIAN_POINT('Ctrl Pts',(21.033661663671,-17.8240731045976,-18.9085856191335));
#52421=CARTESIAN_POINT('Ctrl Pts',(21.068174170418,-17.9007003556771,-18.9127595790936));
#52422=CARTESIAN_POINT('Ctrl Pts',(21.1027039969298,-17.9773660613949,-18.9169356337148));
#52423=CARTESIAN_POINT('Ctrl Pts',(21.1334254624243,-18.055674100626,-18.9211116883359));
#52424=CARTESIAN_POINT('Ctrl Pts',(21.1602010986746,-18.1352085769364,-18.9252877429571));
#52425=CARTESIAN_POINT('Ctrl Pts',(21.1870245435949,-18.2148850643459,-18.9294712540441));
#52426=CARTESIAN_POINT('Ctrl Pts',(21.2098879571468,-18.295791920553,-18.9336547651311));
#52427=CARTESIAN_POINT('Ctrl Pts',(21.2287042787308,-18.377499728736,-18.9378382762182));
#52428=CARTESIAN_POINT('Ctrl Pts',(21.2457310808275,-18.4514367452501,-18.94162391599));
#52429=CARTESIAN_POINT('Ctrl Pts',(21.2594446082458,-18.5260292265647,-18.9454095557619));
#52430=CARTESIAN_POINT('Ctrl Pts',(21.2698170137415,-18.6009557395155,-18.9491951955337));
#52431=CARTESIAN_POINT('Ctrl Pts',(21.2812826384042,-18.6837792730856,-18.9533798299225));
#52432=CARTESIAN_POINT('Ctrl Pts',(21.2887076244828,-18.7673192548721,-18.9575644643113));
#52433=CARTESIAN_POINT('Ctrl Pts',(21.2920126435715,-18.851147060883,-18.9617490987001));
#52434=CARTESIAN_POINT('Ctrl Pts',(21.2953129583745,-18.934855548388,-18.9659277767799));
#52435=CARTESIAN_POINT('Ctrl Pts',(21.294504936491,-19.0188505906155,-18.9701064548596));
#52436=CARTESIAN_POINT('Ctrl Pts',(21.2895607321101,-19.1026961993451,-18.9742851329393));
#52437=CARTESIAN_POINT('Ctrl Pts',(21.2845279064127,-19.1880446804597,-18.9785387108258));
#52438=CARTESIAN_POINT('Ctrl Pts',(21.2752090914542,-19.2732378406073,-18.9827922887123));
#52439=CARTESIAN_POINT('Ctrl Pts',(21.2616304174303,-19.3578133473421,-18.9870458665988));
#52440=CARTESIAN_POINT('Ctrl Pts',(21.2483149925156,-19.4407491927399,-18.9912169805726));
#52441=CARTESIAN_POINT('Ctrl Pts',(21.2309034822292,-19.5230906447102,-18.9953880945464));
#52442=CARTESIAN_POINT('Ctrl Pts',(21.2094728610011,-19.6044064028251,-18.9995592085202));
#52443=CARTESIAN_POINT('Ctrl Pts',(21.1880494310247,-19.6856948746526,-19.0037289228364));
#52444=CARTESIAN_POINT('Ctrl Pts',(21.1626096856898,-19.7659578917013,-19.0078986371526));
#52445=CARTESIAN_POINT('Ctrl Pts',(21.1332813336496,-19.8447760536666,-19.0120683514689));
#52446=CARTESIAN_POINT('Ctrl Pts',(21.1039540252378,-19.9235914109442,-19.0162379174088));
#52447=CARTESIAN_POINT('Ctrl Pts',(21.0707385464732,-20.0009615845084,-19.0204074833488));
#52448=CARTESIAN_POINT('Ctrl Pts',(21.0338114728018,-20.0764852998459,-19.0245770492887));
#52449=CARTESIAN_POINT('Ctrl Pts',(20.9955860886931,-20.1546643360123,-19.0288932120326));
#52450=CARTESIAN_POINT('Ctrl Pts',(20.9533834858384,-20.2308641813314,-19.0332093747765));
#52451=CARTESIAN_POINT('Ctrl Pts',(20.9074514472649,-20.3046672933068,-19.0375255375203));
#52452=CARTESIAN_POINT('Ctrl Pts',(20.8630156401099,-20.3760662765228,-19.041701101708));
#52453=CARTESIAN_POINT('Ctrl Pts',(20.815089945817,-20.4452219153955,-19.0458766658958));
#52454=CARTESIAN_POINT('Ctrl Pts',(20.7639418957712,-20.5117871328463,-19.0500522300835));
#52455=CARTESIAN_POINT('Ctrl Pts',(20.7102104791443,-20.5817144014031,-19.0544386921054));
#52456=CARTESIAN_POINT('Ctrl Pts',(20.6529230087043,-20.6487822429891,-19.0588251541274));
#52457=CARTESIAN_POINT('Ctrl Pts',(20.5924345734849,-20.7126308346942,-19.0632116161493));
#52458=CARTESIAN_POINT('Ctrl Pts',(20.5319461382654,-20.7764794263994,-19.0675980781712));
#52459=CARTESIAN_POINT('Ctrl Pts',(20.4682572109593,-20.837108423261,-19.0719845401932));
#52460=CARTESIAN_POINT('Ctrl Pts',(20.4017623229462,-20.8942072068039,-19.0763710022151));
#52461=CARTESIAN_POINT('Ctrl Pts',(20.3383269634742,-20.9486787905254,-19.0805556366056));
#52462=CARTESIAN_POINT('Ctrl Pts',(20.2721020634022,-21.0001406364731,-19.0847402709961));
#52463=CARTESIAN_POINT('Ctrl Pts',(20.2034050887149,-21.0482940359737,-19.0889249053866));
#52464=CARTESIAN_POINT('Ctrl Pts',(20.1348058956689,-21.0963788950696,-19.093103583468));
#52465=CARTESIAN_POINT('Ctrl Pts',(20.0637419907205,-21.141164399806,-19.0972822615493));
#52466=CARTESIAN_POINT('Ctrl Pts',(19.990564898557,-21.1823911441078,-19.1014609396307));
#52467=CARTESIAN_POINT('Ctrl Pts',(19.9160761595504,-21.2243568482045,-19.1057145175168));
#52468=CARTESIAN_POINT('Ctrl Pts',(19.8393980962008,-21.2626346413139,-19.1099680954028));
#52469=CARTESIAN_POINT('Ctrl Pts',(19.7609336007081,-21.2969962430112,-19.1142216732889));
#52470=CARTESIAN_POINT('Ctrl Pts',(19.683990292633,-21.3306916779815,-19.1183927872642));
#52471=CARTESIAN_POINT('Ctrl Pts',(19.6053296420408,-21.360621219484,-19.1225639012394));
#52472=CARTESIAN_POINT('Ctrl Pts',(19.5253559691356,-21.3866161360907,-19.1267350152147));
#52473=CARTESIAN_POINT('Ctrl Pts',(19.4454091321695,-21.412602329852,-19.1309047295323));
#52474=CARTESIAN_POINT('Ctrl Pts',(19.3641505850609,-21.4346563787685,-19.1350744438499));
#52475=CARTESIAN_POINT('Ctrl Pts',(19.2820021033665,-21.4526586521766,-19.1392441581676));
#52476=CARTESIAN_POINT('Ctrl Pts',(19.1998565448683,-21.4706602849865,-19.1434137241088));
#52477=CARTESIAN_POINT('Ctrl Pts',(19.1168215642993,-21.4846103313103,-19.1475832900501));
#52478=CARTESIAN_POINT('Ctrl Pts',(19.0333301469624,-21.4944400608706,-19.1517528559914));
#52479=CARTESIAN_POINT('Ctrl Pts',(18.9469032742685,-21.5046153916102,-19.1560690187335));
#52480=CARTESIAN_POINT('Ctrl Pts',(18.8599877947896,-21.5103752123296,-19.1603851814756));
#52481=CARTESIAN_POINT('Ctrl Pts',(18.7730689159398,-21.511701861508,-19.1647013442177));
#52482=CARTESIAN_POINT('Ctrl Pts',(18.688981410545,-21.512985295227,-19.1688769084066));
#52483=CARTESIAN_POINT('Ctrl Pts',(18.6048911930078,-21.510120006403,-19.1730524725954));
#52484=CARTESIAN_POINT('Ctrl Pts',(18.5212349098899,-21.5031430803525,-19.1772280367843));
#52485=CARTESIAN_POINT('Ctrl Pts',(18.4333533466026,-21.495813766338,-19.181614498803));
#52486=CARTESIAN_POINT('Ctrl Pts',(18.3459512843982,-21.4839466202446,-19.1860009608217));
#52487=CARTESIAN_POINT('Ctrl Pts',(18.2595234803591,-21.467645450438,-19.1903874228405));
#52488=CARTESIAN_POINT('Ctrl Pts',(18.1730956763199,-21.4513442806314,-19.1947738848592));
#52489=CARTESIAN_POINT('Ctrl Pts',(18.0876426763647,-21.4306092978499,-19.1991603468779));
#52490=CARTESIAN_POINT('Ctrl Pts',(18.0036392138265,-21.4056041086573,-19.2035468088966));
#52491=CARTESIAN_POINT('Ctrl Pts',(17.9235008748327,-21.3817494451997,-19.2077314433107));
#52492=CARTESIAN_POINT('Ctrl Pts',(17.8443833236107,-21.3539201055369,-19.2119160777248));
#52493=CARTESIAN_POINT('Ctrl Pts',(17.7667095652025,-21.3222213429866,-19.2161007121389));
#52494=CARTESIAN_POINT('Ctrl Pts',(17.6891463657735,-21.2905676997005,-19.2202793902439));
#52495=CARTESIAN_POINT('Ctrl Pts',(17.6130232994484,-21.2550557457776,-19.224458068349));
#52496=CARTESIAN_POINT('Ctrl Pts',(17.5387487593335,-21.2158406462658,-19.228636746454));
#52497=CARTESIAN_POINT('Ctrl Pts',(17.4631429019428,-21.1759226445297,-19.2328903243342));
#52498=CARTESIAN_POINT('Ctrl Pts',(17.3894529543292,-21.1321675712374,-19.2371439022144));
#52499=CARTESIAN_POINT('Ctrl Pts',(17.3180889421044,-21.0847906311049,-19.2413974800945));
#52500=CARTESIAN_POINT('Ctrl Pts',(17.2481084600712,-21.0383321851128,-19.2455685940936));
#52501=CARTESIAN_POINT('Ctrl Pts',(17.1803649335769,-20.9883913190988,-19.2497397080926));
#52502=CARTESIAN_POINT('Ctrl Pts',(17.1152190899104,-20.9352166712514,-19.2539108220917));
#52503=CARTESIAN_POINT('Ctrl Pts',(17.0500951065615,-20.882059866671,-19.2580805364331));
#52504=CARTESIAN_POINT('Ctrl Pts',(16.987567430963,-20.8256717259896,-19.2622502507746));
#52505=CARTESIAN_POINT('Ctrl Pts',(16.9279649526829,-20.7663421418967,-19.266419965116));
#52506=CARTESIAN_POINT('Ctrl Pts',(16.8683645953157,-20.707014669006,-19.270589531081));
#52507=CARTESIAN_POINT('Ctrl Pts',(16.8116895537436,-20.6447462859623,-19.2747590970461));
#52508=CARTESIAN_POINT('Ctrl Pts',(16.7582319859876,-20.5798638624914,-19.2789286630111));
#52509=CARTESIAN_POINT('Ctrl Pts',(16.7028949166956,-20.5127002537798,-19.283244825725));
#52510=CARTESIAN_POINT('Ctrl Pts',(16.6510061189315,-20.4427357723036,-19.2875609884389));
#52511=CARTESIAN_POINT('Ctrl Pts',(16.6028430768027,-20.370368840855,-19.2918771511528));
#52512=CARTESIAN_POINT('Ctrl Pts',(16.5562489402056,-20.3003592538356,-19.2960527153651));
#52513=CARTESIAN_POINT('Ctrl Pts',(16.5131417547233,-20.2281017614849,-19.3002282795774));
#52514=CARTESIAN_POINT('Ctrl Pts',(16.4737266859787,-20.1539835880423,-19.3044038437897));
#52515=CARTESIAN_POINT('Ctrl Pts',(16.4323208564678,-20.0761218830912,-19.3087903057544));
#52516=CARTESIAN_POINT('Ctrl Pts',(16.3949901703475,-19.9962071202823,-19.3131767677191));
#52517=CARTESIAN_POINT('Ctrl Pts',(16.3619151438293,-19.9147115015028,-19.3175632296838));
#52518=CARTESIAN_POINT('Ctrl Pts',(16.3288401173112,-19.8332158827234,-19.3219496916486));
#52519=CARTESIAN_POINT('Ctrl Pts',(16.3000208686933,-19.7501399810729,-19.3263361536133));
#52520=CARTESIAN_POINT('Ctrl Pts',(16.2755767948947,-19.6659715292643,-19.330722615578));
#52521=CARTESIAN_POINT('Ctrl Pts',(16.2465257453528,-19.5659398453678,-19.3359357942364));
#52522=CARTESIAN_POINT('Ctrl Pts',(16.2235642356486,-19.464065347825,-19.3411489728948));
#52523=CARTESIAN_POINT('Ctrl Pts',(16.2068848499427,-19.3610098022674,-19.3463621515532));
#52524=CARTESIAN_POINT('Ctrl Pts',(16.1904712789856,-19.2595966243872,-19.3514922492277));
#52525=CARTESIAN_POINT('Ctrl Pts',(16.1801412137013,-19.1570396545395,-19.3566223469021));
#52526=CARTESIAN_POINT('Ctrl Pts',(16.1760324691903,-19.0539907413612,-19.3617524445766));
#52527=CARTESIAN_POINT('Ctrl Pts',(16.1747089805837,-19.0207971314519,-19.363404926449));
#52528=CARTESIAN_POINT('Ctrl Pts',(16.1740306434087,-18.9875526505075,-19.3650574083215));
#52529=CARTESIAN_POINT('Ctrl Pts',(16.1740010149447,-18.9542795868247,-19.3667098901939));
#52530=CARTESIAN_POINT('Origin',(18.734,-18.952,1.76670989022851));
#52531=CARTESIAN_POINT('',(20.293535888361,-16.9218650751948,-18.0500683203253));
#52532=CARTESIAN_POINT('',(20.293535888361,-16.9218650751948,-18.1167065567592));
#52533=CARTESIAN_POINT('',(20.293535888361,-16.9218650751948,1.76670989022851));
#52534=CARTESIAN_POINT('',(16.1743944468539,-18.9516176052701,-18.6332901348849));
#52535=CARTESIAN_POINT('Ctrl Pts',(20.293535888361,-16.9218650751948,-18.1167065567592));
#52536=CARTESIAN_POINT('Ctrl Pts',(20.3602206256079,-16.9730918383383,-18.1208760361824));
#52537=CARTESIAN_POINT('Ctrl Pts',(20.4243870824807,-17.0276141077345,-18.1250455156056));
#52538=CARTESIAN_POINT('Ctrl Pts',(20.4857019893154,-17.0851469954417,-18.1292149950289));
#52539=CARTESIAN_POINT('Ctrl Pts',(20.5470276420194,-17.1426899661927,-18.1333852051827));
#52540=CARTESIAN_POINT('Ctrl Pts',(20.6055004178084,-17.2032442872454,-18.1375554153366));
#52541=CARTESIAN_POINT('Ctrl Pts',(20.6608233620813,-17.2664876946941,-18.1417256254905));
#52542=CARTESIAN_POINT('Ctrl Pts',(20.7162074135451,-17.3298009579145,-18.1459004418675));
#52543=CARTESIAN_POINT('Ctrl Pts',(20.7684343867049,-17.3958088885422,-18.1500752582446));
#52544=CARTESIAN_POINT('Ctrl Pts',(20.8172475188104,-17.464155997636,-18.1542500746216));
#52545=CARTESIAN_POINT('Ctrl Pts',(20.8660913992488,-17.5325461598914,-18.158427520796));
#52546=CARTESIAN_POINT('Ctrl Pts',(20.9115169101421,-17.60327804657,-18.1626049669703));
#52547=CARTESIAN_POINT('Ctrl Pts',(20.953311845506,-17.6759690707523,-18.1667824131447));
#52548=CARTESIAN_POINT('Ctrl Pts',(20.995175289534,-17.7487792472892,-18.1709667068295));
#52549=CARTESIAN_POINT('Ctrl Pts',(21.0333960713853,-17.82355456178,-18.1751510005143));
#52550=CARTESIAN_POINT('Ctrl Pts',(21.0678091437387,-17.8998902715962,-18.1793352941991));
#52551=CARTESIAN_POINT('Ctrl Pts',(21.0825869345977,-17.9326706389858,-18.1811321293184));
#52552=CARTESIAN_POINT('Ctrl Pts',(21.0966631843942,-17.9657385349447,-18.1829289644377));
#52553=CARTESIAN_POINT('Ctrl Pts',(21.1100276507034,-17.9990610706384,-18.184725799557));
#52554=CARTESIAN_POINT('Ctrl Pts',(21.1411520453503,-18.0766656473997,-18.1889104339505));
#52555=CARTESIAN_POINT('Ctrl Pts',(21.1685283427045,-18.1559410996702,-18.193095068344));
#52556=CARTESIAN_POINT('Ctrl Pts',(21.1919760688458,-18.2364906394873,-18.1972797027375));
#52557=CARTESIAN_POINT('Ctrl Pts',(21.2153904200512,-18.3169255270045,-18.2014583808218));
#52558=CARTESIAN_POINT('Ctrl Pts',(21.2348871797097,-18.3986304619535,-18.2056370589062));
#52559=CARTESIAN_POINT('Ctrl Pts',(21.2503340551361,-18.4811890793937,-18.2098157369906));
#52560=CARTESIAN_POINT('Ctrl Pts',(21.2660578047011,-18.5652275007066,-18.2140693148759));
#52561=CARTESIAN_POINT('Ctrl Pts',(21.2775848741471,-18.6501500625618,-18.2183228927613));
#52562=CARTESIAN_POINT('Ctrl Pts',(21.2848289888802,-18.7355018025751,-18.2225764706466));
#52563=CARTESIAN_POINT('Ctrl Pts',(21.2919326623144,-18.819198832569,-18.226747584625));
#52564=CARTESIAN_POINT('Ctrl Pts',(21.2949179252555,-18.9033080688148,-18.2309186986034));
#52565=CARTESIAN_POINT('Ctrl Pts',(21.2937553357682,-18.9873923862785,-18.2350898125818));
#52566=CARTESIAN_POINT('Ctrl Pts',(21.2925931363989,-19.0714484884373,-18.2392595269026));
#52567=CARTESIAN_POINT('Ctrl Pts',(21.287285855196,-19.1554792288145,-18.2434292412234));
#52568=CARTESIAN_POINT('Ctrl Pts',(21.2778561566697,-19.2390467804623,-18.2475989555442));
#52569=CARTESIAN_POINT('Ctrl Pts',(21.2684267936925,-19.3226113584179,-18.2517685214887));
#52570=CARTESIAN_POINT('Ctrl Pts',(21.2548753574853,-19.4057123233788,-18.2559380874332));
#52571=CARTESIAN_POINT('Ctrl Pts',(21.2372763100333,-19.4879176388457,-18.2601076533776));
#52572=CARTESIAN_POINT('Ctrl Pts',(21.2190585017878,-19.5730131917741,-18.264423816116));
#52573=CARTESIAN_POINT('Ctrl Pts',(21.1965032689152,-19.6571484255578,-18.2687399788544));
#52574=CARTESIAN_POINT('Ctrl Pts',(21.1697502461668,-19.7398583237475,-18.2730561415928));
#52575=CARTESIAN_POINT('Ctrl Pts',(21.1438687003148,-19.819873955721,-18.2772317057849));
#52576=CARTESIAN_POINT('Ctrl Pts',(21.1140588617648,-19.8985552629124,-18.281407269977));
#52577=CARTESIAN_POINT('Ctrl Pts',(21.0804965434243,-19.9755008410831,-18.2855828341691));
#52578=CARTESIAN_POINT('Ctrl Pts',(21.0452390721828,-20.0563327574599,-18.2899692961807));
#52579=CARTESIAN_POINT('Ctrl Pts',(21.0058403441651,-20.1352484709672,-18.2943557581922));
#52580=CARTESIAN_POINT('Ctrl Pts',(20.9625580617869,-20.2118130675798,-18.2987422202038));
#52581=CARTESIAN_POINT('Ctrl Pts',(20.9192757794087,-20.2883776641924,-18.3031286822153));
#52582=CARTESIAN_POINT('Ctrl Pts',(20.8721103180846,-20.3625906950211,-18.3075151442269));
#52583=CARTESIAN_POINT('Ctrl Pts',(20.8213695361433,-20.4340554711552,-18.3119016062384));
#52584=CARTESIAN_POINT('Ctrl Pts',(20.7729634127897,-20.5022320470106,-18.3160862406309));
#52585=CARTESIAN_POINT('Ctrl Pts',(20.7211235735796,-20.5681614794158,-18.3202708750235));
#52586=CARTESIAN_POINT('Ctrl Pts',(20.6660859672863,-20.6314772445661,-18.324455509416));
#52587=CARTESIAN_POINT('Ctrl Pts',(20.6111267002133,-20.6947028875616,-18.3286341874995));
#52588=CARTESIAN_POINT('Ctrl Pts',(20.5529790062393,-20.7553219086264,-18.3328128655829));
#52589=CARTESIAN_POINT('Ctrl Pts',(20.4919213748666,-20.8129977001026,-18.3369915436664));
#52590=CARTESIAN_POINT('Ctrl Pts',(20.4297693293237,-20.8717072886989,-18.3412451215519));
#52591=CARTESIAN_POINT('Ctrl Pts',(20.3646022781503,-20.9273667019604,-18.3454986994375));
#52592=CARTESIAN_POINT('Ctrl Pts',(20.2967560739107,-20.9796571340972,-18.3497522773231));
#52593=CARTESIAN_POINT('Ctrl Pts',(20.2302252007411,-21.0309338141631,-18.3539233913005));
#52594=CARTESIAN_POINT('Ctrl Pts',(20.1611185098595,-21.0789706821842,-18.358094505278));
#52595=CARTESIAN_POINT('Ctrl Pts',(20.0897876178816,-21.1235063746623,-18.3622656192554));
#52596=CARTESIAN_POINT('Ctrl Pts',(20.0184806616733,-21.1680271227587,-18.3664353335753));
#52597=CARTESIAN_POINT('Ctrl Pts',(19.9449513765315,-21.2090487851565,-18.3706050478952));
#52598=CARTESIAN_POINT('Ctrl Pts',(19.8695801735013,-21.2463534316994,-18.3747747622151));
#52599=CARTESIAN_POINT('Ctrl Pts',(19.7942116525019,-21.2836567507829,-18.3789443281586));
#52600=CARTESIAN_POINT('Ctrl Pts',(19.7170017566051,-21.3172431136927,-18.3831138941022));
#52601=CARTESIAN_POINT('Ctrl Pts',(19.6383540649958,-21.346941278012,-18.3872834600458));
#52602=CARTESIAN_POINT('Ctrl Pts',(19.5569412175515,-21.3776835931598,-18.3915996227853));
#52603=CARTESIAN_POINT('Ctrl Pts',(19.473988080848,-21.4042590180671,-18.3959157855248));
#52604=CARTESIAN_POINT('Ctrl Pts',(19.3899612417722,-21.4265332588779,-18.4002319482643));
#52605=CARTESIAN_POINT('Ctrl Pts',(19.3086715681612,-21.4480819186317,-18.4044075124555));
#52606=CARTESIAN_POINT('Ctrl Pts',(19.2263775401996,-21.4656052611968,-18.4085830766467));
#52607=CARTESIAN_POINT('Ctrl Pts',(19.1435118395205,-21.4790338449045,-18.4127586408379));
#52608=CARTESIAN_POINT('Ctrl Pts',(19.0564607892627,-21.4931406744569,-18.4171451028516));
#52609=CARTESIAN_POINT('Ctrl Pts',(18.9687793786242,-21.5027281581545,-18.4215315648652));
#52610=CARTESIAN_POINT('Ctrl Pts',(18.8809727909042,-21.5077775722339,-18.4259180268789));
#52611=CARTESIAN_POINT('Ctrl Pts',(18.7931662031843,-21.5128269863133,-18.4303044888925));
#52612=CARTESIAN_POINT('Ctrl Pts',(18.7052350190324,-21.5133384034635,-18.4346909509062));
#52613=CARTESIAN_POINT('Ctrl Pts',(18.6176794289205,-21.5093559636358,-18.4390774129198));
#52614=CARTESIAN_POINT('Ctrl Pts',(18.5341524013308,-21.5055567617695,-18.4432620473123));
#52615=CARTESIAN_POINT('Ctrl Pts',(18.4506562604967,-21.4976540121365,-18.4474466817048));
#52616=CARTESIAN_POINT('Ctrl Pts',(18.3676269095303,-21.4856477179315,-18.4516313160972));
#52617=CARTESIAN_POINT('Ctrl Pts',(18.2847157405683,-21.4736585132003,-18.4558099941806));
#52618=CARTESIAN_POINT('Ctrl Pts',(18.2022704931348,-21.4575774310126,-18.4599886722639));
#52619=CARTESIAN_POINT('Ctrl Pts',(18.1207249420861,-21.4374564376268,-18.4641673503473));
#52620=CARTESIAN_POINT('Ctrl Pts',(18.0377177456259,-21.4169747898918,-18.4684209282329));
#52621=CARTESIAN_POINT('Ctrl Pts',(17.9556432985576,-21.3923069974989,-18.4726745061184));
#52622=CARTESIAN_POINT('Ctrl Pts',(17.8749514567215,-21.3635628957776,-18.476928084004));
#52623=CARTESIAN_POINT('Ctrl Pts',(17.7958239837108,-21.3353760545626,-18.4810991979814));
#52624=CARTESIAN_POINT('Ctrl Pts',(17.7180264386448,-21.3032697094722,-18.4852703119587));
#52625=CARTESIAN_POINT('Ctrl Pts',(17.6419689102691,-21.267398043331,-18.4894414259361));
#52626=CARTESIAN_POINT('Ctrl Pts',(17.5659369037317,-21.2315384142739,-18.4936111402558));
#52627=CARTESIAN_POINT('Ctrl Pts',(17.4916441700223,-21.1919161695519,-18.4977808545756));
#52628=CARTESIAN_POINT('Ctrl Pts',(17.4194798631977,-21.1487332131921,-18.5019505688954));
#52629=CARTESIAN_POINT('Ctrl Pts',(17.347318124289,-21.1055517934674,-18.5061201348388));
#52630=CARTESIAN_POINT('Ctrl Pts',(17.2772850559936,-21.0588101509788,-18.5102897007822));
#52631=CARTESIAN_POINT('Ctrl Pts',(17.2097430958425,-21.0087549416807,-18.5144592667256));
#52632=CARTESIAN_POINT('Ctrl Pts',(17.1398264436723,-20.9569398529571,-18.5187754294653));
#52633=CARTESIAN_POINT('Ctrl Pts',(17.0725797574076,-20.9015741660664,-18.5230915922049));
#52634=CARTESIAN_POINT('Ctrl Pts',(17.0083685115613,-20.8429775160242,-18.5274077549445));
#52635=CARTESIAN_POINT('Ctrl Pts',(16.9462489403141,-20.7862896457115,-18.5315833191356));
#52636=CARTESIAN_POINT('Ctrl Pts',(16.886970385841,-20.7265784444844,-18.5357588833267));
#52637=CARTESIAN_POINT('Ctrl Pts',(16.8308254399578,-20.6641701416647,-18.5399344475178));
#52638=CARTESIAN_POINT('Ctrl Pts',(16.7718447463027,-20.598609743801,-18.5443209095317));
#52639=CARTESIAN_POINT('Ctrl Pts',(16.7163229051915,-20.5300730764182,-18.5487073715456));
#52640=CARTESIAN_POINT('Ctrl Pts',(16.6645491064847,-20.4589747839061,-18.5530938335595));
#52641=CARTESIAN_POINT('Ctrl Pts',(16.6127753077778,-20.3878764913939,-18.5574802955735));
#52642=CARTESIAN_POINT('Ctrl Pts',(16.5647498046499,-20.3142171013321,-18.5618667575874));
#52643=CARTESIAN_POINT('Ctrl Pts',(16.5207062260026,-20.2384410868689,-18.5662532196013));
#52644=CARTESIAN_POINT('Ctrl Pts',(16.4770273612297,-20.1632925546556,-18.5706033584189));
#52645=CARTESIAN_POINT('Ctrl Pts',(16.4371122169919,-20.0858014915384,-18.5749534972364));
#52646=CARTESIAN_POINT('Ctrl Pts',(16.4012086273382,-20.0063644586359,-18.579303636054));
#52647=CARTESIAN_POINT('Ctrl Pts',(16.3640774712897,-19.924211423433,-18.5838025088638));
#52648=CARTESIAN_POINT('Ctrl Pts',(16.3312374248383,-19.8399772763342,-18.5883013816736));
#52649=CARTESIAN_POINT('Ctrl Pts',(16.3029130373491,-19.7541322709061,-18.5928002544834));
#52650=CARTESIAN_POINT('Ctrl Pts',(16.2756354411693,-19.6714598603193,-18.5971328613515));
#52651=CARTESIAN_POINT('Ctrl Pts',(16.252545805577,-19.5872939815205,-18.6014654682196));
#52652=CARTESIAN_POINT('Ctrl Pts',(16.2337970621825,-19.5020775124732,-18.6057980750876));
#52653=CARTESIAN_POINT('Ctrl Pts',(16.2150725182341,-19.416971034336,-18.6101250897577));
#52654=CARTESIAN_POINT('Ctrl Pts',(16.2006778102741,-19.3308170607077,-18.6144521044277));
#52655=CARTESIAN_POINT('Ctrl Pts',(16.190716084581,-19.244073493441,-18.6187791190978));
#52656=CARTESIAN_POINT('Ctrl Pts',(16.180768168227,-19.1574501735471,-18.6231001354885));
#52657=CARTESIAN_POINT('Ctrl Pts',(16.1752410444518,-19.0702392928349,-18.6274211518792));
#52658=CARTESIAN_POINT('Ctrl Pts',(16.1741865858058,-18.9829076772249,-18.6317421682699));
#52659=CARTESIAN_POINT('Ctrl Pts',(16.1740606709629,-18.9724792486655,-18.6322581487704));
#52660=CARTESIAN_POINT('Ctrl Pts',(16.1739984722012,-18.9620491070313,-18.632774129271));
#52661=CARTESIAN_POINT('Ctrl Pts',(16.1740000284928,-18.9516180532909,-18.6332901097715));
#52662=CARTESIAN_POINT('Ctrl Pts',(16.178162963747,-18.9516133246024,-18.6332903748342));
#52663=CARTESIAN_POINT('Ctrl Pts',(16.1776269370726,-18.5470182282415,-18.6533365919837));
#52664=CARTESIAN_POINT('Ctrl Pts',(16.4590847030962,-17.2875284349863,-18.7157747446936));
#52665=CARTESIAN_POINT('Ctrl Pts',(18.2370603661219,-16.0736326739786,-18.8102032534018));
#52666=CARTESIAN_POINT('Ctrl Pts',(19.7793305886778,-16.5353973209162,-18.8845855449605));
#52667=CARTESIAN_POINT('Ctrl Pts',(20.2933494025375,-16.9221164381226,-18.9165759009586));
#52668=CARTESIAN_POINT('',(16.1740000028035,-18.9518801919504,-18.5667098901964));
#52669=CARTESIAN_POINT('Ctrl Pts',(16.1740000028035,-18.9518801913083,-18.5667098902285));
#52670=CARTESIAN_POINT('Ctrl Pts',(16.1740003013853,-18.945500276023,-18.5670291853155));
#52671=CARTESIAN_POINT('Ctrl Pts',(16.1740244495167,-18.9391204260769,-18.5673484804024));
#52672=CARTESIAN_POINT('Ctrl Pts',(16.1740724460423,-18.9327407557765,-18.5676677754894));
#52673=CARTESIAN_POINT('Ctrl Pts',(16.1747014814392,-18.8491297362399,-18.5718524098819));
#52674=CARTESIAN_POINT('Ctrl Pts',(16.1794322843349,-18.7653939703416,-18.5760370442745));
#52675=CARTESIAN_POINT('Ctrl Pts',(16.1882813814472,-18.6819690477863,-18.580221678667));
#52676=CARTESIAN_POINT('Ctrl Pts',(16.1971178829649,-18.5986628702823,-18.5844003567505));
#52677=CARTESIAN_POINT('Ctrl Pts',(16.2100609870472,-18.515667110836,-18.5885790348339));
#52678=CARTESIAN_POINT('Ctrl Pts',(16.2270752140172,-18.433417202922,-18.5927577129174));
#52679=CARTESIAN_POINT('Ctrl Pts',(16.2443944087803,-18.3496930245081,-18.5970112908029));
#52680=CARTESIAN_POINT('Ctrl Pts',(16.2659321081157,-18.2667421815311,-18.6012648686885));
#52681=CARTESIAN_POINT('Ctrl Pts',(16.2915956147072,-18.1850183713396,-18.605518446574));
#52682=CARTESIAN_POINT('Ctrl Pts',(16.3167615841415,-18.1048789366913,-18.6096895605515));
#52683=CARTESIAN_POINT('Ctrl Pts',(16.3458946705844,-18.0259198416596,-18.613860674529));
#52684=CARTESIAN_POINT('Ctrl Pts',(16.3788563531112,-17.9485567268056,-18.6180317885065));
#52685=CARTESIAN_POINT('Ctrl Pts',(16.411806975027,-17.8712195718919,-18.6222015028263));
#52686=CARTESIAN_POINT('Ctrl Pts',(16.4485834613785,-17.79547775642,-18.6263712171462));
#52687=CARTESIAN_POINT('Ctrl Pts',(16.4889988104968,-17.7217278109584,-18.6305409314661));
#52688=CARTESIAN_POINT('Ctrl Pts',(16.5294127214635,-17.6479804898363,-18.6347104974097));
#52689=CARTESIAN_POINT('Ctrl Pts',(16.5734650159172,-17.5762253008164,-18.6388800633533));
#52690=CARTESIAN_POINT('Ctrl Pts',(16.620922959331,-17.5068337741985,-18.6430496292968));
#52691=CARTESIAN_POINT('Ctrl Pts',(16.6700494655017,-17.4350025270905,-18.6473657920363));
#52692=CARTESIAN_POINT('Ctrl Pts',(16.7228252639786,-17.3657046830183,-18.6516819547758));
#52693=CARTESIAN_POINT('Ctrl Pts',(16.7789448088305,-17.2993175745228,-18.6559981175153));
#52694=CARTESIAN_POINT('Ctrl Pts',(16.8332362653982,-17.2350930191197,-18.6601736817066));
#52695=CARTESIAN_POINT('Ctrl Pts',(16.8906566126944,-17.1735927891267,-18.6643492458978));
#52696=CARTESIAN_POINT('Ctrl Pts',(16.9508909514351,-17.1151216368725,-18.668524810089));
#52697=CARTESIAN_POINT('Ctrl Pts',(17.0141675834549,-17.0536972456977,-18.6729112721026));
#52698=CARTESIAN_POINT('Ctrl Pts',(17.0805495076473,-16.9956163559342,-18.6772977341163));
#52699=CARTESIAN_POINT('Ctrl Pts',(17.1496333442479,-16.9411836731961,-18.6816841961299));
#52700=CARTESIAN_POINT('Ctrl Pts',(17.2187171808487,-16.886750990458,-18.6860706581436));
#52701=CARTESIAN_POINT('Ctrl Pts',(17.2905024122582,-16.835966787744,-18.6904571201572));
#52702=CARTESIAN_POINT('Ctrl Pts',(17.3645537444778,-16.7890813808106,-18.6948435821709));
#52703=CARTESIAN_POINT('Ctrl Pts',(17.4351978651041,-16.7443532409684,-18.6990282165633));
#52704=CARTESIAN_POINT('Ctrl Pts',(17.5081670866298,-16.703006515634,-18.7032128509558));
#52705=CARTESIAN_POINT('Ctrl Pts',(17.5831040926459,-16.665290877607,-18.7073974853483));
#52706=CARTESIAN_POINT('Ctrl Pts',(17.6579344351092,-16.6276289231224,-18.7115761634316));
#52707=CARTESIAN_POINT('Ctrl Pts',(17.734726591191,-16.5935879949174,-18.715754841515));
#52708=CARTESIAN_POINT('Ctrl Pts',(17.813095225772,-16.5633739520795,-18.7199335195984));
#52709=CARTESIAN_POINT('Ctrl Pts',(17.8928685618193,-16.532618344233,-18.7241870974839));
#52710=CARTESIAN_POINT('Ctrl Pts',(17.974275041662,-16.5058284229431,-18.7284406753695));
#52711=CARTESIAN_POINT('Ctrl Pts',(18.0568830023301,-16.4831718222066,-18.7326942532551));
#52712=CARTESIAN_POINT('Ctrl Pts',(18.13788944647,-16.4609544638901,-18.7368653672325));
#52713=CARTESIAN_POINT('Ctrl Pts',(18.2200507369796,-16.4427117186152,-18.7410364812098));
#52714=CARTESIAN_POINT('Ctrl Pts',(18.3029424071743,-16.428552090558,-18.7452075951871));
#52715=CARTESIAN_POINT('Ctrl Pts',(18.3858062622685,-16.4143972139007,-18.7493773095069));
#52716=CARTESIAN_POINT('Ctrl Pts',(18.4693995572162,-16.4043228107592,-18.7535470238267));
#52717=CARTESIAN_POINT('Ctrl Pts',(18.5532876521047,-16.3983862767995,-18.7577167381465));
#52718=CARTESIAN_POINT('Ctrl Pts',(18.6371727618947,-16.3924499540871,-18.7618863040899));
#52719=CARTESIAN_POINT('Ctrl Pts',(18.7213521918228,-16.3906512394234,-18.7660558700333));
#52720=CARTESIAN_POINT('Ctrl Pts',(18.8053875689175,-16.3929955422071,-18.7702254359768));
#52721=CARTESIAN_POINT('Ctrl Pts',(18.8923775262289,-16.3954222677854,-18.7745415987164));
#52722=CARTESIAN_POINT('Ctrl Pts',(18.9792125852183,-16.4022887536939,-18.778857761456));
#52723=CARTESIAN_POINT('Ctrl Pts',(19.0654100827152,-16.4135423271059,-18.7831739241957));
#52724=CARTESIAN_POINT('Ctrl Pts',(19.1487997057717,-16.4244293165444,-18.7873494883867));
#52725=CARTESIAN_POINT('Ctrl Pts',(19.2315922114996,-16.4394218336012,-18.7915250525778));
#52726=CARTESIAN_POINT('Ctrl Pts',(19.3133609024086,-16.4584200544678,-18.7957006167689));
#52727=CARTESIAN_POINT('Ctrl Pts',(19.3992595355481,-16.4783778303156,-18.8000870787828));
#52728=CARTESIAN_POINT('Ctrl Pts',(19.4840276488776,-16.5027564393573,-18.8044735407967));
#52729=CARTESIAN_POINT('Ctrl Pts',(19.5671906913809,-16.5313816344173,-18.8088600028106));
#52730=CARTESIAN_POINT('Ctrl Pts',(19.6503537338842,-16.5600068294773,-18.8132464648245));
#52731=CARTESIAN_POINT('Ctrl Pts',(19.7319111958456,-16.5928783231054,-18.8176329268384));
#52732=CARTESIAN_POINT('Ctrl Pts',(19.8114169849416,-16.6297655931066,-18.8220193888523));
#52733=CARTESIAN_POINT('Ctrl Pts',(19.8872706217461,-16.6649584213673,-18.8262043557615));
#52734=CARTESIAN_POINT('Ctrl Pts',(19.9615393050001,-16.7039371893188,-18.8303893226708));
#52735=CARTESIAN_POINT('Ctrl Pts',(20.0338195953306,-16.7465365521971,-18.83457428958));
#52736=CARTESIAN_POINT('Ctrl Pts',(20.1059885648684,-16.7890703066665,-18.8387528111107));
#52737=CARTESIAN_POINT('Ctrl Pts',(20.1761748342821,-16.8352133429708,-18.8429313326414));
#52738=CARTESIAN_POINT('Ctrl Pts',(20.2439967783581,-16.884753103921,-18.8471098541721));
#52739=CARTESIAN_POINT('Ctrl Pts',(20.2606541312307,-16.8969202762222,-18.8481361165208));
#52740=CARTESIAN_POINT('Ctrl Pts',(20.2771689760538,-16.9092921241003,-18.8491623788695));
#52741=CARTESIAN_POINT('Ctrl Pts',(20.293535888361,-16.9218650751948,-18.8501886412182));
#52742=CARTESIAN_POINT('Ctrl Pts',(20.293535888361,-16.9218650751948,-18.0500683203253));
#52743=CARTESIAN_POINT('Ctrl Pts',(20.3406388678367,-16.9580492647496,-18.0530337298048));
#52744=CARTESIAN_POINT('Ctrl Pts',(20.3864285999648,-16.9958326961473,-18.0559991392842));
#52745=CARTESIAN_POINT('Ctrl Pts',(20.43079571541,-17.0351055584184,-18.0589645487637));
#52746=CARTESIAN_POINT('Ctrl Pts',(20.4934043225857,-17.0905254157142,-18.0631491831568));
#52747=CARTESIAN_POINT('Ctrl Pts',(20.5534114448282,-17.1491189671381,-18.0673338175499));
#52748=CARTESIAN_POINT('Ctrl Pts',(20.6104778947947,-17.210612418114,-18.071518451943));
#52749=CARTESIAN_POINT('Ctrl Pts',(20.6674631177332,-17.2720183407738,-18.075697130027));
#52750=CARTESIAN_POINT('Ctrl Pts',(20.721515672228,-17.3363156298581,-18.079875808111));
#52751=CARTESIAN_POINT('Ctrl Pts',(20.7723306651571,-17.4031913935285,-18.084054486195));
#52752=CARTESIAN_POINT('Ctrl Pts',(20.8240564803135,-17.4712658571988,-18.0883080640805));
#52753=CARTESIAN_POINT('Ctrl Pts',(20.8724271646772,-17.5420118234209,-18.0925616419659));
#52754=CARTESIAN_POINT('Ctrl Pts',(20.9171616597699,-17.6150612701733,-18.0968152198513));
#52755=CARTESIAN_POINT('Ctrl Pts',(20.9610288893839,-17.6866945108573,-18.1009863338293));
#52756=CARTESIAN_POINT('Ctrl Pts',(21.0013994094996,-17.7605423037904,-18.1051574478073));
#52757=CARTESIAN_POINT('Ctrl Pts',(21.0380509604127,-17.8362270966629,-18.1093285617853));
#52758=CARTESIAN_POINT('Ctrl Pts',(21.0746902125439,-17.9118864927723,-18.1134982761058));
#52759=CARTESIAN_POINT('Ctrl Pts',(21.1076127735552,-17.9893812509009,-18.1176679904262));
#52760=CARTESIAN_POINT('Ctrl Pts',(21.136642647489,-18.068309834576,-18.1218377047466));
#52761=CARTESIAN_POINT('Ctrl Pts',(21.1656714884152,-18.1472356096333,-18.1260072706907));
#52762=CARTESIAN_POINT('Ctrl Pts',(21.1908077596747,-18.2275946767429,-18.1301768366348));
#52763=CARTESIAN_POINT('Ctrl Pts',(21.2119243630671,-18.3089674573408,-18.1343464025789));
#52764=CARTESIAN_POINT('Ctrl Pts',(21.2337834001839,-18.3932012045179,-18.1386625653178));
#52765=CARTESIAN_POINT('Ctrl Pts',(21.2513347146948,-18.478520765314,-18.1429787280566));
#52766=CARTESIAN_POINT('Ctrl Pts',(21.264494683606,-18.5644478664209,-18.1472948907955));
#52767=CARTESIAN_POINT('Ctrl Pts',(21.2772259679145,-18.6475759012496,-18.1514704549872));
#52768=CARTESIAN_POINT('Ctrl Pts',(21.2858476079666,-18.731272029579,-18.1556460191789));
#52769=CARTESIAN_POINT('Ctrl Pts',(21.290336834896,-18.8150986247191,-18.1598215833707));
#52770=CARTESIAN_POINT('Ctrl Pts',(21.2950528020053,-18.9031591018971,-18.1642080453831));
#52771=CARTESIAN_POINT('Ctrl Pts',(21.295207927637,-18.9913629881317,-18.1685945073955));
#52772=CARTESIAN_POINT('Ctrl Pts',(21.2908376238656,-19.0792059950831,-18.1729809694079));
#52773=CARTESIAN_POINT('Ctrl Pts',(21.2864673200943,-19.1670490020345,-18.1773674314203));
#52774=CARTESIAN_POINT('Ctrl Pts',(21.2775717212915,-19.2545305601574,-18.1817538934327));
#52775=CARTESIAN_POINT('Ctrl Pts',(21.2642482087235,-19.3411580684654,-18.1861403554451));
#52776=CARTESIAN_POINT('Ctrl Pts',(21.2515377307187,-19.4237997167046,-18.1903249898381));
#52777=CARTESIAN_POINT('Ctrl Pts',(21.2347505437471,-19.5059717882466,-18.1945096242311));
#52778=CARTESIAN_POINT('Ctrl Pts',(21.2139332700428,-19.5872408804027,-18.1986942586241));
#52779=CARTESIAN_POINT('Ctrl Pts',(21.193145627151,-19.6683942960652,-18.202872936708));
#52780=CARTESIAN_POINT('Ctrl Pts',(21.168339404859,-19.748646843478,-18.2070516147919));
#52781=CARTESIAN_POINT('Ctrl Pts',(21.1396126628223,-19.8275727933582,-18.2112302928758));
#52782=CARTESIAN_POINT('Ctrl Pts',(21.1103710145797,-19.9079134341683,-18.2154838707612));
#52783=CARTESIAN_POINT('Ctrl Pts',(21.0770669868023,-19.986878974605,-18.2197374486467));
#52784=CARTESIAN_POINT('Ctrl Pts',(21.039857896146,-20.0640338856263,-18.2239910265321));
#52785=CARTESIAN_POINT('Ctrl Pts',(21.0033701763203,-20.1396929981408,-18.22816214051));
#52786=CARTESIAN_POINT('Ctrl Pts',(20.9631276659828,-20.2136106264638,-18.2323332544879));
#52787=CARTESIAN_POINT('Ctrl Pts',(20.9193275219143,-20.2853955234528,-18.2365043684658));
#52788=CARTESIAN_POINT('Ctrl Pts',(20.8755420754071,-20.3571563323264,-18.2406740827861));
#52789=CARTESIAN_POINT('Ctrl Pts',(20.8282016054836,-20.4267854387981,-18.2448437971064));
#52790=CARTESIAN_POINT('Ctrl Pts',(20.7775484774992,-20.4939175140424,-18.2490135114267));
#52791=CARTESIAN_POINT('Ctrl Pts',(20.7268971519705,-20.5610472004393,-18.2531830773707));
#52792=CARTESIAN_POINT('Ctrl Pts',(20.672933680517,-20.6256796655625,-18.2573526433147));
#52793=CARTESIAN_POINT('Ctrl Pts',(20.6159420664663,-20.6874809300205,-18.2615222092587));
#52794=CARTESIAN_POINT('Ctrl Pts',(20.5569466975706,-20.7514550506984,-18.2658383719977));
#52795=CARTESIAN_POINT('Ctrl Pts',(20.4947066427107,-20.8123947886944,-18.2701545347367));
#52796=CARTESIAN_POINT('Ctrl Pts',(20.4295787905098,-20.8699709500337,-18.2744706974756));
#52797=CARTESIAN_POINT('Ctrl Pts',(20.3665724712459,-20.9256715739718,-18.2786462616673));
#52798=CARTESIAN_POINT('Ctrl Pts',(20.3008640027604,-20.9782241356929,-18.2828218258589));
#52799=CARTESIAN_POINT('Ctrl Pts',(20.2328090354881,-21.0273726111567,-18.2869973900505));
#52800=CARTESIAN_POINT('Ctrl Pts',(20.1613167736014,-21.0790034592787,-18.2913838520632));
#52801=CARTESIAN_POINT('Ctrl Pts',(20.0872352304043,-21.1268769860889,-18.2957703140758));
#52802=CARTESIAN_POINT('Ctrl Pts',(20.0110076004693,-21.1707500058239,-18.3001567760885));
#52803=CARTESIAN_POINT('Ctrl Pts',(19.9347799705344,-21.214623025559,-18.3045432381012));
#52804=CARTESIAN_POINT('Ctrl Pts',(19.8564068054921,-21.2544953429201,-18.3089297001138));
#52805=CARTESIAN_POINT('Ctrl Pts',(19.7763550154486,-21.2901822045703,-18.3133161621265));
#52806=CARTESIAN_POINT('Ctrl Pts',(19.6999865269343,-21.3242270608135,-18.3175007965194));
#52807=CARTESIAN_POINT('Ctrl Pts',(19.6218062328675,-21.3545898770089,-18.3216854309123));
#52808=CARTESIAN_POINT('Ctrl Pts',(19.5422037920528,-21.3810752624222,-18.3258700653053));
#52809=CARTESIAN_POINT('Ctrl Pts',(19.4627146554599,-21.4075229491676,-18.3300487433891));
#52810=CARTESIAN_POINT('Ctrl Pts',(19.3818078256885,-21.4301040236941,-18.3342274214729));
#52811=CARTESIAN_POINT('Ctrl Pts',(19.2998943515241,-21.4486704994679,-18.3384060995568));
#52812=CARTESIAN_POINT('Ctrl Pts',(19.2165126372027,-21.467569765977,-18.3426596774422));
#52813=CARTESIAN_POINT('Ctrl Pts',(19.1320882756879,-21.4823088984316,-18.3469132553277));
#52814=CARTESIAN_POINT('Ctrl Pts',(19.0470726305021,-21.4927844316334,-18.3511668332132));
#52815=CARTESIAN_POINT('Ctrl Pts',(18.9637051794954,-21.5030568761824,-18.355337947191));
#52816=CARTESIAN_POINT('Ctrl Pts',(18.8797696442091,-21.5092295037566,-18.3595090611688));
#52817=CARTESIAN_POINT('Ctrl Pts',(18.7957017187999,-21.5112563173502,-18.3636801751467));
#52818=CARTESIAN_POINT('Ctrl Pts',(18.7116620031949,-21.513282450827,-18.3678498894669));
#52819=CARTESIAN_POINT('Ctrl Pts',(18.6274904452119,-21.5111655221263,-18.3720196037872));
#52820=CARTESIAN_POINT('Ctrl Pts',(18.5436254163484,-21.5049115765924,-18.3761893181075));
#52821=CARTESIAN_POINT('Ctrl Pts',(18.4597633717625,-21.4986578536007,-18.3803588840514));
#52822=CARTESIAN_POINT('Ctrl Pts',(18.3762082933047,-21.4882674415331,-18.3845284499953));
#52823=CARTESIAN_POINT('Ctrl Pts',(18.2933947304044,-21.4737983655329,-18.3886980159393));
#52824=CARTESIAN_POINT('Ctrl Pts',(18.2076695447891,-21.4588205746693,-18.3930141786783));
#52825=CARTESIAN_POINT('Ctrl Pts',(18.1227395078358,-21.4394720625982,-18.3973303414174));
#52826=CARTESIAN_POINT('Ctrl Pts',(18.0390745966241,-21.415874729718,-18.4016465041564));
#52827=CARTESIAN_POINT('Ctrl Pts',(17.9581350610998,-21.3930460774757,-18.405822068348));
#52828=CARTESIAN_POINT('Ctrl Pts',(17.878379925585,-21.3662413589922,-18.4099976325396));
#52829=CARTESIAN_POINT('Ctrl Pts',(17.8002169726158,-21.3356210390432,-18.4141731967311));
#52830=CARTESIAN_POINT('Ctrl Pts',(17.7181061946998,-21.3034541595236,-18.4185596587439));
#52831=CARTESIAN_POINT('Ctrl Pts',(17.6377532005344,-21.2670763374213,-18.4229461207567));
#52832=CARTESIAN_POINT('Ctrl Pts',(17.559602363678,-21.2267285973938,-18.4273325827695));
#52833=CARTESIAN_POINT('Ctrl Pts',(17.4814515268215,-21.1863808573663,-18.4317190447823));
#52834=CARTESIAN_POINT('Ctrl Pts',(17.4055033100765,-21.1420635575358,-18.4361055067951));
#52835=CARTESIAN_POINT('Ctrl Pts',(17.3321657913464,-21.0940692919344,-18.4404919688079));
#52836=CARTESIAN_POINT('Ctrl Pts',(17.2622960528831,-21.0483444454524,-18.4446710160258));
#52837=CARTESIAN_POINT('Ctrl Pts',(17.19453408493,-20.9991112651902,-18.4488500632436));
#52838=CARTESIAN_POINT('Ctrl Pts',(17.1292545139165,-20.9465906660001,-18.4530291104615));
#52839=CARTESIAN_POINT('Ctrl Pts',(17.0640679209105,-20.8941448721524,-18.4572022054423));
#52840=CARTESIAN_POINT('Ctrl Pts',(17.0013570587501,-20.8384212459578,-18.461375300423));
#52841=CARTESIAN_POINT('Ctrl Pts',(16.9414683281885,-20.7796843834625,-18.4655483954038));
#52842=CARTESIAN_POINT('Ctrl Pts',(16.8809773183908,-20.7203568256503,-18.4697634576868));
#52843=CARTESIAN_POINT('Ctrl Pts',(16.8233659292103,-20.6579553356915,-18.4739785199699));
#52844=CARTESIAN_POINT('Ctrl Pts',(16.7689574885196,-20.5927949073772,-18.4781935822529));
#52845=CARTESIAN_POINT('Ctrl Pts',(16.715187711247,-20.5283993526991,-18.4823591668069));
#52846=CARTESIAN_POINT('Ctrl Pts',(16.6645463875622,-20.4613096522779,-18.4865247513609));
#52847=CARTESIAN_POINT('Ctrl Pts',(16.6173078768047,-20.3918661241945,-18.4906903359149));
#52848=CARTESIAN_POINT('Ctrl Pts',(16.5700850499656,-20.3224456524398,-18.4948545374302));
#52849=CARTESIAN_POINT('Ctrl Pts',(16.5262630517185,-20.2506732862345,-18.4990187389455));
#52850=CARTESIAN_POINT('Ctrl Pts',(16.4860739671284,-20.1769198140034,-18.5031829404608));
#52851=CARTESIAN_POINT('Ctrl Pts',(16.4458860826634,-20.1031685441962,-18.5073470176248));
#52852=CARTESIAN_POINT('Ctrl Pts',(16.4093311160888,-20.0274366916313,-18.5115110947889));
#52853=CARTESIAN_POINT('Ctrl Pts',(16.3765953977372,-19.9501200034215,-18.5156751719529));
#52854=CARTESIAN_POINT('Ctrl Pts',(16.3431614559385,-19.8711542197504,-18.5199280651399));
#52855=CARTESIAN_POINT('Ctrl Pts',(16.313711777103,-19.7905356687049,-18.5241809583268));
#52856=CARTESIAN_POINT('Ctrl Pts',(16.2883925214925,-19.7087060598861,-18.5284338515138));
#52857=CARTESIAN_POINT('Ctrl Pts',(16.2635663208297,-19.6284699613234,-18.5326039259141));
#52858=CARTESIAN_POINT('Ctrl Pts',(16.2427111716313,-19.5470700198228,-18.5367740003145));
#52859=CARTESIAN_POINT('Ctrl Pts',(16.2259135016087,-19.4649348073461,-18.5409440747148));
#52860=CARTESIAN_POINT('Ctrl Pts',(16.2086154222952,-19.3803527541242,-18.5452383772951));
#52861=CARTESIAN_POINT('Ctrl Pts',(16.1956204803925,-19.294991452669,-18.5495326798753));
#52862=CARTESIAN_POINT('Ctrl Pts',(16.1869656326132,-19.2093245642189,-18.5538269824556));
#52863=CARTESIAN_POINT('Ctrl Pts',(16.1783107848339,-19.1236576757689,-18.5581212850358));
#52864=CARTESIAN_POINT('Ctrl Pts',(16.1739959871027,-19.0376857298059,-18.5624155876161));
#52865=CARTESIAN_POINT('Ctrl Pts',(16.1740000028035,-18.9518801919504,-18.5667098901964));
#52866=CARTESIAN_POINT('Origin',(18.734,-18.952,1.76670989022851));
#52867=CARTESIAN_POINT('',(20.2917780564659,-16.9241894633619,-17.2500265416684));
#52868=CARTESIAN_POINT('',(20.294455276885,-16.9206896363573,-17.3168007021646));
#52869=CARTESIAN_POINT('',(20.293535888361,-16.9218650751948,1.76670989022851));
#52870=CARTESIAN_POINT('',(16.1740010840393,-18.9543559031924,-17.8332901097715));
#52871=CARTESIAN_POINT('Ctrl Pts',(20.294455276885,-16.9206896363574,-17.3168007021646));
#52872=CARTESIAN_POINT('Ctrl Pts',(20.846620702996,-17.3535718202006,-17.3517574545992));
#52873=CARTESIAN_POINT('Ctrl Pts',(21.6812137686398,-18.8317283057607,-17.4291061425942));
#52874=CARTESIAN_POINT('Ctrl Pts',(20.5976437703141,-21.3373977591934,-17.5488467661498));
#52875=CARTESIAN_POINT('Ctrl Pts',(17.7370130079676,-21.8102000472194,-17.6760225728312));
#52876=CARTESIAN_POINT('Ctrl Pts',(16.2862274700061,-20.2077259602722,-17.7708370079896));
#52877=CARTESIAN_POINT('Ctrl Pts',(16.1722336653236,-19.1559927438033,-17.8232595075876));
#52878=CARTESIAN_POINT('Ctrl Pts',(16.1740883619038,-18.9543565896946,-17.833290071625));
#52879=CARTESIAN_POINT('Ctrl Pts',(16.1740010840393,-18.9543559031924,-17.8332901097715));
#52880=CARTESIAN_POINT('Ctrl Pts',(16.1739248258781,-18.8714913735434,-17.837412174938));
#52881=CARTESIAN_POINT('Ctrl Pts',(16.177876160498,-18.7885152466554,-17.8415342401044));
#52882=CARTESIAN_POINT('Ctrl Pts',(16.1858608731257,-18.7058557534858,-17.8456563052709));
#52883=CARTESIAN_POINT('Ctrl Pts',(16.1938402258665,-18.6232517470386,-17.8497756034244));
#52884=CARTESIAN_POINT('Ctrl Pts',(16.205847540348,-18.5409644216311,-17.853894901578));
#52885=CARTESIAN_POINT('Ctrl Pts',(16.2218365582967,-18.4594202174575,-17.8580141997315));
#52886=CARTESIAN_POINT('Ctrl Pts',(16.2378199266111,-18.3779048264942,-17.862132042353));
#52887=CARTESIAN_POINT('Ctrl Pts',(16.2577821151893,-18.2971324990612,-17.8662498849744));
#52888=CARTESIAN_POINT('Ctrl Pts',(16.2816254461127,-18.2175212409839,-17.8703677275959));
#52889=CARTESIAN_POINT('Ctrl Pts',(16.3054679320359,-18.1379128043045,-17.8744854242824));
#52890=CARTESIAN_POINT('Ctrl Pts',(16.3331911499574,-18.0594658076281,-17.8786031209688));
#52891=CARTESIAN_POINT('Ctrl Pts',(16.364647494651,-17.9825833169392,-17.8827208176552));
#52892=CARTESIAN_POINT('Ctrl Pts',(16.396133878009,-17.905627408714,-17.8868424464612));
#52893=CARTESIAN_POINT('Ctrl Pts',(16.4313603282317,-17.8302394286303,-17.8909640752672));
#52894=CARTESIAN_POINT('Ctrl Pts',(16.470131238009,-17.7568020128526,-17.8950857040732));
#52895=CARTESIAN_POINT('Ctrl Pts',(16.5089205032735,-17.683329829267,-17.8992092842006));
#52896=CARTESIAN_POINT('Ctrl Pts',(16.5512573267501,-17.6118104548626,-17.903332864328));
#52897=CARTESIAN_POINT('Ctrl Pts',(16.5969016205558,-17.5425992349311,-17.9074564444553));
#52898=CARTESIAN_POINT('Ctrl Pts',(16.6426258760308,-17.4732667677586,-17.9115872484506));
#52899=CARTESIAN_POINT('Ctrl Pts',(16.691668894117,-17.4062509123682,-17.915718052446));
#52900=CARTESIAN_POINT('Ctrl Pts',(16.743749207993,-17.3418752269108,-17.9198488564413));
#52901=CARTESIAN_POINT('Ctrl Pts',(16.7879829276106,-17.2871985975131,-17.9233572996922));
#52902=CARTESIAN_POINT('Ctrl Pts',(16.8344068718464,-17.2344260450368,-17.9268657429432));
#52903=CARTESIAN_POINT('Ctrl Pts',(16.8828286089277,-17.1837340469049,-17.9303741861941));
#52904=CARTESIAN_POINT('Ctrl Pts',(16.9405827898754,-17.1232720517519,-17.9345588205871));
#52905=CARTESIAN_POINT('Ctrl Pts',(17.0014097311533,-17.0655300202436,-17.9387434549801));
#52906=CARTESIAN_POINT('Ctrl Pts',(17.0650229727702,-17.0108365131759,-17.9429280893731));
#52907=CARTESIAN_POINT('Ctrl Pts',(17.1285456688113,-16.9562208555459,-17.947106767457));
#52908=CARTESIAN_POINT('Ctrl Pts',(17.1948464417151,-16.9046454006959,-17.9512854455408));
#52909=CARTESIAN_POINT('Ctrl Pts',(17.2636010628229,-16.8564029572581,-17.9554641236247));
#52910=CARTESIAN_POINT('Ctrl Pts',(17.3335880611023,-16.807295802692,-17.9597177015102));
#52911=CARTESIAN_POINT('Ctrl Pts',(17.4061174102896,-16.7616426719217,-17.9639712793956));
#52912=CARTESIAN_POINT('Ctrl Pts',(17.4808106950308,-16.7197104654837,-17.9682248572811));
#52913=CARTESIAN_POINT('Ctrl Pts',(17.5540559046941,-16.6785911966922,-17.972395971259));
#52914=CARTESIAN_POINT('Ctrl Pts',(17.6293814748141,-16.6410501005274,-17.9765670852369));
#52915=CARTESIAN_POINT('Ctrl Pts',(17.7064016963159,-16.6072949596451,-17.9807381992148));
#52916=CARTESIAN_POINT('Ctrl Pts',(17.7833960729384,-16.5735511456264,-17.9849079135351));
#52917=CARTESIAN_POINT('Ctrl Pts',(17.8620835505878,-16.5435909483342,-17.9890776278554));
#52918=CARTESIAN_POINT('Ctrl Pts',(17.942056207647,-16.5175750104483,-17.9932473421757));
#52919=CARTESIAN_POINT('Ctrl Pts',(18.0220260189362,-16.4915599983211,-17.9974169081197));
#52920=CARTESIAN_POINT('Ctrl Pts',(18.1032804809772,-16.4694891080432,-18.0015864740637));
#52921=CARTESIAN_POINT('Ctrl Pts',(18.185395497294,-16.4514734355319,-18.0057560400077));
#52922=CARTESIAN_POINT('Ctrl Pts',(18.270397576287,-16.4328243541994,-18.0100722027467));
#52923=CARTESIAN_POINT('Ctrl Pts',(18.3563213344852,-16.4185210722996,-18.0143883654857));
#52924=CARTESIAN_POINT('Ctrl Pts',(18.4426856715113,-16.4086290160464,-18.0187045282247));
#52925=CARTESIAN_POINT('Ctrl Pts',(18.5262366993404,-16.3990591924854,-18.0228800924163));
#52926=CARTESIAN_POINT('Ctrl Pts',(18.6101995699748,-16.3936175999792,-18.0270556566079));
#52927=CARTESIAN_POINT('Ctrl Pts',(18.6941361080731,-16.3923103957471,-18.0312312207995));
#52928=CARTESIAN_POINT('Ctrl Pts',(18.7823120811743,-16.3909371677368,-18.0356176828122));
#52929=CARTESIAN_POINT('Ctrl Pts',(18.870458408217,-16.3941269389876,-18.0400041448249));
#52930=CARTESIAN_POINT('Ctrl Pts',(18.9580725064405,-16.4018251997446,-18.0443906068375));
#52931=CARTESIAN_POINT('Ctrl Pts',(19.0456866046639,-16.4095234605017,-18.0487770688502));
#52932=CARTESIAN_POINT('Ctrl Pts',(19.132767910028,-16.4217300548923,-18.0531635308629));
#52933=CARTESIAN_POINT('Ctrl Pts',(19.2188278686569,-16.4383289917386,-18.0575499928755));
#52934=CARTESIAN_POINT('Ctrl Pts',(19.3009320014006,-16.4541649430446,-18.06173482709));
#52935=CARTESIAN_POINT('Ctrl Pts',(19.3824122424308,-16.4740572520235,-18.0659196613044));
#52936=CARTESIAN_POINT('Ctrl Pts',(19.4628372070832,-16.4979428846151,-18.0701044955188));
#52937=CARTESIAN_POINT('Ctrl Pts',(19.5431287709651,-16.5217888981431,-18.0742823883549));
#52938=CARTESIAN_POINT('Ctrl Pts',(19.6223681012692,-16.5496149366889,-18.078460281191));
#52939=CARTESIAN_POINT('Ctrl Pts',(19.700133730563,-16.5813069336862,-18.0826381740271));
#52940=CARTESIAN_POINT('Ctrl Pts',(19.7778242916654,-16.6129683379793,-18.0868120338879));
#52941=CARTESIAN_POINT('Ctrl Pts',(19.8540435523397,-16.648488119696,-18.0909858937488));
#52942=CARTESIAN_POINT('Ctrl Pts',(19.9283857679273,-16.6877026172844,-18.0951597536096));
#52943=CARTESIAN_POINT('Ctrl Pts',(20.0026788000524,-16.726891171272,-18.0993308521204));
#52944=CARTESIAN_POINT('Ctrl Pts',(20.075096847298,-16.7697693732459,-18.1035019506312));
#52945=CARTESIAN_POINT('Ctrl Pts',(20.1452559587291,-16.8161262633405,-18.107673049142));
#52946=CARTESIAN_POINT('Ctrl Pts',(20.1959047159558,-16.8495918934532,-18.1106842183477));
#52947=CARTESIAN_POINT('Ctrl Pts',(20.2453766322748,-16.8848694611075,-18.1136953875534));
#52948=CARTESIAN_POINT('Ctrl Pts',(20.293535888361,-16.9218650751948,-18.1167065567592));
#52949=CARTESIAN_POINT('',(16.1740009581142,-18.9497851537726,-17.7667099127478));
#52950=CARTESIAN_POINT('Ctrl Pts',(16.1740009581142,-18.9497851537726,-17.7667099127478));
#52951=CARTESIAN_POINT('Ctrl Pts',(16.1740887027229,-18.8483667747388,-17.7717442924632));
#52952=CARTESIAN_POINT('Ctrl Pts',(16.1802070184517,-18.74721232135,-17.7767786721785));
#52953=CARTESIAN_POINT('Ctrl Pts',(16.1922394471764,-18.6469536230176,-17.7818130518939));
#52954=CARTESIAN_POINT('Ctrl Pts',(16.2044426849046,-18.5452716801573,-17.78691889826));
#52955=CARTESIAN_POINT('Ctrl Pts',(16.2227290670666,-18.4445110968517,-17.7920247446261));
#52956=CARTESIAN_POINT('Ctrl Pts',(16.2469282568539,-18.3453088558055,-17.7971305909922));
#52957=CARTESIAN_POINT('Ctrl Pts',(16.2587491290733,-18.2968503319625,-17.7996247057951));
#52958=CARTESIAN_POINT('Ctrl Pts',(16.2719801580747,-18.2487633198967,-17.8021188205979));
#52959=CARTESIAN_POINT('Ctrl Pts',(16.2865973915759,-18.201120201178,-17.8046129354008));
#52960=CARTESIAN_POINT('Ctrl Pts',(16.3111222362101,-18.1211844127561,-17.8087975697938));
#52961=CARTESIAN_POINT('Ctrl Pts',(16.3396130703746,-18.0423026572186,-17.8129822041869));
#52962=CARTESIAN_POINT('Ctrl Pts',(16.3719611025222,-17.9648970434642,-17.8171668385799));
#52963=CARTESIAN_POINT('Ctrl Pts',(16.4042630912499,-17.8876016070201,-17.8213455166639));
#52964=CARTESIAN_POINT('Ctrl Pts',(16.440411196743,-17.8117785597319,-17.8255241947478));
#52965=CARTESIAN_POINT('Ctrl Pts',(16.4802468398231,-17.7378349811527,-17.8297028728318));
#52966=CARTESIAN_POINT('Ctrl Pts',(16.5207965081759,-17.6625660170697,-17.8339564507172));
#52967=CARTESIAN_POINT('Ctrl Pts',(16.5651670712163,-17.5892450243182,-17.8382100286026));
#52968=CARTESIAN_POINT('Ctrl Pts',(16.6131398985284,-17.5182802121802,-17.8424636064881));
#52969=CARTESIAN_POINT('Ctrl Pts',(16.6601826789718,-17.448691191402,-17.846634720466));
#52970=CARTESIAN_POINT('Ctrl Pts',(16.7106890267627,-17.3813682068563,-17.8508058344439));
#52971=CARTESIAN_POINT('Ctrl Pts',(16.7644072919755,-17.3166698912768,-17.8549769484219));
#52972=CARTESIAN_POINT('Ctrl Pts',(16.8181075315056,-17.2519932858419,-17.8591466627423));
#52973=CARTESIAN_POINT('Ctrl Pts',(16.8750172543249,-17.1899399538654,-17.8633163770626));
#52974=CARTESIAN_POINT('Ctrl Pts',(16.9348438240379,-17.1308363460421,-17.867486091383));
#52975=CARTESIAN_POINT('Ctrl Pts',(16.9946682648647,-17.0717348413788,-17.871655657327));
#52976=CARTESIAN_POINT('Ctrl Pts',(17.0574090183535,-17.0155831748762,-17.8758252232711));
#52977=CARTESIAN_POINT('Ctrl Pts',(17.1227367799307,-16.9626707573527,-17.8799947892151));
#52978=CARTESIAN_POINT('Ctrl Pts',(17.1903613850146,-16.9078980045034,-17.884310951954));
#52979=CARTESIAN_POINT('Ctrl Pts',(17.2607578915086,-16.8565968547188,-17.8886271146929));
#52980=CARTESIAN_POINT('Ctrl Pts',(17.3335255671368,-16.8090414462952,-17.8929432774319));
#52981=CARTESIAN_POINT('Ctrl Pts',(17.403922843385,-16.7630351502993,-17.8971188416235));
#52982=CARTESIAN_POINT('Ctrl Pts',(17.4765387490618,-16.7205345053978,-17.9012944058152));
#52983=CARTESIAN_POINT('Ctrl Pts',(17.5509843556044,-16.681741427697,-17.9054699700069));
#52984=CARTESIAN_POINT('Ctrl Pts',(17.6291900327561,-16.6409890038631,-17.9098564320194));
#52985=CARTESIAN_POINT('Ctrl Pts',(17.7094145736833,-16.6043287713981,-17.914242894032));
#52986=CARTESIAN_POINT('Ctrl Pts',(17.7911842815274,-16.5719372863303,-17.9186293560446));
#52987=CARTESIAN_POINT('Ctrl Pts',(17.8729539893715,-16.5395458012624,-17.9230158180571));
#52988=CARTESIAN_POINT('Ctrl Pts',(17.9562682900625,-16.5114231770868,-17.9274022800697));
#52989=CARTESIAN_POINT('Ctrl Pts',(18.0406384682269,-16.4876847226345,-17.9317887420822));
#52990=CARTESIAN_POINT('Ctrl Pts',(18.1211305077812,-16.465037424071,-17.9359735770737));
#52991=CARTESIAN_POINT('Ctrl Pts',(18.2028831083918,-16.4462957978936,-17.9401584120651));
#52992=CARTESIAN_POINT('Ctrl Pts',(18.2854823965109,-16.4315968657057,-17.9443432470566));
#52993=CARTESIAN_POINT('Ctrl Pts',(18.3679630513099,-16.4169190448757,-17.9485220715741));
#52994=CARTESIAN_POINT('Ctrl Pts',(18.4512875288656,-16.406272464111,-17.9527008960917));
#52995=CARTESIAN_POINT('Ctrl Pts',(18.5350276579563,-16.3997441336924,-17.9568797206092));
#52996=CARTESIAN_POINT('Ctrl Pts',(18.6186666109273,-16.3932236909036,-17.9610534962063));
#52997=CARTESIAN_POINT('Ctrl Pts',(18.702719760757,-16.3908116415349,-17.9652272718033));
#52998=CARTESIAN_POINT('Ctrl Pts',(18.7867510727816,-16.3925435490479,-17.9694010474004));
#52999=CARTESIAN_POINT('Ctrl Pts',(18.8707269523644,-16.3942743140836,-17.9735720697075));
#53000=CARTESIAN_POINT('Ctrl Pts',(18.9546805641743,-16.4001435983918,-17.9777430920145));
#53001=CARTESIAN_POINT('Ctrl Pts',(19.0381741527013,-16.4101349200187,-17.9819141143216));
#53002=CARTESIAN_POINT('Ctrl Pts',(19.1216377101414,-16.4201226479535,-17.9860836363897));
#53003=CARTESIAN_POINT('Ctrl Pts',(19.20464111675,-16.4342294129592,-17.9902531584578));
#53004=CARTESIAN_POINT('Ctrl Pts',(19.2867513915057,-16.4523868500929,-17.994422680526));
#53005=CARTESIAN_POINT('Ctrl Pts',(19.3688567634641,-16.4705432030477,-17.9985919536323));
#53006=CARTESIAN_POINT('Ctrl Pts',(19.4500686609567,-16.4927496461544,-18.0027612267386));
#53007=CARTESIAN_POINT('Ctrl Pts',(19.5299652993024,-16.5188869236498,-18.0069304998449));
#53008=CARTESIAN_POINT('Ctrl Pts',(19.6099224331162,-16.5450439915502,-18.0111029298066));
#53009=CARTESIAN_POINT('Ctrl Pts',(19.6885618814584,-16.5751376935414,-18.0152753597682));
#53010=CARTESIAN_POINT('Ctrl Pts',(19.7654786756165,-16.6089994149065,-18.0194477897299));
#53011=CARTESIAN_POINT('Ctrl Pts',(19.8424284165325,-16.6428756406975,-18.023622006922));
#53012=CARTESIAN_POINT('Ctrl Pts',(19.9176536212663,-16.6805228962852,-18.0277962241141));
#53013=CARTESIAN_POINT('Ctrl Pts',(19.9907728936478,-16.7217260496091,-18.0319704413063));
#53014=CARTESIAN_POINT('Ctrl Pts',(20.0639908538905,-16.7629848141412,-18.0361502923696));
#53015=CARTESIAN_POINT('Ctrl Pts',(20.1350968176494,-16.807808813561,-18.040330143433));
#53016=CARTESIAN_POINT('Ctrl Pts',(20.2037378785288,-16.8559392736808,-18.0445099944964));
#53017=CARTESIAN_POINT('Ctrl Pts',(20.2341639531921,-16.8772737483295,-18.0463627697727));
#53018=CARTESIAN_POINT('Ctrl Pts',(20.2641061463923,-16.8992573468981,-18.048215545049));
#53019=CARTESIAN_POINT('Ctrl Pts',(20.293535888361,-16.9218650751948,-18.0500683203253));
#53020=CARTESIAN_POINT('Ctrl Pts',(20.2917780564658,-16.9241894633618,-17.2500265416684));
#53021=CARTESIAN_POINT('Ctrl Pts',(20.5375805774977,-17.1103101642375,-17.2653209306706));
#53022=CARTESIAN_POINT('Ctrl Pts',(21.3400060360654,-17.9709561757374,-17.3230072552333));
#53023=CARTESIAN_POINT('Ctrl Pts',(21.4691813208793,-20.2489483349579,-17.4230855153565));
#53024=CARTESIAN_POINT('Ctrl Pts',(19.1239734689994,-21.9538681741735,-17.5502613220379));
#53025=CARTESIAN_POINT('Ctrl Pts',(16.6895185822271,-21.0089844641567,-17.6648027803286));
#53026=CARTESIAN_POINT('Ctrl Pts',(16.1805386002103,-19.5488856395492,-17.7369523030588));
#53027=CARTESIAN_POINT('Ctrl Pts',(16.1756126004107,-18.9497870014945,-17.7667098902285));
#53028=CARTESIAN_POINT('Origin',(18.734,-18.952,1.76670989022851));
#53029=CARTESIAN_POINT('',(20.293535888361,-16.9218650751947,-16.4501666918036));
#53030=CARTESIAN_POINT('',(20.293535888361,-16.9218650751947,-16.516630357267));
#53031=CARTESIAN_POINT('',(20.293535888361,-16.9218650751948,1.76670989022851));
#53032=CARTESIAN_POINT('',(16.1737370593341,-18.9511644347003,-17.0332901097715));
#53033=CARTESIAN_POINT('Ctrl Pts',(20.293535888361,-16.9218650751947,-16.516630357267));
#53034=CARTESIAN_POINT('Ctrl Pts',(20.3601025931298,-16.9730011665887,-16.5208151876277));
#53035=CARTESIAN_POINT('Ctrl Pts',(20.4240566331923,-17.0273416960463,-16.5250000179883));
#53036=CARTESIAN_POINT('Ctrl Pts',(20.4850922791488,-17.0845750805172,-16.529184848349));
#53037=CARTESIAN_POINT('Ctrl Pts',(20.4960575761564,-17.0948572860978,-16.5299366697988));
#53038=CARTESIAN_POINT('Ctrl Pts',(20.506928783665,-17.1052327721162,-16.5306884912485));
#53039=CARTESIAN_POINT('Ctrl Pts',(20.5177042670234,-17.115699619397,-16.5314403126983));
#53040=CARTESIAN_POINT('Ctrl Pts',(20.5776805529838,-17.1739580385085,-16.5356249470914));
#53041=CARTESIAN_POINT('Ctrl Pts',(20.6349112416909,-17.2352663353223,-16.5398095814844));
#53042=CARTESIAN_POINT('Ctrl Pts',(20.6890701824651,-17.2993353087707,-16.5439942158775));
#53043=CARTESIAN_POINT('Ctrl Pts',(20.7431520346907,-17.3633130879657,-16.5481728939614));
#53044=CARTESIAN_POINT('Ctrl Pts',(20.7941705292093,-17.4300433902867,-16.5523515720453));
#53045=CARTESIAN_POINT('Ctrl Pts',(20.8418355824982,-17.4991995466842,-16.5565302501293));
#53046=CARTESIAN_POINT('Ctrl Pts',(20.8903549976109,-17.5695952774835,-16.5607838280147));
#53047=CARTESIAN_POINT('Ctrl Pts',(20.9353992222982,-17.6425043486949,-16.5650374059002));
#53048=CARTESIAN_POINT('Ctrl Pts',(20.9767045339426,-17.7175461234078,-16.5692909837856));
#53049=CARTESIAN_POINT('Ctrl Pts',(21.01720906152,-17.7911330668859,-16.5734620977636));
#53050=CARTESIAN_POINT('Ctrl Pts',(21.0541181225501,-17.8667703369927,-16.5776332117415));
#53051=CARTESIAN_POINT('Ctrl Pts',(21.0872271712958,-17.9440704983605,-16.5818043257195));
#53052=CARTESIAN_POINT('Ctrl Pts',(21.1203251099804,-18.0213447209125,-16.5859740400399));
#53053=CARTESIAN_POINT('Ctrl Pts',(21.149625387836,-18.1002803040063,-16.5901437543602));
#53054=CARTESIAN_POINT('Ctrl Pts',(21.1749707834402,-18.1804679952254,-16.5943134686806));
#53055=CARTESIAN_POINT('Ctrl Pts',(21.2003152771464,-18.2606528330223,-16.5984830346246));
#53056=CARTESIAN_POINT('Ctrl Pts',(21.2217050305799,-18.3420892514568,-16.6026526005687));
#53057=CARTESIAN_POINT('Ctrl Pts',(21.2390325027795,-18.4243522386871,-16.6068221665127));
#53058=CARTESIAN_POINT('Ctrl Pts',(21.2569691875259,-18.5095074910661,-16.6111383292517));
#53059=CARTESIAN_POINT('Ctrl Pts',(21.2705525077454,-18.5955480019175,-16.6154544919906));
#53060=CARTESIAN_POINT('Ctrl Pts',(21.2797210678871,-18.6819921399002,-16.6197706547295));
#53061=CARTESIAN_POINT('Ctrl Pts',(21.2885909631465,-18.7656203691804,-16.6239462189212));
#53062=CARTESIAN_POINT('Ctrl Pts',(21.2933293236125,-18.8496258601582,-16.6281217831129));
#53063=CARTESIAN_POINT('Ctrl Pts',(21.2939336612287,-18.9335704012973,-16.6322973473045));
#53064=CARTESIAN_POINT('Ctrl Pts',(21.2945685225012,-19.0217547816502,-16.6366838093171));
#53065=CARTESIAN_POINT('Ctrl Pts',(21.2906407927078,-19.1098713098954,-16.6410702713296));
#53066=CARTESIAN_POINT('Ctrl Pts',(21.2822091879386,-19.197417877314,-16.6454567333422));
#53067=CARTESIAN_POINT('Ctrl Pts',(21.2737775831694,-19.2849644447327,-16.6498431953547));
#53068=CARTESIAN_POINT('Ctrl Pts',(21.2608422640144,-19.3719404886095,-16.6542296573672));
#53069=CARTESIAN_POINT('Ctrl Pts',(21.2435233083642,-19.4578584434176,-16.6586161193798));
#53070=CARTESIAN_POINT('Ctrl Pts',(21.2270012235362,-19.5398231857641,-16.6628007537728));
#53071=CARTESIAN_POINT('Ctrl Pts',(21.2064285344955,-19.6211301562754,-16.6669853881659));
#53072=CARTESIAN_POINT('Ctrl Pts',(21.1818718743957,-19.7013485747917,-16.6711700225589));
#53073=CARTESIAN_POINT('Ctrl Pts',(21.1573501676621,-19.7814528123184,-16.6753487006429));
#53074=CARTESIAN_POINT('Ctrl Pts',(21.1288558871501,-19.8604711393629,-16.6795273787268));
#53075=CARTESIAN_POINT('Ctrl Pts',(21.0965066931248,-19.9379828218283,-16.6837060568108));
#53076=CARTESIAN_POINT('Ctrl Pts',(21.0635776630456,-20.0168838454952,-16.6879596346962));
#53077=CARTESIAN_POINT('Ctrl Pts',(21.0266542567594,-20.0942232074709,-16.6922132125816));
#53078=CARTESIAN_POINT('Ctrl Pts',(20.98591378162,-20.1695731272289,-16.6964667904671));
#53079=CARTESIAN_POINT('Ctrl Pts',(20.9459631400897,-20.243462241759,-16.700637904445));
#53080=CARTESIAN_POINT('Ctrl Pts',(20.9023423404873,-20.3154379408342,-16.704809018423));
#53081=CARTESIAN_POINT('Ctrl Pts',(20.8552664379161,-20.3851185224436,-16.7089801324009));
#53082=CARTESIAN_POINT('Ctrl Pts',(20.8082063321186,-20.4547757220608,-16.7131498467213));
#53083=CARTESIAN_POINT('Ctrl Pts',(20.7576936832431,-20.5221389528648,-16.7173195610417));
#53084=CARTESIAN_POINT('Ctrl Pts',(20.7039875068322,-20.5868544959491,-16.721489275362));
#53085=CARTESIAN_POINT('Ctrl Pts',(20.6502832415176,-20.6515677361767,-16.7256588413061));
#53086=CARTESIAN_POINT('Ctrl Pts',(20.5933859690516,-20.713633122547,-16.7298284072501));
#53087=CARTESIAN_POINT('Ctrl Pts',(20.5335948472511,-20.7727301792818,-16.7339979731942));
#53088=CARTESIAN_POINT('Ctrl Pts',(20.4717015433682,-20.8339050156273,-16.7383141359331));
#53089=CARTESIAN_POINT('Ctrl Pts',(20.406707483555,-20.8918985349615,-16.742630298672));
#53090=CARTESIAN_POINT('Ctrl Pts',(20.3389844113022,-20.9463984154318,-16.7469464614109));
#53091=CARTESIAN_POINT('Ctrl Pts',(20.2734674110048,-20.9991229680282,-16.7511220256026));
#53092=CARTESIAN_POINT('Ctrl Pts',(20.2053968718997,-21.0485777582944,-16.7552975897943));
#53093=CARTESIAN_POINT('Ctrl Pts',(20.1351399138028,-21.0945234985756,-16.759473153986));
#53094=CARTESIAN_POINT('Ctrl Pts',(20.0613344437724,-21.1427898489728,-16.7638596159985));
#53095=CARTESIAN_POINT('Ctrl Pts',(19.9851163826192,-21.1871830552703,-16.7682460780111));
#53096=CARTESIAN_POINT('Ctrl Pts',(19.9069397062211,-21.2274807064816,-16.7726325400236));
#53097=CARTESIAN_POINT('Ctrl Pts',(19.828763029823,-21.2677783576928,-16.7770190020362));
#53098=CARTESIAN_POINT('Ctrl Pts',(19.748628298259,-21.3039802842616,-16.7814054640487));
#53099=CARTESIAN_POINT('Ctrl Pts',(19.6670104728628,-21.3359235427187,-16.7857919260613));
#53100=CARTESIAN_POINT('Ctrl Pts',(19.5891480045999,-21.3663970445028,-16.7899765604543));
#53101=CARTESIAN_POINT('Ctrl Pts',(19.5096461031211,-21.3931085897472,-16.7941611948473));
#53102=CARTESIAN_POINT('Ctrl Pts',(19.4289030536307,-21.4158810332593,-16.7983458292404));
#53103=CARTESIAN_POINT('Ctrl Pts',(19.3482749318772,-21.4386210630167,-16.8025245073243));
#53104=CARTESIAN_POINT('Ctrl Pts',(19.2664096101498,-21.4574330041518,-16.8067031854083));
#53105=CARTESIAN_POINT('Ctrl Pts',(19.1837245465112,-21.4721880549406,-16.8108818634922));
#53106=CARTESIAN_POINT('Ctrl Pts',(19.0995574125316,-21.4872075794106,-16.8151354413777));
#53107=CARTESIAN_POINT('Ctrl Pts',(19.0145413088146,-21.49802316776,-16.8193890192631));
#53108=CARTESIAN_POINT('Ctrl Pts',(18.9291319041929,-21.5045523579284,-16.8236425971485));
#53109=CARTESIAN_POINT('Ctrl Pts',(18.8453783275425,-21.5109549670048,-16.8278137111265));
#53110=CARTESIAN_POINT('Ctrl Pts',(18.7612470435307,-21.5132358584627,-16.8319848251044));
#53111=CARTESIAN_POINT('Ctrl Pts',(18.6771754083916,-21.5113692515517,-16.8361559390824));
#53112=CARTESIAN_POINT('Ctrl Pts',(18.5931319843017,-21.5095032709988,-16.8403256534027));
#53113=CARTESIAN_POINT('Ctrl Pts',(18.5091486288698,-21.5034925662839,-16.8444953677231));
#53114=CARTESIAN_POINT('Ctrl Pts',(18.4256629639196,-21.4933634671532,-16.8486650820435));
#53115=CARTESIAN_POINT('Ctrl Pts',(18.3421802697477,-21.4832347284594,-16.8528346479875));
#53116=CARTESIAN_POINT('Ctrl Pts',(18.2591956874268,-21.4689879429832,-16.8570042139316));
#53117=CARTESIAN_POINT('Ctrl Pts',(18.1771406148225,-21.4507011876452,-16.8611737798756));
#53118=CARTESIAN_POINT('Ctrl Pts',(18.0922005870914,-21.4317714925488,-16.8654899426145));
#53119=CARTESIAN_POINT('Ctrl Pts',(18.0082571631379,-21.4085125658604,-16.8698061053535));
#53120=CARTESIAN_POINT('Ctrl Pts',(17.9257741739147,-21.3810679311309,-16.8741222680924));
#53121=CARTESIAN_POINT('Ctrl Pts',(17.8459780593898,-21.3545173024911,-16.8782978322841));
#53122=CARTESIAN_POINT('Ctrl Pts',(17.7675491154084,-21.3240496914869,-16.8824733964757));
#53123=CARTESIAN_POINT('Ctrl Pts',(17.6908872600138,-21.2898442659165,-16.8866489606674));
#53124=CARTESIAN_POINT('Ctrl Pts',(17.6103533965495,-21.2539112056161,-16.8910354226799));
#53125=CARTESIAN_POINT('Ctrl Pts',(17.5317703445183,-21.2138530785411,-16.8954218846925));
#53126=CARTESIAN_POINT('Ctrl Pts',(17.4555708448951,-21.169931219713,-16.899808346705));
#53127=CARTESIAN_POINT('Ctrl Pts',(17.3793713452718,-21.1260093608849,-16.9041948087175));
#53128=CARTESIAN_POINT('Ctrl Pts',(17.3055558437865,-21.0782241494638,-16.9085812707301));
#53129=CARTESIAN_POINT('Ctrl Pts',(17.2345184376722,-21.0268867545577,-16.9129677327426));
#53130=CARTESIAN_POINT('Ctrl Pts',(17.167299168743,-20.9783086554537,-16.9171184300413));
#53131=CARTESIAN_POINT('Ctrl Pts',(17.1023079512147,-20.9263629083338,-16.9212691273401));
#53132=CARTESIAN_POINT('Ctrl Pts',(17.0399060592653,-20.8712826055498,-16.9254198246388));
#53133=CARTESIAN_POINT('Ctrl Pts',(16.9775932241692,-20.8162809106139,-16.9295645982704));
#53134=CARTESIAN_POINT('Ctrl Pts',(16.9178627255451,-20.7581538490648,-16.9337093719019));
#53135=CARTESIAN_POINT('Ctrl Pts',(16.8610458812396,-20.6971770308534,-16.9378541455334));
#53136=CARTESIAN_POINT('Ctrl Pts',(16.8042942087153,-20.6362701561228,-16.9419941649009));
#53137=CARTESIAN_POINT('Ctrl Pts',(16.7504498675423,-20.5725203603437,-16.9461341842684));
#53138=CARTESIAN_POINT('Ctrl Pts',(16.6998090154257,-20.506241628022,-16.9502742036359));
#53139=CARTESIAN_POINT('Ctrl Pts',(16.6491995836852,-20.4400040186794,-16.9544116543072));
#53140=CARTESIAN_POINT('Ctrl Pts',(16.6017899801564,-20.3712409577298,-16.9585491049784));
#53141=CARTESIAN_POINT('Ctrl Pts',(16.5578367768806,-20.3003002730633,-16.9626865556497));
#53142=CARTESIAN_POINT('Ctrl Pts',(16.5138971231855,-20.2293814574863,-16.9668227308571));
#53143=CARTESIAN_POINT('Ctrl Pts',(16.4734120005631,-20.1562867489274,-16.9709589060645));
#53144=CARTESIAN_POINT('Ctrl Pts',(16.4365944037611,-20.0813925475095,-16.9750950812719));
#53145=CARTESIAN_POINT('Ctrl Pts',(16.3997766632186,-20.0064980536954,-16.9792312726275));
#53146=CARTESIAN_POINT('Ctrl Pts',(16.366626681762,-19.9298044742117,-16.983367463983));
#53147=CARTESIAN_POINT('Ctrl Pts',(16.3373106052886,-19.8517110343203,-16.9875036553386));
#53148=CARTESIAN_POINT('Ctrl Pts',(16.3079666664254,-19.773543373383,-16.9916437777855));
#53149=CARTESIAN_POINT('Ctrl Pts',(16.2824640727847,-19.6939736349118,-16.9957839002324));
#53150=CARTESIAN_POINT('Ctrl Pts',(16.2609198329124,-19.6134185415892,-16.9999240226793));
#53151=CARTESIAN_POINT('Ctrl Pts',(16.2393648184702,-19.532823161559,-17.0040662156583));
#53152=CARTESIAN_POINT('Ctrl Pts',(16.2217721969233,-19.4512419037245,-17.0082084086373));
#53153=CARTESIAN_POINT('Ctrl Pts',(16.2082078057625,-19.3691016561093,-17.0123506016162));
#53154=CARTESIAN_POINT('Ctrl Pts',(16.1946210138151,-19.2868257587522,-17.016499635181));
#53155=CARTESIAN_POINT('Ctrl Pts',(16.1850757885661,-19.2039894937103,-17.0206486687457));
#53156=CARTESIAN_POINT('Ctrl Pts',(16.1795860271471,-19.1210244221821,-17.0247977023105));
#53157=CARTESIAN_POINT('Ctrl Pts',(16.1758404729028,-19.06441901585,-17.0276285047975));
#53158=CARTESIAN_POINT('Ctrl Pts',(16.1739816679355,-19.0077536994294,-17.0304593072845));
#53159=CARTESIAN_POINT('Ctrl Pts',(16.1740001363332,-18.9511645205579,-17.0332901097715));
#53160=CARTESIAN_POINT('Ctrl Pts',(16.1700998810729,-18.9511632476738,-17.0332901097715));
#53161=CARTESIAN_POINT('Ctrl Pts',(16.1699051733629,-18.905425756545,-17.0355745863224));
#53162=CARTESIAN_POINT('Ctrl Pts',(16.1917620149477,-18.0111494804083,-17.0802509984337));
#53163=CARTESIAN_POINT('Ctrl Pts',(17.2348044654712,-16.3222275152694,-17.1673193461055));
#53164=CARTESIAN_POINT('Ctrl Pts',(19.3369083681933,-16.2828821706046,-17.2595384003524));
#53165=CARTESIAN_POINT('Ctrl Pts',(20.177011556488,-16.8286170585391,-17.3093655190387));
#53166=CARTESIAN_POINT('Ctrl Pts',(20.294455276885,-16.9206896363574,-17.3168007021646));
#53167=CARTESIAN_POINT('',(16.1741505163153,-18.9531967450726,-16.9667098397546));
#53168=CARTESIAN_POINT('Ctrl Pts',(16.1776746515055,-18.9531940792248,-16.9667098902285));
#53169=CARTESIAN_POINT('Ctrl Pts',(16.1797896608842,-18.4498774694967,-16.9916592919231));
#53170=CARTESIAN_POINT('Ctrl Pts',(16.5671404047359,-17.0883638912152,-17.0590006291781));
#53171=CARTESIAN_POINT('Ctrl Pts',(18.4733994257987,-16.0873963198054,-17.1534395129914));
#53172=CARTESIAN_POINT('Ctrl Pts',(19.8562820548392,-16.5944336060539,-17.2229289951101));
#53173=CARTESIAN_POINT('Ctrl Pts',(20.2917780564658,-16.9241894633618,-17.2500265416684));
#53174=CARTESIAN_POINT('Ctrl Pts',(20.293535888361,-16.9218650751947,-16.4501666918036));
#53175=CARTESIAN_POINT('Ctrl Pts',(20.3601794064216,-16.9730601740388,-16.4543369075911));
#53176=CARTESIAN_POINT('Ctrl Pts',(20.4243360771708,-17.0275684722783,-16.4585071233785));
#53177=CARTESIAN_POINT('Ctrl Pts',(20.4856660020915,-17.0851132286299,-16.462677339166));
#53178=CARTESIAN_POINT('Ctrl Pts',(20.5469851039405,-17.1426478298895,-16.4668468190233));
#53179=CARTESIAN_POINT('Ctrl Pts',(20.6054781157674,-17.2032175098257,-16.4710162988806));
#53180=CARTESIAN_POINT('Ctrl Pts',(20.6608402898758,-17.2665070461995,-16.4751857787379));
#53181=CARTESIAN_POINT('Ctrl Pts',(20.7162093011933,-17.3298043988087,-16.4793557735244));
#53182=CARTESIAN_POINT('Ctrl Pts',(20.7684464051496,-17.3958219277228,-16.483525768311));
#53183=CARTESIAN_POINT('Ctrl Pts',(20.817286518905,-17.4642106062521,-16.4876957630976));
#53184=CARTESIAN_POINT('Ctrl Pts',(20.8661791251708,-17.5326727877516,-16.4918702397225));
#53185=CARTESIAN_POINT('Ctrl Pts',(20.9116671848706,-17.6035108313142,-16.4960447163474));
#53186=CARTESIAN_POINT('Ctrl Pts',(20.9535287399399,-17.6763463743709,-16.5002191929724));
#53187=CARTESIAN_POINT('Ctrl Pts',(20.9954147215154,-17.7492244174694,-16.5043961054332));
#53188=CARTESIAN_POINT('Ctrl Pts',(21.0336697764926,-17.8241018708103,-16.508573017894));
#53189=CARTESIAN_POINT('Ctrl Pts',(21.0681188608709,-17.9005775619065,-16.5127499303549));
#53190=CARTESIAN_POINT('Ctrl Pts',(21.1026261840292,-17.9771825409365,-16.5169339042018));
#53191=CARTESIAN_POINT('Ctrl Pts',(21.1333145214185,-18.0553907244829,-16.5211178780488));
#53192=CARTESIAN_POINT('Ctrl Pts',(21.1600578420673,-18.1347831701783,-16.5253018518957));
#53193=CARTESIAN_POINT('Ctrl Pts',(21.1761504177396,-18.1825569286034,-16.527819524126));
#53194=CARTESIAN_POINT('Ctrl Pts',(21.1908155027428,-18.2307592272839,-16.5303371963562));
#53195=CARTESIAN_POINT('Ctrl Pts',(21.2040345704695,-18.2792970784325,-16.5328548685865));
#53196=CARTESIAN_POINT('Ctrl Pts',(21.2260060426843,-18.3599720602032,-16.5370395029795));
#53197=CARTESIAN_POINT('Ctrl Pts',(21.244061800264,-18.4418747378537,-16.5412241373726));
#53198=CARTESIAN_POINT('Ctrl Pts',(21.2580683099057,-18.5245901651463,-16.5454087717656));
#53199=CARTESIAN_POINT('Ctrl Pts',(21.2720548830146,-18.607187857266,-16.5495874498496));
#53200=CARTESIAN_POINT('Ctrl Pts',(21.2820035803663,-18.6905955514662,-16.5537661279335));
#53201=CARTESIAN_POINT('Ctrl Pts',(21.28783098536,-18.7743844088622,-16.5579448060174));
#53202=CARTESIAN_POINT('Ctrl Pts',(21.2937628424001,-18.8596751213091,-16.5621983839029));
#53203=CARTESIAN_POINT('Ctrl Pts',(21.2954240788116,-18.9453603308623,-16.5664519617883));
#53204=CARTESIAN_POINT('Ctrl Pts',(21.2927814384536,-19.0309781629654,-16.5707055396738));
#53205=CARTESIAN_POINT('Ctrl Pts',(21.2901900308356,-19.1149361263238,-16.5748766536517));
#53206=CARTESIAN_POINT('Ctrl Pts',(21.2834601502021,-19.1988288204156,-16.5790477676297));
#53207=CARTESIAN_POINT('Ctrl Pts',(21.2726129381323,-19.2822186402178,-16.5832188816076));
#53208=CARTESIAN_POINT('Ctrl Pts',(21.2617693659493,-19.3655804777606,-16.587388595928));
#53209=CARTESIAN_POINT('Ctrl Pts',(21.246811265521,-19.4484393203326,-16.5915583102484));
#53210=CARTESIAN_POINT('Ctrl Pts',(21.2278116184524,-19.5303628719687,-16.5957280245688));
#53211=CARTESIAN_POINT('Ctrl Pts',(21.2088126474728,-19.6122835084131,-16.5998975905128));
#53212=CARTESIAN_POINT('Ctrl Pts',(21.1857725205575,-19.6932684721477,-16.6040671564568));
#53213=CARTESIAN_POINT('Ctrl Pts',(21.1588150040535,-19.7728971897365,-16.6082367224009));
#53214=CARTESIAN_POINT('Ctrl Pts',(21.1309096945249,-19.855325554803,-16.6125528851398));
#53215=CARTESIAN_POINT('Ctrl Pts',(21.0988065683011,-19.93630002845,-16.6168690478787));
#53216=CARTESIAN_POINT('Ctrl Pts',(21.0626979316573,-20.015374789571,-16.6211852106176));
#53217=CARTESIAN_POINT('Ctrl Pts',(21.0277655300541,-20.0918736986657,-16.6253607748093));
#53218=CARTESIAN_POINT('Ctrl Pts',(20.9890848280185,-20.1665943642433,-16.629536339001));
#53219=CARTESIAN_POINT('Ctrl Pts',(20.9468767362672,-20.239158323629,-16.6337119031927));
#53220=CARTESIAN_POINT('Ctrl Pts',(20.9025368141418,-20.3153873160988,-16.6380983652052));
#53221=CARTESIAN_POINT('Ctrl Pts',(20.8543041199709,-20.3892355173249,-16.6424848272177));
#53222=CARTESIAN_POINT('Ctrl Pts',(20.8024847707862,-20.4603006175911,-16.6468712892303));
#53223=CARTESIAN_POINT('Ctrl Pts',(20.7506654216015,-20.5313657178572,-16.6512577512428));
#53224=CARTESIAN_POINT('Ctrl Pts',(20.6952598420584,-20.5996473145404,-16.6556442132554));
#53225=CARTESIAN_POINT('Ctrl Pts',(20.6366195645772,-20.664786849695,-16.6600306752679));
#53226=CARTESIAN_POINT('Ctrl Pts',(20.5806774131886,-20.7269292182772,-16.664215309661));
#53227=CARTESIAN_POINT('Ctrl Pts',(20.5215834617877,-20.7864436190212,-16.668399944054));
#53228=CARTESIAN_POINT('Ctrl Pts',(20.4596143354494,-20.8429931690229,-16.6725845784471));
#53229=CARTESIAN_POINT('Ctrl Pts',(20.3977334144921,-20.8994622277398,-16.676763256531));
#53230=CARTESIAN_POINT('Ctrl Pts',(20.3329857844078,-20.9529745107158,-16.6809419346149));
#53231=CARTESIAN_POINT('Ctrl Pts',(20.2656868790094,-21.0032277554359,-16.6851206126989));
#53232=CARTESIAN_POINT('Ctrl Pts',(20.1971816890986,-21.0543817534511,-16.6893741905843));
#53233=CARTESIAN_POINT('Ctrl Pts',(20.1260331836046,-21.1021583691593,-16.6936277684698));
#53234=CARTESIAN_POINT('Ctrl Pts',(20.0526117250174,-21.1462796354719,-16.6978813463552));
#53235=CARTESIAN_POINT('Ctrl Pts',(19.980613684675,-21.1895455249415,-16.7020524603332));
#53236=CARTESIAN_POINT('Ctrl Pts',(19.9064304485057,-21.2292962845166,-16.7062235743111));
#53237=CARTESIAN_POINT('Ctrl Pts',(19.8304414166174,-21.2653128236203,-16.7103946882891));
#53238=CARTESIAN_POINT('Ctrl Pts',(19.7544778835828,-21.3013172770264,-16.7145644026094));
#53239=CARTESIAN_POINT('Ctrl Pts',(19.676710173617,-21.3335898016788,-16.7187341169298));
#53240=CARTESIAN_POINT('Ctrl Pts',(19.5975412827729,-21.3619577699509,-16.7229038312502));
#53241=CARTESIAN_POINT('Ctrl Pts',(19.5183752090976,-21.3903247287691,-16.7270733971942));
#53242=CARTESIAN_POINT('Ctrl Pts',(19.4378084870364,-21.4147872530806,-16.7312429631383));
#53243=CARTESIAN_POINT('Ctrl Pts',(19.356261744668,-21.435221762373,-16.7354125290823));
#53244=CARTESIAN_POINT('Ctrl Pts',(19.271847919437,-21.4563747238033,-16.7397286918212));
#53245=CARTESIAN_POINT('Ctrl Pts',(19.1863843882472,-21.4732110218617,-16.7440448545601));
#53246=CARTESIAN_POINT('Ctrl Pts',(19.1003501078358,-21.4856510411832,-16.7483610172991));
#53247=CARTESIAN_POINT('Ctrl Pts',(19.0171183850596,-21.4976858281838,-16.7525365814907));
#53248=CARTESIAN_POINT('Ctrl Pts',(18.9333529997362,-21.5056063582133,-16.7567121456824));
#53249=CARTESIAN_POINT('Ctrl Pts',(18.8494917538631,-21.5093935275568,-16.7608877098741));
#53250=CARTESIAN_POINT('Ctrl Pts',(18.7613948758223,-21.5133719778208,-16.7652741718866));
#53251=CARTESIAN_POINT('Ctrl Pts',(18.6731927827732,-21.5127885456943,-16.7696606338992));
#53252=CARTESIAN_POINT('Ctrl Pts',(18.5853894488633,-21.5076828645375,-16.7740470959117));
#53253=CARTESIAN_POINT('Ctrl Pts',(18.4975861149534,-21.5025771833808,-16.7784335579242));
#53254=CARTESIAN_POINT('Ctrl Pts',(18.4101821085832,-21.4929493923299,-16.7828200199368));
#53255=CARTESIAN_POINT('Ctrl Pts',(18.3236691980734,-21.4789009939035,-16.7872064819493));
#53256=CARTESIAN_POINT('Ctrl Pts',(18.2411368748189,-21.4654989831133,-16.7913911163424));
#53257=CARTESIAN_POINT('Ctrl Pts',(18.1591082470633,-21.4480243381486,-16.7955757507354));
#53258=CARTESIAN_POINT('Ctrl Pts',(18.0780163119226,-21.4265273085938,-16.7997603851285));
#53259=CARTESIAN_POINT('Ctrl Pts',(17.9970398011144,-21.4050608773998,-16.8039390632124));
#53260=CARTESIAN_POINT('Ctrl Pts',(17.9169977755054,-21.3795835508677,-16.8081177412964));
#53261=CARTESIAN_POINT('Ctrl Pts',(17.8383151283769,-21.3501969499492,-16.8122964193803));
#53262=CARTESIAN_POINT('Ctrl Pts',(17.7582221513468,-21.3202836153289,-16.8165499972658));
#53263=CARTESIAN_POINT('Ctrl Pts',(17.6795382417637,-21.2863195576311,-16.8208035751512));
#53264=CARTESIAN_POINT('Ctrl Pts',(17.6026975961514,-21.248465734786,-16.8250571530366));
#53265=CARTESIAN_POINT('Ctrl Pts',(17.5273466563964,-21.2113457821624,-16.8292282670146));
#53266=CARTESIAN_POINT('Ctrl Pts',(17.4537685795459,-21.1704857525209,-16.8333993809925));
#53267=CARTESIAN_POINT('Ctrl Pts',(17.3823529481854,-21.126086071737,-16.8375704949705));
#53268=CARTESIAN_POINT('Ctrl Pts',(17.3109612810297,-21.0817012896948,-16.8417402092909));
#53269=CARTESIAN_POINT('Ctrl Pts',(17.2417310086115,-21.0337794581179,-16.8459099236112));
#53270=CARTESIAN_POINT('Ctrl Pts',(17.1750254175657,-20.9825659928512,-16.8500796379316));
#53271=CARTESIAN_POINT('Ctrl Pts',(17.1083222001911,-20.9313543499794,-16.8542492038757));
#53272=CARTESIAN_POINT('Ctrl Pts',(17.0441438499404,-20.8768515871274,-16.8584187698197));
#53273=CARTESIAN_POINT('Ctrl Pts',(16.9828219564691,-20.8193444941562,-16.8625883357638));
#53274=CARTESIAN_POINT('Ctrl Pts',(16.9193440608722,-20.7598155227389,-16.8669044985027));
#53275=CARTESIAN_POINT('Ctrl Pts',(16.858927610118,-20.6970673867186,-16.8712206612416));
#53276=CARTESIAN_POINT('Ctrl Pts',(16.8018987983269,-20.6314597186278,-16.8755368239805));
#53277=CARTESIAN_POINT('Ctrl Pts',(16.7467276940815,-20.5679892134243,-16.8797123881722));
#53278=CARTESIAN_POINT('Ctrl Pts',(16.6947271674384,-20.5018430132072,-16.8838879523639));
#53279=CARTESIAN_POINT('Ctrl Pts',(16.6461502555163,-20.4333788996942,-16.8880635165556));
#53280=CARTESIAN_POINT('Ctrl Pts',(16.5951198392536,-20.3614568265656,-16.8924499785681));
#53281=CARTESIAN_POINT('Ctrl Pts',(16.5478682932594,-20.2869770238506,-16.8968364405806));
#53282=CARTESIAN_POINT('Ctrl Pts',(16.5046350837971,-20.210384706838,-16.9012229025932));
#53283=CARTESIAN_POINT('Ctrl Pts',(16.4614018743349,-20.1337923898254,-16.9056093646057));
#53284=CARTESIAN_POINT('Ctrl Pts',(16.4221871920777,-20.0550881117615,-16.9099958266183));
#53285=CARTESIAN_POINT('Ctrl Pts',(16.3871718743353,-19.9747403133684,-16.9143822886308));
#53286=CARTESIAN_POINT('Ctrl Pts',(16.3503471043863,-19.8902404606612,-16.9189954255353));
#53287=CARTESIAN_POINT('Ctrl Pts',(16.3180481684136,-19.8036540013278,-16.9236085624399));
#53288=CARTESIAN_POINT('Ctrl Pts',(16.290492039707,-19.7154584782324,-16.9282216993444));
#53289=CARTESIAN_POINT('Ctrl Pts',(16.2630147812854,-19.6275153855894,-16.9328216326736));
#53290=CARTESIAN_POINT('Ctrl Pts',(16.2402533773008,-19.5379726851084,-16.9374215660028));
#53291=CARTESIAN_POINT('Ctrl Pts',(16.2223767943064,-19.4473270360289,-16.9420214993319));
#53292=CARTESIAN_POINT('Ctrl Pts',(16.2045882581333,-19.3571278403507,-16.9465987767929));
#53293=CARTESIAN_POINT('Ctrl Pts',(16.1916366671696,-19.2658368103364,-16.9511760542539));
#53294=CARTESIAN_POINT('Ctrl Pts',(16.1836406660146,-19.17396231111,-16.9557533317148));
#53295=CARTESIAN_POINT('Ctrl Pts',(16.1772607284146,-19.100656472263,-16.9594055003442));
#53296=CARTESIAN_POINT('Ctrl Pts',(16.1740347749072,-19.0269796000837,-16.9630576689735));
#53297=CARTESIAN_POINT('Ctrl Pts',(16.1740002797795,-18.9531968587196,-16.9667098376028));
#53298=CARTESIAN_POINT('Origin',(18.734,-18.952,1.76670989022851));
#53299=CARTESIAN_POINT('',(20.295887153474,-16.918834963786,-15.6501589836526));
#53300=CARTESIAN_POINT('',(20.293535888361,-16.9218650751948,-15.7166572089129));
#53301=CARTESIAN_POINT('',(20.293535888361,-16.9218650751948,1.76670989022851));
#53302=CARTESIAN_POINT('',(16.1740007055014,-18.9500994299064,-16.2332901098004));
#53303=CARTESIAN_POINT('Ctrl Pts',(20.293535888361,-16.9218650751948,-15.7166572089129));
#53304=CARTESIAN_POINT('Ctrl Pts',(20.3624598556926,-16.9748119997112,-15.7209678975543));
#53305=CARTESIAN_POINT('Ctrl Pts',(20.428659775607,-17.0312538804154,-15.7252785861958));
#53306=CARTESIAN_POINT('Ctrl Pts',(20.4917771265502,-17.090866051737,-15.7295892748372));
#53307=CARTESIAN_POINT('Ctrl Pts',(20.5529161182364,-17.148609730652,-15.7337648486385));
#53308=CARTESIAN_POINT('Ctrl Pts',(20.6111626415143,-17.2093275174942,-15.7379404224398));
#53309=CARTESIAN_POINT('Ctrl Pts',(20.6662297662403,-17.2726881973693,-15.7421159962412));
#53310=CARTESIAN_POINT('Ctrl Pts',(20.7239697161052,-17.3391242515049,-15.7464942423026));
#53311=CARTESIAN_POINT('Ctrl Pts',(20.7782134511509,-17.4084658019913,-15.750872488364));
#53312=CARTESIAN_POINT('Ctrl Pts',(20.8286804992412,-17.4802956797988,-15.7552507344255));
#53313=CARTESIAN_POINT('Ctrl Pts',(20.8791475473314,-17.5521255576064,-15.7596289804869));
#53314=CARTESIAN_POINT('Ctrl Pts',(20.9258376665922,-17.626443235887,-15.7640072265483));
#53315=CARTESIAN_POINT('Ctrl Pts',(20.9685260259021,-17.7028028820213,-15.7683854726098));
#53316=CARTESIAN_POINT('Ctrl Pts',(21.0093266510939,-17.775785806455,-15.7725701070028));
#53317=CARTESIAN_POINT('Ctrl Pts',(21.0466238491571,-17.850905564207,-15.7767547413958));
#53318=CARTESIAN_POINT('Ctrl Pts',(21.0801878476017,-17.9277917283258,-15.7809393757889));
#53319=CARTESIAN_POINT('Ctrl Pts',(21.1137040718491,-18.0045684545067,-15.7851180538728));
#53320=CARTESIAN_POINT('Ctrl Pts',(21.1434974687763,-18.0831061749367,-15.7892967319568));
#53321=CARTESIAN_POINT('Ctrl Pts',(21.1693835453414,-18.1630088802273,-15.7934754100407));
#53322=CARTESIAN_POINT('Ctrl Pts',(21.195733611225,-18.2443437840852,-15.7977289879261));
#53323=CARTESIAN_POINT('Ctrl Pts',(21.218034666248,-18.3270926679896,-15.8019825658116));
#53324=CARTESIAN_POINT('Ctrl Pts',(21.2361429171342,-18.4108153529199,-15.806236143697));
#53325=CARTESIAN_POINT('Ctrl Pts',(21.2539001042416,-18.4929149102315,-15.810407257675));
#53326=CARTESIAN_POINT('Ctrl Pts',(21.2676255061034,-18.575950377106,-15.8145783716529));
#53327=CARTESIAN_POINT('Ctrl Pts',(21.2772339776254,-18.6594919914747,-15.8187494856309));
#53328=CARTESIAN_POINT('Ctrl Pts',(21.2868392249321,-18.7430055726479,-15.8229191999513));
#53329=CARTESIAN_POINT('Ctrl Pts',(21.2923302330118,-18.8270245073654,-15.8270889142716));
#53330=CARTESIAN_POINT('Ctrl Pts',(21.2936734448665,-18.9111116685929,-15.831258628592));
#53331=CARTESIAN_POINT('Ctrl Pts',(21.295016608924,-18.9951958376383,-15.8354281945361));
#53332=CARTESIAN_POINT('Ctrl Pts',(21.2922122637205,-19.0793477683788,-15.8395977604801));
#53333=CARTESIAN_POINT('Ctrl Pts',(21.285278964847,-19.1631294473285,-15.8437673264241));
#53334=CARTESIAN_POINT('Ctrl Pts',(21.2781018997383,-19.2498567867541,-15.8480834891631));
#53335=CARTESIAN_POINT('Ctrl Pts',(21.2665001742353,-19.3361868282291,-15.852399651902));
#53336=CARTESIAN_POINT('Ctrl Pts',(21.2505527597975,-19.421640508427,-15.8567158146409));
#53337=CARTESIAN_POINT('Ctrl Pts',(21.2351248307076,-19.5043105439806,-15.8608913788326));
#53338=CARTESIAN_POINT('Ctrl Pts',(21.2156301415435,-19.5861599891145,-15.8650669430243));
#53339=CARTESIAN_POINT('Ctrl Pts',(21.192191685782,-19.6667682393282,-15.8692425072159));
#53340=CARTESIAN_POINT('Ctrl Pts',(21.1675694093396,-19.7514478206323,-15.8736289692285));
#53341=CARTESIAN_POINT('Ctrl Pts',(21.1385946886759,-19.8347569748337,-15.878015431241));
#53342=CARTESIAN_POINT('Ctrl Pts',(21.1054674445918,-19.9162313826262,-15.8824018932535));
#53343=CARTESIAN_POINT('Ctrl Pts',(21.0723402005077,-19.9977057904187,-15.8867883552661));
#53344=CARTESIAN_POINT('Ctrl Pts',(21.0350607478796,-20.0773449585575,-15.8911748172786));
#53345=CARTESIAN_POINT('Ctrl Pts',(20.9938836431737,-20.1547160593073,-15.8955612792911));
#53346=CARTESIAN_POINT('Ctrl Pts',(20.9546011580944,-20.2285272010203,-15.8997459136842));
#53347=CARTESIAN_POINT('Ctrl Pts',(20.9116255956986,-20.3005491422943,-15.9039305480772));
#53348=CARTESIAN_POINT('Ctrl Pts',(20.8651440549404,-20.3703881757446,-15.9081151824703));
#53349=CARTESIAN_POINT('Ctrl Pts',(20.8187286749022,-20.4401278019752,-15.9122938605542));
#53350=CARTESIAN_POINT('Ctrl Pts',(20.7688174815646,-20.5076903123668,-15.9164725386382));
#53351=CARTESIAN_POINT('Ctrl Pts',(20.7156435935688,-20.5727062250969,-15.9206512167221));
#53352=CARTESIAN_POINT('Ctrl Pts',(20.6615166018461,-20.6388875013365,-15.9249047946076));
#53353=CARTESIAN_POINT('Ctrl Pts',(20.6040090238882,-20.7024295607932,-15.929158372493));
#53354=CARTESIAN_POINT('Ctrl Pts',(20.5434131480185,-20.7629732355222,-15.9334119503784));
#53355=CARTESIAN_POINT('Ctrl Pts',(20.4839920414457,-20.8223431529752,-15.9375830643564));
#53356=CARTESIAN_POINT('Ctrl Pts',(20.4216016541568,-20.878829567176,-15.9417541783343));
#53357=CARTESIAN_POINT('Ctrl Pts',(20.3565572606157,-20.9321282625181,-15.9459252923123));
#53358=CARTESIAN_POINT('Ctrl Pts',(20.2915346933491,-20.9854090729684,-15.9500950066327));
#53359=CARTESIAN_POINT('Ctrl Pts',(20.2238602440649,-21.0355039976099,-15.954264720953));
#53360=CARTESIAN_POINT('Ctrl Pts',(20.1538833036554,-21.0821482117451,-15.9584344352734));
#53361=CARTESIAN_POINT('Ctrl Pts',(20.0839088533259,-21.1287907660788,-15.9626040012174));
#53362=CARTESIAN_POINT('Ctrl Pts',(20.0116324580351,-21.1719825996021,-15.9667735671615));
#53363=CARTESIAN_POINT('Ctrl Pts',(19.937432461597,-21.211502226238,-15.9709431331055));
#53364=CARTESIAN_POINT('Ctrl Pts',(19.8606236848194,-21.2524113141939,-15.9752592958444));
#53365=CARTESIAN_POINT('Ctrl Pts',(19.7817539879933,-21.2893849131306,-15.9795754585833));
#53366=CARTESIAN_POINT('Ctrl Pts',(19.7012689333162,-21.3222301176555,-15.9838916213223));
#53367=CARTESIAN_POINT('Ctrl Pts',(19.6234056708299,-21.3540053930976,-15.9880671855139));
#53368=CARTESIAN_POINT('Ctrl Pts',(19.5440311349293,-21.3819169968656,-15.9922427497056));
#53369=CARTESIAN_POINT('Ctrl Pts',(19.4635655614735,-21.4058406817705,-15.9964183138973));
#53370=CARTESIAN_POINT('Ctrl Pts',(19.3790358631909,-21.4309726951269,-16.0008047759098));
#53371=CARTESIAN_POINT('Ctrl Pts',(19.2933025817205,-21.4517032054839,-16.0051912379224));
#53372=CARTESIAN_POINT('Ctrl Pts',(19.2068643494563,-21.4679489873631,-16.0095776999349));
#53373=CARTESIAN_POINT('Ctrl Pts',(19.1204261171922,-21.4841947692422,-16.0139641619475));
#53374=CARTESIAN_POINT('Ctrl Pts',(19.0332835193119,-21.4959558204205,-16.01835062396));
#53375=CARTESIAN_POINT('Ctrl Pts',(18.9459382820314,-21.5032119011579,-16.0227370859726));
#53376=CARTESIAN_POINT('Ctrl Pts',(18.862611928595,-21.5101341188644,-16.0269217203656));
#53377=CARTESIAN_POINT('Ctrl Pts',(18.7787910168741,-21.5129825827272,-16.0311063547587));
#53378=CARTESIAN_POINT('Ctrl Pts',(18.6949078655888,-21.5117015070174,-16.0352909891517));
#53379=CARTESIAN_POINT('Ctrl Pts',(18.6111441115866,-21.5104222547603,-16.0394696672357));
#53380=CARTESIAN_POINT('Ctrl Pts',(18.5273187500332,-21.5050251452316,-16.0436483453196));
#53381=CARTESIAN_POINT('Ctrl Pts',(18.4438686393689,-21.4955062008138,-16.0478270234036));
#53382=CARTESIAN_POINT('Ctrl Pts',(18.3589227454455,-21.4858166361585,-16.052080601289));
#53383=CARTESIAN_POINT('Ctrl Pts',(18.2743661679602,-21.4718559754809,-16.0563341791745));
#53384=CARTESIAN_POINT('Ctrl Pts',(18.1906591204409,-21.4536755762089,-16.0605877570599));
#53385=CARTESIAN_POINT('Ctrl Pts',(18.1085748973785,-21.4358476394529,-16.0647588710379));
#53386=CARTESIAN_POINT('Ctrl Pts',(18.0273080288923,-21.413962221893,-16.0689299850158));
#53387=CARTESIAN_POINT('Ctrl Pts',(17.9472849642516,-21.3881197533223,-16.0731010989937));
#53388=CARTESIAN_POINT('Ctrl Pts',(17.8672887521231,-21.3622859564417,-16.0772708133141));
#53389=CARTESIAN_POINT('Ctrl Pts',(17.7885359523432,-21.3324978868904,-16.0814405276345));
#53390=CARTESIAN_POINT('Ctrl Pts',(17.7114383592364,-21.2989059825308,-16.0856102419549));
#53391=CARTESIAN_POINT('Ctrl Pts',(17.634343509593,-21.2653152735153,-16.0897798078989));
#53392=CARTESIAN_POINT('Ctrl Pts',(17.558904170915,-21.2279211833515,-16.0939493738429));
#53393=CARTESIAN_POINT('Ctrl Pts',(17.485511368273,-21.1869219531,-16.098118939787));
#53394=CARTESIAN_POINT('Ctrl Pts',(17.4095381652297,-21.1444812404909,-16.1024351025259));
#53395=CARTESIAN_POINT('Ctrl Pts',(17.3357585487131,-21.098177414705,-16.1067512652648));
#53396=CARTESIAN_POINT('Ctrl Pts',(17.2645758959971,-21.0482807070083,-16.1110674280037));
#53397=CARTESIAN_POINT('Ctrl Pts',(17.1957120107063,-21.0000093793167,-16.1152429921954));
#53398=CARTESIAN_POINT('Ctrl Pts',(17.1292788382186,-20.948375977651,-16.1194185563871));
#53399=CARTESIAN_POINT('Ctrl Pts',(17.0656083164573,-20.8936666012181,-16.1235941205788));
#53400=CARTESIAN_POINT('Ctrl Pts',(16.9987219480043,-20.8361939842407,-16.1279805825913));
#53401=CARTESIAN_POINT('Ctrl Pts',(16.9348850702689,-20.7753268941812,-16.1323670446039));
#53402=CARTESIAN_POINT('Ctrl Pts',(16.8744375629656,-20.7114395535996,-16.1367535066164));
#53403=CARTESIAN_POINT('Ctrl Pts',(16.8139900556624,-20.647552213018,-16.141139968629));
#53404=CARTESIAN_POINT('Ctrl Pts',(16.7569322374057,-20.5806451127529,-16.1455264306415));
#53405=CARTESIAN_POINT('Ctrl Pts',(16.703552701499,-20.5111291697643,-16.149912892654));
#53406=CARTESIAN_POINT('Ctrl Pts',(16.6525544398241,-20.4447143500982,-16.1541036735168));
#53407=CARTESIAN_POINT('Ctrl Pts',(16.6047208600206,-20.3756679864259,-16.1582944543796));
#53408=CARTESIAN_POINT('Ctrl Pts',(16.5603345705066,-20.304323408296,-16.1624852352424));
#53409=CARTESIAN_POINT('Ctrl Pts',(16.516010837252,-20.2330793803581,-16.1666701097864));
#53410=CARTESIAN_POINT('Ctrl Pts',(16.4751249866854,-20.1595439541278,-16.1708549843304));
#53411=CARTESIAN_POINT('Ctrl Pts',(16.437918752824,-20.0840825528056,-16.1750398588744));
#53412=CARTESIAN_POINT('Ctrl Pts',(16.4007539244065,-20.0087051296905,-16.1792200762261));
#53413=CARTESIAN_POINT('Ctrl Pts',(16.3672607802463,-19.9314063968238,-16.1834002935778));
#53414=CARTESIAN_POINT('Ctrl Pts',(16.3376364602565,-19.8525785836828,-16.1875805109294));
#53415=CARTESIAN_POINT('Ctrl Pts',(16.3080359860442,-19.7738142221415,-16.1917573634601));
#53416=CARTESIAN_POINT('Ctrl Pts',(16.2822983085876,-19.6935236530688,-16.1959342159908));
#53417=CARTESIAN_POINT('Ctrl Pts',(16.2605729619717,-19.6121202068944,-16.2001110685215));
#53418=CARTESIAN_POINT('Ctrl Pts',(16.2388581016535,-19.5307560521889,-16.2042859049868));
#53419=CARTESIAN_POINT('Ctrl Pts',(16.2211518401956,-19.4482805298204,-16.2084607414521));
#53420=CARTESIAN_POINT('Ctrl Pts',(16.2075538451849,-19.3651220483341,-16.2126355779174));
#53421=CARTESIAN_POINT('Ctrl Pts',(16.1939550163507,-19.2819584676039,-16.216810670382));
#53422=CARTESIAN_POINT('Ctrl Pts',(16.1844650395067,-19.1981122945307,-16.2209857628465));
#53423=CARTESIAN_POINT('Ctrl Pts',(16.1791322578279,-19.1140210480408,-16.2251608553111));
#53424=CARTESIAN_POINT('Ctrl Pts',(16.1756711337436,-19.0594434830796,-16.2278706067979));
#53425=CARTESIAN_POINT('Ctrl Pts',(16.1739601228212,-19.0047628516759,-16.2305803582847));
#53426=CARTESIAN_POINT('Ctrl Pts',(16.174000705501,-18.9500994304892,-16.2332901097715));
#53427=CARTESIAN_POINT('Ctrl Pts',(16.1740007055014,-18.9500994299065,-16.2332901098004));
#53428=CARTESIAN_POINT('Ctrl Pts',(16.1740727513108,-18.8530563258851,-16.2381006886061));
#53429=CARTESIAN_POINT('Ctrl Pts',(16.1796667621363,-18.7562381388328,-16.2429112674118));
#53430=CARTESIAN_POINT('Ctrl Pts',(16.1906824963738,-18.6602191305988,-16.2477218462176));
#53431=CARTESIAN_POINT('Ctrl Pts',(16.2018903455192,-18.5625255464786,-16.2526163217372));
#53432=CARTESIAN_POINT('Ctrl Pts',(16.2187106399962,-18.465659449398,-16.2575107972569));
#53433=CARTESIAN_POINT('Ctrl Pts',(16.2409867483463,-18.3702054253614,-16.2624052727765));
#53434=CARTESIAN_POINT('Ctrl Pts',(16.2632628566963,-18.2747514013248,-16.2672997482962));
#53435=CARTESIAN_POINT('Ctrl Pts',(16.2909946214078,-18.1807095711099,-16.2721942238158));
#53436=CARTESIAN_POINT('Ctrl Pts',(16.3239764935689,-18.088642195582,-16.2770886993355));
#53437=CARTESIAN_POINT('Ctrl Pts',(16.3521750361989,-18.0099272639074,-16.2812733337285));
#53438=CARTESIAN_POINT('Ctrl Pts',(16.3842865295797,-17.9324488089606,-16.2854579681216));
#53439=CARTESIAN_POINT('Ctrl Pts',(16.4201827606336,-17.8566234515881,-16.2896426025146));
#53440=CARTESIAN_POINT('Ctrl Pts',(16.4560278978456,-17.7809060222267,-16.2938212805986));
#53441=CARTESIAN_POINT('Ctrl Pts',(16.4956468770877,-17.7068374289188,-16.2979999586825));
#53442=CARTESIAN_POINT('Ctrl Pts',(16.5388624466768,-17.6348169747563,-16.3021786367664));
#53443=CARTESIAN_POINT('Ctrl Pts',(16.5828526242923,-17.561505605713,-16.3064322146519));
#53444=CARTESIAN_POINT('Ctrl Pts',(16.6305694356435,-17.4903169777092,-16.3106857925373));
#53445=CARTESIAN_POINT('Ctrl Pts',(16.6817755898823,-17.4216487427662,-16.3149393704227));
#53446=CARTESIAN_POINT('Ctrl Pts',(16.7319890129005,-17.3543117755527,-16.3191104844007));
#53447=CARTESIAN_POINT('Ctrl Pts',(16.7855574030481,-17.289398733779,-16.3232815983786));
#53448=CARTESIAN_POINT('Ctrl Pts',(16.8422127801053,-17.2272562176824,-16.3274527123566));
#53449=CARTESIAN_POINT('Ctrl Pts',(16.8988491459036,-17.1651345541072,-16.331622426677));
#53450=CARTESIAN_POINT('Ctrl Pts',(16.9585701316816,-17.1057819095285,-16.3357921409973));
#53451=CARTESIAN_POINT('Ctrl Pts',(17.0210683042877,-17.0495108394989,-16.3399618553177));
#53452=CARTESIAN_POINT('Ctrl Pts',(17.0835642529406,-16.9932417718355,-16.3441314212617));
#53453=CARTESIAN_POINT('Ctrl Pts',(17.1488368494855,-16.9400543678788,-16.3483009872058));
#53454=CARTESIAN_POINT('Ctrl Pts',(17.2165437463576,-16.8902224857465,-16.3524705531498));
#53455=CARTESIAN_POINT('Ctrl Pts',(17.2866311341982,-16.8386385761127,-16.3567867158888));
#53456=CARTESIAN_POINT('Ctrl Pts',(17.3593267625534,-16.790650851497,-16.3611028786277));
#53457=CARTESIAN_POINT('Ctrl Pts',(17.4342176396319,-16.7465146076938,-16.3654190413666));
#53458=CARTESIAN_POINT('Ctrl Pts',(17.5066689542667,-16.7038160973902,-16.3695946055583));
#53459=CARTESIAN_POINT('Ctrl Pts',(17.5811742544606,-16.664722174367,-16.37377016975));
#53460=CARTESIAN_POINT('Ctrl Pts',(17.6573356824289,-16.6294165359951,-16.3779457339416));
#53461=CARTESIAN_POINT('Ctrl Pts',(17.7373438430673,-16.5923276937602,-16.3823321959542));
#53462=CARTESIAN_POINT('Ctrl Pts',(17.8191792885611,-16.5594201038736,-16.3867186579667));
#53463=CARTESIAN_POINT('Ctrl Pts',(17.902360657527,-16.5308482071437,-16.3911051199793));
#53464=CARTESIAN_POINT('Ctrl Pts',(17.985542026493,-16.5022763104139,-16.3954915819918));
#53465=CARTESIAN_POINT('Ctrl Pts',(18.0700687402227,-16.4780401936422,-16.3998780440043));
#53466=CARTESIAN_POINT('Ctrl Pts',(18.155447269861,-16.4582324209244,-16.4042645060169));
#53467=CARTESIAN_POINT('Ctrl Pts',(18.2369040239202,-16.4393344980206,-16.4084494803759));
#53468=CARTESIAN_POINT('Ctrl Pts',(18.3194392781939,-16.4243966729015,-16.4126344547349));
#53469=CARTESIAN_POINT('Ctrl Pts',(18.4026332182035,-16.4135366743004,-16.4168194290939));
#53470=CARTESIAN_POINT('Ctrl Pts',(18.4856850454026,-16.4026952268693,-16.4209972546333));
#53471=CARTESIAN_POINT('Ctrl Pts',(18.5693928687512,-16.3959178140199,-16.4251750801727));
#53472=CARTESIAN_POINT('Ctrl Pts',(18.6533252588854,-16.3932714903402,-16.4293529057121));
#53473=CARTESIAN_POINT('Ctrl Pts',(18.7371760689814,-16.3906277388162,-16.4335266705169));
#53474=CARTESIAN_POINT('Ctrl Pts',(18.821250555471,-16.3921071193265,-16.4377004353216));
#53475=CARTESIAN_POINT('Ctrl Pts',(18.9051115090561,-16.3977249851536,-16.4418742001264));
#53476=CARTESIAN_POINT('Ctrl Pts',(18.9889161108074,-16.4033390759575,-16.4460451602969));
#53477=CARTESIAN_POINT('Ctrl Pts',(19.0725070069923,-16.4130860985607,-16.4502161204674));
#53478=CARTESIAN_POINT('Ctrl Pts',(19.1554476929898,-16.426929339192,-16.4543870806379));
#53479=CARTESIAN_POINT('Ctrl Pts',(19.238357526517,-16.4407674303823,-16.4585564892849));
#53480=CARTESIAN_POINT('Ctrl Pts',(19.3206171772897,-16.4586986359201,-16.4627258979319));
#53481=CARTESIAN_POINT('Ctrl Pts',(19.4017973253963,-16.480634642107,-16.4668953065789));
#53482=CARTESIAN_POINT('Ctrl Pts',(19.4830102717198,-16.5025795108288,-16.4710663997408));
#53483=CARTESIAN_POINT('Ctrl Pts',(19.5631423969829,-16.5285323016481,-16.4752374929027));
#53484=CARTESIAN_POINT('Ctrl Pts',(19.6417773433661,-16.5583541834952,-16.4794085860646));
#53485=CARTESIAN_POINT('Ctrl Pts',(19.7204244341719,-16.5881806710494,-16.4835803234123));
#53486=CARTESIAN_POINT('Ctrl Pts',(19.7975734594219,-16.6218772648632,-16.48775206076));
#53487=CARTESIAN_POINT('Ctrl Pts',(19.8728278889775,-16.6592568745524,-16.4919237981077));
#53488=CARTESIAN_POINT('Ctrl Pts',(19.9481771492369,-16.6966835875779,-16.4961007924057));
#53489=CARTESIAN_POINT('Ctrl Pts',(20.0216266360836,-16.7378023734385,-16.5002777867036));
#53490=CARTESIAN_POINT('Ctrl Pts',(20.0928045893757,-16.7823801973867,-16.5044547810015));
#53491=CARTESIAN_POINT('Ctrl Pts',(20.1619637771322,-16.8256936948059,-16.5085133064234));
#53492=CARTESIAN_POINT('Ctrl Pts',(20.2289782742483,-16.8722723536246,-16.5125718318452));
#53493=CARTESIAN_POINT('Ctrl Pts',(20.293535888361,-16.9218650751947,-16.516630357267));
#53494=CARTESIAN_POINT('',(16.1740005630998,-18.9536979607663,-16.1667098902285));
#53495=CARTESIAN_POINT('Ctrl Pts',(16.1740005630998,-18.9536979607663,-16.1667098902285));
#53496=CARTESIAN_POINT('Ctrl Pts',(16.1739457994085,-18.8711312597184,-16.1708335669039));
#53497=CARTESIAN_POINT('Ctrl Pts',(16.1778897355288,-18.7884072256501,-16.1749572435793));
#53498=CARTESIAN_POINT('Ctrl Pts',(16.185851592152,-18.7059518510905,-16.1790809202548));
#53499=CARTESIAN_POINT('Ctrl Pts',(16.193849980064,-18.6231181475504,-16.1832235175451));
#53500=CARTESIAN_POINT('Ctrl Pts',(16.2059033176551,-18.5405560554534,-16.1873661148355));
#53501=CARTESIAN_POINT('Ctrl Pts',(16.2219780566694,-18.4586991220099,-16.1915087121259));
#53502=CARTESIAN_POINT('Ctrl Pts',(16.23794569149,-18.3773875921872,-16.1956237077524));
#53503=CARTESIAN_POINT('Ctrl Pts',(16.2578812222445,-18.2967723256482,-16.1997387033789));
#53504=CARTESIAN_POINT('Ctrl Pts',(16.2816998746989,-18.2172727748012,-16.2038536990054));
#53505=CARTESIAN_POINT('Ctrl Pts',(16.3055083094402,-18.1378073276299,-16.2079669293832));
#53506=CARTESIAN_POINT('Ctrl Pts',(16.33319642467,-18.0594570997615,-16.2120801597611));
#53507=CARTESIAN_POINT('Ctrl Pts',(16.3646289972004,-17.9826285278118,-16.2161933901389));
#53508=CARTESIAN_POINT('Ctrl Pts',(16.3960581246075,-17.9058083765508,-16.2203061696919));
#53509=CARTESIAN_POINT('Ctrl Pts',(16.4312307139714,-17.8305099882011,-16.2244189492448));
#53510=CARTESIAN_POINT('Ctrl Pts',(16.4699631644818,-17.7571204213743,-16.2285317287977));
#53511=CARTESIAN_POINT('Ctrl Pts',(16.5091807554343,-17.6828116189603,-16.2326960226666));
#53512=CARTESIAN_POINT('Ctrl Pts',(16.5520477937181,-17.6104602387452,-16.2368603165354));
#53513=CARTESIAN_POINT('Ctrl Pts',(16.5983263505015,-17.5404412648289,-16.2410246104042));
#53514=CARTESIAN_POINT('Ctrl Pts',(16.6440925485816,-17.4711974842891,-16.2451428005836));
#53515=CARTESIAN_POINT('Ctrl Pts',(16.6931947649454,-17.404235069768,-16.2492609907631));
#53516=CARTESIAN_POINT('Ctrl Pts',(16.7453611252722,-17.3398847975652,-16.2533791809425));
#53517=CARTESIAN_POINT('Ctrl Pts',(16.7984034996616,-17.2744539105174,-16.257566526656));
#53518=CARTESIAN_POINT('Ctrl Pts',(16.8546135316781,-17.2117240820489,-16.2617538723695));
#53519=CARTESIAN_POINT('Ctrl Pts',(16.9136665630955,-17.1520038393131,-16.265941218083));
#53520=CARTESIAN_POINT('Ctrl Pts',(16.9727195945129,-17.0922835965773,-16.2701285637965));
#53521=CARTESIAN_POINT('Ctrl Pts',(17.0346152026565,-17.0355732283015,-16.27431590951));
#53522=CARTESIAN_POINT('Ctrl Pts',(17.098995528925,-16.9821369642626,-16.2785032552236));
#53523=CARTESIAN_POINT('Ctrl Pts',(17.1633341687151,-16.9287353003848,-16.2826878896166));
#53524=CARTESIAN_POINT('Ctrl Pts',(17.2304115572044,-16.8783896656035,-16.2868725240096));
#53525=CARTESIAN_POINT('Ctrl Pts',(17.2999052707799,-16.8313934104547,-16.2910571584027));
#53526=CARTESIAN_POINT('Ctrl Pts',(17.3693000686557,-16.7844640486581,-16.2952358364866));
#53527=CARTESIAN_POINT('Ctrl Pts',(17.4411039821924,-16.7408748523863,-16.2994145145706));
#53528=CARTESIAN_POINT('Ctrl Pts',(17.5149611920067,-16.7008793047448,-16.3035931926545));
#53529=CARTESIAN_POINT('Ctrl Pts',(17.5901422392268,-16.6601668656561,-16.3078467705399));
#53530=CARTESIAN_POINT('Ctrl Pts',(17.6674505464318,-16.6231784826193,-16.3121003484254));
#53531=CARTESIAN_POINT('Ctrl Pts',(17.746479455157,-16.5901356572587,-16.3163539263108));
#53532=CARTESIAN_POINT('Ctrl Pts',(17.8239762342743,-16.5577334315455,-16.3205250402888));
#53533=CARTESIAN_POINT('Ctrl Pts',(17.9031270518497,-16.5291253296779,-16.3246961542667));
#53534=CARTESIAN_POINT('Ctrl Pts',(17.9835248188147,-16.5044732887209,-16.3288672682447));
#53535=CARTESIAN_POINT('Ctrl Pts',(18.0638956075326,-16.4798295199942,-16.333036982565));
#53536=CARTESIAN_POINT('Ctrl Pts',(18.1455120751843,-16.4591393105014,-16.3372066968854));
#53537=CARTESIAN_POINT('Ctrl Pts',(18.2279505020326,-16.4425152111226,-16.3413764112058));
#53538=CARTESIAN_POINT('Ctrl Pts',(18.3103859953678,-16.4258917033007,-16.3455459771498));
#53539=CARTESIAN_POINT('Ctrl Pts',(18.3936429386218,-16.4133341080144,-16.3497155430939));
#53540=CARTESIAN_POINT('Ctrl Pts',(18.4772872562555,-16.404903895178,-16.3538851090379));
#53541=CARTESIAN_POINT('Ctrl Pts',(18.563872404911,-16.3961772864581,-16.3582012717768));
#53542=CARTESIAN_POINT('Ctrl Pts',(18.6508721501762,-16.3918737507556,-16.3625174345158));
#53543=CARTESIAN_POINT('Ctrl Pts',(18.7378010569178,-16.3920028218831,-16.3668335972547));
#53544=CARTESIAN_POINT('Ctrl Pts',(18.8218982636656,-16.3921276885323,-16.3710091614464));
#53545=CARTESIAN_POINT('Ctrl Pts',(18.9059287081098,-16.3964007414036,-16.3751847256381));
#53546=CARTESIAN_POINT('Ctrl Pts',(18.9894564259426,-16.4047775883436,-16.3793602898297));
#53547=CARTESIAN_POINT('Ctrl Pts',(19.077202930235,-16.4135775299085,-16.3837467518423));
#53548=CARTESIAN_POINT('Ctrl Pts',(19.1643940106306,-16.4269066375599,-16.3881332138548));
#53549=CARTESIAN_POINT('Ctrl Pts',(19.2505367177893,-16.4446528323394,-16.3925196758674));
#53550=CARTESIAN_POINT('Ctrl Pts',(19.336679424948,-16.462399027119,-16.3969061378799));
#53551=CARTESIAN_POINT('Ctrl Pts',(19.4217732165569,-16.4845620891763,-16.4012925998925));
#53552=CARTESIAN_POINT('Ctrl Pts',(19.5053461655912,-16.510970485056,-16.405679061905));
#53553=CARTESIAN_POINT('Ctrl Pts',(19.5850559562966,-16.5361581532281,-16.4098627597761));
#53554=CARTESIAN_POINT('Ctrl Pts',(19.6636790298742,-16.5653010733602,-16.4140464576472));
#53555=CARTESIAN_POINT('Ctrl Pts',(19.7407944846487,-16.5982870043948,-16.4182301555183));
#53556=CARTESIAN_POINT('Ctrl Pts',(19.817813812666,-16.6312318174641,-16.4224086382829));
#53557=CARTESIAN_POINT('Ctrl Pts',(19.8933288322728,-16.668009955813,-16.4265871210475));
#53558=CARTESIAN_POINT('Ctrl Pts',(19.9669338586819,-16.7084594721477,-16.4307656038121));
#53559=CARTESIAN_POINT('Ctrl Pts',(20.0404561874598,-16.7488635421407,-16.434939391916));
#53560=CARTESIAN_POINT('Ctrl Pts',(20.1120723866515,-16.7929305724585,-16.4391131800199));
#53561=CARTESIAN_POINT('Ctrl Pts',(20.1813982979639,-16.8404512397174,-16.4432869681238));
#53562=CARTESIAN_POINT('Ctrl Pts',(20.2194886451346,-16.8665609392425,-16.4455802093504));
#53563=CARTESIAN_POINT('Ctrl Pts',(20.2568879854969,-16.8937124046252,-16.447873450577));
#53564=CARTESIAN_POINT('Ctrl Pts',(20.293535888361,-16.9218650751947,-16.4501666918036));
#53565=CARTESIAN_POINT('Ctrl Pts',(20.295887153474,-16.918834963786,-15.6501589836526));
#53566=CARTESIAN_POINT('Ctrl Pts',(20.9266956757797,-17.4084201070463,-15.6900393319344));
#53567=CARTESIAN_POINT('Ctrl Pts',(21.731566631022,-19.0750468017155,-15.7723116157766));
#53568=CARTESIAN_POINT('Ctrl Pts',(20.3102572374462,-21.5363190520979,-15.8969758351793));
#53569=CARTESIAN_POINT('Ctrl Pts',(17.414194801089,-21.6762257759895,-16.0241516418607));
#53570=CARTESIAN_POINT('Ctrl Pts',(16.2227678370508,-20.0081650868305,-16.1140629935438));
#53571=CARTESIAN_POINT('Ctrl Pts',(16.1704459057083,-19.0564768309817,-16.1615824096664));
#53572=CARTESIAN_POINT('Ctrl Pts',(16.1712325076282,-18.9536997967236,-16.1667098902285));
#53573=CARTESIAN_POINT('Origin',(18.734,-18.952,1.76670989022851));
#53574=CARTESIAN_POINT('',(20.2935358883611,-16.9218650751948,-14.8500370296196));
#53575=CARTESIAN_POINT('',(20.293535888361,-16.9218650751948,-14.9167585823994));
#53576=CARTESIAN_POINT('',(20.293535888361,-16.9218650751948,1.76670989022851));
#53577=CARTESIAN_POINT('',(16.174000571626,-18.9537107672549,-15.4332901097416));
#53578=CARTESIAN_POINT('Ctrl Pts',(20.293535888361,-16.9218650751948,-14.9167585823994));
#53579=CARTESIAN_POINT('Ctrl Pts',(20.3601520173691,-16.9730391339543,-14.92092957676));
#53580=CARTESIAN_POINT('Ctrl Pts',(20.4242947459017,-17.0275324319862,-14.9251005711207));
#53581=CARTESIAN_POINT('Ctrl Pts',(20.4856216570591,-17.0850716214805,-14.9292715654813));
#53582=CARTESIAN_POINT('Ctrl Pts',(20.5469290962655,-17.1425925416659,-14.9334412355066));
#53583=CARTESIAN_POINT('Ctrl Pts',(20.6054221585251,-17.2031571180328,-14.9376109055319));
#53584=CARTESIAN_POINT('Ctrl Pts',(20.6607930947023,-17.2664530946285,-14.9417805755571));
#53585=CARTESIAN_POINT('Ctrl Pts',(20.7161630599139,-17.3297479612879,-14.9459501724645));
#53586=CARTESIAN_POINT('Ctrl Pts',(20.7684107058034,-17.395773785992,-14.9501197693719));
#53587=CARTESIAN_POINT('Ctrl Pts',(20.8172675301325,-17.4641840174619,-14.9542893662793));
#53588=CARTESIAN_POINT('Ctrl Pts',(20.8671067638701,-17.5339698368045,-14.9585428051328));
#53589=CARTESIAN_POINT('Ctrl Pts',(20.9134170197272,-17.6062366054209,-14.9627962439863));
#53590=CARTESIAN_POINT('Ctrl Pts',(20.9559598088395,-17.6805855876616,-14.9670496828397));
#53591=CARTESIAN_POINT('Ctrl Pts',(20.9977248092744,-17.7535752843976,-14.9712253581838));
#53592=CARTESIAN_POINT('Ctrl Pts',(21.0358587906801,-17.8285712512628,-14.9754010335279));
#53593=CARTESIAN_POINT('Ctrl Pts',(21.0701835580393,-17.905173183785,-14.979576708872));
#53594=CARTESIAN_POINT('Ctrl Pts',(21.1054671694712,-17.9839149504446,-14.9838690294802));
#53595=CARTESIAN_POINT('Ctrl Pts',(21.1367253892166,-18.0643532541545,-14.9881613500884));
#53596=CARTESIAN_POINT('Ctrl Pts',(21.163819136657,-18.1460353834469,-14.9924536706966));
#53597=CARTESIAN_POINT('Ctrl Pts',(21.1909128840974,-18.2277175127393,-14.9967459913047));
#53598=CARTESIAN_POINT('Ctrl Pts',(21.213842087396,-18.3106429475775,-15.0010383119129));
#53599=CARTESIAN_POINT('Ctrl Pts',(21.2325245180281,-18.3943484665022,-15.0053306325211));
#53600=CARTESIAN_POINT('Ctrl Pts',(21.25073824177,-18.4759539720913,-15.0095152669141));
#53601=CARTESIAN_POINT('Ctrl Pts',(21.2649836214983,-18.5586046111965,-15.0136999013072));
#53602=CARTESIAN_POINT('Ctrl Pts',(21.2751464736302,-18.6418797014761,-15.0178845357002));
#53603=CARTESIAN_POINT('Ctrl Pts',(21.2852948602001,-18.725036259972,-15.0220632137842));
#53604=CARTESIAN_POINT('Ctrl Pts',(21.2913722063418,-18.8088150514091,-15.0262418918681));
#53605=CARTESIAN_POINT('Ctrl Pts',(21.2933150345072,-18.8927838354387,-15.0304205699521));
#53606=CARTESIAN_POINT('Ctrl Pts',(21.2952926864712,-18.9782576995749,-15.0346741478375));
#53607=CARTESIAN_POINT('Ctrl Pts',(21.2929860350544,-19.0639279639717,-15.0389277257229));
#53608=CARTESIAN_POINT('Ctrl Pts',(21.2863832385264,-19.1493317097919,-15.0431813036084));
#53609=CARTESIAN_POINT('Ctrl Pts',(21.2799084500935,-19.2330797373477,-15.0473524175863));
#53610=CARTESIAN_POINT('Ctrl Pts',(21.2693026454397,-19.3165710082865,-15.0515235315643));
#53611=CARTESIAN_POINT('Ctrl Pts',(21.2546071988876,-19.3993693651963,-15.0556946455422));
#53612=CARTESIAN_POINT('Ctrl Pts',(21.2399166835345,-19.4821399383178,-15.0598643598626));
#53613=CARTESIAN_POINT('Ctrl Pts',(21.2211393320557,-19.5642176066098,-15.064034074183));
#53614=CARTESIAN_POINT('Ctrl Pts',(21.1983680574964,-19.6451739155445,-15.0682037885034));
#53615=CARTESIAN_POINT('Ctrl Pts',(21.1755975932368,-19.7261273437063,-15.0723733544474));
#53616=CARTESIAN_POINT('Ctrl Pts',(21.1488336138537,-19.8059590492309,-15.0765429203915));
#53617=CARTESIAN_POINT('Ctrl Pts',(21.1182192201024,-19.8842546382263,-15.0807124863355));
#53618=CARTESIAN_POINT('Ctrl Pts',(21.0865284620338,-19.9653030035426,-15.0850286490744));
#53619=CARTESIAN_POINT('Ctrl Pts',(21.0507116827588,-20.0447047315976,-15.0893448118133));
#53620=CARTESIAN_POINT('Ctrl Pts',(21.0109816181364,-20.1220233803941,-15.0936609745523));
#53621=CARTESIAN_POINT('Ctrl Pts',(20.9725457561902,-20.1968233823388,-15.0978365387439));
#53622=CARTESIAN_POINT('Ctrl Pts',(20.9304479207722,-20.2696735493082,-15.1020121029356));
#53623=CARTESIAN_POINT('Ctrl Pts',(20.8849263037079,-20.3402060495537,-15.1061876671273));
#53624=CARTESIAN_POINT('Ctrl Pts',(20.8371054979832,-20.4143009787113,-15.1105741291398));
#53625=CARTESIAN_POINT('Ctrl Pts',(20.7855062921192,-20.4858374838363,-15.1149605911524));
#53626=CARTESIAN_POINT('Ctrl Pts',(20.7304530967375,-20.5544278556389,-15.1193470531649));
#53627=CARTESIAN_POINT('Ctrl Pts',(20.6753999013558,-20.6230182274415,-15.1237335151775));
#53628=CARTESIAN_POINT('Ctrl Pts',(20.6168931592929,-20.6886620833861,-15.12811997719));
#53629=CARTESIAN_POINT('Ctrl Pts',(20.5553006227462,-20.7510175211999,-15.1325064392025));
#53630=CARTESIAN_POINT('Ctrl Pts',(20.4965420501079,-20.810503892887,-15.1366910735956));
#53631=CARTESIAN_POINT('Ctrl Pts',(20.4347566962297,-20.8672192262126,-15.1408757079886));
#53632=CARTESIAN_POINT('Ctrl Pts',(20.3702364829786,-20.9208398034807,-15.1450603423817));
#53633=CARTESIAN_POINT('Ctrl Pts',(20.3058081062651,-20.9743840584939,-15.1492390204656));
#53634=CARTESIAN_POINT('Ctrl Pts',(20.2386529531481,-21.0248420156527,-15.1534176985496));
#53635=CARTESIAN_POINT('Ctrl Pts',(20.1691001101646,-21.0719263368819,-15.1575963766335));
#53636=CARTESIAN_POINT('Ctrl Pts',(20.0983005824574,-21.1198546107302,-15.1618499545189));
#53637=CARTESIAN_POINT('Ctrl Pts',(20.0250169010501,-21.1642867711771,-15.1661035324044));
#53638=CARTESIAN_POINT('Ctrl Pts',(19.9496318977225,-21.2049622920146,-15.1703571102898));
#53639=CARTESIAN_POINT('Ctrl Pts',(19.8757083797861,-21.2448492385089,-15.1745282242678));
#53640=CARTESIAN_POINT('Ctrl Pts',(19.7997647128025,-21.281123676622,-15.1786993382457));
#53641=CARTESIAN_POINT('Ctrl Pts',(19.722190031268,-21.3135843118768,-15.1828704522237));
#53642=CARTESIAN_POINT('Ctrl Pts',(19.6446413806671,-21.3460340546519,-15.1870401665441));
#53643=CARTESIAN_POINT('Ctrl Pts',(19.5654632264914,-21.3746723587588,-15.1912098808644));
#53644=CARTESIAN_POINT('Ctrl Pts',(19.4850661232634,-21.3993454350553,-15.1953795951848));
#53645=CARTESIAN_POINT('Ctrl Pts',(19.4046718809095,-21.4240176333779,-15.1995491611288));
#53646=CARTESIAN_POINT('Ctrl Pts',(19.3230592157836,-21.4447247502806,-15.2037187270729));
#53647=CARTESIAN_POINT('Ctrl Pts',(19.2406540252945,-21.4613628072985,-15.2078882930169));
#53648=CARTESIAN_POINT('Ctrl Pts',(19.1553515699655,-21.4785858378759,-15.2122044557559));
#53649=CARTESIAN_POINT('Ctrl Pts',(19.0692003389645,-21.4914482440571,-15.2165206184948));
#53650=CARTESIAN_POINT('Ctrl Pts',(18.9826824608282,-21.4998926652582,-15.2208367812337));
#53651=CARTESIAN_POINT('Ctrl Pts',(18.8989828934722,-21.5080620103268,-15.2250123454254));
#53652=CARTESIAN_POINT('Ctrl Pts',(18.8149406719769,-21.512096806535,-15.2291879096171));
#53653=CARTESIAN_POINT('Ctrl Pts',(18.7309940133496,-21.5119982351643,-15.2333634738087));
#53654=CARTESIAN_POINT('Ctrl Pts',(18.6428074085592,-21.5118946851879,-15.2377499358213));
#53655=CARTESIAN_POINT('Ctrl Pts',(18.5547268571684,-21.5072292722347,-15.2421363978338));
#53656=CARTESIAN_POINT('Ctrl Pts',(18.4672539586503,-21.4980649146132,-15.2465228598464));
#53657=CARTESIAN_POINT('Ctrl Pts',(18.3797810601321,-21.4889005569917,-15.2509093218589));
#53658=CARTESIAN_POINT('Ctrl Pts',(18.2929163758375,-21.4752374199981,-15.2552957838715));
#53659=CARTESIAN_POINT('Ctrl Pts',(18.20714644876,-21.4571996598167,-15.259682245884));
#53660=CARTESIAN_POINT('Ctrl Pts',(18.125322923169,-21.4399918437196,-15.263866880277));
#53661=CARTESIAN_POINT('Ctrl Pts',(18.0441910630359,-21.41873907309,-15.2680515146701));
#53662=CARTESIAN_POINT('Ctrl Pts',(17.9641810754837,-21.3935115857715,-15.2722361490631));
#53663=CARTESIAN_POINT('Ctrl Pts',(17.8842849722453,-21.3683200066586,-15.2764148271471));
#53664=CARTESIAN_POINT('Ctrl Pts',(17.8055080047354,-21.3391650856198,-15.280593505231));
#53665=CARTESIAN_POINT('Ctrl Pts',(17.728269907104,-21.3061680017032,-15.284772183315));
#53666=CARTESIAN_POINT('Ctrl Pts',(17.6496473720827,-21.2725794687721,-15.2890257612004));
#53667=CARTESIAN_POINT('Ctrl Pts',(17.5726198898779,-21.2350097758299,-15.2932793390859));
#53668=CARTESIAN_POINT('Ctrl Pts',(17.4976137413827,-21.1936398059239,-15.2975329169713));
#53669=CARTESIAN_POINT('Ctrl Pts',(17.4240617334387,-21.1530718736114,-15.3017040309492));
#53670=CARTESIAN_POINT('Ctrl Pts',(17.3524538049873,-21.1088499333756,-15.3058751449272));
#53671=CARTESIAN_POINT('Ctrl Pts',(17.2831698439507,-21.0611922288634,-15.3100462589051));
#53672=CARTESIAN_POINT('Ctrl Pts',(17.2139091318162,-21.0135505163542,-15.3142159732255));
#53673=CARTESIAN_POINT('Ctrl Pts',(17.1469712170494,-20.9624755897518,-15.3183856875459));
#53674=CARTESIAN_POINT('Ctrl Pts',(17.0827076373574,-20.9082294172919,-15.3225554018663));
#53675=CARTESIAN_POINT('Ctrl Pts',(17.0184463444393,-20.8539851751436,-15.3267249678103));
#53676=CARTESIAN_POINT('Ctrl Pts',(16.9568595483704,-20.7965702088949,-15.3308945337544));
#53677=CARTESIAN_POINT('Ctrl Pts',(16.8982652087742,-20.7362863492957,-15.3350640996984));
#53678=CARTESIAN_POINT('Ctrl Pts',(16.8376107644816,-20.6738829835612,-15.3393802624373));
#53679=CARTESIAN_POINT('Ctrl Pts',(16.7801634890496,-20.6084056085283,-15.3436964251763));
#53680=CARTESIAN_POINT('Ctrl Pts',(16.7262325806843,-20.5402285698017,-15.3480125879152));
#53681=CARTESIAN_POINT('Ctrl Pts',(16.6740584659864,-20.4742723909407,-15.3521881521069));
#53682=CARTESIAN_POINT('Ctrl Pts',(16.6251753803869,-20.4057901412944,-15.3563637162985));
#53683=CARTESIAN_POINT('Ctrl Pts',(16.5798195291698,-20.335150931422,-15.3605392804902));
#53684=CARTESIAN_POINT('Ctrl Pts',(16.532172861731,-20.2609439029878,-15.3649257425028));
#53685=CARTESIAN_POINT('Ctrl Pts',(16.488419403819,-20.1843567987727,-15.3693122045153));
#53686=CARTESIAN_POINT('Ctrl Pts',(16.4487777573746,-20.1058454410405,-15.3736986665278));
#53687=CARTESIAN_POINT('Ctrl Pts',(16.4091361109301,-20.0273340833083,-15.3780851285404));
#53688=CARTESIAN_POINT('Ctrl Pts',(16.3736064408137,-19.9468990335382,-15.3824715905529));
#53689=CARTESIAN_POINT('Ctrl Pts',(16.3423477078172,-19.8650166007783,-15.3868580525655));
#53690=CARTESIAN_POINT('Ctrl Pts',(16.3083133302778,-19.7758633510063,-15.3916340140292));
#53691=CARTESIAN_POINT('Ctrl Pts',(16.2792349760223,-19.6847190703936,-15.396409975493));
#53692=CARTESIAN_POINT('Ctrl Pts',(16.2553188691393,-19.5921092496716,-15.4011859369567));
#53693=CARTESIAN_POINT('Ctrl Pts',(16.2315006236314,-19.4998783754247,-15.405942355852));
#53694=CARTESIAN_POINT('Ctrl Pts',(16.212802591162,-19.406194112186,-15.4106987747473));
#53695=CARTESIAN_POINT('Ctrl Pts',(16.1993817363336,-19.3115973546745,-15.4154551936426));
#53696=CARTESIAN_POINT('Ctrl Pts',(16.1860549755609,-19.2176638181479,-15.4201782651282));
#53697=CARTESIAN_POINT('Ctrl Pts',(16.1779317634136,-19.1228307363238,-15.4249013366138));
#53698=CARTESIAN_POINT('Ctrl Pts',(16.1751178968034,-19.0276464271479,-15.4296244080995));
#53699=CARTESIAN_POINT('Ctrl Pts',(16.1743899245164,-19.0030214008619,-15.4308463086469));
#53700=CARTESIAN_POINT('Ctrl Pts',(16.1740170525925,-18.9783729560401,-15.4320682091942));
#53701=CARTESIAN_POINT('Ctrl Pts',(16.174000571626,-18.9537107672549,-15.4332901097416));
#53702=CARTESIAN_POINT('Ctrl Pts',(16.1740005716256,-18.9537107666516,-15.4332901097715));
#53703=CARTESIAN_POINT('Ctrl Pts',(16.1739440307447,-18.8691027211111,-15.437482057942));
#53704=CARTESIAN_POINT('Ctrl Pts',(16.1780862675835,-18.7844696898645,-15.4416740061124));
#53705=CARTESIAN_POINT('Ctrl Pts',(16.1864081330308,-18.7002547332075,-15.4458659542829));
#53706=CARTESIAN_POINT('Ctrl Pts',(16.1947304086796,-18.6160356254258,-15.4500581090829));
#53707=CARTESIAN_POINT('Ctrl Pts',(16.2072326772703,-18.5322350838834,-15.4542502638829));
#53708=CARTESIAN_POINT('Ctrl Pts',(16.2238439368849,-18.4492908009531,-15.4584424186829));
#53709=CARTESIAN_POINT('Ctrl Pts',(16.2404607969944,-18.3663185533138,-15.4626359868701));
#53710=CARTESIAN_POINT('Ctrl Pts',(16.2611893110379,-18.2842035816671,-15.4668295550574));
#53711=CARTESIAN_POINT('Ctrl Pts',(16.2859076895265,-18.2033718951305,-15.4710231232446));
#53712=CARTESIAN_POINT('Ctrl Pts',(16.3106584247114,-18.122434398808,-15.4752221808701));
#53713=CARTESIAN_POINT('Ctrl Pts',(16.3394093150966,-18.0427839738199,-15.4794212384956));
#53714=CARTESIAN_POINT('Ctrl Pts',(16.3719892689075,-17.9648296468169,-15.4836202961211));
#53715=CARTESIAN_POINT('Ctrl Pts',(16.4045936038559,-17.8868169828627,-15.4878224961022));
#53716=CARTESIAN_POINT('Ctrl Pts',(16.4410325111314,-17.8105033515335,-15.4920246960833));
#53717=CARTESIAN_POINT('Ctrl Pts',(16.4810885578785,-17.7362738655611,-15.4962268960645));
#53718=CARTESIAN_POINT('Ctrl Pts',(16.5212156880346,-17.6619126520384,-15.5004365532643));
#53719=CARTESIAN_POINT('Ctrl Pts',(16.5649725361192,-17.5896433529152,-15.5046462104641));
#53720=CARTESIAN_POINT('Ctrl Pts',(16.612098119287,-17.5198224940229,-15.5088558676639));
#53721=CARTESIAN_POINT('Ctrl Pts',(16.6314200308983,-17.4911953158863,-15.5105818648582));
#53722=CARTESIAN_POINT('Ctrl Pts',(16.6513077816386,-17.4629793510679,-15.5123078620525));
#53723=CARTESIAN_POINT('Ctrl Pts',(16.6717415022699,-17.4351974787271,-15.5140338592469));
#53724=CARTESIAN_POINT('Ctrl Pts',(16.7212825156696,-17.3678410665133,-15.5182184936399));
#53725=CARTESIAN_POINT('Ctrl Pts',(16.7742191330187,-17.3027889832897,-15.522403128033));
#53726=CARTESIAN_POINT('Ctrl Pts',(16.8303093008605,-17.2404037502934,-15.526587762426));
#53727=CARTESIAN_POINT('Ctrl Pts',(16.8863196312909,-17.1781073149545,-15.53076644051));
#53728=CARTESIAN_POINT('Ctrl Pts',(16.9454742913219,-17.1184705290969,-15.5349451185939));
#53729=CARTESIAN_POINT('Ctrl Pts',(17.0074891937055,-17.0618252896231,-15.5391237966778));
#53730=CARTESIAN_POINT('Ctrl Pts',(17.070615668645,-17.004164724942,-15.5433773745633));
#53731=CARTESIAN_POINT('Ctrl Pts',(17.1367056485332,-16.949604396855,-15.5476309524487));
#53732=CARTESIAN_POINT('Ctrl Pts',(17.2054179892121,-16.8984574422974,-15.5518845303342));
#53733=CARTESIAN_POINT('Ctrl Pts',(17.272798207086,-16.8483020712589,-15.5560556443121));
#53734=CARTESIAN_POINT('Ctrl Pts',(17.3426996279386,-16.8014291923403,-15.5602267582901));
#53735=CARTESIAN_POINT('Ctrl Pts',(17.4147663076937,-16.7580942442566,-15.564397872268));
#53736=CARTESIAN_POINT('Ctrl Pts',(17.4868088047782,-16.7147738376334,-15.5685675865884));
#53737=CARTESIAN_POINT('Ctrl Pts',(17.5610147238611,-16.6749892409427,-15.5727373009088));
#53738=CARTESIAN_POINT('Ctrl Pts',(17.6370000578042,-16.6389519834594,-15.5769070152291));
#53739=CARTESIAN_POINT('Ctrl Pts',(17.7129826878631,-16.6029160083363,-15.5810765811732));
#53740=CARTESIAN_POINT('Ctrl Pts',(17.7907441908668,-16.570627303655,-15.5852461471172));
#53741=CARTESIAN_POINT('Ctrl Pts',(17.8698781766138,-16.5422503295264,-15.5894157130613));
#53742=CARTESIAN_POINT('Ctrl Pts',(17.9517944156772,-16.5128756559942,-15.5937318758002));
#53743=CARTESIAN_POINT('Ctrl Pts',(18.0351809497174,-16.4876930819298,-15.5980480385391));
#53744=CARTESIAN_POINT('Ctrl Pts',(18.1195690084032,-16.4668290689441,-15.602364201278));
#53745=CARTESIAN_POINT('Ctrl Pts',(18.2012081349535,-16.4466446989869,-15.6065397654697));
#53746=CARTESIAN_POINT('Ctrl Pts',(18.28378406749,-16.4305019005906,-15.6107153296614));
#53747=CARTESIAN_POINT('Ctrl Pts',(18.3668630221885,-16.4184628600466,-15.6148908938531));
#53748=CARTESIAN_POINT('Ctrl Pts',(18.4541380973873,-16.4058157561847,-15.6192773558656));
#53749=CARTESIAN_POINT('Ctrl Pts',(18.541967764093,-16.3976979204099,-15.6236638178782));
#53750=CARTESIAN_POINT('Ctrl Pts',(18.6298465962986,-16.3941196141146,-15.6280502798907));
#53751=CARTESIAN_POINT('Ctrl Pts',(18.7177254285043,-16.3905413078192,-15.6324367419032));
#53752=CARTESIAN_POINT('Ctrl Pts',(18.8056528468588,-16.391502448601,-15.6368232039158));
#53753=CARTESIAN_POINT('Ctrl Pts',(18.8931294701919,-16.3969505265619,-15.6412096659283));
#53754=CARTESIAN_POINT('Ctrl Pts',(18.9765715593007,-16.4021473321696,-15.6453938186788));
#53755=CARTESIAN_POINT('Ctrl Pts',(19.059914071307,-16.4114456475973,-15.6495779714293));
#53756=CARTESIAN_POINT('Ctrl Pts',(19.1427213148447,-16.4248381755828,-15.6537621241798));
#53757=CARTESIAN_POINT('Ctrl Pts',(19.2254168838738,-16.4382126422983,-15.6579406341485));
#53758=CARTESIAN_POINT('Ctrl Pts',(19.3075781677335,-16.4556702853466,-15.6621191441173));
#53759=CARTESIAN_POINT('Ctrl Pts',(19.3887723742188,-16.4771518959823,-15.666297654086));
#53760=CARTESIAN_POINT('Ctrl Pts',(19.4703186695032,-16.4987266590094,-15.6704942836549));
#53761=CARTESIAN_POINT('Ctrl Pts',(19.5508890109359,-16.5243603457589,-15.6746909132238));
#53762=CARTESIAN_POINT('Ctrl Pts',(19.630053111369,-16.5539406134113,-15.6788875427928));
#53763=CARTESIAN_POINT('Ctrl Pts',(19.7087329159883,-16.5833399202531,-15.6830584989804));
#53764=CARTESIAN_POINT('Ctrl Pts',(19.7860232004139,-16.6166374960991,-15.6872294551681));
#53765=CARTESIAN_POINT('Ctrl Pts',(19.8615163112604,-16.653673006763,-15.6914004113557));
#53766=CARTESIAN_POINT('Ctrl Pts',(19.937706443364,-16.6910504630417,-15.6956098776153));
#53767=CARTESIAN_POINT('Ctrl Pts',(20.0120655925479,-16.7322350830384,-15.6998193438748));
#53768=CARTESIAN_POINT('Ctrl Pts',(20.0841966779277,-16.7770128894835,-15.7040288101343));
#53769=CARTESIAN_POINT('Ctrl Pts',(20.1563277633076,-16.8217906959285,-15.7082382763939));
#53770=CARTESIAN_POINT('Ctrl Pts',(20.2262303743025,-16.8701614355123,-15.7124477426534));
#53771=CARTESIAN_POINT('Ctrl Pts',(20.293535888361,-16.9218650751948,-15.7166572089129));
#53772=CARTESIAN_POINT('',(16.1740008768645,-18.949881145288,-15.3667098902285));
#53773=CARTESIAN_POINT('Ctrl Pts',(16.1723624843679,-18.9498797892267,-15.3667098902285));
#53774=CARTESIAN_POINT('Ctrl Pts',(16.1710770695818,-18.8056440598866,-15.3738974629702));
#53775=CARTESIAN_POINT('Ctrl Pts',(16.2478506876061,-17.8120819459935,-15.4234769712724));
#53776=CARTESIAN_POINT('Ctrl Pts',(17.5479306946412,-16.1669449835732,-15.515448415135));
#53777=CARTESIAN_POINT('Ctrl Pts',(19.5288321013839,-16.3593204888311,-15.6027438735347));
#53778=CARTESIAN_POINT('Ctrl Pts',(20.2561600515754,-16.8880018374306,-15.6476473963739));
#53779=CARTESIAN_POINT('Ctrl Pts',(20.295887153474,-16.918834963786,-15.6501589836526));
#53780=CARTESIAN_POINT('Ctrl Pts',(20.2935358883611,-16.9218650751948,-14.8500370296196));
#53781=CARTESIAN_POINT('Ctrl Pts',(20.360176577277,-16.9730580007091,-14.8542147193799));
#53782=CARTESIAN_POINT('Ctrl Pts',(20.4242278292755,-17.0274848208923,-14.8583924091402));
#53783=CARTESIAN_POINT('Ctrl Pts',(20.4853757399687,-17.0848409233681,-14.8625700989005));
#53784=CARTESIAN_POINT('Ctrl Pts',(20.5466225444612,-17.1422897871961,-14.8667545451895));
#53785=CARTESIAN_POINT('Ctrl Pts',(20.6049563187768,-17.2026770568638,-14.8709389914784));
#53786=CARTESIAN_POINT('Ctrl Pts',(20.6601019172694,-17.2656633182276,-14.8751234377674));
#53787=CARTESIAN_POINT('Ctrl Pts',(20.6796325173081,-17.2879708008238,-14.8766054190876));
#53788=CARTESIAN_POINT('Ctrl Pts',(20.6987636051395,-17.3106040028926,-14.8780874004077));
#53789=CARTESIAN_POINT('Ctrl Pts',(20.7174842649081,-17.3335469821889,-14.8795693817278));
#53790=CARTESIAN_POINT('Ctrl Pts',(20.770345333846,-17.398330511467,-14.8837540161209));
#53791=CARTESIAN_POINT('Ctrl Pts',(20.8201275486196,-17.4658271045687,-14.8879386505139));
#53792=CARTESIAN_POINT('Ctrl Pts',(20.866540268707,-17.5357118928893,-14.892123284907));
#53793=CARTESIAN_POINT('Ctrl Pts',(20.912886926032,-17.6054972088638,-14.8963019629909));
#53794=CARTESIAN_POINT('Ctrl Pts',(20.9558733628219,-17.6776635880367,-14.9004806410749));
#53795=CARTESIAN_POINT('Ctrl Pts',(20.9952490842181,-17.7518531010236,-14.9046593191588));
#53796=CARTESIAN_POINT('Ctrl Pts',(21.0353305871216,-17.8273724077117,-14.9089128970442));
#53797=CARTESIAN_POINT('Ctrl Pts',(21.0716703524657,-17.9049877173955,-14.9131664749297));
#53798=CARTESIAN_POINT('Ctrl Pts',(21.1040502914402,-17.9842905311798,-14.9174200528151));
#53799=CARTESIAN_POINT('Ctrl Pts',(21.1358024821134,-18.0620559051722,-14.9215911667931));
#53800=CARTESIAN_POINT('Ctrl Pts',(21.1637468322872,-18.1414434905285,-14.925762280771));
#53801=CARTESIAN_POINT('Ctrl Pts',(21.1877248192283,-18.222044856513,-14.929933394749));
#53802=CARTESIAN_POINT('Ctrl Pts',(21.2116947601243,-18.3026191759308,-14.9341031090694));
#53803=CARTESIAN_POINT('Ctrl Pts',(21.2317008500143,-18.3844060265126,-14.9382728233897));
#53804=CARTESIAN_POINT('Ctrl Pts',(21.2476340898709,-18.46698076096,-14.9424425377101));
#53805=CARTESIAN_POINT('Ctrl Pts',(21.2635667627544,-18.5495525570439,-14.9466121036542));
#53806=CARTESIAN_POINT('Ctrl Pts',(21.2754267874402,-18.6329117293876,-14.9507816695982));
#53807=CARTESIAN_POINT('Ctrl Pts',(21.2831563307877,-18.7166237029669,-14.9549512355422));
#53808=CARTESIAN_POINT('Ctrl Pts',(21.2911576353439,-18.8032788862672,-14.9592673982812));
#53809=CARTESIAN_POINT('Ctrl Pts',(21.2947325504218,-18.8903116161907,-14.9635835610201));
#53810=CARTESIAN_POINT('Ctrl Pts',(21.2938756072079,-18.9772363947924,-14.967899723759));
#53811=CARTESIAN_POINT('Ctrl Pts',(21.293046578829,-19.0613296078741,-14.9720752879507));
#53812=CARTESIAN_POINT('Ctrl Pts',(21.2880700686645,-19.1453213272334,-14.9762508521424));
#53813=CARTESIAN_POINT('Ctrl Pts',(21.2789941177451,-19.2287759755517,-14.9804264163341));
#53814=CARTESIAN_POINT('Ctrl Pts',(21.2694597621209,-19.3164457197619,-14.9848128783466));
#53815=CARTESIAN_POINT('Ctrl Pts',(21.2554010498833,-19.4035221357511,-14.9891993403591));
#53816=CARTESIAN_POINT('Ctrl Pts',(21.2369341836446,-19.4895132299242,-14.9935858023717));
#53817=CARTESIAN_POINT('Ctrl Pts',(21.2184673174058,-19.5755043240972,-14.9979722643842));
#53818=CARTESIAN_POINT('Ctrl Pts',(21.1955925215497,-19.6604095560011,-15.0023587263967));
#53819=CARTESIAN_POINT('Ctrl Pts',(21.1684852750765,-19.7437584514458,-15.0067451884093));
#53820=CARTESIAN_POINT('Ctrl Pts',(21.142625273196,-19.8232723406584,-15.0109298228023));
#53821=CARTESIAN_POINT('Ctrl Pts',(21.1128174886275,-19.9016659307485,-15.0151144571954));
#53822=CARTESIAN_POINT('Ctrl Pts',(21.0791777662538,-19.9785189938178,-15.0192990915884));
#53823=CARTESIAN_POINT('Ctrl Pts',(21.0455859258611,-20.0552626660644,-15.0234777696724));
#53824=CARTESIAN_POINT('Ctrl Pts',(21.0081731644859,-20.1304697489562,-15.0276564477563));
#53825=CARTESIAN_POINT('Ctrl Pts',(20.9671048559811,-20.2037358755718,-15.0318351258403));
#53826=CARTESIAN_POINT('Ctrl Pts',(20.9253004275616,-20.2783152448517,-15.0360887037257));
#53827=CARTESIAN_POINT('Ctrl Pts',(20.8797082607492,-20.3508829316546,-15.0403422816111));
#53828=CARTESIAN_POINT('Ctrl Pts',(20.8305537911317,-20.4210344451004,-15.0445958594966));
#53829=CARTESIAN_POINT('Ctrl Pts',(20.7823522768248,-20.4898259345685,-15.0487669734745));
#53830=CARTESIAN_POINT('Ctrl Pts',(20.7307256276405,-20.5562937050241,-15.0529380874525));
#53831=CARTESIAN_POINT('Ctrl Pts',(20.675931463843,-20.6200833881244,-15.0571092014304));
#53832=CARTESIAN_POINT('Ctrl Pts',(20.6211556867563,-20.6838516659805,-15.0612789157508));
#53833=CARTESIAN_POINT('Ctrl Pts',(20.5632148054787,-20.7449432925553,-15.0654486300712));
#53834=CARTESIAN_POINT('Ctrl Pts',(20.5024068820801,-20.8030367633874,-15.0696183443915));
#53835=CARTESIAN_POINT('Ctrl Pts',(20.4416011224884,-20.8611281670045,-15.0737879103356));
#53836=CARTESIAN_POINT('Ctrl Pts',(20.3779288568417,-20.9162213098335,-15.0779574762796));
#53837=CARTESIAN_POINT('Ctrl Pts',(20.3117241899802,-20.9680323361373,-15.0821270422237));
#53838=CARTESIAN_POINT('Ctrl Pts',(20.2431918487041,-21.0216649742102,-15.0864432049626));
#53839=CARTESIAN_POINT('Ctrl Pts',(20.1719461297946,-21.0717800780495,-15.0907593677015));
#53840=CARTESIAN_POINT('Ctrl Pts',(20.0983923000264,-21.1181102584191,-15.0950755304404));
#53841=CARTESIAN_POINT('Ctrl Pts',(20.0272344785266,-21.1629312380363,-15.0992510946321));
#53842=CARTESIAN_POINT('Ctrl Pts',(19.9539170439582,-21.2042099051979,-15.1034266588238));
#53843=CARTESIAN_POINT('Ctrl Pts',(19.8788322516134,-21.2417508850672,-15.1076022230155));
#53844=CARTESIAN_POINT('Ctrl Pts',(19.7999551049042,-21.2811879705845,-15.111988685028));
#53845=CARTESIAN_POINT('Ctrl Pts',(19.7191279049091,-21.3164996308723,-15.1163751470406));
#53846=CARTESIAN_POINT('Ctrl Pts',(19.6368272386519,-21.3475172671363,-15.1207616090531));
#53847=CARTESIAN_POINT('Ctrl Pts',(19.5545265723946,-21.3785349034004,-15.1251480710657));
#53848=CARTESIAN_POINT('Ctrl Pts',(19.4707530157655,-21.4052584117748,-15.1295345330782));
#53849=CARTESIAN_POINT('Ctrl Pts',(19.3859971465586,-21.4275806835729,-15.1339209950908));
#53850=CARTESIAN_POINT('Ctrl Pts',(19.3051410205324,-21.4488758745561,-15.1381056294838));
#53851=CARTESIAN_POINT('Ctrl Pts',(19.2230900288836,-21.4662452083819,-15.1422902638769));
#53852=CARTESIAN_POINT('Ctrl Pts',(19.1402602214101,-21.4795586308728,-15.1464748982699));
#53853=CARTESIAN_POINT('Ctrl Pts',(19.0575483119153,-21.4928531033548,-15.1506535763538));
#53854=CARTESIAN_POINT('Ctrl Pts',(18.974060238839,-21.5021030592902,-15.1548322544378));
#53855=CARTESIAN_POINT('Ctrl Pts',(18.8902255244996,-21.5072286757734,-15.1590109325217));
#53856=CARTESIAN_POINT('Ctrl Pts',(18.8048881331567,-21.5124461652484,-15.1632645104072));
#53857=CARTESIAN_POINT('Ctrl Pts',(18.7191920174691,-21.5133898805874,-15.1675180882926));
#53858=CARTESIAN_POINT('Ctrl Pts',(18.6335993142633,-21.510030434202,-15.171771666178));
#53859=CARTESIAN_POINT('Ctrl Pts',(18.5496659926296,-21.5067361172402,-15.175942780156));
#53860=CARTESIAN_POINT('Ctrl Pts',(18.4658325904026,-21.4993040188572,-15.1801138941339));
#53861=CARTESIAN_POINT('Ctrl Pts',(18.3825365202413,-21.4877589440631,-15.1842850081119));
#53862=CARTESIAN_POINT('Ctrl Pts',(18.2992684008808,-21.4762177433303,-15.1884547224323));
#53863=CARTESIAN_POINT('Ctrl Pts',(18.2165377107911,-21.4605663702896,-15.1926244367526));
#53864=CARTESIAN_POINT('Ctrl Pts',(18.1347761196902,-21.4408814237055,-15.196794151073));
#53865=CARTESIAN_POINT('Ctrl Pts',(18.0530174380175,-21.4211971775963,-15.200963717017));
#53866=CARTESIAN_POINT('Ctrl Pts',(17.9722282338226,-21.3974797518311,-15.2051332829611));
#53867=CARTESIAN_POINT('Ctrl Pts',(17.8928280294726,-21.3698564299807,-15.2093028489051));
#53868=CARTESIAN_POINT('Ctrl Pts',(17.8106362118883,-21.3412619062111,-15.213619011644));
#53869=CARTESIAN_POINT('Ctrl Pts',(17.729933384083,-21.3084818866878,-15.217935174383));
#53870=CARTESIAN_POINT('Ctrl Pts',(17.6511637413075,-21.2717124039115,-15.2222513371219));
#53871=CARTESIAN_POINT('Ctrl Pts',(17.5749600113602,-21.2361406831691,-15.2264269013136));
#53872=CARTESIAN_POINT('Ctrl Pts',(17.5005658480113,-21.1968356830554,-15.2306024655052));
#53873=CARTESIAN_POINT('Ctrl Pts',(17.4283578509295,-21.1540214755017,-15.2347780296969));
#53874=CARTESIAN_POINT('Ctrl Pts',(17.3525027995735,-21.1090448241056,-15.2391644917095));
#53875=CARTESIAN_POINT('Ctrl Pts',(17.2790610511148,-21.0601954720667,-15.243550953722));
#53876=CARTESIAN_POINT('Ctrl Pts',(17.2084323379748,-21.007782894321,-15.2479374157345));
#53877=CARTESIAN_POINT('Ctrl Pts',(17.1378036248349,-20.9553703165754,-15.252323877747));
#53878=CARTESIAN_POINT('Ctrl Pts',(17.0699883460669,-20.8993949411349,-15.2567103397596));
#53879=CARTESIAN_POINT('Ctrl Pts',(17.0053421035814,-20.8402112903883,-15.2610968017721));
#53880=CARTESIAN_POINT('Ctrl Pts',(16.9445899812057,-20.7845927075508,-15.2652190348167));
#53881=CARTESIAN_POINT('Ctrl Pts',(16.8863955977248,-20.7259204795934,-15.2693412678613));
#53882=CARTESIAN_POINT('Ctrl Pts',(16.8310887538618,-20.6644627847987,-15.2734635009059));
#53883=CARTESIAN_POINT('Ctrl Pts',(16.7758743514522,-20.6031078121671,-15.2775788439313));
#53884=CARTESIAN_POINT('Ctrl Pts',(16.7235382140149,-20.5389769727691,-15.2816941869567));
#53885=CARTESIAN_POINT('Ctrl Pts',(16.6743754759298,-20.4723771965696,-15.2858095299821));
#53886=CARTESIAN_POINT('Ctrl Pts',(16.6252589923643,-20.4058400804408,-15.2899210011073));
#53887=CARTESIAN_POINT('Ctrl Pts',(16.5793102664141,-20.336839014796,-15.2940324722326));
#53888=CARTESIAN_POINT('Ctrl Pts',(16.5367853878613,-20.2657153223604,-15.2981439433578));
#53889=CARTESIAN_POINT('Ctrl Pts',(16.4942868717937,-20.1946357216976,-15.3022528656552));
#53890=CARTESIAN_POINT('Ctrl Pts',(16.4552082342186,-20.1214365120742,-15.3063617879525));
#53891=CARTESIAN_POINT('Ctrl Pts',(16.4197623875945,-20.0464881330228,-15.3104707102498));
#53892=CARTESIAN_POINT('Ctrl Pts',(16.3843271437787,-19.971562173052,-15.3145784034577));
#53893=CARTESIAN_POINT('Ctrl Pts',(16.3525227351499,-19.894888512104,-15.3186860966657));
#53894=CARTESIAN_POINT('Ctrl Pts',(16.3245154961056,-19.8168609284116,-15.3227937898736));
#53895=CARTESIAN_POINT('Ctrl Pts',(16.2964946934766,-19.7387955568548,-15.3269034723902));
#53896=CARTESIAN_POINT('Ctrl Pts',(16.272274898332,-19.6593753990486,-15.3310131549069));
#53897=CARTESIAN_POINT('Ctrl Pts',(16.2519734104534,-19.5790119686126,-15.3351228374235));
#53898=CARTESIAN_POINT('Ctrl Pts',(16.231666738396,-19.4986280166076,-15.3392335693868));
#53899=CARTESIAN_POINT('Ctrl Pts',(16.2152804642378,-19.4173007774467,-15.3433443013501));
#53900=CARTESIAN_POINT('Ctrl Pts',(16.2028808242122,-19.3354523672626,-15.3474550333134));
#53901=CARTESIAN_POINT('Ctrl Pts',(16.1904661338132,-19.2535046115225,-15.3515707547805));
#53902=CARTESIAN_POINT('Ctrl Pts',(16.1820477886731,-19.1710348943536,-15.3556864762476));
#53903=CARTESIAN_POINT('Ctrl Pts',(16.1776401048971,-19.0884700945614,-15.3598021977147));
#53904=CARTESIAN_POINT('Ctrl Pts',(16.1751742007241,-19.04227873994,-15.362104761886));
#53905=CARTESIAN_POINT('Ctrl Pts',(16.173962657598,-18.9960576424388,-15.3644073260572));
#53906=CARTESIAN_POINT('Ctrl Pts',(16.1740008768645,-18.949881145288,-15.3667098902285));
#53907=CARTESIAN_POINT('Origin',(18.734,-18.952,1.76670989022851));
#53908=CARTESIAN_POINT('',(20.2909850430174,-16.9251769135511,-14.0501277865439));
#53909=CARTESIAN_POINT('',(20.2961055948522,-16.9185282149957,-14.1167030459603));
#53910=CARTESIAN_POINT('',(20.293535888361,-16.9218650751948,1.76670989022851));
#53911=CARTESIAN_POINT('',(16.1738766836434,-18.9531301832654,-14.6332901097715));
#53912=CARTESIAN_POINT('Ctrl Pts',(20.2961055948522,-16.9185282149957,-14.1167030459603));
#53913=CARTESIAN_POINT('Ctrl Pts',(20.959851318088,-17.429684584912,-14.1585606281177));
#53914=CARTESIAN_POINT('Ctrl Pts',(21.7469835062583,-19.1757114502307,-14.2428101458356));
#53915=CARTESIAN_POINT('Ctrl Pts',(20.1889474246921,-21.6065091003007,-14.369451599114));
#53916=CARTESIAN_POINT('Ctrl Pts',(17.2895133775451,-21.6122159629899,-14.4966274057954));
#53917=CARTESIAN_POINT('Ctrl Pts',(16.2008983314107,-19.9284205945985,-14.5845735760146));
#53918=CARTESIAN_POINT('Ctrl Pts',(16.1700292378907,-19.0164624118087,-14.6301278106733));
#53919=CARTESIAN_POINT('Ctrl Pts',(16.1703790167221,-18.9531317273334,-14.6332901097715));
#53920=CARTESIAN_POINT('Ctrl Pts',(16.1740002494514,-18.9531301287164,-14.6332901097715));
#53921=CARTESIAN_POINT('Ctrl Pts',(16.1739637014967,-18.8703406609987,-14.6374299052976));
#53922=CARTESIAN_POINT('Ctrl Pts',(16.1779474618949,-18.787387492894,-14.6415697008237));
#53923=CARTESIAN_POINT('Ctrl Pts',(16.1859729132155,-18.7046986352396,-14.6457094963498));
#53924=CARTESIAN_POINT('Ctrl Pts',(16.1939875490477,-18.6221212131097,-14.6498437128863));
#53925=CARTESIAN_POINT('Ctrl Pts',(16.2060330170348,-18.5398078587028,-14.6539779294227));
#53926=CARTESIAN_POINT('Ctrl Pts',(16.2220786798974,-18.4581869973217,-14.6581121459591));
#53927=CARTESIAN_POINT('Ctrl Pts',(16.2381078732803,-18.3766499126678,-14.6622421190812));
#53928=CARTESIAN_POINT('Ctrl Pts',(16.2581290152451,-18.2958043686403,-14.6663720922033));
#53929=CARTESIAN_POINT('Ctrl Pts',(16.2820597821146,-18.2160725797227,-14.6705020653254));
#53930=CARTESIAN_POINT('Ctrl Pts',(16.3059775967093,-18.1363839447938,-14.6746298031431));
#53931=CARTESIAN_POINT('Ctrl Pts',(16.3338007023324,-18.0578083185529,-14.6787575409609));
#53932=CARTESIAN_POINT('Ctrl Pts',(16.3653962152435,-17.9807553805363,-14.6828852787787));
#53933=CARTESIAN_POINT('Ctrl Pts',(16.3969845852848,-17.9037198620533,-14.6870120834293));
#53934=CARTESIAN_POINT('Ctrl Pts',(16.4323434905918,-17.8282067834232,-14.69113888808));
#53935=CARTESIAN_POINT('Ctrl Pts',(16.4712914723378,-17.7546069488907,-14.6952656927306));
#53936=CARTESIAN_POINT('Ctrl Pts',(16.510242924153,-17.6810005569833,-14.6993928650588));
#53937=CARTESIAN_POINT('Ctrl Pts',(16.5527838651356,-17.609308162424,-14.703520037387));
#53938=CARTESIAN_POINT('Ctrl Pts',(16.5986870593953,-17.5398956675635,-14.7076472097152));
#53939=CARTESIAN_POINT('Ctrl Pts',(16.6446377721095,-17.4704113176929,-14.7117786544443));
#53940=CARTESIAN_POINT('Ctrl Pts',(16.6939574240315,-17.4032119705958,-14.7159100991734));
#53941=CARTESIAN_POINT('Ctrl Pts',(16.746376041612,-17.3386336435756,-14.7200415439026));
#53942=CARTESIAN_POINT('Ctrl Pts',(16.7988250781874,-17.2740178411719,-14.7241753861462));
#53943=CARTESIAN_POINT('Ctrl Pts',(16.8543763437697,-17.2120264344659,-14.7283092283899));
#53944=CARTESIAN_POINT('Ctrl Pts',(16.9127219511753,-17.1529596255589,-14.7324430706335));
#53945=CARTESIAN_POINT('Ctrl Pts',(16.9711635405876,-17.0937956482256,-14.7365837132944));
#53946=CARTESIAN_POINT('Ctrl Pts',(17.0324082986517,-17.0375661867597,-14.7407243559553));
#53947=CARTESIAN_POINT('Ctrl Pts',(17.0961145829386,-16.9845317383557,-14.7448649986161));
#53948=CARTESIAN_POINT('Ctrl Pts',(17.1274705472736,-16.9584284066154,-14.7469030054635));
#53949=CARTESIAN_POINT('Ctrl Pts',(17.1594223751532,-16.9330984310461,-14.7489410123109));
#53950=CARTESIAN_POINT('Ctrl Pts',(17.1919269101816,-16.9085689182999,-14.7509790191583));
#53951=CARTESIAN_POINT('Ctrl Pts',(17.2586683911458,-16.8582025307613,-14.7551636535514));
#53952=CARTESIAN_POINT('Ctrl Pts',(17.3280042311001,-16.8110156651531,-14.7593482879444));
#53953=CARTESIAN_POINT('Ctrl Pts',(17.3995987737075,-16.767286433587,-14.7635329223375));
#53954=CARTESIAN_POINT('Ctrl Pts',(17.4710914103451,-16.7236194451695,-14.7677116004214));
#53955=CARTESIAN_POINT('Ctrl Pts',(17.5448359744308,-16.6834005528598,-14.7718902785053));
#53956=CARTESIAN_POINT('Ctrl Pts',(17.6204652949934,-16.6468664982813,-14.7760689565893));
#53957=CARTESIAN_POINT('Ctrl Pts',(17.6974502167732,-16.6096775970311,-14.7803225344747));
#53958=CARTESIAN_POINT('Ctrl Pts',(17.7763877432994,-16.5763072247155,-14.7845761123602));
#53959=CARTESIAN_POINT('Ctrl Pts',(17.8568613993349,-16.5469578225687,-14.7888296902456));
#53960=CARTESIAN_POINT('Ctrl Pts',(17.9357749165169,-16.5181774158532,-14.7930008042235));
#53961=CARTESIAN_POINT('Ctrl Pts',(18.0161650809,-16.4932636267837,-14.7971719182015));
#53962=CARTESIAN_POINT('Ctrl Pts',(18.0976177441666,-16.4723593759457,-14.8013430321794));
#53963=CARTESIAN_POINT('Ctrl Pts',(18.1790430752053,-16.451462139731,-14.8055127464998));
#53964=CARTESIAN_POINT('Ctrl Pts',(18.2615297518284,-16.434571883947,-14.8096824608202));
#53965=CARTESIAN_POINT('Ctrl Pts',(18.3446492988108,-16.4217814261445,-14.8138521751405));
#53966=CARTESIAN_POINT('Ctrl Pts',(18.4277658880431,-16.4089914234813,-14.8180217410846));
#53967=CARTESIAN_POINT('Ctrl Pts',(18.5115148480479,-16.4003009978601,-14.8221913070286));
#53968=CARTESIAN_POINT('Ctrl Pts',(18.5954597232801,-16.3957514612764,-14.8263608729727));
#53969=CARTESIAN_POINT('Ctrl Pts',(18.6823559967683,-16.3910419685989,-14.8306770357116));
#53970=CARTESIAN_POINT('Ctrl Pts',(18.7694616919212,-16.3907699986349,-14.8349931984505));
#53971=CARTESIAN_POINT('Ctrl Pts',(18.8562914526112,-16.3949226056652,-14.8393093611894));
#53972=CARTESIAN_POINT('Ctrl Pts',(18.9402927429795,-16.3989399419582,-14.8434849253811));
#53973=CARTESIAN_POINT('Ctrl Pts',(19.0240353356995,-16.4070979281598,-14.8476604895728));
#53974=CARTESIAN_POINT('Ctrl Pts',(19.1070857885139,-16.4193320402372,-14.8518360537645));
#53975=CARTESIAN_POINT('Ctrl Pts',(19.1943309222662,-16.4321840682319,-14.856222515777));
#53976=CARTESIAN_POINT('Ctrl Pts',(19.2808115861347,-16.4495346990029,-14.8606089777895));
#53977=CARTESIAN_POINT('Ctrl Pts',(19.3660405469235,-16.471249156597,-14.8649954398021));
#53978=CARTESIAN_POINT('Ctrl Pts',(19.4512695077123,-16.4929636141912,-14.8693819018146));
#53979=CARTESIAN_POINT('Ctrl Pts',(19.5352462338659,-16.5190416538915,-14.8737683638271));
#53980=CARTESIAN_POINT('Ctrl Pts',(19.6175072439393,-16.549290082031,-14.8781548258396));
#53981=CARTESIAN_POINT('Ctrl Pts',(19.6959730538366,-16.5781429664043,-14.8823389137093));
#53982=CARTESIAN_POINT('Ctrl Pts',(19.7731699980655,-16.6108972906671,-14.886523001579));
#53983=CARTESIAN_POINT('Ctrl Pts',(19.8486827058591,-16.6474214126529,-14.8907070894487));
#53984=CARTESIAN_POINT('Ctrl Pts',(19.9270438220701,-16.6853232579325,-14.8950490049405));
#53985=CARTESIAN_POINT('Ctrl Pts',(20.0035906250348,-16.7272848683664,-14.8993909204323));
#53986=CARTESIAN_POINT('Ctrl Pts',(20.0778772798292,-16.7731026052706,-14.9037328359241));
#53987=CARTESIAN_POINT('Ctrl Pts',(20.1521639346237,-16.8189203421747,-14.9080747514158));
#53988=CARTESIAN_POINT('Ctrl Pts',(20.2241899296921,-16.8685939797933,-14.9124166669076));
#53989=CARTESIAN_POINT('Ctrl Pts',(20.293535888361,-16.9218650751948,-14.9167585823994));
#53990=CARTESIAN_POINT('',(16.1743645121285,-18.9514398261319,-14.566709915053));
#53991=CARTESIAN_POINT('Ctrl Pts',(16.1740000613162,-18.9514396975223,-14.5667099174731));
#53992=CARTESIAN_POINT('Ctrl Pts',(16.1740197372988,-18.8615409084374,-14.571157199272));
#53993=CARTESIAN_POINT('Ctrl Pts',(16.1787790795978,-18.7717655181971,-14.575604481071));
#53994=CARTESIAN_POINT('Ctrl Pts',(16.1882138900512,-18.6826060832318,-14.58005176287));
#53995=CARTESIAN_POINT('Ctrl Pts',(16.1976832329536,-18.5931203148802,-14.5845153222119));
#53996=CARTESIAN_POINT('Ctrl Pts',(16.211862232535,-18.504255369482,-14.5889788815538));
#53997=CARTESIAN_POINT('Ctrl Pts',(16.23063522025,-18.4164957707849,-14.5934424408956));
#53998=CARTESIAN_POINT('Ctrl Pts',(16.2494446598934,-18.3285657673207,-14.5979146672301));
#53999=CARTESIAN_POINT('Ctrl Pts',(16.2728657964755,-18.241745739755,-14.6023868935646));
#54000=CARTESIAN_POINT('Ctrl Pts',(16.3007333122773,-18.1565044145825,-14.606859119899));
#54001=CARTESIAN_POINT('Ctrl Pts',(16.3286838403159,-18.0710091710796,-14.6113446681784));
#54002=CARTESIAN_POINT('Ctrl Pts',(16.3611071025136,-17.9871023685302,-14.6158302164579));
#54003=CARTESIAN_POINT('Ctrl Pts',(16.3977895032111,-17.9052333045547,-14.6203157647373));
#54004=CARTESIAN_POINT('Ctrl Pts',(16.4111522146039,-17.8754099382236,-14.6219497659465));
#54005=CARTESIAN_POINT('Ctrl Pts',(16.4250796827618,-17.8458567318514,-14.6235837671557));
#54006=CARTESIAN_POINT('Ctrl Pts',(16.4395601204677,-17.8165945045,-14.625217768365));
#54007=CARTESIAN_POINT('Ctrl Pts',(16.4766441429939,-17.7416547050056,-14.629402402758));
#54008=CARTESIAN_POINT('Ctrl Pts',(16.5174725051856,-17.6683941847451,-14.6335870371511));
#54009=CARTESIAN_POINT('Ctrl Pts',(16.5618698248528,-17.5972120083883,-14.6377716715441));
#54010=CARTESIAN_POINT('Ctrl Pts',(16.6062039504308,-17.526131151049,-14.641950349628));
#54011=CARTESIAN_POINT('Ctrl Pts',(16.6540967016935,-17.4571231485617,-14.646129027712));
#54012=CARTESIAN_POINT('Ctrl Pts',(16.7053259809371,-17.3905642106128,-14.6503077057959));
#54013=CARTESIAN_POINT('Ctrl Pts',(16.7574735081934,-17.3228122515363,-14.6545612836814));
#54014=CARTESIAN_POINT('Ctrl Pts',(16.8130781406444,-17.2575984516733,-14.6588148615668));
#54015=CARTESIAN_POINT('Ctrl Pts',(16.871858331947,-17.1952904599505,-14.6630684394522));
#54016=CARTESIAN_POINT('Ctrl Pts',(16.9294989545411,-17.1341904302313,-14.6672395534302));
#54017=CARTESIAN_POINT('Ctrl Pts',(16.9901927757376,-17.0758848946116,-14.6714106674081));
#54018=CARTESIAN_POINT('Ctrl Pts',(17.0536336491123,-17.0206872529794,-14.6755817813861));
#54019=CARTESIAN_POINT('Ctrl Pts',(17.1170532342893,-16.9655081334488,-14.6797514957065));
#54020=CARTESIAN_POINT('Ctrl Pts',(17.1832176941667,-16.913435138433,-14.6839212100268));
#54021=CARTESIAN_POINT('Ctrl Pts',(17.2517856166925,-16.8647433023425,-14.6880909243472));
#54022=CARTESIAN_POINT('Ctrl Pts',(17.3203510992773,-16.8160531989164,-14.6922604902913));
#54023=CARTESIAN_POINT('Ctrl Pts',(17.3913194988898,-16.7707442808558,-14.6964300562353));
#54024=CARTESIAN_POINT('Ctrl Pts',(17.4643191824367,-16.7290491185112,-14.7005996221793));
#54025=CARTESIAN_POINT('Ctrl Pts',(17.5398854448023,-16.6858880056951,-14.7049157849183));
#54026=CARTESIAN_POINT('Ctrl Pts',(17.6176280306767,-16.6465997576135,-14.7092319476572));
#54027=CARTESIAN_POINT('Ctrl Pts',(17.697107273311,-16.6113903628884,-14.7135481103961));
#54028=CARTESIAN_POINT('Ctrl Pts',(17.7739974879763,-16.5773279104932,-14.7177236745878));
#54029=CARTESIAN_POINT('Ctrl Pts',(17.8525124972024,-16.5470827802973,-14.7218992387795));
#54030=CARTESIAN_POINT('Ctrl Pts',(17.9322359204944,-16.5207915842498,-14.7260748029711));
#54031=CARTESIAN_POINT('Ctrl Pts',(18.0159859843726,-16.4931724823913,-14.7304612649837));
#54032=CARTESIAN_POINT('Ctrl Pts',(18.1010691812454,-16.4699173921692,-14.7348477269962));
#54033=CARTESIAN_POINT('Ctrl Pts',(18.1869895560292,-16.4511242385543,-14.7392341890088));
#54034=CARTESIAN_POINT('Ctrl Pts',(18.272909930813,-16.4323310849394,-14.7436206510213));
#54035=CARTESIAN_POINT('Ctrl Pts',(18.3596668986516,-16.4179998874471,-14.7480071130339));
#54036=CARTESIAN_POINT('Ctrl Pts',(18.446759550604,-16.4081657042506,-14.7523935750464));
#54037=CARTESIAN_POINT('Ctrl Pts',(18.5298216106109,-16.3987866407306,-14.7565770344168));
#54038=CARTESIAN_POINT('Ctrl Pts',(18.6134980569013,-16.3934626556782,-14.7607604937872));
#54039=CARTESIAN_POINT('Ctrl Pts',(18.697358772211,-16.3922622360042,-14.7649439531576));
#54040=CARTESIAN_POINT('Ctrl Pts',(18.7811102468205,-16.3910633800503,-14.7691219629677));
#54041=CARTESIAN_POINT('Ctrl Pts',(18.8650450584583,-16.3939774328894,-14.7732999727777));
#54042=CARTESIAN_POINT('Ctrl Pts',(18.9487268680229,-16.401021291318,-14.7774779825877));
#54043=CARTESIAN_POINT('Ctrl Pts',(19.032324781039,-16.4080580878126,-14.7816518036666));
#54044=CARTESIAN_POINT('Ctrl Pts',(19.1156697399224,-16.419216429775,-14.7858256247455));
#54045=CARTESIAN_POINT('Ctrl Pts',(19.1983256615619,-16.4344611859963,-14.7899994458244));
#54046=CARTESIAN_POINT('Ctrl Pts',(19.2809235142156,-16.4496952321861,-14.7941703346323));
#54047=CARTESIAN_POINT('Ctrl Pts',(19.3628328402599,-16.4690099061368,-14.7983412234403));
#54048=CARTESIAN_POINT('Ctrl Pts',(19.4436242958238,-16.4923184436239,-14.8025121122482));
#54049=CARTESIAN_POINT('Ctrl Pts',(19.5244040000537,-16.5156235908217,-14.8066823943892));
#54050=CARTESIAN_POINT('Ctrl Pts',(19.6040657115566,-16.5429213326382,-14.8108526765302));
#54051=CARTESIAN_POINT('Ctrl Pts',(19.6821928869636,-16.574074381081,-14.8150229586711));
#54052=CARTESIAN_POINT('Ctrl Pts',(19.7603101594137,-16.6052234807403,-14.8191927122109));
#54053=CARTESIAN_POINT('Ctrl Pts',(19.836892857112,-16.6402267397378,-14.8233624657506));
#54054=CARTESIAN_POINT('Ctrl Pts',(19.9115437773171,-16.6788984509042,-14.8275322192903));
#54055=CARTESIAN_POINT('Ctrl Pts',(19.9862468140621,-16.7175971602077,-14.8317048838875));
#54056=CARTESIAN_POINT('Ctrl Pts',(20.0590149720314,-16.7599692220591,-14.8358775484848));
#54057=CARTESIAN_POINT('Ctrl Pts',(20.1294756726678,-16.8057829450421,-14.8400502130821));
#54058=CARTESIAN_POINT('Ctrl Pts',(20.1856890006227,-16.8423329908352,-14.8433791519279));
#54059=CARTESIAN_POINT('Ctrl Pts',(20.2404341046543,-16.8810726448914,-14.8467080907738));
#54060=CARTESIAN_POINT('Ctrl Pts',(20.2935358883611,-16.9218650751948,-14.8500370296196));
#54061=CARTESIAN_POINT('Ctrl Pts',(20.2909850430174,-16.9251769135511,-14.0501277865439));
#54062=CARTESIAN_POINT('Ctrl Pts',(20.6448529485284,-17.1976900198726,-14.072256704909));
#54063=CARTESIAN_POINT('Ctrl Pts',(21.4803859272375,-18.2487089187753,-14.1367775588346));
#54064=CARTESIAN_POINT('Ctrl Pts',(21.2244734545047,-20.6727073586304,-14.2436903483206));
#54065=CARTESIAN_POINT('Ctrl Pts',(18.6352034645934,-21.9774803067,-14.3708661550021));
#54066=CARTESIAN_POINT('Ctrl Pts',(16.5197423660721,-20.7321305462553,-14.478539335638));
#54067=CARTESIAN_POINT('Ctrl Pts',(16.1790023713152,-19.4133917175901,-14.5438205807135));
#54068=CARTESIAN_POINT('Ctrl Pts',(16.1781028623508,-18.9514411453429,-14.5667098902285));
#54069=CARTESIAN_POINT('Origin',(18.734,-18.952,1.76670989022851));
#54070=CARTESIAN_POINT('',(20.293535888361,-16.9218650751948,-13.2501880128791));
#54071=CARTESIAN_POINT('',(20.293535888361,-16.9218650751948,-13.3166223775484));
#54072=CARTESIAN_POINT('',(20.293535888361,-16.9218650751948,1.76670989022851));
#54073=CARTESIAN_POINT('',(16.1740010575059,-18.949673107456,-13.8332901097715));
#54074=CARTESIAN_POINT('Ctrl Pts',(20.293535888361,-16.9218650751947,-13.3166223775484));
#54075=CARTESIAN_POINT('Ctrl Pts',(20.3602103318618,-16.9730839307523,-13.3207986507083));
#54076=CARTESIAN_POINT('Ctrl Pts',(20.4243042225914,-17.0275488083323,-13.3249749238681));
#54077=CARTESIAN_POINT('Ctrl Pts',(20.4855003242258,-17.0849577899156,-13.329151197028));
#54078=CARTESIAN_POINT('Ctrl Pts',(20.546804110082,-17.1424677916838,-13.3333348190011));
#54079=CARTESIAN_POINT('Ctrl Pts',(20.6051996004652,-17.2029319152096,-13.3375184409743));
#54080=CARTESIAN_POINT('Ctrl Pts',(20.6604076911347,-17.2660126312641,-13.3417020629474));
#54081=CARTESIAN_POINT('Ctrl Pts',(20.7059043008509,-17.3179970176855,-13.3451497571858));
#54082=CARTESIAN_POINT('Ctrl Pts',(20.7492369233109,-17.3717576847194,-13.3485974514241));
#54083=CARTESIAN_POINT('Ctrl Pts',(20.7902715950829,-17.4270911085396,-13.3520451456625));
#54084=CARTESIAN_POINT('Ctrl Pts',(20.8400773745207,-17.4942519796594,-13.3562297800555));
#54085=CARTESIAN_POINT('Ctrl Pts',(20.8866820202992,-17.5639804959204,-13.3604144144486));
#54086=CARTESIAN_POINT('Ctrl Pts',(20.9298102405872,-17.6359386840529,-13.3645990488416));
#54087=CARTESIAN_POINT('Ctrl Pts',(20.9728770731919,-17.7077944486113,-13.3687777269256));
#54088=CARTESIAN_POINT('Ctrl Pts',(21.0124770746365,-17.7818731899369,-13.3729564050095));
#54089=CARTESIAN_POINT('Ctrl Pts',(21.0483765860078,-17.8578057676359,-13.3771350830935));
#54090=CARTESIAN_POINT('Ctrl Pts',(21.0849195703199,-17.9350993822183,-13.3813886609789));
#54091=CARTESIAN_POINT('Ctrl Pts',(21.1176278099319,-18.0143135596366,-13.3856422388643));
#54092=CARTESIAN_POINT('Ctrl Pts',(21.1463023579538,-18.0950301441645,-13.3898958167498));
#54093=CARTESIAN_POINT('Ctrl Pts',(21.1744209939084,-18.1741818801958,-13.3940669307277));
#54094=CARTESIAN_POINT('Ctrl Pts',(21.1986607834443,-18.2547778355445,-13.3982380447057));
#54095=CARTESIAN_POINT('Ctrl Pts',(21.2188822787495,-18.3364026797032,-13.4024091586836));
#54096=CARTESIAN_POINT('Ctrl Pts',(21.2390969885367,-18.4180001338572,-13.406578873004));
#54097=CARTESIAN_POINT('Ctrl Pts',(21.2552959714612,-18.5006253449795,-13.4107485873244));
#54098=CARTESIAN_POINT('Ctrl Pts',(21.2673900009521,-18.5838490756821,-13.4149183016447));
#54099=CARTESIAN_POINT('Ctrl Pts',(21.2794836000854,-18.667069844927,-13.4190878675888));
#54100=CARTESIAN_POINT('Ctrl Pts',(21.2874724709,-18.750888636033,-13.4232574335328));
#54101=CARTESIAN_POINT('Ctrl Pts',(21.2913189573956,-18.83486866284,-13.4274269994769));
#54102=CARTESIAN_POINT('Ctrl Pts',(21.2953006816113,-18.9218013237892,-13.4317431622158));
#54103=CARTESIAN_POINT('Ctrl Pts',(21.2948432851383,-19.0089062426183,-13.4360593249547));
#54104=CARTESIAN_POINT('Ctrl Pts',(21.2899637772452,-19.0956981886119,-13.4403754876936));
#54105=CARTESIAN_POINT('Ctrl Pts',(21.2852432188086,-19.1796628960937,-13.4445510518853));
#54106=CARTESIAN_POINT('Ctrl Pts',(21.2763843217563,-19.26333424434,-13.448726616077));
#54107=CARTESIAN_POINT('Ctrl Pts',(21.2634552371752,-19.3462793465638,-13.4529021802687));
#54108=CARTESIAN_POINT('Ctrl Pts',(21.249873135268,-19.4334138087177,-13.4572886422812));
#54109=CARTESIAN_POINT('Ctrl Pts',(21.231798989378,-19.5197461599058,-13.4616751042938));
#54110=CARTESIAN_POINT('Ctrl Pts',(21.2093716504546,-19.6047903125243,-13.4660615663063));
#54111=CARTESIAN_POINT('Ctrl Pts',(21.1869443115312,-19.6898344651427,-13.4704480283188));
#54112=CARTESIAN_POINT('Ctrl Pts',(21.1601640287334,-19.7735898897036,-13.4748344903314));
#54113=CARTESIAN_POINT('Ctrl Pts',(21.1292278697972,-19.855594738667,-13.4792209523439));
#54114=CARTESIAN_POINT('Ctrl Pts',(21.099715129392,-19.9338264229693,-13.483405586737));
#54115=CARTESIAN_POINT('Ctrl Pts',(21.0663106928263,-20.0107562780701,-13.48759022113));
#54116=CARTESIAN_POINT('Ctrl Pts',(21.0291497318875,-20.0859698885847,-13.4917748555231));
#54117=CARTESIAN_POINT('Ctrl Pts',(20.9920416649769,-20.1610764418345,-13.495953533607));
#54118=CARTESIAN_POINT('Ctrl Pts',(20.9511878964455,-20.2344711938786,-13.500132211691));
#54119=CARTESIAN_POINT('Ctrl Pts',(20.9067723398086,-20.3057578658544,-13.5043108897749));
#54120=CARTESIAN_POINT('Ctrl Pts',(20.8615606662401,-20.3783223001923,-13.5085644676604));
#54121=CARTESIAN_POINT('Ctrl Pts',(20.8126584286878,-20.4487018853357,-13.5128180455458));
#54122=CARTESIAN_POINT('Ctrl Pts',(20.7603095437647,-20.5165029986702,-13.5170716234313));
#54123=CARTESIAN_POINT('Ctrl Pts',(20.7089755441263,-20.5829896551198,-13.5212427374092));
#54124=CARTESIAN_POINT('Ctrl Pts',(20.6543276385962,-20.6469965440968,-13.5254138513872));
#54125=CARTESIAN_POINT('Ctrl Pts',(20.596639573948,-20.7081816015329,-13.5295849653651));
#54126=CARTESIAN_POINT('Ctrl Pts',(20.5389708670871,-20.7693461277322,-13.5337546796855));
#54127=CARTESIAN_POINT('Ctrl Pts',(20.4782643424754,-20.8276903684964,-13.5379243940059));
#54128=CARTESIAN_POINT('Ctrl Pts',(20.4148326241775,-20.8829069603429,-13.5420941083262));
#54129=CARTESIAN_POINT('Ctrl Pts',(20.3514031630524,-20.938121587346,-13.5462636742703));
#54130=CARTESIAN_POINT('Ctrl Pts',(20.2852490485947,-20.9902084853113,-13.5504332402143));
#54131=CARTESIAN_POINT('Ctrl Pts',(20.216717166363,-21.0388995674379,-13.5546028061583));
#54132=CARTESIAN_POINT('Ctrl Pts',(20.1457757876953,-21.0893025679451,-13.5589189688973));
#54133=CARTESIAN_POINT('Ctrl Pts',(20.0722867555766,-21.1360662103826,-13.5632351316362));
#54134=CARTESIAN_POINT('Ctrl Pts',(19.9966672790439,-21.1789421506702,-13.5675512943751));
#54135=CARTESIAN_POINT('Ctrl Pts',(19.9235110990054,-21.2204214117129,-13.5717268585668));
#54136=CARTESIAN_POINT('Ctrl Pts',(19.848361583456,-21.2582621950959,-13.5759024227585));
#54137=CARTESIAN_POINT('Ctrl Pts',(19.7716196105685,-21.2922874916907,-13.5800779869502));
#54138=CARTESIAN_POINT('Ctrl Pts',(19.6910015830673,-21.3280313251289,-13.5844644489627));
#54139=CARTESIAN_POINT('Ctrl Pts',(19.6086265457421,-21.3595638930066,-13.5888509109752));
#54140=CARTESIAN_POINT('Ctrl Pts',(19.5249783787279,-21.3867388369977,-13.5932373729878));
#54141=CARTESIAN_POINT('Ctrl Pts',(19.4413302117137,-21.4139137809889,-13.5976238350003));
#54142=CARTESIAN_POINT('Ctrl Pts',(19.3564094950911,-21.4367310239951,-13.6020102970128));
#54143=CARTESIAN_POINT('Ctrl Pts',(19.2707112385803,-21.4551062794819,-13.6063967590254));
#54144=CARTESIAN_POINT('Ctrl Pts',(19.1889560858866,-21.4726360622251,-13.6105813934184));
#54145=CARTESIAN_POINT('Ctrl Pts',(19.1061890642126,-21.486188888916,-13.6147660278115));
#54146=CARTESIAN_POINT('Ctrl Pts',(19.022831797239,-21.4956541024486,-13.6189506622045));
#54147=CARTESIAN_POINT('Ctrl Pts',(18.9395931790174,-21.5051058434214,-13.6231293402885));
#54148=CARTESIAN_POINT('Ctrl Pts',(18.8557664374668,-21.5104814765754,-13.6273080183724));
#54149=CARTESIAN_POINT('Ctrl Pts',(18.7717843292959,-21.5117211458398,-13.6314866964564));
#54150=CARTESIAN_POINT('Ctrl Pts',(18.686296902193,-21.5129830352849,-13.6357402743418));
#54151=CARTESIAN_POINT('Ctrl Pts',(18.6006489552154,-21.5099591270341,-13.6399938522272));
#54152=CARTESIAN_POINT('Ctrl Pts',(18.5153034901261,-21.5026414559026,-13.6442474301127));
#54153=CARTESIAN_POINT('Ctrl Pts',(18.4316126134154,-21.4954656521053,-13.6484185440906));
#54154=CARTESIAN_POINT('Ctrl Pts',(18.3482130743116,-21.4841611267896,-13.6525896580686));
#54155=CARTESIAN_POINT('Ctrl Pts',(18.2655406684996,-21.4687729048784,-13.6567607720465));
#54156=CARTESIAN_POINT('Ctrl Pts',(18.1828960042119,-21.4533898466338,-13.6609304863669));
#54157=CARTESIAN_POINT('Ctrl Pts',(18.1009784405235,-21.4339258973908,-13.6651002006873));
#54158=CARTESIAN_POINT('Ctrl Pts',(18.0202156389588,-21.4104775544904,-13.6692699150076));
#54159=CARTESIAN_POINT('Ctrl Pts',(17.9394557112809,-21.3870300459825,-13.6734394809517));
#54160=CARTESIAN_POINT('Ctrl Pts',(17.8598509055781,-21.3595985548015,-13.6776090468957));
#54161=CARTESIAN_POINT('Ctrl Pts',(17.7818144029982,-21.3283296465058,-13.6817786128398));
#54162=CARTESIAN_POINT('Ctrl Pts',(17.7010342332561,-21.2959613619688,-13.6860947755787));
#54163=CARTESIAN_POINT('Ctrl Pts',(17.621935191217,-21.2594809885572,-13.6904109383176));
#54164=CARTESIAN_POINT('Ctrl Pts',(17.5449519222894,-21.219104909106,-13.6947271010565));
#54165=CARTESIAN_POINT('Ctrl Pts',(17.4704763752499,-21.1800440761962,-13.6989026652482));
#54166=CARTESIAN_POINT('Ctrl Pts',(17.3979812574151,-21.1373377246259,-13.7030782294399));
#54167=CARTESIAN_POINT('Ctrl Pts',(17.3278323932016,-21.091227117814,-13.7072537936316));
#54168=CARTESIAN_POINT('Ctrl Pts',(17.2541404766197,-21.0427875738696,-13.7116402556441));
#54169=CARTESIAN_POINT('Ctrl Pts',(17.1830385318335,-20.9905911845411,-13.7160267176566));
#54170=CARTESIAN_POINT('Ctrl Pts',(17.1149115381732,-20.9349655954603,-13.7204131796692));
#54171=CARTESIAN_POINT('Ctrl Pts',(17.0467845445129,-20.8793400063795,-13.7247996416817));
#54172=CARTESIAN_POINT('Ctrl Pts',(16.9816328807925,-20.8202856635707,-13.7291861036943));
#54173=CARTESIAN_POINT('Ctrl Pts',(16.9197953580219,-20.7581731691688,-13.7335725657068));
#54174=CARTESIAN_POINT('Ctrl Pts',(16.8612222805613,-20.6993396360182,-13.7377274633762));
#54175=CARTESIAN_POINT('Ctrl Pts',(16.8053896617352,-20.6375286216453,-13.7418823610455));
#54176=CARTESIAN_POINT('Ctrl Pts',(16.7526212754374,-20.5730300274365,-13.7460372587149));
#54177=CARTESIAN_POINT('Ctrl Pts',(16.7002946208399,-20.5090713601742,-13.7501573751423));
#54178=CARTESIAN_POINT('Ctrl Pts',(16.6509814300939,-20.4424702805592,-13.7542774915697));
#54179=CARTESIAN_POINT('Ctrl Pts',(16.6049624110076,-20.3735480803186,-13.7583976079971));
#54180=CARTESIAN_POINT('Ctrl Pts',(16.5589874739682,-20.3046919012954,-13.7625137777266));
#54181=CARTESIAN_POINT('Ctrl Pts',(16.5163007099123,-20.2335194044224,-13.7666299474561));
#54182=CARTESIAN_POINT('Ctrl Pts',(16.4771421768208,-20.1603843618463,-13.7707461171856));
#54183=CARTESIAN_POINT('Ctrl Pts',(16.4380086398887,-20.0872960037358,-13.7748596594307));
#54184=CARTESIAN_POINT('Ctrl Pts',(16.4023990866291,-20.0122480031431,-13.7789732016757));
#54185=CARTESIAN_POINT('Ctrl Pts',(16.3705090605919,-19.9356211564092,-13.7830867439208));
#54186=CARTESIAN_POINT('Ctrl Pts',(16.3380758082443,-19.8576890200784,-13.7872703577417));
#54187=CARTESIAN_POINT('Ctrl Pts',(16.3094902338592,-19.7781241832446,-13.7914539715626));
#54188=CARTESIAN_POINT('Ctrl Pts',(16.2849076425233,-19.6973500013747,-13.7956375853835));
#54189=CARTESIAN_POINT('Ctrl Pts',(16.2607361379239,-19.6179265800639,-13.7997512379815));
#54190=CARTESIAN_POINT('Ctrl Pts',(16.2404348481341,-19.5373344318006,-13.8038648905795));
#54191=CARTESIAN_POINT('Ctrl Pts',(16.2241009663662,-19.455990913573,-13.8079785431774));
#54192=CARTESIAN_POINT('Ctrl Pts',(16.2073503971231,-19.3725722716413,-13.8121971376098));
#54193=CARTESIAN_POINT('Ctrl Pts',(16.1947725425284,-19.2883639128979,-13.8164157320421));
#54194=CARTESIAN_POINT('Ctrl Pts',(16.1864159534739,-19.2038243949375,-13.8206343264745));
#54195=CARTESIAN_POINT('Ctrl Pts',(16.1780593644194,-19.1192848769771,-13.8248529209068));
#54196=CARTESIAN_POINT('Ctrl Pts',(16.1739240322153,-19.0344147354448,-13.8290715153392));
#54197=CARTESIAN_POINT('Ctrl Pts',(16.1740010575059,-18.949673107456,-13.8332901097715));
#54198=CARTESIAN_POINT('Ctrl Pts',(16.1735504202813,-18.9496726978525,-13.8332901097715));
#54199=CARTESIAN_POINT('Ctrl Pts',(16.1718449019213,-18.765781352641,-13.8424428639771));
#54200=CARTESIAN_POINT('Ctrl Pts',(16.2739023737919,-17.7320561796712,-13.8939875537431));
#54201=CARTESIAN_POINT('Ctrl Pts',(17.6781137265109,-16.1150307104843,-13.9879241790696));
#54202=CARTESIAN_POINT('Ctrl Pts',(19.6033699086469,-16.3924605121711,-14.0732424035937));
#54203=CARTESIAN_POINT('Ctrl Pts',(20.287632224731,-16.9120027987701,-14.1161686925573));
#54204=CARTESIAN_POINT('Ctrl Pts',(20.2961055948522,-16.9185282149957,-14.1167030459603));
#54205=CARTESIAN_POINT('',(16.1740010826188,-18.9543543591274,-13.7667098774921));
#54206=CARTESIAN_POINT('Ctrl Pts',(16.1744182719781,-18.9543537193378,-13.7667098902285));
#54207=CARTESIAN_POINT('Ctrl Pts',(16.1802301241212,-18.3145386211268,-13.7985275695778));
#54208=CARTESIAN_POINT('Ctrl Pts',(16.7471749526305,-16.8130883553205,-13.8727371844876));
#54209=CARTESIAN_POINT('Ctrl Pts',(18.7905373395045,-16.1321011936949,-13.9672098165927));
#54210=CARTESIAN_POINT('Ctrl Pts',(19.9669551317519,-16.6756419987287,-14.0298647693485));
#54211=CARTESIAN_POINT('Ctrl Pts',(20.2909850430174,-16.9251769135511,-14.0501277865439));
#54212=CARTESIAN_POINT('Ctrl Pts',(20.293535888361,-16.9218650751948,-13.2501880128791));
#54213=CARTESIAN_POINT('Ctrl Pts',(20.362109517474,-16.9745428722663,-13.2544909999071));
#54214=CARTESIAN_POINT('Ctrl Pts',(20.4280925084506,-17.030761458256,-13.2587939869351));
#54215=CARTESIAN_POINT('Ctrl Pts',(20.4911037568818,-17.0902303075966,-13.2630969739631));
#54216=CARTESIAN_POINT('Ctrl Pts',(20.5521864303202,-17.1478790035749,-13.2672682601696));
#54217=CARTESIAN_POINT('Ctrl Pts',(20.6104762833583,-17.2085815368414,-13.2714395463762));
#54218=CARTESIAN_POINT('Ctrl Pts',(20.6656594876492,-17.2720322551385,-13.2756108325828));
#54219=CARTESIAN_POINT('Ctrl Pts',(20.7208228024687,-17.3354601041358,-13.2797806153486));
#54220=CARTESIAN_POINT('Ctrl Pts',(20.772881390616,-17.4016338242775,-13.2839503981144));
#54221=CARTESIAN_POINT('Ctrl Pts',(20.8215597182926,-17.4702124232663,-13.2881201808803));
#54222=CARTESIAN_POINT('Ctrl Pts',(20.8702351033456,-17.5387868766527,-13.2922897115811));
#54223=CARTESIAN_POINT('Ctrl Pts',(20.9155303683828,-17.6097655443968,-13.296459242282));
#54224=CARTESIAN_POINT('Ctrl Pts',(20.9572123841055,-17.6827771294371,-13.3006287729829));
#54225=CARTESIAN_POINT('Ctrl Pts',(20.9989043835118,-17.7558062022249,-13.3047993023705));
#54226=CARTESIAN_POINT('Ctrl Pts',(21.0369811882063,-17.8308687591357,-13.308969831758));
#54227=CARTESIAN_POINT('Ctrl Pts',(21.0712555052538,-17.907568717837,-13.3131403611456));
#54228=CARTESIAN_POINT('Ctrl Pts',(21.105568902902,-17.9843561321234,-13.3173156458954));
#54229=CARTESIAN_POINT('Ctrl Pts',(21.1360709750617,-18.0627842525363,-13.3214909306453));
#54230=CARTESIAN_POINT('Ctrl Pts',(21.1626227268541,-18.1424373707935,-13.3256662153951));
#54231=CARTESIAN_POINT('Ctrl Pts',(21.1891927341781,-18.2221452541761,-13.3298443708422));
#54232=CARTESIAN_POINT('Ctrl Pts',(21.2118068930584,-18.3030793690225,-13.3340225262894));
#54233=CARTESIAN_POINT('Ctrl Pts',(21.2303768173696,-18.3848115077863,-13.3382006817365));
#54234=CARTESIAN_POINT('Ctrl Pts',(21.248976043095,-18.4666726113865,-13.3423854298796));
#54235=CARTESIAN_POINT('Ctrl Pts',(21.2635182251543,-18.5493337992202,-13.3465701780226));
#54236=CARTESIAN_POINT('Ctrl Pts',(21.2739665901778,-18.6323600137957,-13.3507549261656));
#54237=CARTESIAN_POINT('Ctrl Pts',(21.2762176599804,-18.6502477698261,-13.3516565179606));
#54238=CARTESIAN_POINT('Ctrl Pts',(21.278278897623,-18.6681524664035,-13.3525581097556));
#54239=CARTESIAN_POINT('Ctrl Pts',(21.2801502518719,-18.6860697555883,-13.3534597015506));
#54240=CARTESIAN_POINT('Ctrl Pts',(21.2888359269133,-18.7692307880738,-13.3576443359436));
#54241=CARTESIAN_POINT('Ctrl Pts',(21.2934592377886,-18.852972557727,-13.3618289703367));
#54242=CARTESIAN_POINT('Ctrl Pts',(21.2939552539536,-18.9368640244712,-13.3660136047297));
#54243=CARTESIAN_POINT('Ctrl Pts',(21.294450564101,-19.0206360820962,-13.3701922828137));
#54244=CARTESIAN_POINT('Ctrl Pts',(21.2908302458307,-19.1045569574875,-13.3743709608976));
#54245=CARTESIAN_POINT('Ctrl Pts',(21.2830810689264,-19.1881899744725,-13.3785496389816));
#54246=CARTESIAN_POINT('Ctrl Pts',(21.2751929935952,-19.2733220531809,-13.382803216867));
#54247=CARTESIAN_POINT('Ctrl Pts',(21.2630265340501,-19.3581553727241,-13.3870567947524));
#54248=CARTESIAN_POINT('Ctrl Pts',(21.2466232879999,-19.4422287349806,-13.3913103726379));
#54249=CARTESIAN_POINT('Ctrl Pts',(21.2305380508826,-19.5246721710542,-13.3954814866158));
#54250=CARTESIAN_POINT('Ctrl Pts',(21.2103789301821,-19.6063843810837,-13.3996526005938));
#54251=CARTESIAN_POINT('Ctrl Pts',(21.1862373001536,-19.686936884185,-13.4038237145717));
#54252=CARTESIAN_POINT('Ctrl Pts',(21.1621037710821,-19.7674623571159,-13.4079934288921));
#54253=CARTESIAN_POINT('Ctrl Pts',(21.133990518692,-19.8468284556772,-13.4121631432125));
#54254=CARTESIAN_POINT('Ctrl Pts',(21.1020392245072,-19.9246202913754,-13.4163328575329));
#54255=CARTESIAN_POINT('Ctrl Pts',(21.0700890672866,-20.0024093589063,-13.4205024234769));
#54256=CARTESIAN_POINT('Ctrl Pts',(21.0343013153839,-20.0786238497405,-13.4246719894209));
#54257=CARTESIAN_POINT('Ctrl Pts',(20.9948658827286,-20.1528686274167,-13.428841555365));
#54258=CARTESIAN_POINT('Ctrl Pts',(20.9540439489101,-20.2297237598852,-13.4331577181039));
#54259=CARTESIAN_POINT('Ctrl Pts',(20.9093133043205,-20.3044676260572,-13.4374738808428));
#54260=CARTESIAN_POINT('Ctrl Pts',(20.8609355752996,-20.3766912151498,-13.4417900435817));
#54261=CARTESIAN_POINT('Ctrl Pts',(20.8141337457131,-20.4465621284243,-13.4459656077734));
#54262=CARTESIAN_POINT('Ctrl Pts',(20.7639191093594,-20.514074089366,-13.4501411719651));
#54263=CARTESIAN_POINT('Ctrl Pts',(20.71057067018,-20.5788891744014,-13.4543167361568));
#54264=CARTESIAN_POINT('Ctrl Pts',(20.6545277281615,-20.6469779152985,-13.4587031981693));
#54265=CARTESIAN_POINT('Ctrl Pts',(20.5950264806454,-20.7120897510531,-13.4630896601819));
#54266=CARTESIAN_POINT('Ctrl Pts',(20.5324338669328,-20.7738769514622,-13.4674761221944));
#54267=CARTESIAN_POINT('Ctrl Pts',(20.4698412532202,-20.8356641518712,-13.4718625842069));
#54268=CARTESIAN_POINT('Ctrl Pts',(20.4041577572906,-20.8941263879947,-13.4762490462195));
#54269=CARTESIAN_POINT('Ctrl Pts',(20.3357880909558,-20.9489664272771,-13.480635508232));
#54270=CARTESIAN_POINT('Ctrl Pts',(20.2705642143173,-21.0012831950598,-13.4848201426251));
#54271=CARTESIAN_POINT('Ctrl Pts',(20.2026531489501,-21.0504984994761,-13.4890047770181));
#54272=CARTESIAN_POINT('Ctrl Pts',(20.1323821856731,-21.0963244303958,-13.4931894114112));
#54273=CARTESIAN_POINT('Ctrl Pts',(20.0622112444146,-21.1420851337748,-13.4973680894951));
#54274=CARTESIAN_POINT('Ctrl Pts',(19.9896874593621,-21.1844657972013,-13.5015467675791));
#54275=CARTESIAN_POINT('Ctrl Pts',(19.9151708448061,-21.2232189316268,-13.505725445663));
#54276=CARTESIAN_POINT('Ctrl Pts',(19.8393185734882,-21.2626666881356,-13.5099790235484));
#54277=CARTESIAN_POINT('Ctrl Pts',(19.7614017031197,-21.2983552879197,-13.5142326014339));
#54278=CARTESIAN_POINT('Ctrl Pts',(19.6818305443852,-21.3300700702735,-13.5184861793193));
#54279=CARTESIAN_POINT('Ctrl Pts',(19.603802027833,-21.361169999685,-13.5226572932973));
#54280=CARTESIAN_POINT('Ctrl Pts',(19.5241832407486,-21.3884486389203,-13.5268284072752));
#54281=CARTESIAN_POINT('Ctrl Pts',(19.4433839268982,-21.4117508906917,-13.5309995212532));
#54282=CARTESIAN_POINT('Ctrl Pts',(19.3626117260378,-21.4350453231675,-13.5351692355735));
#54283=CARTESIAN_POINT('Ctrl Pts',(19.2806602267964,-21.4543658907802,-13.5393389498939));
#54284=CARTESIAN_POINT('Ctrl Pts',(19.1979549742611,-21.4696071539973,-13.5435086642143));
#54285=CARTESIAN_POINT('Ctrl Pts',(19.1152526647336,-21.4848478748648,-13.5476782301583));
#54286=CARTESIAN_POINT('Ctrl Pts',(19.0317971078102,-21.4960094974156,-13.5518477961024));
#54287=CARTESIAN_POINT('Ctrl Pts',(18.9480233475311,-21.5030378293376,-13.5560173620464));
#54288=CARTESIAN_POINT('Ctrl Pts',(18.8613042051868,-21.5103132687396,-13.5603335247854));
#54289=CARTESIAN_POINT('Ctrl Pts',(18.7742445926768,-21.5131593125471,-13.5646496875243));
#54290=CARTESIAN_POINT('Ctrl Pts',(18.6873300367179,-21.5115745573293,-13.5689658502632));
#54291=CARTESIAN_POINT('Ctrl Pts',(18.6032467132776,-21.5100414253459,-13.5731414144549));
#54292=CARTESIAN_POINT('Ctrl Pts',(18.5192996078627,-21.5043618068031,-13.5773169786466));
#54293=CARTESIAN_POINT('Ctrl Pts',(18.4359238802629,-21.4945873882411,-13.5814925428382));
#54294=CARTESIAN_POINT('Ctrl Pts',(18.3483370428691,-21.4843192870339,-13.5858790048508));
#54295=CARTESIAN_POINT('Ctrl Pts',(18.2613813964208,-21.4695319558998,-13.5902654668633));
#54296=CARTESIAN_POINT('Ctrl Pts',(18.1755479442734,-21.4503457129578,-13.5946519288759));
#54297=CARTESIAN_POINT('Ctrl Pts',(18.089714492126,-21.4311594700159,-13.5990383908884));
#54298=CARTESIAN_POINT('Ctrl Pts',(18.0050037728348,-21.4075745441673,-13.6034248529009));
#54299=CARTESIAN_POINT('Ctrl Pts',(17.921884774769,-21.379770347654,-13.6078113149135));
#54300=CARTESIAN_POINT('Ctrl Pts',(17.842590205016,-21.353245463438,-13.6119959493065));
#54301=CARTESIAN_POINT('Ctrl Pts',(17.7644489508446,-21.3227823154618,-13.6161805836996));
#54302=CARTESIAN_POINT('Ctrl Pts',(17.6878802554244,-21.2885002632162,-13.6203652180926));
#54303=CARTESIAN_POINT('Ctrl Pts',(17.6114205460648,-21.2542670072286,-13.6245438961766));
#54304=CARTESIAN_POINT('Ctrl Pts',(17.536529365682,-21.2162258304372,-13.6287225742605));
#54305=CARTESIAN_POINT('Ctrl Pts',(17.4636096823068,-21.1745454867587,-13.6329012523445));
#54306=CARTESIAN_POINT('Ctrl Pts',(17.3893829660135,-21.1321180528749,-13.6371548302299));
#54307=CARTESIAN_POINT('Ctrl Pts',(17.3171995773182,-21.0859198576823,-13.6414084081153));
#54308=CARTESIAN_POINT('Ctrl Pts',(17.2474621052952,-21.0361797157651,-13.6456619860008));
#54309=CARTESIAN_POINT('Ctrl Pts',(17.1790766302489,-20.9874038835589,-13.6498330999787));
#54310=CARTESIAN_POINT('Ctrl Pts',(17.1130434722312,-20.9352224936048,-13.6540042139567));
#54311=CARTESIAN_POINT('Ctrl Pts',(17.0497148300457,-20.879896124347,-13.6581753279346));
#54312=CARTESIAN_POINT('Ctrl Pts',(16.9864074383977,-20.8245883203866,-13.662345042255));
#54313=CARTESIAN_POINT('Ctrl Pts',(16.9258031063752,-20.7661379354358,-13.6665147565754));
#54314=CARTESIAN_POINT('Ctrl Pts',(16.8682208314237,-20.7048457131495,-13.6706844708957));
#54315=CARTESIAN_POINT('Ctrl Pts',(16.8106406054966,-20.6435556719036,-13.6748540368398));
#54316=CARTESIAN_POINT('Ctrl Pts',(16.7560825371937,-20.5794243302491,-13.6790236027838));
#54317=CARTESIAN_POINT('Ctrl Pts',(16.7048276747609,-20.512788158106,-13.6831931687279));
#54318=CARTESIAN_POINT('Ctrl Pts',(16.6517707545947,-20.4438091403549,-13.6875093314668));
#54319=CARTESIAN_POINT('Ctrl Pts',(16.6022539651132,-20.3721462932498,-13.6918254942057));
#54320=CARTESIAN_POINT('Ctrl Pts',(16.5565412927829,-20.2982071082729,-13.6961416569446));
#54321=CARTESIAN_POINT('Ctrl Pts',(16.5123177059456,-20.2266764844696,-13.7003172211363));
#54322=CARTESIAN_POINT('Ctrl Pts',(16.4716543903427,-20.1530159839383,-13.704492785328));
#54323=CARTESIAN_POINT('Ctrl Pts',(16.4347434295141,-20.0776194841408,-13.7086683495197));
#54324=CARTESIAN_POINT('Ctrl Pts',(16.3959681838015,-19.9984148863766,-13.7130548115322));
#54325=CARTESIAN_POINT('Ctrl Pts',(16.3613345469612,-19.9172948468639,-13.7174412735447));
#54326=CARTESIAN_POINT('Ctrl Pts',(16.3310071212994,-19.8347373476376,-13.7218277355573));
#54327=CARTESIAN_POINT('Ctrl Pts',(16.3006796956376,-19.7521798484113,-13.7262141975698));
#54328=CARTESIAN_POINT('Ctrl Pts',(16.2746585801944,-19.668185466211,-13.7306006595824));
#54329=CARTESIAN_POINT('Ctrl Pts',(16.253046772176,-19.5832456584798,-13.7349871215949));
#54330=CARTESIAN_POINT('Ctrl Pts',(16.2263033450823,-19.4781373050522,-13.7404151277539));
#54331=CARTESIAN_POINT('Ctrl Pts',(16.2062281520528,-19.3712684537335,-13.745843133913));
#54332=CARTESIAN_POINT('Ctrl Pts',(16.193006541868,-19.2633715557504,-13.751271140072));
#54333=CARTESIAN_POINT('Ctrl Pts',(16.1804712473274,-19.161075437704,-13.7564173858787));
#54334=CARTESIAN_POINT('Ctrl Pts',(16.1740962693079,-19.0578550605845,-13.7615636316854));
#54335=CARTESIAN_POINT('Ctrl Pts',(16.1740010826188,-18.9543543591274,-13.7667098774921));
#54336=CARTESIAN_POINT('Origin',(18.734,-18.952,1.76670989022851));
#54337=CARTESIAN_POINT('',(20.2954167197789,-16.919379410122,-12.4500366865268));
#54338=CARTESIAN_POINT('',(20.293535888361,-16.9218650751948,-12.5167193514887));
#54339=CARTESIAN_POINT('',(20.293535888361,-16.9218650751948,1.76670989022851));
#54340=CARTESIAN_POINT('',(16.174000001606,-18.9520906788002,-13.0332901097364));
#54341=CARTESIAN_POINT('Ctrl Pts',(20.293535888361,-16.9218650751948,-12.5167193514888));
#54342=CARTESIAN_POINT('Ctrl Pts',(20.3602126490049,-16.9730857107659,-12.5208888673399));
#54343=CARTESIAN_POINT('Ctrl Pts',(20.4243799356247,-17.0276073698207,-12.5250583831911));
#54344=CARTESIAN_POINT('Ctrl Pts',(20.4857025055872,-17.085147479869,-12.5292278990423));
#54345=CARTESIAN_POINT('Ctrl Pts',(20.5470295704357,-17.1426918075526,-12.533397720515));
#54346=CARTESIAN_POINT('Ctrl Pts',(20.6055111700133,-17.2032547098065,-12.5375675419877));
#54347=CARTESIAN_POINT('Ctrl Pts',(20.6608480451726,-17.2665159120257,-12.5417373634604));
#54348=CARTESIAN_POINT('Ctrl Pts',(20.7162427485479,-17.3298432235519,-12.5459115424856));
#54349=CARTESIAN_POINT('Ctrl Pts',(20.768485861661,-17.3958741188096,-12.5500857215108));
#54350=CARTESIAN_POINT('Ctrl Pts',(20.8173179976359,-17.4642546855304,-12.554259900536));
#54351=CARTESIAN_POINT('Ctrl Pts',(20.866176429233,-17.5326720745099,-12.5584363273153));
#54352=CARTESIAN_POINT('Ctrl Pts',(20.9116199773849,-17.6034412672135,-12.5626127540945));
#54353=CARTESIAN_POINT('Ctrl Pts',(20.9534335859414,-17.6761808288023,-12.5667891808738));
#54354=CARTESIAN_POINT('Ctrl Pts',(20.9953200425185,-17.7490471178675,-12.570972883859));
#54355=CARTESIAN_POINT('Ctrl Pts',(21.033563718021,-17.8238902224893,-12.5751565868442));
#54356=CARTESIAN_POINT('Ctrl Pts',(21.0679964529279,-17.9003058630381,-12.5793402898293));
#54357=CARTESIAN_POINT('Ctrl Pts',(21.0944703234963,-17.9590586104676,-12.5825569617442));
#54358=CARTESIAN_POINT('Ctrl Pts',(21.1186923494888,-18.0187404702052,-12.585773633659));
#54359=CARTESIAN_POINT('Ctrl Pts',(21.1406062076889,-18.0791617783844,-12.5889903055739));
#54360=CARTESIAN_POINT('Ctrl Pts',(21.1691143947643,-18.1577650960285,-12.5931749399669));
#54361=CARTESIAN_POINT('Ctrl Pts',(21.193820633909,-18.2379128391996,-12.59735957436));
#54362=CARTESIAN_POINT('Ctrl Pts',(21.2145578396958,-18.319202398927,-12.601544208753));
#54363=CARTESIAN_POINT('Ctrl Pts',(21.2352655286369,-18.4003762530279,-12.605722886837));
#54364=CARTESIAN_POINT('Ctrl Pts',(21.25201529302,-18.4826882535134,-12.6099015649209));
#54365=CARTESIAN_POINT('Ctrl Pts',(21.2646888572063,-18.5657178388643,-12.6140802430049));
#54366=CARTESIAN_POINT('Ctrl Pts',(21.2775895859224,-18.6502356698601,-12.6183338208903));
#54367=CARTESIAN_POINT('Ctrl Pts',(21.2862663809329,-18.735496610923,-12.6225873987757));
#54368=CARTESIAN_POINT('Ctrl Pts',(21.2906482513971,-18.8210430657493,-12.6268409766612));
#54369=CARTESIAN_POINT('Ctrl Pts',(21.2949451707518,-18.9049310356185,-12.6310120906391));
#54370=CARTESIAN_POINT('Ctrl Pts',(21.2951121858363,-18.9890930669704,-12.6351832046171));
#54371=CARTESIAN_POINT('Ctrl Pts',(21.2911345092731,-19.073091294008,-12.639354318595));
#54372=CARTESIAN_POINT('Ctrl Pts',(21.2871581674578,-19.1570613346294,-12.6435240329154));
#54373=CARTESIAN_POINT('Ctrl Pts',(21.2790399178704,-19.2408672209645,-12.6476937472358));
#54374=CARTESIAN_POINT('Ctrl Pts',(21.2668170738604,-19.3240721305894,-12.6518634615562));
#54375=CARTESIAN_POINT('Ctrl Pts',(21.2545946647916,-19.4072740794265,-12.6560330275002));
#54376=CARTESIAN_POINT('Ctrl Pts',(21.2382680194079,-19.4898746390487,-12.6602025934442));
#54377=CARTESIAN_POINT('Ctrl Pts',(21.2179260255778,-19.5714445087795,-12.6643721593883));
#54378=CARTESIAN_POINT('Ctrl Pts',(21.1968688323393,-19.6558822745029,-12.6686883221272));
#54379=CARTESIAN_POINT('Ctrl Pts',(21.1715088054102,-19.7392150119469,-12.6730044848661));
#54380=CARTESIAN_POINT('Ctrl Pts',(21.1420010732758,-19.8209826414278,-12.6773206476051));
#54381=CARTESIAN_POINT('Ctrl Pts',(21.113454552412,-19.9000866989788,-12.6814962117967));
#54382=CARTESIAN_POINT('Ctrl Pts',(21.0810266246877,-19.9777256330122,-12.6856717759884));
#54383=CARTESIAN_POINT('Ctrl Pts',(21.0449064462655,-20.0535041518799,-12.6898473401801));
#54384=CARTESIAN_POINT('Ctrl Pts',(21.0069619234988,-20.1331100635892,-12.6942338021926));
#54385=CARTESIAN_POINT('Ctrl Pts',(20.9649426346355,-20.2106621684913,-12.6986202642052));
#54386=CARTESIAN_POINT('Ctrl Pts',(20.9191207015645,-20.2857344261862,-12.7030067262177));
#54387=CARTESIAN_POINT('Ctrl Pts',(20.8732987684935,-20.3608066838811,-12.7073931882303));
#54388=CARTESIAN_POINT('Ctrl Pts',(20.8236745814507,-20.433398658303,-12.7117796502428));
#54389=CARTESIAN_POINT('Ctrl Pts',(20.7705691100602,-20.5031241923033,-12.7161661122553));
#54390=CARTESIAN_POINT('Ctrl Pts',(20.7199071001297,-20.5696415511261,-12.7203507466484));
#54391=CARTESIAN_POINT('Ctrl Pts',(20.6658885504363,-20.6337980416559,-12.7245353810414));
#54392=CARTESIAN_POINT('Ctrl Pts',(20.6087615512374,-20.6952352468906,-12.7287200154345));
#54393=CARTESIAN_POINT('Ctrl Pts',(20.5517158652512,-20.7565850038679,-12.7328986935184));
#54394=CARTESIAN_POINT('Ctrl Pts',(20.4915708287757,-20.8152228296984,-12.7370773716023));
#54395=CARTESIAN_POINT('Ctrl Pts',(20.4286160471336,-20.8708216313137,-12.7412560496863));
#54396=CARTESIAN_POINT('Ctrl Pts',(20.3645328462752,-20.9274170014899,-12.7455096275717));
#54397=CARTESIAN_POINT('Ctrl Pts',(20.2975384722485,-20.9808629432569,-12.7497632054571));
#54398=CARTESIAN_POINT('Ctrl Pts',(20.2279792651332,-21.0308520763518,-12.7540167833426));
#54399=CARTESIAN_POINT('Ctrl Pts',(20.1597685989815,-21.0798720725558,-12.7581878973205));
#54400=CARTESIAN_POINT('Ctrl Pts',(20.0890920516424,-21.1255678171228,-12.7623590112985));
#54401=CARTESIAN_POINT('Ctrl Pts',(20.0163097948304,-21.1676898677572,-12.7665301252764));
#54402=CARTESIAN_POINT('Ctrl Pts',(19.9435519608075,-21.2097977839308,-12.7706998395968));
#54403=CARTESIAN_POINT('Ctrl Pts',(19.8686902184419,-21.2483341575376,-12.7748695539171));
#54404=CARTESIAN_POINT('Ctrl Pts',(19.7921120632718,-21.2830939195062,-12.7790392682375));
#54405=CARTESIAN_POINT('Ctrl Pts',(19.715536633081,-21.3178524445734,-12.7832088341816));
#54406=CARTESIAN_POINT('Ctrl Pts',(19.6372453307739,-21.3488344358332,-12.7873784001256));
#54407=CARTESIAN_POINT('Ctrl Pts',(19.5576472435982,-21.3758822616029,-12.7915479660696));
#54408=CARTESIAN_POINT('Ctrl Pts',(19.4752505858723,-21.4038810555595,-12.7958641288086));
#54409=CARTESIAN_POINT('Ctrl Pts',(19.3914540397878,-21.4276637164715,-12.8001802915475));
#54410=CARTESIAN_POINT('Ctrl Pts',(19.3067284276564,-21.4471116504386,-12.8044964542864));
#54411=CARTESIAN_POINT('Ctrl Pts',(19.2247627434287,-21.4659260700022,-12.8086720184781));
#54412=CARTESIAN_POINT('Ctrl Pts',(19.1419280643015,-21.4806837970704,-12.8128475826698));
#54413=CARTESIAN_POINT('Ctrl Pts',(19.058659154638,-21.4913299181693,-12.8170231468614));
#54414=CARTESIAN_POINT('Ctrl Pts',(18.9711845303003,-21.5025137495362,-12.821409608874));
#54415=CARTESIAN_POINT('Ctrl Pts',(18.8832312388616,-21.5091596607904,-12.8257960708865));
#54416=CARTESIAN_POINT('Ctrl Pts',(18.7953048072929,-21.5112658557881,-12.830182532899));
#54417=CARTESIAN_POINT('Ctrl Pts',(18.7073783757242,-21.5133720507858,-12.8345689949116));
#54418=CARTESIAN_POINT('Ctrl Pts',(18.6194793819154,-21.5109386216197,-12.8389554569241));
#54419=CARTESIAN_POINT('Ctrl Pts',(18.5321062576875,-21.5040264334084,-12.8433419189367));
#54420=CARTESIAN_POINT('Ctrl Pts',(18.4487533004234,-21.497432285223,-12.8475265533297));
#54421=CARTESIAN_POINT('Ctrl Pts',(18.3655686284663,-21.4867379250515,-12.8517111877228));
#54422=CARTESIAN_POINT('Ctrl Pts',(18.2829879003454,-21.4719579532137,-12.8558958221158));
#54423=CARTESIAN_POINT('Ctrl Pts',(18.2005247156697,-21.4571990188365,-12.8600745001997));
#54424=CARTESIAN_POINT('Ctrl Pts',(18.1186642162802,-21.4383661042868,-12.8642531782836));
#54425=CARTESIAN_POINT('Ctrl Pts',(18.0378381935519,-21.4155256725358,-12.8684318563676));
#54426=CARTESIAN_POINT('Ctrl Pts',(17.9555634224545,-21.3922758424606,-12.872685434253));
#54427=CARTESIAN_POINT('Ctrl Pts',(17.8743610594202,-21.3648734505898,-12.8769390121385));
#54428=CARTESIAN_POINT('Ctrl Pts',(17.7946770299223,-21.3334433350144,-12.8811925900239));
#54429=CARTESIAN_POINT('Ctrl Pts',(17.7165378308269,-21.3026225535603,-12.8853637040018));
#54430=CARTESIAN_POINT('Ctrl Pts',(17.6398590665666,-21.2679290019,-12.8895348179798));
#54431=CARTESIAN_POINT('Ctrl Pts',(17.5650454327544,-21.2295305090636,-12.8937059319577));
#54432=CARTESIAN_POINT('Ctrl Pts',(17.4902569033794,-21.1911449012123,-12.8978756462781));
#54433=CARTESIAN_POINT('Ctrl Pts',(17.4173326704122,-21.1490570311436,-12.9020453605985));
#54434=CARTESIAN_POINT('Ctrl Pts',(17.3466549084742,-21.103481721284,-12.9062150749189));
#54435=CARTESIAN_POINT('Ctrl Pts',(17.2759796615541,-21.0579080331895,-12.9103846408629));
#54436=CARTESIAN_POINT('Ctrl Pts',(17.207551112884,-21.0088474020654,-12.9145542068069));
#54437=CARTESIAN_POINT('Ctrl Pts',(17.1417232369319,-20.9565584825076,-12.918723772751));
#54438=CARTESIAN_POINT('Ctrl Pts',(17.0735809340686,-20.9024311490435,-12.9230399354899));
#54439=CARTESIAN_POINT('Ctrl Pts',(17.0082259988608,-20.8448446181551,-12.9273560982288));
#54440=CARTESIAN_POINT('Ctrl Pts',(16.9460129971982,-20.7841305842685,-12.9316722609678));
#54441=CARTESIAN_POINT('Ctrl Pts',(16.8858265775212,-20.7253943036498,-12.9358478251595));
#54442=CARTESIAN_POINT('Ctrl Pts',(16.8285808237902,-20.6637315251356,-12.9400233893511));
#54443=CARTESIAN_POINT('Ctrl Pts',(16.7745572392501,-20.5994780931304,-12.9441989535428));
#54444=CARTESIAN_POINT('Ctrl Pts',(16.7178050518835,-20.5319793730225,-12.9485854155554));
#54445=CARTESIAN_POINT('Ctrl Pts',(16.6646094437671,-20.4616218795447,-12.9529718775679));
#54446=CARTESIAN_POINT('Ctrl Pts',(16.6152455573351,-20.3888297086599,-12.9573583395805));
#54447=CARTESIAN_POINT('Ctrl Pts',(16.565881670903,-20.316037537775,-12.961744801593));
#54448=CARTESIAN_POINT('Ctrl Pts',(16.5203497415207,-20.240811225245,-12.9661312636056));
#54449=CARTESIAN_POINT('Ctrl Pts',(16.4788683829465,-20.1636028184871,-12.9705177256181));
#54450=CARTESIAN_POINT('Ctrl Pts',(16.4371381237558,-20.0859311380873,-12.9749305077209));
#54451=CARTESIAN_POINT('Ctrl Pts',(16.3993648293879,-20.0059905501582,-12.9793432898236));
#54452=CARTESIAN_POINT('Ctrl Pts',(16.3657873879881,-19.9241980375972,-12.9837560719264));
#54453=CARTESIAN_POINT('Ctrl Pts',(16.3323070847553,-19.8426421474352,-12.9881560880307));
#54454=CARTESIAN_POINT('Ctrl Pts',(16.302998596953,-19.7592453620159,-12.9925561041351));
#54455=CARTESIAN_POINT('Ctrl Pts',(16.278054237255,-19.6744475139794,-12.9969561202394));
#54456=CARTESIAN_POINT('Ctrl Pts',(16.2531532512186,-19.5897971138313,-13.0013484855236));
#54457=CARTESIAN_POINT('Ctrl Pts',(16.2326014031163,-19.5037508664346,-13.0057408508078));
#54458=CARTESIAN_POINT('Ctrl Pts',(16.2165427462274,-19.4167676574675,-13.010133216092));
#54459=CARTESIAN_POINT('Ctrl Pts',(16.200521001668,-19.3299843875664,-13.0145154851125));
#54460=CARTESIAN_POINT('Ctrl Pts',(16.1889719431305,-19.2422688247292,-13.018897754133));
#54461=CARTESIAN_POINT('Ctrl Pts',(16.1819893075699,-19.1540926166946,-13.0232800231536));
#54462=CARTESIAN_POINT('Ctrl Pts',(16.176672671659,-19.0869545296414,-13.0266167186812));
#54463=CARTESIAN_POINT('Ctrl Pts',(16.1740023911013,-19.0195497546633,-13.0299534142088));
#54464=CARTESIAN_POINT('Ctrl Pts',(16.174000001606,-18.9520906788001,-13.0332901097364));
#54465=CARTESIAN_POINT('Ctrl Pts',(16.174000001606,-18.9520906780897,-13.0332901097715));
#54466=CARTESIAN_POINT('Ctrl Pts',(16.1739968821085,-18.8640218456489,-13.0376462156856));
#54467=CARTESIAN_POINT('Ctrl Pts',(16.1785426714359,-18.776035607655,-13.0420023215996));
#54468=CARTESIAN_POINT('Ctrl Pts',(16.1875860737584,-18.6886065372053,-13.0463584275137));
#54469=CARTESIAN_POINT('Ctrl Pts',(16.1966529338892,-18.6009506832622,-13.050725832792));
#54470=CARTESIAN_POINT('Ctrl Pts',(16.2102406836425,-18.5138552818865,-13.0550932380704));
#54471=CARTESIAN_POINT('Ctrl Pts',(16.2282463851318,-18.4277874271108,-13.0594606433487));
#54472=CARTESIAN_POINT('Ctrl Pts',(16.2462755658188,-18.3416073409855,-13.0638337436661));
#54473=CARTESIAN_POINT('Ctrl Pts',(16.2687340840993,-18.2564578570398,-13.0682068439834));
#54474=CARTESIAN_POINT('Ctrl Pts',(16.2954690366781,-18.1727909517206,-13.0725799443007));
#54475=CARTESIAN_POINT('Ctrl Pts',(16.3222767415772,-18.0888963683653,-13.0769649448896));
#54476=CARTESIAN_POINT('Ctrl Pts',(16.3533840099471,-18.0064928038111,-13.0813499454785));
#54477=CARTESIAN_POINT('Ctrl Pts',(16.3885892814888,-17.9260133716794,-13.0857349460673));
#54478=CARTESIAN_POINT('Ctrl Pts',(16.4205927188907,-17.8528533488879,-13.0897211414781));
#54479=CARTESIAN_POINT('Ctrl Pts',(16.4559819492917,-17.7812832866316,-13.0937073368888));
#54480=CARTESIAN_POINT('Ctrl Pts',(16.4945737975983,-17.7116088181558,-13.0976935322996));
#54481=CARTESIAN_POINT('Ctrl Pts',(16.5350868078939,-17.638465846711,-13.1018781666926));
#54482=CARTESIAN_POINT('Ctrl Pts',(16.5792624158945,-17.5671736686978,-13.1060628010856));
#54483=CARTESIAN_POINT('Ctrl Pts',(16.6269069559,-17.4981228031552,-13.1102474354787));
#54484=CARTESIAN_POINT('Ctrl Pts',(16.6744836797999,-17.4291702229729,-13.1144261135626));
#54485=CARTESIAN_POINT('Ctrl Pts',(16.7255192690589,-17.3624529938655,-13.1186047916466));
#54486=CARTESIAN_POINT('Ctrl Pts',(16.779774450421,-17.2983366420662,-13.1227834697305));
#54487=CARTESIAN_POINT('Ctrl Pts',(16.8350021169166,-17.2330710507404,-13.1270370476159));
#54488=CARTESIAN_POINT('Ctrl Pts',(16.8935656995715,-17.1705009170566,-13.1312906255014));
#54489=CARTESIAN_POINT('Ctrl Pts',(16.9551669364595,-17.110980463967,-13.1355442033868));
#54490=CARTESIAN_POINT('Ctrl Pts',(17.0155739131654,-17.0526139310053,-13.1397153173648));
#54491=CARTESIAN_POINT('Ctrl Pts',(17.0789014673906,-16.9971802202222,-13.1438864313427));
#54492=CARTESIAN_POINT('Ctrl Pts',(17.1448292745174,-16.9449782250137,-13.1480575453207));
#54493=CARTESIAN_POINT('Ctrl Pts',(17.2107349589319,-16.8927937466888,-13.152227259641));
#54494=CARTESIAN_POINT('Ctrl Pts',(17.2792388030076,-16.8438391155734,-13.1563969739614));
#54495=CARTESIAN_POINT('Ctrl Pts',(17.3499870301182,-16.7983732683683,-13.1605666882818));
#54496=CARTESIAN_POINT('Ctrl Pts',(17.4207327397034,-16.752909039033,-13.1647362542258));
#54497=CARTESIAN_POINT('Ctrl Pts',(17.4937222860638,-16.7109335947647,-13.1689058201699));
#54498=CARTESIAN_POINT('Ctrl Pts',(17.5685736694554,-16.6726620548779,-13.1730753861139));
#54499=CARTESIAN_POINT('Ctrl Pts',(17.6460567351476,-16.6330449348619,-13.1773915488529));
#54500=CARTESIAN_POINT('Ctrl Pts',(17.7255345286225,-16.5973972639687,-13.1817077115918));
#54501=CARTESIAN_POINT('Ctrl Pts',(17.8065583197874,-16.5659044592045,-13.1860238743307));
#54502=CARTESIAN_POINT('Ctrl Pts',(17.8849427694772,-16.535437529243,-13.1901994385224));
#54503=CARTESIAN_POINT('Ctrl Pts',(17.9647735800337,-16.5088590368059,-13.1943750027141));
#54504=CARTESIAN_POINT('Ctrl Pts',(18.0456284938944,-16.4862861744351,-13.1985505669058));
#54505=CARTESIAN_POINT('Ctrl Pts',(18.1305671972398,-16.4625732104478,-13.2029370289183));
#54506=CARTESIAN_POINT('Ctrl Pts',(18.2166356079047,-16.4432812873466,-13.2073234909308));
#54507=CARTESIAN_POINT('Ctrl Pts',(18.3033337697292,-16.4284852688949,-13.2117099529434));
#54508=CARTESIAN_POINT('Ctrl Pts',(18.3900319315538,-16.4136892504433,-13.2160964149559));
#54509=CARTESIAN_POINT('Ctrl Pts',(18.4773592594053,-16.4033891290646,-13.2204828769685));
#54510=CARTESIAN_POINT('Ctrl Pts',(18.5648137584887,-16.3975967398073,-13.224869338981));
#54511=CARTESIAN_POINT('Ctrl Pts',(18.6482240610121,-16.3920722105338,-13.2290529559168));
#54512=CARTESIAN_POINT('Ctrl Pts',(18.7320604262271,-16.3906271591048,-13.2332365728525));
#54513=CARTESIAN_POINT('Ctrl Pts',(18.8158899787624,-16.3933100947207,-13.2374201897883));
#54514=CARTESIAN_POINT('Ctrl Pts',(18.8996093084473,-16.3959895026926,-13.2415983059171));
#54515=CARTESIAN_POINT('Ctrl Pts',(18.9833213878534,-16.4027861079022,-13.245776422046));
#54516=CARTESIAN_POINT('Ctrl Pts',(19.0665895300201,-16.4136965893493,-13.2499545381748));
#54517=CARTESIAN_POINT('Ctrl Pts',(19.1497731758387,-16.4245959993852,-13.2541284145602));
#54518=CARTESIAN_POINT('Ctrl Pts',(19.2325133255144,-16.4396009359381,-13.2583022909457));
#54519=CARTESIAN_POINT('Ctrl Pts',(19.3143759725404,-16.4586561146729,-13.2624761673311));
#54520=CARTESIAN_POINT('Ctrl Pts',(19.396180111325,-16.4776976744371,-13.2666470605958));
#54521=CARTESIAN_POINT('Ctrl Pts',(19.4771075468216,-16.5007836209281,-13.2708179538604));
#54522=CARTESIAN_POINT('Ctrl Pts',(19.5567334109211,-16.5278074056391,-13.274988847125));
#54523=CARTESIAN_POINT('Ctrl Pts',(19.6363403165266,-16.554824756131,-13.2791587473222));
#54524=CARTESIAN_POINT('Ctrl Pts',(19.7146458288506,-16.5857779414159,-13.2833286475194));
#54525=CARTESIAN_POINT('Ctrl Pts',(19.7912403187458,-16.6205105815341,-13.2874985477165));
#54526=CARTESIAN_POINT('Ctrl Pts',(19.8678247271481,-16.655238650085,-13.2916678990646));
#54527=CARTESIAN_POINT('Ctrl Pts',(19.9426981444006,-16.6937449890619,-13.2958372504126));
#54528=CARTESIAN_POINT('Ctrl Pts',(20.0154725000699,-16.7358257668756,-13.3000066017606));
#54529=CARTESIAN_POINT('Ctrl Pts',(20.0882810786158,-16.7779263336005,-13.3041779137883));
#54530=CARTESIAN_POINT('Ctrl Pts',(20.1589882301708,-16.8236044584369,-13.308349225816));
#54531=CARTESIAN_POINT('Ctrl Pts',(20.2272328428162,-16.8726117060214,-13.3125205378436));
#54532=CARTESIAN_POINT('Ctrl Pts',(20.2496021804837,-16.8886753867558,-13.3138878177452));
#54533=CARTESIAN_POINT('Ctrl Pts',(20.2717071853379,-16.905096413494,-13.3152550976468));
#54534=CARTESIAN_POINT('Ctrl Pts',(20.293535888361,-16.9218650751947,-13.3166223775484));
#54535=CARTESIAN_POINT('',(16.1736697275687,-18.9513574892655,-12.9667098340851));
#54536=CARTESIAN_POINT('Ctrl Pts',(16.1740000808904,-18.9513564484225,-12.9667098902285));
#54537=CARTESIAN_POINT('Ctrl Pts',(16.1740088273484,-18.9165636940743,-12.9684506873211));
#54538=CARTESIAN_POINT('Ctrl Pts',(16.1747268399112,-18.881780730387,-12.9701914844137));
#54539=CARTESIAN_POINT('Ctrl Pts',(16.1761531171477,-18.8470270326105,-12.9719322815063));
#54540=CARTESIAN_POINT('Ctrl Pts',(16.1795816894971,-18.7634839708603,-12.9761169158993));
#54541=CARTESIAN_POINT('Ctrl Pts',(16.1871139062631,-18.6799535889704,-12.9803015502924));
#54542=CARTESIAN_POINT('Ctrl Pts',(16.1987516982625,-18.5968717857769,-12.9844861846854));
#54543=CARTESIAN_POINT('Ctrl Pts',(16.2103729253055,-18.5139082392468,-12.9886648627694));
#54544=CARTESIAN_POINT('Ctrl Pts',(16.2260880567288,-18.4313924548469,-12.9928435408533));
#54545=CARTESIAN_POINT('Ctrl Pts',(16.2458470513543,-18.3497584337278,-12.9970222189372));
#54546=CARTESIAN_POINT('Ctrl Pts',(16.2659602117581,-18.2666611814494,-13.0012757968227));
#54547=CARTESIAN_POINT('Ctrl Pts',(16.2902636140324,-18.1844780963255,-13.0055293747081));
#54548=CARTESIAN_POINT('Ctrl Pts',(16.3186494198465,-18.1036595170853,-13.0097829525935));
#54549=CARTESIAN_POINT('Ctrl Pts',(16.3464849114244,-18.0244077637083,-13.0139540665715));
#54550=CARTESIAN_POINT('Ctrl Pts',(16.3782457689155,-17.9464685351598,-13.0181251805494));
#54551=CARTESIAN_POINT('Ctrl Pts',(16.4137796304914,-17.8702526002262,-13.0222962945274));
#54552=CARTESIAN_POINT('Ctrl Pts',(16.4493015683369,-17.7940622402856,-13.0264660088478));
#54553=CARTESIAN_POINT('Ctrl Pts',(16.4885938016076,-17.7195944421082,-13.0306357231681));
#54554=CARTESIAN_POINT('Ctrl Pts',(16.5314561548595,-17.6472392517271,-13.0348054374885));
#54555=CARTESIAN_POINT('Ctrl Pts',(16.5743169828848,-17.5748866360543,-13.0389750034325));
#54556=CARTESIAN_POINT('Ctrl Pts',(16.6207474431035,-17.5046468740728,-13.0431445693766));
#54557=CARTESIAN_POINT('Ctrl Pts',(16.6705024900493,-17.4368834941077,-13.0473141353206));
#54558=CARTESIAN_POINT('Ctrl Pts',(16.7220068630664,-17.366737637298,-13.0516302980595));
#54559=CARTESIAN_POINT('Ctrl Pts',(16.7770736453878,-17.2992459668448,-13.0559464607985));
#54560=CARTESIAN_POINT('Ctrl Pts',(16.8353848266788,-17.234775371818,-13.0602626235374));
#54561=CARTESIAN_POINT('Ctrl Pts',(16.8917965273724,-17.1724048996433,-13.0644381877291));
#54562=CARTESIAN_POINT('Ctrl Pts',(16.9512441342268,-17.1128620023875,-13.0686137519207));
#54563=CARTESIAN_POINT('Ctrl Pts',(17.0134027193002,-17.0564407163983,-13.0727893161124));
#54564=CARTESIAN_POINT('Ctrl Pts',(17.078700786738,-16.9971697253824,-13.077175778125));
#54565=CARTESIAN_POINT('Ctrl Pts',(17.146990440611,-16.9413443477726,-13.0815622401375));
#54566=CARTESIAN_POINT('Ctrl Pts',(17.2178583236867,-16.889255610274,-13.0859487021501));
#54567=CARTESIAN_POINT('Ctrl Pts',(17.2887262067624,-16.8371668727754,-13.0903351641627));
#54568=CARTESIAN_POINT('Ctrl Pts',(17.3621717925896,-16.7888150309009,-13.0947216261752));
#54569=CARTESIAN_POINT('Ctrl Pts',(17.4377516489583,-16.7444356832877,-13.0991080881878));
#54570=CARTESIAN_POINT('Ctrl Pts',(17.5098539640989,-16.7020982952443,-13.1032927225808));
#54571=CARTESIAN_POINT('Ctrl Pts',(17.5841668423745,-16.6632182861073,-13.1074773569739));
#54572=CARTESIAN_POINT('Ctrl Pts',(17.6603248069611,-16.6280332231607,-13.1116619913669));
#54573=CARTESIAN_POINT('Ctrl Pts',(17.7363743701116,-16.5928982417961,-13.1158406694509));
#54574=CARTESIAN_POINT('Ctrl Pts',(17.8142633889644,-16.5614479512896,-13.1200193475348));
#54575=CARTESIAN_POINT('Ctrl Pts',(17.8935998508937,-16.5338751915209,-13.1241980256187));
#54576=CARTESIAN_POINT('Ctrl Pts',(17.9743583618848,-16.5058082098496,-13.1284516035042));
#54577=CARTESIAN_POINT('Ctrl Pts',(18.0566163014193,-16.4817593798135,-13.1327051813896));
#54578=CARTESIAN_POINT('Ctrl Pts',(18.1399366350505,-16.461881786255,-13.136958759275));
#54579=CARTESIAN_POINT('Ctrl Pts',(18.221641641428,-16.4423895586354,-13.141129873253));
#54580=CARTESIAN_POINT('Ctrl Pts',(18.3043677482547,-16.4269083873418,-13.145300987231));
#54581=CARTESIAN_POINT('Ctrl Pts',(18.3876870934188,-16.4155325015417,-13.1494721012089));
#54582=CARTESIAN_POINT('Ctrl Pts',(18.470978479972,-16.4041604330299,-13.1536418155293));
#54583=CARTESIAN_POINT('Ctrl Pts',(18.5548622540878,-16.39689097632,-13.1578115298496));
#54584=CARTESIAN_POINT('Ctrl Pts',(18.6389020976076,-16.3937669400618,-13.16198124417));
#54585=CARTESIAN_POINT('Ctrl Pts',(18.7229389506291,-16.3906430149703,-13.1661508101141));
#54586=CARTESIAN_POINT('Ctrl Pts',(18.8071314022655,-16.3916642332765,-13.1703203760581));
#54587=CARTESIAN_POINT('Ctrl Pts',(18.8910411442615,-16.3968213215102,-13.1744899420021));
#54588=CARTESIAN_POINT('Ctrl Pts',(18.9779010492721,-16.4021597266042,-13.1788061047411));
#54589=CARTESIAN_POINT('Ctrl Pts',(19.0644574681809,-16.4119302148937,-13.18312226748));
#54590=CARTESIAN_POINT('Ctrl Pts',(19.1502297723791,-16.4260639801085,-13.1874384302189));
#54591=CARTESIAN_POINT('Ctrl Pts',(19.2332080527898,-16.4397373394081,-13.1916139944106));
#54592=CARTESIAN_POINT('Ctrl Pts',(19.3154520685914,-16.4574939280207,-13.1957895586023));
#54593=CARTESIAN_POINT('Ctrl Pts',(19.3965387044157,-16.4792196892665,-13.1999651227939));
#54594=CARTESIAN_POINT('Ctrl Pts',(19.4817208334502,-16.5020427670648,-13.2043515848065));
#54595=CARTESIAN_POINT('Ctrl Pts',(19.5656250358877,-16.5292463408117,-13.208738046819));
#54596=CARTESIAN_POINT('Ctrl Pts',(19.6477828618953,-16.5606403697255,-13.2131245088315));
#54597=CARTESIAN_POINT('Ctrl Pts',(19.7299406879029,-16.5920343986394,-13.2175109708441));
#54598=CARTESIAN_POINT('Ctrl Pts',(19.8103516376767,-16.6276185783624,-13.2218974328566));
#54599=CARTESIAN_POINT('Ctrl Pts',(19.888577588602,-16.6671475776545,-13.2262838948691));
#54600=CARTESIAN_POINT('Ctrl Pts',(19.9631842212831,-16.704847669447,-13.2304674063032));
#54601=CARTESIAN_POINT('Ctrl Pts',(20.0360812001481,-16.7462759047423,-13.2346509177373));
#54602=CARTESIAN_POINT('Ctrl Pts',(20.1068712604678,-16.7912537163791,-13.2388344291714));
#54603=CARTESIAN_POINT('Ctrl Pts',(20.170910038113,-16.8319419721225,-13.242618957074));
#54604=CARTESIAN_POINT('Ctrl Pts',(20.2332245718103,-16.875534330629,-13.2464034849766));
#54605=CARTESIAN_POINT('Ctrl Pts',(20.293535888361,-16.9218650751948,-13.2501880128791));
#54606=CARTESIAN_POINT('Ctrl Pts',(20.2954167197789,-16.919379410122,-12.4500366865268));
#54607=CARTESIAN_POINT('Ctrl Pts',(20.3656979408681,-16.9725279852605,-12.4544341426114));
#54608=CARTESIAN_POINT('Ctrl Pts',(21.0821531496881,-17.5778644531088,-12.5012235342565));
#54609=CARTESIAN_POINT('Ctrl Pts',(21.7088251808773,-19.5120955140474,-12.590404861462));
#54610=CARTESIAN_POINT('Ctrl Pts',(19.8732647581097,-21.7565262795287,-12.7175806681434));
#54611=CARTESIAN_POINT('Ctrl Pts',(17.0319370527368,-21.4324760457865,-12.8430154491732));
#54612=CARTESIAN_POINT('Ctrl Pts',(16.1727139550341,-19.7651271422422,-12.9260582946424));
#54613=CARTESIAN_POINT('Ctrl Pts',(16.1699654914217,-18.9513691601896,-12.9667092045512));
#54614=CARTESIAN_POINT('Origin',(18.734,-18.952,1.76670989022851));
#54615=CARTESIAN_POINT('',(20.293535888361,-16.9218650751948,-11.6500725313516));
#54616=CARTESIAN_POINT('',(20.293535888361,-16.9218650751948,-11.7167617890113));
#54617=CARTESIAN_POINT('',(20.293535888361,-16.9218650751948,1.76670989022851));
#54618=CARTESIAN_POINT('',(16.1740010233873,-18.9542890482673,-12.2332901098107));
#54619=CARTESIAN_POINT('Ctrl Pts',(20.293535888361,-16.9218650751948,-11.7167617890113));
#54620=CARTESIAN_POINT('Ctrl Pts',(20.360016796482,-16.9729352581854,-11.7209383138016));
#54621=CARTESIAN_POINT('Ctrl Pts',(20.4240745379401,-17.0273421081747,-11.725114838592));
#54622=CARTESIAN_POINT('Ctrl Pts',(20.485358352181,-17.0848246139568,-11.7292913633823));
#54623=CARTESIAN_POINT('Ctrl Pts',(20.5465832917244,-17.1422518969172,-11.7334638758305));
#54624=CARTESIAN_POINT('Ctrl Pts',(20.6050392660196,-17.202748650016,-11.7376363882786));
#54625=CARTESIAN_POINT('Ctrl Pts',(20.6604085786251,-17.2660136453103,-11.7418089007268));
#54626=CARTESIAN_POINT('Ctrl Pts',(20.7157496012222,-17.3292463164316,-11.7459792813007));
#54627=CARTESIAN_POINT('Ctrl Pts',(20.7680067910422,-17.3952440759125,-11.7501496618745));
#54628=CARTESIAN_POINT('Ctrl Pts',(20.816900154276,-17.463669745212,-11.7543200424484));
#54629=CARTESIAN_POINT('Ctrl Pts',(20.8657832032303,-17.5320809798025,-11.7584895432614));
#54630=CARTESIAN_POINT('Ctrl Pts',(20.9113035680159,-17.6029187325087,-11.7626590440744));
#54631=CARTESIAN_POINT('Ctrl Pts',(20.9532231573676,-17.6758148340451,-11.7668285448873));
#54632=CARTESIAN_POINT('Ctrl Pts',(20.9951464783424,-17.7487174246902,-11.7709984168634));
#54633=CARTESIAN_POINT('Ctrl Pts',(21.0334681592267,-17.8236783285432,-11.7751682888395));
#54634=CARTESIAN_POINT('Ctrl Pts',(21.0679955424597,-17.9003038424628,-11.7793381608156));
#54635=CARTESIAN_POINT('Ctrl Pts',(21.102559332555,-17.977010152964,-11.7835124296483));
#54636=CARTESIAN_POINT('Ctrl Pts',(21.1333206472027,-18.0553841579024,-11.7876866984811));
#54637=CARTESIAN_POINT('Ctrl Pts',(21.160134794313,-18.1350116525776,-11.7918609673138));
#54638=CARTESIAN_POINT('Ctrl Pts',(21.1869637585583,-18.2146831483293,-11.796037542791));
#54639=CARTESIAN_POINT('Ctrl Pts',(21.2098410870979,-18.2956090701708,-11.8002141182683));
#54640=CARTESIAN_POINT('Ctrl Pts',(21.2286725247027,-18.3773618577806,-11.8043906937455));
#54641=CARTESIAN_POINT('Ctrl Pts',(21.2475364626071,-18.4592557387125,-11.8085744773795));
#54642=CARTESIAN_POINT('Ctrl Pts',(21.2623404828511,-18.5419788823773,-11.8127582610135));
#54643=CARTESIAN_POINT('Ctrl Pts',(21.2730418541168,-18.6250956362436,-11.8169420446475));
#54644=CARTESIAN_POINT('Ctrl Pts',(21.280709708843,-18.6846512930032,-11.8199398515935));
#54645=CARTESIAN_POINT('Ctrl Pts',(21.2862722940103,-18.7444088953349,-11.8229376585394));
#54646=CARTESIAN_POINT('Ctrl Pts',(21.2897303495758,-18.8042083214207,-11.8259354654853));
#54647=CARTESIAN_POINT('Ctrl Pts',(21.2945574443532,-18.8876822540643,-11.8301200998784));
#54648=CARTESIAN_POINT('Ctrl Pts',(21.295299648515,-18.9715482669722,-11.8343047342714));
#54649=CARTESIAN_POINT('Ctrl Pts',(21.2919120526423,-19.0553727766261,-11.8384893686645));
#54650=CARTESIAN_POINT('Ctrl Pts',(21.288529278593,-19.1390779724659,-11.8426680467484));
#54651=CARTESIAN_POINT('Ctrl Pts',(21.281028398999,-19.2227413266667,-11.8468467248323));
#54652=CARTESIAN_POINT('Ctrl Pts',(21.2694164102339,-19.3059260187056,-11.8510254029163));
#54653=CARTESIAN_POINT('Ctrl Pts',(21.2575962849155,-19.3906017365655,-11.8552789808017));
#54654=CARTESIAN_POINT('Ctrl Pts',(21.2415161896729,-19.4747809821048,-11.8595325586872));
#54655=CARTESIAN_POINT('Ctrl Pts',(21.2212390250856,-19.5580049769524,-11.8637861365726));
#54656=CARTESIAN_POINT('Ctrl Pts',(21.2013549729015,-19.6396155122616,-11.8679572505505));
#54657=CARTESIAN_POINT('Ctrl Pts',(21.1774352498111,-19.7203070376072,-11.8721283645285));
#54658=CARTESIAN_POINT('Ctrl Pts',(21.1495909652079,-19.7996557607932,-11.8762994785064));
#54659=CARTESIAN_POINT('Ctrl Pts',(21.1217560240233,-19.8789778577488,-11.8804691928268));
#54660=CARTESIAN_POINT('Ctrl Pts',(21.0899992889562,-19.9569576137028,-11.8846389071472));
#54661=CARTESIAN_POINT('Ctrl Pts',(21.0544814935982,-20.0331871428518,-11.8888086214675));
#54662=CARTESIAN_POINT('Ctrl Pts',(21.0189649621159,-20.109413959427,-11.8929781874116));
#54663=CARTESIAN_POINT('Ctrl Pts',(20.9796878315025,-20.1838902563956,-11.8971477533556));
#54664=CARTESIAN_POINT('Ctrl Pts',(20.936858101798,-20.2562301113465,-11.9013173192997));
#54665=CARTESIAN_POINT('Ctrl Pts',(20.8925225316333,-20.3311133463566,-11.9056334820386));
#54666=CARTESIAN_POINT('Ctrl Pts',(20.8443801641983,-20.4037066556453,-11.9099496447775));
#54667=CARTESIAN_POINT('Ctrl Pts',(20.7927112772807,-20.4736135766998,-11.9142658075164));
#54668=CARTESIAN_POINT('Ctrl Pts',(20.7427254989198,-20.5412432871539,-11.9184413717081));
#54669=CARTESIAN_POINT('Ctrl Pts',(20.689439760407,-20.6063586052094,-11.9226169358998));
#54670=CARTESIAN_POINT('Ctrl Pts',(20.6331484080957,-20.6686348837268,-11.9267925000914));
#54671=CARTESIAN_POINT('Ctrl Pts',(20.5740139133991,-20.7340565890242,-11.931178962104));
#54672=CARTESIAN_POINT('Ctrl Pts',(20.5115626117393,-20.796344505447,-11.9355654241165));
#54673=CARTESIAN_POINT('Ctrl Pts',(20.4461771444977,-20.8551682599969,-11.9399518861291));
#54674=CARTESIAN_POINT('Ctrl Pts',(20.3807916772561,-20.9139920145469,-11.9443383481416));
#54675=CARTESIAN_POINT('Ctrl Pts',(20.3124725431191,-20.9693513010386,-11.9487248101541));
#54676=CARTESIAN_POINT('Ctrl Pts',(20.2416377781119,-21.0209679383717,-11.9531112721667));
#54677=CARTESIAN_POINT('Ctrl Pts',(20.1740622256448,-21.0702096177069,-11.9572959065597));
#54678=CARTESIAN_POINT('Ctrl Pts',(20.1039459219093,-21.1162287760929,-11.9614805409528));
#54679=CARTESIAN_POINT('Ctrl Pts',(20.0316291334116,-21.1587529612808,-11.9656651753458));
#54680=CARTESIAN_POINT('Ctrl Pts',(19.9594152789112,-21.2012166185545,-11.9698438534297));
#54681=CARTESIAN_POINT('Ctrl Pts',(19.8850075541825,-21.2401949526838,-11.9740225315137));
#54682=CARTESIAN_POINT('Ctrl Pts',(19.8087770431608,-21.2754574038476,-11.9782012095976));
#54683=CARTESIAN_POINT('Ctrl Pts',(19.731180155015,-21.311351909106,-11.9824547874831));
#54684=CARTESIAN_POINT('Ctrl Pts',(19.6516948805992,-21.343395722762,-11.9867083653685));
#54685=CARTESIAN_POINT('Ctrl Pts',(19.5707410268107,-21.3713934062181,-11.9909619432539));
#54686=CARTESIAN_POINT('Ctrl Pts',(19.4913566214465,-21.3988482999475,-11.9951330572319));
#54687=CARTESIAN_POINT('Ctrl Pts',(19.4105605259062,-21.4224123904405,-11.9993041712098));
#54688=CARTESIAN_POINT('Ctrl Pts',(19.3287692237674,-21.4419497124358,-12.0034752851878));
#54689=CARTESIAN_POINT('Ctrl Pts',(19.24700536749,-21.461480478494,-12.0076449995082));
#54690=CARTESIAN_POINT('Ctrl Pts',(19.1642474149188,-21.4769870528098,-12.0118147138285));
#54691=CARTESIAN_POINT('Ctrl Pts',(19.0809253355101,-21.4883838060477,-12.0159844281489));
#54692=CARTESIAN_POINT('Ctrl Pts',(18.9976062210585,-21.4997801537403,-12.0201539940929));
#54693=CARTESIAN_POINT('Ctrl Pts',(18.9137234755862,-21.5070669096296,-12.024323560037));
#54694=CARTESIAN_POINT('Ctrl Pts',(18.8297141852437,-21.5102100763509,-12.028493125981));
#54695=CARTESIAN_POINT('Ctrl Pts',(18.7427512318894,-21.5134637529366,-12.0328092887199));
#54696=CARTESIAN_POINT('Ctrl Pts',(18.6556531965172,-21.5122770220956,-12.0371254514589));
#54697=CARTESIAN_POINT('Ctrl Pts',(18.5689051504098,-21.5066709554537,-12.0414416141978));
#54698=CARTESIAN_POINT('Ctrl Pts',(18.4849829127802,-21.501247505843,-12.0456171783895));
#54699=CARTESIAN_POINT('Ctrl Pts',(18.4013886754049,-21.4916883190585,-12.0497927425811));
#54700=CARTESIAN_POINT('Ctrl Pts',(18.3185547392503,-21.4780651684627,-12.0539683067728));
#54701=CARTESIAN_POINT('Ctrl Pts',(18.2315370578994,-21.4637539449163,-12.0583547687854));
#54702=CARTESIAN_POINT('Ctrl Pts',(18.1453590723583,-21.444957551129,-12.0627412307979));
#54703=CARTESIAN_POINT('Ctrl Pts',(18.0605056905581,-21.4218189033104,-12.0671276928105));
#54704=CARTESIAN_POINT('Ctrl Pts',(17.9756523087579,-21.3986802554919,-12.071514154823));
#54705=CARTESIAN_POINT('Ctrl Pts',(17.8921240580818,-21.371199607226,-12.0759006168356));
#54706=CARTESIAN_POINT('Ctrl Pts',(17.8103811197836,-21.3395778865008,-12.0802870788481));
#54707=CARTESIAN_POINT('Ctrl Pts',(17.7323992952486,-21.3094111280208,-12.0844717132412));
#54708=CARTESIAN_POINT('Ctrl Pts',(17.6557518403844,-21.2753637103368,-12.0886563476342));
#54709=CARTESIAN_POINT('Ctrl Pts',(17.5808520242221,-21.2375742704973,-12.0928409820273));
#54710=CARTESIAN_POINT('Ctrl Pts',(17.5060588186775,-21.1998386192481,-12.0970196601112));
#54711=CARTESIAN_POINT('Ctrl Pts',(17.4330087179883,-21.1583717310105,-12.1011983381951));
#54712=CARTESIAN_POINT('Ctrl Pts',(17.3620964471735,-21.113360830991,-12.1053770162791));
#54713=CARTESIAN_POINT('Ctrl Pts',(17.289913124868,-21.0675431429373,-12.1096305941645));
#54714=CARTESIAN_POINT('Ctrl Pts',(17.2199454771429,-21.018053314544,-12.11388417205));
#54715=CARTESIAN_POINT('Ctrl Pts',(17.1525850704414,-20.9651385497698,-12.1181377499354));
#54716=CARTESIAN_POINT('Ctrl Pts',(17.0865305766668,-20.9132496409654,-12.1223088639133));
#54717=CARTESIAN_POINT('Ctrl Pts',(17.0229835115634,-20.8580677061308,-12.1264799778913));
#54718=CARTESIAN_POINT('Ctrl Pts',(16.9622836350606,-20.7998693466276,-12.1306510918693));
#54719=CARTESIAN_POINT('Ctrl Pts',(16.9016041269875,-20.741690516146,-12.1348208061896));
#54720=CARTESIAN_POINT('Ctrl Pts',(16.8437702418585,-20.6804975893352,-12.13899052051));
#54721=CARTESIAN_POINT('Ctrl Pts',(16.7890867147049,-20.6166057529284,-12.1431602348304));
#54722=CARTESIAN_POINT('Ctrl Pts',(16.7344051334259,-20.5527161900675,-12.1473298007744));
#54723=CARTESIAN_POINT('Ctrl Pts',(16.682873985715,-20.4861282586161,-12.1514993667185));
#54724=CARTESIAN_POINT('Ctrl Pts',(16.6347584444192,-20.4171910767278,-12.1556689326625));
#54725=CARTESIAN_POINT('Ctrl Pts',(16.5849512200484,-20.3458301485675,-12.1599850954014));
#54726=CARTESIAN_POINT('Ctrl Pts',(16.5388045582795,-20.2719521294865,-12.1643012581404));
#54727=CARTESIAN_POINT('Ctrl Pts',(16.496563301095,-20.1959762933404,-12.1686174208793));
#54728=CARTESIAN_POINT('Ctrl Pts',(16.4556980484202,-20.1224753620654,-12.172792985071));
#54729=CARTESIAN_POINT('Ctrl Pts',(16.4184878365308,-20.0470116310055,-12.1769685492626));
#54730=CARTESIAN_POINT('Ctrl Pts',(16.3851063117009,-19.9699874464201,-12.1811441134543));
#54731=CARTESIAN_POINT('Ctrl Pts',(16.350038765409,-19.8890729533789,-12.1855305754669));
#54732=CARTESIAN_POINT('Ctrl Pts',(16.3191970489118,-19.8064367740456,-12.1899170374794));
#54733=CARTESIAN_POINT('Ctrl Pts',(16.2927234637601,-19.7225639970856,-12.1943034994919));
#54734=CARTESIAN_POINT('Ctrl Pts',(16.2662498786084,-19.6386912201256,-12.1986899615045));
#54735=CARTESIAN_POINT('Ctrl Pts',(16.2441444970407,-19.5535824262448,-12.203076423517));
#54736=CARTESIAN_POINT('Ctrl Pts',(16.2264874578015,-19.4677333135615,-12.2074628855296));
#54737=CARTESIAN_POINT('Ctrl Pts',(16.2025156137684,-19.3511814097151,-12.2134181072288));
#54738=CARTESIAN_POINT('Ctrl Pts',(16.1866633864905,-19.2329068373031,-12.219373328928));
#54739=CARTESIAN_POINT('Ctrl Pts',(16.1791211349008,-19.1138455580776,-12.2253285506272));
#54740=CARTESIAN_POINT('Ctrl Pts',(16.1757600463668,-19.060787728371,-12.2279824036753));
#54741=CARTESIAN_POINT('Ctrl Pts',(16.1740486686438,-19.0075739736056,-12.2306362567234));
#54742=CARTESIAN_POINT('Ctrl Pts',(16.174001023388,-18.9542890490546,-12.2332901097715));
#54743=CARTESIAN_POINT('Ctrl Pts',(16.1740010233873,-18.9542890482673,-12.2332901098107));
#54744=CARTESIAN_POINT('Ctrl Pts',(16.1739252094451,-18.869501140071,-12.2375129674107));
#54745=CARTESIAN_POINT('Ctrl Pts',(16.1780663695147,-18.7845778436852,-12.2417358250107));
#54746=CARTESIAN_POINT('Ctrl Pts',(16.1864353355331,-18.6999796032861,-12.2459586826108));
#54747=CARTESIAN_POINT('Ctrl Pts',(16.1945865434513,-18.6175825848873,-12.2500716626647));
#54748=CARTESIAN_POINT('Ctrl Pts',(16.2067481850333,-18.5354944186516,-12.2541846427187));
#54749=CARTESIAN_POINT('Ctrl Pts',(16.2228775801224,-18.4541403888766,-12.2582976227727));
#54750=CARTESIAN_POINT('Ctrl Pts',(16.2389992540557,-18.3728253033474,-12.2624086339395));
#54751=CARTESIAN_POINT('Ctrl Pts',(16.2590848209399,-18.2922441216164,-12.2665196451063));
#54752=CARTESIAN_POINT('Ctrl Pts',(16.2830401055299,-18.2128142346481,-12.2706306562731));
#54753=CARTESIAN_POINT('Ctrl Pts',(16.3069915898917,-18.13339694831,-12.2747410152756));
#54754=CARTESIAN_POINT('Ctrl Pts',(16.3348114354692,-18.0551310480635,-12.2788513742782));
#54755=CARTESIAN_POINT('Ctrl Pts',(16.3663553936721,-17.9784194855451,-12.2829617332808));
#54756=CARTESIAN_POINT('Ctrl Pts',(16.3994039228382,-17.8980489659369,-12.2872681465249));
#54757=CARTESIAN_POINT('Ctrl Pts',(16.4365404963283,-17.8193852938553,-12.2915745597691));
#54758=CARTESIAN_POINT('Ctrl Pts',(16.4775431085385,-17.74286713014,-12.2958809730133));
#54759=CARTESIAN_POINT('Ctrl Pts',(16.5167281737212,-17.6697408322964,-12.2999964933322));
#54760=CARTESIAN_POINT('Ctrl Pts',(16.5594435017452,-17.5985742591835,-12.304112013651));
#54761=CARTESIAN_POINT('Ctrl Pts',(16.6054498638679,-17.5297221375653,-12.3082275339699));
#54762=CARTESIAN_POINT('Ctrl Pts',(16.6514869443888,-17.46082404346,-12.3123458022172));
#54763=CARTESIAN_POINT('Ctrl Pts',(16.7008191449124,-17.394243852655,-12.3164640704645));
#54764=CARTESIAN_POINT('Ctrl Pts',(16.7531665958489,-17.3303036582026,-12.3205823387118));
#54765=CARTESIAN_POINT('Ctrl Pts',(16.8055945346489,-17.2662651512335,-12.3247069390843));
#54766=CARTESIAN_POINT('Ctrl Pts',(16.8610466479906,-17.204875081261,-12.3288315394568));
#54767=CARTESIAN_POINT('Ctrl Pts',(16.9192065009782,-17.1464184992341,-12.3329561398293));
#54768=CARTESIAN_POINT('Ctrl Pts',(16.9271149034353,-17.1384697484517,-12.3335169906232));
#54769=CARTESIAN_POINT('Ctrl Pts',(16.9350733229401,-17.1305751748483,-12.3340778414171));
#54770=CARTESIAN_POINT('Ctrl Pts',(16.9430809195059,-17.122735435449,-12.334638692211));
#54771=CARTESIAN_POINT('Ctrl Pts',(17.0028274053095,-17.0642413698601,-12.338823326604));
#54772=CARTESIAN_POINT('Ctrl Pts',(17.0655538444185,-17.0085686402268,-12.3430079609971));
#54773=CARTESIAN_POINT('Ctrl Pts',(17.1309629349575,-16.9560360303603,-12.3471925953901));
#54774=CARTESIAN_POINT('Ctrl Pts',(17.1962789237522,-16.9035781941616,-12.3513712734741));
#54775=CARTESIAN_POINT('Ctrl Pts',(17.2642696237812,-16.854251885356,-12.355549951558));
#54776=CARTESIAN_POINT('Ctrl Pts',(17.3346011829202,-16.8083388908795,-12.359728629642));
#54777=CARTESIAN_POINT('Ctrl Pts',(17.4061933847103,-16.7616029389742,-12.3639822075274));
#54778=CARTESIAN_POINT('Ctrl Pts',(17.480210846325,-16.7184042096098,-12.3682357854128));
#54779=CARTESIAN_POINT('Ctrl Pts',(17.556266426922,-16.6789967816026,-12.3724893632983));
#54780=CARTESIAN_POINT('Ctrl Pts',(17.630847521679,-16.6403533434846,-12.3766604772762));
#54781=CARTESIAN_POINT('Ctrl Pts',(17.7073879875337,-16.6053557363937,-12.3808315912542));
#54782=CARTESIAN_POINT('Ctrl Pts',(17.7854953736993,-16.5741987101765,-12.3850027052321));
#54783=CARTESIAN_POINT('Ctrl Pts',(17.8635765501771,-16.5430521390004,-12.3891724195525));
#54784=CARTESIAN_POINT('Ctrl Pts',(17.943223175792,-16.5157437595366,-12.3933421338729));
#54785=CARTESIAN_POINT('Ctrl Pts',(18.0240221782539,-16.4924204642605,-12.3975118481933));
#54786=CARTESIAN_POINT('Ctrl Pts',(18.1048183055405,-16.4690979989273,-12.4016814141373));
#54787=CARTESIAN_POINT('Ctrl Pts',(18.186766285919,-16.4497604625988,-12.4058509800813));
#54788=CARTESIAN_POINT('Ctrl Pts',(18.2694385404887,-16.4345046871272,-12.4100205460254));
#54789=CARTESIAN_POINT('Ctrl Pts',(18.3550174495419,-16.41871253741,-12.4143367087643));
#54790=CARTESIAN_POINT('Ctrl Pts',(18.4413719926993,-16.407294614139,-12.4186528715032));
#54791=CARTESIAN_POINT('Ctrl Pts',(18.5280191484753,-16.4003001961819,-12.4229690342421));
#54792=CARTESIAN_POINT('Ctrl Pts',(18.6118437822656,-16.3935336206541,-12.4271445984338));
#54793=CARTESIAN_POINT('Ctrl Pts',(18.6959417854338,-16.3909067522804,-12.4313201626255));
#54794=CARTESIAN_POINT('Ctrl Pts',(18.7798750222018,-16.3924110716097,-12.4354957268172));
#54795=CARTESIAN_POINT('Ctrl Pts',(18.8680475272268,-16.3939913705323,-12.4398821888297));
#54796=CARTESIAN_POINT('Ctrl Pts',(18.9560376012528,-16.4001311167978,-12.4442686508423));
#54797=CARTESIAN_POINT('Ctrl Pts',(19.0433447687657,-16.4107590011891,-12.4486551128548));
#54798=CARTESIAN_POINT('Ctrl Pts',(19.1306519362786,-16.4213868855805,-12.4530415748673));
#54799=CARTESIAN_POINT('Ctrl Pts',(19.2172756387744,-16.4365027334242,-12.4574280368799));
#54800=CARTESIAN_POINT('Ctrl Pts',(19.3027314805895,-16.4559742583486,-12.4618144988924));
#54801=CARTESIAN_POINT('Ctrl Pts',(19.3842631981423,-16.4745516526699,-12.4659995349797));
#54802=CARTESIAN_POINT('Ctrl Pts',(19.4650354649563,-16.4971626268787,-12.4701845710669));
#54803=CARTESIAN_POINT('Ctrl Pts',(19.5446191872091,-16.5237297239952,-12.4743696071542));
#54804=CARTESIAN_POINT('Ctrl Pts',(19.6240693838797,-16.5502522468318,-12.4785476215872));
#54805=CARTESIAN_POINT('Ctrl Pts',(19.7023345681444,-16.5807175510206,-12.4827256360202));
#54806=CARTESIAN_POINT('Ctrl Pts',(19.7789972930805,-16.6149975058947,-12.4869036504532));
#54807=CARTESIAN_POINT('Ctrl Pts',(19.8555857432772,-16.6492442486084,-12.4910776170138));
#54808=CARTESIAN_POINT('Ctrl Pts',(19.9305743987682,-16.6872981181988,-12.4952515835743));
#54809=CARTESIAN_POINT('Ctrl Pts',(20.0035631940899,-16.7289819397467,-12.4994255501349));
#54810=CARTESIAN_POINT('Ctrl Pts',(20.0764986900048,-16.7706353220615,-12.5035964686941));
#54811=CARTESIAN_POINT('Ctrl Pts',(20.1474368294329,-16.8159131614313,-12.5077673872534));
#54812=CARTESIAN_POINT('Ctrl Pts',(20.2160009920398,-16.8645917841512,-12.5119383058127));
#54813=CARTESIAN_POINT('Ctrl Pts',(20.2421989296968,-16.8831915814033,-12.5135319877047));
#54814=CARTESIAN_POINT('Ctrl Pts',(20.2680505442949,-16.9022874066306,-12.5151256695967));
#54815=CARTESIAN_POINT('Ctrl Pts',(20.293535888361,-16.9218650751948,-12.5167193514888));
#54816=CARTESIAN_POINT('',(16.1740007840082,-18.949996472737,-12.1667098902285));
#54817=CARTESIAN_POINT('Ctrl Pts',(16.1763510013672,-18.9499800105097,-12.1667107986216));
#54818=CARTESIAN_POINT('Ctrl Pts',(16.1742902547169,-18.6667985525942,-12.1807663462203));
#54819=CARTESIAN_POINT('Ctrl Pts',(16.3483939296849,-17.5319993745477,-12.2372138293795));
#54820=CARTESIAN_POINT('Ctrl Pts',(17.9381456496072,-16.0798453637573,-12.3316557920145));
#54821=CARTESIAN_POINT('Ctrl Pts',(19.6881796352386,-16.4601701745045,-12.4120422070509));
#54822=CARTESIAN_POINT('Ctrl Pts',(20.2954167197789,-16.919379410122,-12.4500366865268));
#54823=CARTESIAN_POINT('Ctrl Pts',(20.293535888361,-16.9218650751948,-11.6500725313516));
#54824=CARTESIAN_POINT('Ctrl Pts',(20.3602862242945,-16.9731422308047,-11.65424767163));
#54825=CARTESIAN_POINT('Ctrl Pts',(20.4244786682837,-17.0276947507719,-11.6584228119083));
#54826=CARTESIAN_POINT('Ctrl Pts',(20.4857877623676,-17.0852274815556,-11.6625979521867));
#54827=CARTESIAN_POINT('Ctrl Pts',(20.5471067980569,-17.1427695415867,-11.6667737694869));
#54828=CARTESIAN_POINT('Ctrl Pts',(20.6055412419491,-17.2032924338565,-11.6709495867872));
#54829=CARTESIAN_POINT('Ctrl Pts',(20.6608038266511,-17.2664653626809,-11.6751254040874));
#54830=CARTESIAN_POINT('Ctrl Pts',(20.716166721374,-17.3297529600073,-11.679308801133));
#54831=CARTESIAN_POINT('Ctrl Pts',(20.7683459651374,-17.3956998448477,-11.6834921981786));
#54832=CARTESIAN_POINT('Ctrl Pts',(20.8170955367815,-17.4639432186099,-11.6876755952242));
#54833=CARTESIAN_POINT('Ctrl Pts',(20.8656447850406,-17.5319061643976,-11.6918418017134));
#54834=CARTESIAN_POINT('Ctrl Pts',(20.9107923290493,-17.6021463354618,-11.6960080082027));
#54835=CARTESIAN_POINT('Ctrl Pts',(20.9523407266399,-17.6742815566288,-11.700174214692));
#54836=CARTESIAN_POINT('Ctrl Pts',(20.9940729004966,-17.7467358452539,-11.704358849085));
#54837=CARTESIAN_POINT('Ctrl Pts',(21.0323293070735,-17.8213716700562,-11.7085434834781));
#54838=CARTESIAN_POINT('Ctrl Pts',(21.0668754476401,-17.8978215778161,-11.7127281178711));
#54839=CARTESIAN_POINT('Ctrl Pts',(21.1013724160515,-17.9741626685949,-11.7169067959551));
#54840=CARTESIAN_POINT('Ctrl Pts',(21.1321694205718,-18.0523122977904,-11.721085474039));
#54841=CARTESIAN_POINT('Ctrl Pts',(21.1590769104972,-18.1318768518244,-11.725264152123));
#54842=CARTESIAN_POINT('Ctrl Pts',(21.1864666978414,-18.2128675433073,-11.7295177300084));
#54843=CARTESIAN_POINT('Ctrl Pts',(21.2098259193362,-18.2953239658209,-11.7337713078938));
#54844=CARTESIAN_POINT('Ctrl Pts',(21.2290051549003,-18.3788078184229,-11.7380248857793));
#54845=CARTESIAN_POINT('Ctrl Pts',(21.2478125635577,-18.4606731736369,-11.7421959997572));
#54846=CARTESIAN_POINT('Ctrl Pts',(21.2626005065823,-18.5435260079664,-11.7463671137352));
#54847=CARTESIAN_POINT('Ctrl Pts',(21.2732783407021,-18.6269376852954,-11.7505382277131));
#54848=CARTESIAN_POINT('Ctrl Pts',(21.2839525917715,-18.7103213730303,-11.7547079420335));
#54849=CARTESIAN_POINT('Ctrl Pts',(21.2905194146576,-18.7942630754073,-11.7588776563539));
#54850=CARTESIAN_POINT('Ctrl Pts',(21.2929396556081,-18.8783261311161,-11.7630473706742));
#54851=CARTESIAN_POINT('Ctrl Pts',(21.295359810436,-18.9623861955009,-11.7672169366183));
#54852=CARTESIAN_POINT('Ctrl Pts',(21.2936336643145,-19.0465671447647,-11.7713865025623));
#54853=CARTESIAN_POINT('Ctrl Pts',(21.2877741604491,-19.1304307636668,-11.7755560685064));
#54854=CARTESIAN_POINT('Ctrl Pts',(21.2817086436562,-19.2172429239524,-11.7798722312453));
#54855=CARTESIAN_POINT('Ctrl Pts',(21.2712137402018,-19.3037144978784,-11.7841883939842));
#54856=CARTESIAN_POINT('Ctrl Pts',(21.2563622783627,-19.3893654498163,-11.7885045567231));
#54857=CARTESIAN_POINT('Ctrl Pts',(21.2419946013309,-19.4722263310037,-11.7926801209148));
#54858=CARTESIAN_POINT('Ctrl Pts',(21.2235499863025,-19.554318783463,-11.7968556851065));
#54859=CARTESIAN_POINT('Ctrl Pts',(21.2011460288053,-19.6352206616827,-11.8010312492982));
#54860=CARTESIAN_POINT('Ctrl Pts',(21.1776105006753,-19.7202087014454,-11.8054177113107));
#54861=CARTESIAN_POINT('Ctrl Pts',(21.1497053305465,-19.8038821804658,-11.8098041733232));
#54862=CARTESIAN_POINT('Ctrl Pts',(21.1176244749812,-19.8857742565903,-11.8141906353358));
#54863=CARTESIAN_POINT('Ctrl Pts',(21.0855436194159,-19.9676663327147,-11.8185770973483));
#54864=CARTESIAN_POINT('Ctrl Pts',(21.0492873869464,-20.0477765087051,-11.8229635593609));
#54865=CARTESIAN_POINT('Ctrl Pts',(21.0091047687183,-20.1256687315232,-11.8273500213734));
#54866=CARTESIAN_POINT('Ctrl Pts',(20.9707710123197,-20.1999770177056,-11.8315346557664));
#54867=CARTESIAN_POINT('Ctrl Pts',(20.9287215623263,-20.2725435578142,-11.8357192901595));
#54868=CARTESIAN_POINT('Ctrl Pts',(20.8831384590297,-20.3429722800686,-11.8399039245525));
#54869=CARTESIAN_POINT('Ctrl Pts',(20.8376202376386,-20.4133007557544,-11.8440826026365));
#54870=CARTESIAN_POINT('Ctrl Pts',(20.7885786013675,-20.481497074883,-11.8482612807204));
#54871=CARTESIAN_POINT('Ctrl Pts',(20.7362419167442,-20.5471887997452,-11.8524399588044));
#54872=CARTESIAN_POINT('Ctrl Pts',(20.6829671346629,-20.6140580015636,-11.8566935366898));
#54873=CARTESIAN_POINT('Ctrl Pts',(20.6262782358932,-20.6783315077606,-11.8609471145753));
#54874=CARTESIAN_POINT('Ctrl Pts',(20.5664628839088,-20.7396464357072,-11.8652006924607));
#54875=CARTESIAN_POINT('Ctrl Pts',(20.5078071692427,-20.7997726541292,-11.8693718064387));
#54876=CARTESIAN_POINT('Ctrl Pts',(20.4461454804006,-20.8570536417645,-11.8735429204166));
#54877=CARTESIAN_POINT('Ctrl Pts',(20.3817891690389,-20.9111811693659,-11.8777140343946));
#54878=CARTESIAN_POINT('Ctrl Pts',(20.317454453059,-20.9652905339527,-11.8818837487149));
#54879=CARTESIAN_POINT('Ctrl Pts',(20.2504272621008,-21.0162482441942,-11.8860534630353));
#54880=CARTESIAN_POINT('Ctrl Pts',(20.1810535660396,-21.0637850214954,-11.8902231773557));
#54881=CARTESIAN_POINT('Ctrl Pts',(20.1116823385923,-21.1113201072339,-11.8943927432997));
#54882=CARTESIAN_POINT('Ctrl Pts',(20.0399651520291,-21.1554342427326,-11.8985623092438));
#54883=CARTESIAN_POINT('Ctrl Pts',(19.9662774819301,-21.1959011135806,-11.9027318751878));
#54884=CARTESIAN_POINT('Ctrl Pts',(19.8899990442537,-21.2377907496864,-11.9070480379267));
#54885=CARTESIAN_POINT('Ctrl Pts',(19.811609442817,-21.2757716196387,-11.9113642006656));
#54886=CARTESIAN_POINT('Ctrl Pts',(19.7315517321809,-21.309645126312,-11.9156803634045));
#54887=CARTESIAN_POINT('Ctrl Pts',(19.6541018930483,-21.3424152070683,-11.9198559275962));
#54888=CARTESIAN_POINT('Ctrl Pts',(19.5750914116572,-21.3713412922627,-11.9240314917879));
#54889=CARTESIAN_POINT('Ctrl Pts',(19.4949388978056,-21.3962937617656,-11.9282070559796));
#54890=CARTESIAN_POINT('Ctrl Pts',(19.4107380710239,-21.4225065211842,-11.9325935179921));
#54891=CARTESIAN_POINT('Ctrl Pts',(19.3252773774555,-21.4443335563955,-11.9369799800047));
#54892=CARTESIAN_POINT('Ctrl Pts',(19.239054342481,-21.4616852613707,-11.9413664420172));
#54893=CARTESIAN_POINT('Ctrl Pts',(19.1528313075064,-21.4790369663458,-11.9457529040297));
#54894=CARTESIAN_POINT('Ctrl Pts',(19.0658465162267,-21.4919133313661,-11.9501393660423));
#54895=CARTESIAN_POINT('Ctrl Pts',(18.9786013944249,-21.5002876913421,-11.9545258280548));
#54896=CARTESIAN_POINT('Ctrl Pts',(18.8953705500055,-21.5082767346017,-11.9587104624479));
#54897=CARTESIAN_POINT('Ctrl Pts',(18.8115930039276,-21.5121986934545,-11.9628950968409));
#54898=CARTESIAN_POINT('Ctrl Pts',(18.7277003248363,-21.5119922488345,-11.967079731234));
#54899=CARTESIAN_POINT('Ctrl Pts',(18.6439270565898,-21.5117860980629,-11.9712584093179));
#54900=CARTESIAN_POINT('Ctrl Pts',(18.560039436939,-21.507463217065,-11.9754370874018));
#54901=CARTESIAN_POINT('Ctrl Pts',(18.4764742375282,-21.4990140324826,-11.9796157654858));
#54902=CARTESIAN_POINT('Ctrl Pts',(18.391411191975,-21.4904134023389,-11.9838693433712));
#54903=CARTESIAN_POINT('Ctrl Pts',(18.3066827190521,-21.4775370395473,-11.9881229212567));
#54904=CARTESIAN_POINT('Ctrl Pts',(18.2227496524054,-21.460430402081,-11.9923764991421));
#54905=CARTESIAN_POINT('Ctrl Pts',(18.1404437920376,-21.4436554101629,-11.99654761312));
#54906=CARTESIAN_POINT('Ctrl Pts',(18.0589032436853,-21.4228128002076,-12.000718727098));
#54907=CARTESIAN_POINT('Ctrl Pts',(17.9785557081133,-21.3979975310404,-12.004889841076));
#54908=CARTESIAN_POINT('Ctrl Pts',(17.898235133933,-21.3731905888765,-12.0090595553963));
#54909=CARTESIAN_POINT('Ctrl Pts',(17.819107216658,-21.3444137706279,-12.0132292697167));
#54910=CARTESIAN_POINT('Ctrl Pts',(17.7415856439041,-21.3118122268127,-12.0173989840371));
#54911=CARTESIAN_POINT('Ctrl Pts',(17.6640668297004,-21.2792118431003,-12.0215685499811));
#54912=CARTESIAN_POINT('Ctrl Pts',(17.5881546700965,-21.2427871835461,-12.0257381159252));
#54913=CARTESIAN_POINT('Ctrl Pts',(17.5142426975068,-21.2027314639944,-12.0299076818692));
#54914=CARTESIAN_POINT('Ctrl Pts',(17.4377320711412,-21.1612674347574,-12.0342238446081));
#54915=CARTESIAN_POINT('Ctrl Pts',(17.3633653656329,-21.1159125099135,-12.0385400073471));
#54916=CARTESIAN_POINT('Ctrl Pts',(17.2915493867665,-21.0669317313763,-12.042856170086));
#54917=CARTESIAN_POINT('Ctrl Pts',(17.222072805858,-21.0195464965481,-12.0470317342777));
#54918=CARTESIAN_POINT('Ctrl Pts',(17.1549836708369,-20.968768326667,-12.0512072984694));
#54919=CARTESIAN_POINT('Ctrl Pts',(17.0906175572636,-20.914879045409,-12.055382862661));
#54920=CARTESIAN_POINT('Ctrl Pts',(17.0230004643097,-20.8582679446643,-12.0597693246736));
#54921=CARTESIAN_POINT('Ctrl Pts',(16.9583891293619,-20.7982235859986,-12.0641557866861));
#54922=CARTESIAN_POINT('Ctrl Pts',(16.8971281979621,-20.735115807478,-12.0685422486987));
#54923=CARTESIAN_POINT('Ctrl Pts',(16.8358672665623,-20.6720080289574,-12.0729287107112));
#54924=CARTESIAN_POINT('Ctrl Pts',(16.7779570635865,-20.6058373172987,-12.0773151727238));
#54925=CARTESIAN_POINT('Ctrl Pts',(16.7236914224212,-20.5370108589259,-12.0817016347363));
#54926=CARTESIAN_POINT('Ctrl Pts',(16.6719732357611,-20.4714154002739,-12.0858821780095));
#54927=CARTESIAN_POINT('Ctrl Pts',(16.62336875941,-20.403158891998,-12.0900627212828));
#54928=CARTESIAN_POINT('Ctrl Pts',(16.5781640651477,-20.3325692383938,-12.094243264556));
#54929=CARTESIAN_POINT('Ctrl Pts',(16.5330221281564,-20.2620775837719,-12.0984180040186));
#54930=CARTESIAN_POINT('Ctrl Pts',(16.4912708487477,-20.1892595981085,-12.1025927434812));
#54931=CARTESIAN_POINT('Ctrl Pts',(16.4531558825332,-20.1144758542942,-12.1067674829437));
#54932=CARTESIAN_POINT('Ctrl Pts',(16.4150823671081,-20.0397734392997,-12.1109376822935));
#54933=CARTESIAN_POINT('Ctrl Pts',(16.380637519025,-19.9631099194743,-12.1151078816432));
#54934=CARTESIAN_POINT('Ctrl Pts',(16.3500227648594,-19.8848732723855,-12.119278080993));
#54935=CARTESIAN_POINT('Ctrl Pts',(16.319430601241,-19.8066943559144,-12.1234452031635));
#54936=CARTESIAN_POINT('Ctrl Pts',(16.2926630858425,-19.7269450449961,-12.1276123253341));
#54937=CARTESIAN_POINT('Ctrl Pts',(16.2698743296479,-19.6460350716728,-12.1317794475046));
#54938=CARTESIAN_POINT('Ctrl Pts',(16.2470959536797,-19.5651619526576,-12.1359446715605));
#54939=CARTESIAN_POINT('Ctrl Pts',(16.2282928589745,-19.4831296648129,-12.1401098956164));
#54940=CARTESIAN_POINT('Ctrl Pts',(16.2135694674,-19.4003636139762,-12.1442751196724));
#54941=CARTESIAN_POINT('Ctrl Pts',(16.1988435352848,-19.3175832817472,-12.1484410624432));
#54942=CARTESIAN_POINT('Ctrl Pts',(16.1881988016354,-19.2340693856754,-12.1526070052141));
#54943=CARTESIAN_POINT('Ctrl Pts',(16.1816884763611,-19.1502571216887,-12.156772947985));
#54944=CARTESIAN_POINT('Ctrl Pts',(16.1765121589547,-19.0836185341113,-12.1600852620661));
#54945=CARTESIAN_POINT('Ctrl Pts',(16.1739485082683,-19.0167915973248,-12.1633975761473));
#54946=CARTESIAN_POINT('Ctrl Pts',(16.1740007840082,-18.949996472737,-12.1667098902285));
#54947=CARTESIAN_POINT('Origin',(18.734,-18.952,1.76670989022851));
#54948=CARTESIAN_POINT('',(20.2922820154253,-16.9234654489967,-10.8502164909775));
#54949=CARTESIAN_POINT('',(20.2948050591539,-16.920183071726,-10.9165936719733));
#54950=CARTESIAN_POINT('',(20.293535888361,-16.9218650751948,1.76670989022851));
#54951=CARTESIAN_POINT('',(16.1739804747524,-18.9506989546656,-11.4332901033215));
#54952=CARTESIAN_POINT('Ctrl Pts',(20.2948050591539,-16.920183071726,-10.9165936719733));
#54953=CARTESIAN_POINT('Ctrl Pts',(20.3968578832778,-16.9970801053588,-10.9229640542206));
#54954=CARTESIAN_POINT('Ctrl Pts',(21.1313725981362,-17.6446400837689,-10.9717263720284));
#54955=CARTESIAN_POINT('Ctrl Pts',(21.6797113984698,-19.6491907408466,-11.0628806253967));
#54956=CARTESIAN_POINT('Ctrl Pts',(19.742230629931,-21.8062532419297,-11.1900564320781));
#54957=CARTESIAN_POINT('Ctrl Pts',(16.9631832264668,-21.35816637253,-11.3135258905595));
#54958=CARTESIAN_POINT('Ctrl Pts',(16.1754043811927,-19.7256331452917,-11.3946034134805));
#54959=CARTESIAN_POINT('Ctrl Pts',(16.1705865782758,-18.9507193134542,-11.433289000841));
#54960=CARTESIAN_POINT('Ctrl Pts',(16.1740003306697,-18.950698835557,-11.4332901097715));
#54961=CARTESIAN_POINT('Ctrl Pts',(16.174038011382,-18.8765632322752,-11.436996088328));
#54962=CARTESIAN_POINT('Ctrl Pts',(16.1772957565522,-18.8025118189363,-11.4407020668845));
#54963=CARTESIAN_POINT('Ctrl Pts',(16.1837535357011,-18.7287446051466,-11.444408045441));
#54964=CARTESIAN_POINT('Ctrl Pts',(16.1910453870482,-18.6454497843057,-11.448592679834));
#54965=CARTESIAN_POINT('Ctrl Pts',(16.2024358975503,-18.5623575749321,-11.4527773142271));
#54966=CARTESIAN_POINT('Ctrl Pts',(16.217906819526,-18.4799034980302,-11.4569619486201));
#54967=CARTESIAN_POINT('Ctrl Pts',(16.2333557205591,-18.3975667843009,-11.4611406267041));
#54968=CARTESIAN_POINT('Ctrl Pts',(16.2528734125179,-18.3158668471442,-11.465319304788));
#54969=CARTESIAN_POINT('Ctrl Pts',(16.2763898192684,-18.2352349062878,-11.469497982872));
#54970=CARTESIAN_POINT('Ctrl Pts',(16.3003277407088,-18.1531576958409,-11.4737515607574));
#54971=CARTESIAN_POINT('Ctrl Pts',(16.3284090988417,-18.0721876262597,-11.4780051386428));
#54972=CARTESIAN_POINT('Ctrl Pts',(16.3605053261112,-17.9927695620856,-11.4822587165282));
#54973=CARTESIAN_POINT('Ctrl Pts',(16.3919793053844,-17.9148911720571,-11.4864298305062));
#54974=CARTESIAN_POINT('Ctrl Pts',(16.4273136905277,-17.8385055933013,-11.4906009444841));
#54975=CARTESIAN_POINT('Ctrl Pts',(16.4663372697809,-17.7640161019714,-11.4947720584621));
#54976=CARTESIAN_POINT('Ctrl Pts',(16.5053477542952,-17.6895516063097,-11.4989417727825));
#54977=CARTESIAN_POINT('Ctrl Pts',(16.5480447610381,-17.6169823416312,-11.5031114871028));
#54978=CARTESIAN_POINT('Ctrl Pts',(16.5942102750742,-17.5466886704001,-11.5072812014232));
#54979=CARTESIAN_POINT('Ctrl Pts',(16.6403741463431,-17.4763975005194,-11.5114507673673));
#54980=CARTESIAN_POINT('Ctrl Pts',(16.6900060262586,-17.4083821471394,-11.5156203333113));
#54981=CARTESIAN_POINT('Ctrl Pts',(16.7428443053793,-17.3429944065419,-11.5197898992553));
#54982=CARTESIAN_POINT('Ctrl Pts',(16.7975403132107,-17.2753077136495,-11.5241060619943));
#54983=CARTESIAN_POINT('Ctrl Pts',(16.8556720579014,-17.2104372553887,-11.5284222247332));
#54984=CARTESIAN_POINT('Ctrl Pts',(16.9169048877879,-17.1487348078625,-11.5327383874721));
#54985=CARTESIAN_POINT('Ctrl Pts',(16.9761430646814,-17.0890423110745,-11.5369139516638));
#54986=CARTESIAN_POINT('Ctrl Pts',(17.0382830139764,-17.0323148814136,-11.5410895158555));
#54987=CARTESIAN_POINT('Ctrl Pts',(17.1029865459476,-16.9788312001503,-11.5452650800471));
#54988=CARTESIAN_POINT('Ctrl Pts',(17.1709580995006,-16.9226461852919,-11.5496515420597));
#54989=CARTESIAN_POINT('Ctrl Pts',(17.2417585461137,-16.8700415621994,-11.5540380040722));
#54990=CARTESIAN_POINT('Ctrl Pts',(17.3149615008575,-16.8212889126042,-11.5584244660848));
#54991=CARTESIAN_POINT('Ctrl Pts',(17.3881644556012,-16.772536263009,-11.5628109280973));
#54992=CARTESIAN_POINT('Ctrl Pts',(17.4637693807619,-16.7276358177823,-11.5671973901098));
#54993=CARTESIAN_POINT('Ctrl Pts',(17.5413224142637,-16.6868023979171,-11.5715838521224));
#54994=CARTESIAN_POINT('Ctrl Pts',(17.615307117733,-16.6478477842295,-11.5757684865154));
#54995=CARTESIAN_POINT('Ctrl Pts',(17.6913399834857,-16.6124491640088,-11.5799531209085));
#54996=CARTESIAN_POINT('Ctrl Pts',(17.7690449301558,-16.5808269331021,-11.5841377553015));
#54997=CARTESIAN_POINT('Ctrl Pts',(17.8466392734524,-16.549249712527,-11.5883164333855));
#54998=CARTESIAN_POINT('Ctrl Pts',(17.9259005477808,-16.5214383763015,-11.5924951114694));
#54999=CARTESIAN_POINT('Ctrl Pts',(18.0064282347098,-16.4975674125468,-11.5966737895534));
#55000=CARTESIAN_POINT('Ctrl Pts',(18.0883993225526,-16.4732685789225,-11.6009273674388));
#55001=CARTESIAN_POINT('Ctrl Pts',(18.1716822438314,-16.4530529941954,-11.6051809453242));
#55002=CARTESIAN_POINT('Ctrl Pts',(18.2558333466885,-16.4370533501362,-11.6094345232097));
#55003=CARTESIAN_POINT('Ctrl Pts',(18.3383530162095,-16.4213638903979,-11.6136056371876));
#55004=CARTESIAN_POINT('Ctrl Pts',(18.4217070321717,-16.4097284515022,-11.6177767511656));
#55005=CARTESIAN_POINT('Ctrl Pts',(18.5054636294716,-16.4022213571869,-11.6219478651435));
#55006=CARTESIAN_POINT('Ctrl Pts',(18.5891921214364,-16.3947167819496,-11.6261175794639));
#55007=CARTESIAN_POINT('Ctrl Pts',(18.6733224686331,-16.3913378410871,-11.6302872937843));
#55008=CARTESIAN_POINT('Ctrl Pts',(18.7574168390734,-16.3921071015279,-11.6344570081047));
#55009=CARTESIAN_POINT('Ctrl Pts',(18.8415082170751,-16.3928763345952,-11.6386265740487));
#55010=CARTESIAN_POINT('Ctrl Pts',(18.9255631608599,-16.3977934704174,-11.6427961399927));
#55011=CARTESIAN_POINT('Ctrl Pts',(19.009144261199,-16.4068289575101,-11.6469657059368));
#55012=CARTESIAN_POINT('Ctrl Pts',(19.0956639699175,-16.4161821211824,-11.6512818686757));
#55013=CARTESIAN_POINT('Ctrl Pts',(19.1816753701876,-16.4299485702282,-11.6555980314146));
#55014=CARTESIAN_POINT('Ctrl Pts',(19.2667015333782,-16.4480373252909,-11.6599141941535));
#55015=CARTESIAN_POINT('Ctrl Pts',(19.348957978246,-16.46553684106,-11.6640897583452));
#55016=CARTESIAN_POINT('Ctrl Pts',(19.4302919452566,-16.4870812228023,-11.6682653225369));
#55017=CARTESIAN_POINT('Ctrl Pts',(19.5102860518794,-16.5125369513646,-11.6724408867286));
#55018=CARTESIAN_POINT('Ctrl Pts',(19.5943204706598,-16.5392783882613,-11.6768273487411));
#55019=CARTESIAN_POINT('Ctrl Pts',(19.6768755727334,-16.570336474695,-11.6812138107537));
#55020=CARTESIAN_POINT('Ctrl Pts',(19.7574922067679,-16.605499690457,-11.6856002727662));
#55021=CARTESIAN_POINT('Ctrl Pts',(19.8381088408023,-16.640662906219,-11.6899867347787));
#55022=CARTESIAN_POINT('Ctrl Pts',(19.9167865216171,-16.6799309241433,-11.6943731967913));
#55023=CARTESIAN_POINT('Ctrl Pts',(19.9930989518199,-16.7230383965788,-11.6987596588038));
#55024=CARTESIAN_POINT('Ctrl Pts',(20.0658940459174,-16.7641589912696,-11.7029439432528));
#55025=CARTESIAN_POINT('Ctrl Pts',(20.1368080586058,-16.8089259475303,-11.7071282277017));
#55026=CARTESIAN_POINT('Ctrl Pts',(20.2054522028094,-16.8571423879301,-11.7113125121506));
#55027=CARTESIAN_POINT('Ctrl Pts',(20.2352510809046,-16.8780734643726,-11.7131289377709));
#55028=CARTESIAN_POINT('Ctrl Pts',(20.2646224661193,-16.8996539802127,-11.7149453633911));
#55029=CARTESIAN_POINT('Ctrl Pts',(20.293535888361,-16.9218650751948,-11.7167617890113));
#55030=CARTESIAN_POINT('',(16.1740004874608,-18.9535798097909,-11.3667098902285));
#55031=CARTESIAN_POINT('Ctrl Pts',(16.1740004874608,-18.9535798097909,-11.3667098902285));
#55032=CARTESIAN_POINT('Ctrl Pts',(16.1739481146197,-18.8687123476393,-11.3709134538372));
#55033=CARTESIAN_POINT('Ctrl Pts',(16.1781202862138,-18.7838299700766,-11.3751170174459));
#55034=CARTESIAN_POINT('Ctrl Pts',(16.1864949217896,-18.699377996817,-11.3793205810546));
#55035=CARTESIAN_POINT('Ctrl Pts',(16.1948707822013,-18.6149136719983,-11.3835247594573));
#55036=CARTESIAN_POINT('Ctrl Pts',(16.2074502833288,-18.5308803238368,-11.3877289378599));
#55037=CARTESIAN_POINT('Ctrl Pts',(16.2241595327126,-18.447717510946,-11.3919331162626));
#55038=CARTESIAN_POINT('Ctrl Pts',(16.2408759290274,-18.3645191274036,-11.3961390928892));
#55039=CARTESIAN_POINT('Ctrl Pts',(16.2617254950327,-18.2821924593937,-11.4003450695159));
#55040=CARTESIAN_POINT('Ctrl Pts',(16.2865836343726,-18.2011650425965,-11.4045510461425));
#55041=CARTESIAN_POINT('Ctrl Pts',(16.3114761780105,-18.1200254817903,-11.408762843948));
#55042=CARTESIAN_POINT('Ctrl Pts',(16.3403882340966,-18.0401891906195,-11.4129746417534));
#55043=CARTESIAN_POINT('Ctrl Pts',(16.3731460171586,-17.9620664306621,-11.4171864395589));
#55044=CARTESIAN_POINT('Ctrl Pts',(16.4059305542806,-17.8838798659902,-11.4214016772397));
#55045=CARTESIAN_POINT('Ctrl Pts',(16.4425668768385,-17.8074100228066,-11.4256169149205));
#55046=CARTESIAN_POINT('Ctrl Pts',(16.4828349986458,-17.7330430127859,-11.4298321526013));
#55047=CARTESIAN_POINT('Ctrl Pts',(16.5231739006091,-17.6585452862497,-11.4340547994973));
#55048=CARTESIAN_POINT('Ctrl Pts',(16.5671571084147,-17.5861581518398,-11.4382774463933));
#55049=CARTESIAN_POINT('Ctrl Pts',(16.6145212917447,-17.5162388759782,-11.4425000932893));
#55050=CARTESIAN_POINT('Ctrl Pts',(16.6269438222717,-17.4979006660113,-11.4436075959693));
#55051=CARTESIAN_POINT('Ctrl Pts',(16.6395987151329,-17.4797320374711,-11.4447150986492));
#55052=CARTESIAN_POINT('Ctrl Pts',(16.6524807786036,-17.4617390393098,-11.4458226013291));
#55053=CARTESIAN_POINT('Ctrl Pts',(16.7011549053849,-17.3937535433782,-11.4500072357222));
#55054=CARTESIAN_POINT('Ctrl Pts',(16.7532538754926,-17.3280286903786,-11.4541918701152));
#55055=CARTESIAN_POINT('Ctrl Pts',(16.8085402991528,-17.2649300724589,-11.4583765045082));
#55056=CARTESIAN_POINT('Ctrl Pts',(16.8637480294321,-17.2019212676117,-11.4625551825922));
#55057=CARTESIAN_POINT('Ctrl Pts',(16.9221339008883,-17.141531615807,-11.4667338606761));
#55058=CARTESIAN_POINT('Ctrl Pts',(16.9834181011139,-17.0840966258148,-11.4709125387601));
#55059=CARTESIAN_POINT('Ctrl Pts',(17.0458007765844,-17.0256321549048,-11.4751661166455));
#55060=CARTESIAN_POINT('Ctrl Pts',(17.1111864272471,-16.9702297043272,-11.4794196945309));
#55061=CARTESIAN_POINT('Ctrl Pts',(17.1792379481544,-16.9182067553114,-11.4836732724164));
#55062=CARTESIAN_POINT('Ctrl Pts',(17.2459701575374,-16.8671923726767,-11.4878443863943));
#55063=CARTESIAN_POINT('Ctrl Pts',(17.3152654110889,-16.8194279167438,-11.4920155003723));
#55064=CARTESIAN_POINT('Ctrl Pts',(17.386771066055,-16.7751733648402,-11.4961866143502));
#55065=CARTESIAN_POINT('Ctrl Pts',(17.4582527266079,-16.7309336629788,-11.5003563286706));
#55066=CARTESIAN_POINT('Ctrl Pts',(17.5319429246537,-16.6902017679485,-11.504526042991));
#55067=CARTESIAN_POINT('Ctrl Pts',(17.6074603942082,-16.6531941107213,-11.5086957573114));
#55068=CARTESIAN_POINT('Ctrl Pts',(17.6829751765272,-16.6161877703853,-11.5128653232554));
#55069=CARTESIAN_POINT('Ctrl Pts',(17.7603166876029,-16.5829056060342,-11.5170348891994));
#55070=CARTESIAN_POINT('Ctrl Pts',(17.8390806772783,-16.5535172700602,-11.5212044551435));
#55071=CARTESIAN_POINT('Ctrl Pts',(17.9206139116647,-16.5230956764479,-11.5255206178824));
#55072=CARTESIAN_POINT('Ctrl Pts',(18.0036710203271,-16.4968470041693,-11.5298367806213));
#55073=CARTESIAN_POINT('Ctrl Pts',(18.0877848913437,-16.4749037093112,-11.5341529433602));
#55074=CARTESIAN_POINT('Ctrl Pts',(18.1691587618592,-16.453675214975,-11.5383285075519));
#55075=CARTESIAN_POINT('Ctrl Pts',(18.2515211332007,-16.4364759603011,-11.5425040717436));
#55076=CARTESIAN_POINT('Ctrl Pts',(18.3344390537291,-16.4233736831602,-11.5466796359353));
#55077=CARTESIAN_POINT('Ctrl Pts',(18.4215449613046,-16.4096096411485,-11.5510660979478));
#55078=CARTESIAN_POINT('Ctrl Pts',(18.5092634338795,-16.4003673913994,-11.5554525599604));
#55079=CARTESIAN_POINT('Ctrl Pts',(18.5970892183628,-16.3956636688668,-11.5598390219729));
#55080=CARTESIAN_POINT('Ctrl Pts',(18.6849150028461,-16.3909599463343,-11.5642254839854));
#55081=CARTESIAN_POINT('Ctrl Pts',(18.7728475188787,-16.3907946760441,-11.568611945998));
#55082=CARTESIAN_POINT('Ctrl Pts',(18.8603867536229,-16.3951217493771,-11.5729984080105));
#55083=CARTESIAN_POINT('Ctrl Pts',(18.9438873685615,-16.3992491933197,-11.5771825007379));
#55084=CARTESIAN_POINT('Ctrl Pts',(19.0273409554117,-16.4074789682949,-11.5813665934652));
#55085=CARTESIAN_POINT('Ctrl Pts',(19.1103117838484,-16.4198093592036,-11.5855506861926));
#55086=CARTESIAN_POINT('Ctrl Pts',(19.1931709965617,-16.4321231627704,-11.5897291503087));
#55087=CARTESIAN_POINT('Ctrl Pts',(19.2755482894343,-16.448526562281,-11.5939076144249));
#55088=CARTESIAN_POINT('Ctrl Pts',(19.357010161509,-16.4689659006255,-11.598086078541));
#55089=CARTESIAN_POINT('Ctrl Pts',(19.4414693002971,-16.4901572735956,-11.6024182829419));
#55090=CARTESIAN_POINT('Ctrl Pts',(19.5249438451359,-16.5156873315821,-11.6067504873428));
#55091=CARTESIAN_POINT('Ctrl Pts',(19.6069591096031,-16.5454376399185,-11.6110826917437));
#55092=CARTESIAN_POINT('Ctrl Pts',(19.6859209486914,-16.5740803453337,-11.6152536083288));
#55093=CARTESIAN_POINT('Ctrl Pts',(19.763529765532,-16.6066344601364,-11.6194245249139));
#55094=CARTESIAN_POINT('Ctrl Pts',(19.8393764673876,-16.6429432953377,-11.6235954414991));
#55095=CARTESIAN_POINT('Ctrl Pts',(19.9151926442948,-16.6792375178362,-11.6277646794744));
#55096=CARTESIAN_POINT('Ctrl Pts',(19.9892477021866,-16.719283257044,-11.6319339174498));
#55097=CARTESIAN_POINT('Ctrl Pts',(20.0611538617777,-16.7628762878337,-11.6361031554252));
#55098=CARTESIAN_POINT('Ctrl Pts',(20.1330612502713,-16.8064700636442,-11.6402724646544));
#55099=CARTESIAN_POINT('Ctrl Pts',(20.202819273287,-16.8536110146999,-11.6444417738836));
#55100=CARTESIAN_POINT('Ctrl Pts',(20.2700670848392,-16.9040503153462,-11.6486110831128));
#55101=CARTESIAN_POINT('Ctrl Pts',(20.2779244372492,-16.9099437318209,-11.6490982325257));
#55102=CARTESIAN_POINT('Ctrl Pts',(20.2857475543659,-16.9158821298114,-11.6495853819387));
#55103=CARTESIAN_POINT('Ctrl Pts',(20.293535888361,-16.9218650751948,-11.6500725313516));
#55104=CARTESIAN_POINT('Ctrl Pts',(20.2922820154255,-16.9234654489969,-10.8502164909775));
#55105=CARTESIAN_POINT('Ctrl Pts',(20.7519191282237,-17.2828443540149,-10.8791841188528));
#55106=CARTESIAN_POINT('Ctrl Pts',(21.5989576167214,-18.5500198638012,-10.9505436822886));
#55107=CARTESIAN_POINT('Ctrl Pts',(20.9146849414325,-21.0515011378533,-11.0642951812848));
#55108=CARTESIAN_POINT('Ctrl Pts',(18.1490151951601,-21.9220310806025,-11.1914709879662));
#55109=CARTESIAN_POINT('Ctrl Pts',(16.3822353344203,-20.4522479494082,-11.2922755723059));
#55110=CARTESIAN_POINT('Ctrl Pts',(16.1753927157401,-19.2766421922516,-11.350688221085));
#55111=CARTESIAN_POINT('Ctrl Pts',(16.177204683354,-18.953597107844,-11.3667089343037));
#55112=CARTESIAN_POINT('Origin',(18.734,-18.952,1.76670989022851));
#55113=CARTESIAN_POINT('',(20.293535888361,-16.9218650751948,-10.0501312781553));
#55114=CARTESIAN_POINT('',(20.293535888361,-16.9218650751948,-10.1166694971161));
#55115=CARTESIAN_POINT('',(20.293535888361,-16.9218650751948,1.76670989022851));
#55116=CARTESIAN_POINT('',(16.1740004874608,-18.9504201902088,-10.6332901097715));
#55117=CARTESIAN_POINT('Ctrl Pts',(20.293535888361,-16.9218650751947,-10.1166694971161));
#55118=CARTESIAN_POINT('Ctrl Pts',(20.3602256419765,-16.9730956918787,-10.120839657233));
#55119=CARTESIAN_POINT('Ctrl Pts',(20.4243735084243,-17.0276044555347,-10.1250098173499));
#55120=CARTESIAN_POINT('Ctrl Pts',(20.4856520344282,-17.0851001231229,-10.1291799774668));
#55121=CARTESIAN_POINT('Ctrl Pts',(20.5469978537159,-17.1426589298323,-10.1333547170634));
#55122=CARTESIAN_POINT('Ctrl Pts',(20.6054677076776,-17.2032108717433,-10.1375294566601));
#55123=CARTESIAN_POINT('Ctrl Pts',(20.6607708315928,-17.2664276454204,-10.1417041962567));
#55124=CARTESIAN_POINT('Ctrl Pts',(20.7161082334552,-17.329683602078,-10.1458815234378));
#55125=CARTESIAN_POINT('Ctrl Pts',(20.7682747131804,-17.3956073175892,-10.1500588506188));
#55126=CARTESIAN_POINT('Ctrl Pts',(20.8170211514923,-17.4638390939029,-10.1542361777999));
#55127=CARTESIAN_POINT('Ctrl Pts',(20.8658480308291,-17.5321834658074,-10.1584203983765));
#55128=CARTESIAN_POINT('Ctrl Pts',(20.9112433552803,-17.6028431144115,-10.1626046189532));
#55129=CARTESIAN_POINT('Ctrl Pts',(20.9530027200995,-17.6754315810772,-10.1667888395298));
#55130=CARTESIAN_POINT('Ctrl Pts',(20.9725011699955,-17.7093248786989,-10.1687425525621));
#55131=CARTESIAN_POINT('Ctrl Pts',(20.9912075876463,-17.7436383769395,-10.1706962655943));
#55132=CARTESIAN_POINT('Ctrl Pts',(21.0091047687182,-17.7783312684767,-10.1726499786266));
#55133=CARTESIAN_POINT('Ctrl Pts',(21.0474385251168,-17.8526395546591,-10.1768346130197));
#55134=CARTESIAN_POINT('Ctrl Pts',(21.0821992629535,-17.9289661561369,-10.1810192474127));
#55135=CARTESIAN_POINT('Ctrl Pts',(21.1131697431269,-18.0069331593007,-10.1852038818058));
#55136=CARTESIAN_POINT('Ctrl Pts',(21.1440961406553,-18.0847891860861,-10.1893825598897));
#55137=CARTESIAN_POINT('Ctrl Pts',(21.1712428282378,-18.1642805528131,-10.1935612379737));
#55138=CARTESIAN_POINT('Ctrl Pts',(21.1944386775071,-18.2450052940602,-10.1977399160576));
#55139=CARTESIAN_POINT('Ctrl Pts',(21.2180502957041,-18.327176968278,-10.2019934939431));
#55140=CARTESIAN_POINT('Ctrl Pts',(21.2375678238505,-18.4106262399203,-10.2062470718285));
#55141=CARTESIAN_POINT('Ctrl Pts',(21.252862289631,-18.4949083616223,-10.2105006497139));
#55142=CARTESIAN_POINT('Ctrl Pts',(21.2678602423477,-18.5775565099321,-10.2146717636919));
#55143=CARTESIAN_POINT('Ctrl Pts',(21.2787973301571,-18.6610050301441,-10.2188428776698));
#55144=CARTESIAN_POINT('Ctrl Pts',(21.2856028472,-18.7448215499602,-10.2230139916478));
#55145=CARTESIAN_POINT('Ctrl Pts',(21.2924060805859,-18.8286099443337,-10.2271837059682));
#55146=CARTESIAN_POINT('Ctrl Pts',(21.2950804593957,-18.9127656349242,-10.2313534202885));
#55147=CARTESIAN_POINT('Ctrl Pts',(21.2936070835643,-18.9968506161339,-10.2355231346089));
#55148=CARTESIAN_POINT('Ctrl Pts',(21.2921337601619,-19.0809326052393,-10.239692700553));
#55149=CARTESIAN_POINT('Ctrl Pts',(21.2865129844866,-19.1649434300193,-10.243862266497));
#55150=CARTESIAN_POINT('Ctrl Pts',(21.2767779695195,-19.2484459440205,-10.2480318324411));
#55151=CARTESIAN_POINT('Ctrl Pts',(21.2667006834357,-19.3348843034021,-10.25234799518));
#55152=CARTESIAN_POINT('Ctrl Pts',(21.2522145228801,-19.4207774186565,-10.2566641579189));
#55153=CARTESIAN_POINT('Ctrl Pts',(21.2334144574579,-19.5056491396638,-10.2609803206578));
#55154=CARTESIAN_POINT('Ctrl Pts',(21.2152268021893,-19.5877561732863,-10.2651558848495));
#55155=CARTESIAN_POINT('Ctrl Pts',(21.1930021468738,-19.668906892756,-10.2693314490412));
#55156=CARTESIAN_POINT('Ctrl Pts',(21.166877500828,-19.7486850481621,-10.2735070132329));
#55157=CARTESIAN_POINT('Ctrl Pts',(21.1394333610159,-19.8324926085431,-10.2778934752454));
#55158=CARTESIAN_POINT('Ctrl Pts',(21.1076851096662,-19.9147847597334,-10.2822799372579));
#55159=CARTESIAN_POINT('Ctrl Pts',(21.0718481041567,-19.9951041376061,-10.2866663992705));
#55160=CARTESIAN_POINT('Ctrl Pts',(21.0360110986472,-20.0754235154788,-10.291052861283));
#55161=CARTESIAN_POINT('Ctrl Pts',(20.9960856701951,-20.15376963761,-10.2954393232956));
#55162=CARTESIAN_POINT('Ctrl Pts',(20.9523407266399,-20.2297184433712,-10.2998257853081));
#55163=CARTESIAN_POINT('Ctrl Pts',(20.9106085527831,-20.3021727319963,-10.3040104197011));
#55164=CARTESIAN_POINT('Ctrl Pts',(20.8652452879882,-20.3727151532424,-10.3081950540942));
#55165=CARTESIAN_POINT('Ctrl Pts',(20.8164511103895,-20.440958485935,-10.3123796884872));
#55166=CARTESIAN_POINT('Ctrl Pts',(20.7677263852629,-20.5091046826904,-10.3165583665712));
#55167=CARTESIAN_POINT('Ctrl Pts',(20.7155807127377,-20.5749579200271,-10.3207370446551));
#55168=CARTESIAN_POINT('Ctrl Pts',(20.6602594535816,-20.6381567298112,-10.3249157227391));
#55169=CARTESIAN_POINT('Ctrl Pts',(20.603946600614,-20.7024883328402,-10.3291693006245));
#55170=CARTESIAN_POINT('Ctrl Pts',(20.5443434371028,-20.7640689932949,-10.33342287851));
#55171=CARTESIAN_POINT('Ctrl Pts',(20.4817541149309,-20.8225495325551,-10.3376764563954));
#55172=CARTESIAN_POINT('Ctrl Pts',(20.4203782089023,-20.8798963124463,-10.3418475703733));
#55173=CARTESIAN_POINT('Ctrl Pts',(20.3561312476116,-20.9342617737267,-10.3460186843513));
#55174=CARTESIAN_POINT('Ctrl Pts',(20.2893385159965,-20.9853524290338,-10.3501897983292));
#55175=CARTESIAN_POINT('Ctrl Pts',(20.2225681973275,-21.0364259403781,-10.3543595126496));
#55176=CARTESIAN_POINT('Ctrl Pts',(20.1532541699938,-21.0842265489053,-10.35852922697));
#55177=CARTESIAN_POINT('Ctrl Pts',(20.0817544971403,-21.1285012785289,-10.3626989412904));
#55178=CARTESIAN_POINT('Ctrl Pts',(20.0102573685523,-21.1727744326675,-10.3668685072344));
#55179=CARTESIAN_POINT('Ctrl Pts',(19.9365751406472,-21.2135217158936,-10.3710380731785));
#55180=CARTESIAN_POINT('Ctrl Pts',(19.8610933619694,-21.2505344359841,-10.3752076391225));
#55181=CARTESIAN_POINT('Ctrl Pts',(19.78295773707,-21.2888484776529,-10.3795238018614));
#55182=CARTESIAN_POINT('Ctrl Pts',(19.7028941360643,-21.3231602233057,-10.3838399646003));
#55183=CARTESIAN_POINT('Ctrl Pts',(19.6213543310965,-21.3532917963222,-10.3881561273392));
#55184=CARTESIAN_POINT('Ctrl Pts',(19.5424706766991,-21.382441836517,-10.3923316915309));
#55185=CARTESIAN_POINT('Ctrl Pts',(19.4622059796066,-21.4076797638284,-10.3965072557226));
#55186=CARTESIAN_POINT('Ctrl Pts',(19.3809844006654,-21.4288954732277,-10.4006828199143));
#55187=CARTESIAN_POINT('Ctrl Pts',(19.2956605128578,-21.4511827376731,-10.4050692819268));
#55188=CARTESIAN_POINT('Ctrl Pts',(19.2092811104196,-21.469030663203,-10.4094557439394));
#55189=CARTESIAN_POINT('Ctrl Pts',(19.122347333066,-21.4823727687636,-10.4138422059519));
#55190=CARTESIAN_POINT('Ctrl Pts',(19.0354135557123,-21.4957148743243,-10.4182286679644));
#55191=CARTESIAN_POINT('Ctrl Pts',(18.947925988367,-21.50455117729,-10.422615129977));
#55192=CARTESIAN_POINT('Ctrl Pts',(18.8603867536229,-21.5088782506229,-10.4270015919895));
#55193=CARTESIAN_POINT('Ctrl Pts',(18.7768753288337,-21.5130062288976,-10.4311862263825));
#55194=CARTESIAN_POINT('Ctrl Pts',(18.693006041295,-21.5130461767751,-10.4353708607756));
#55195=CARTESIAN_POINT('Ctrl Pts',(18.6092128353628,-21.5089568169099,-10.4395554951686));
#55196=CARTESIAN_POINT('Ctrl Pts',(18.5255388986877,-21.5048732777423,-10.4437341732526));
#55197=CARTESIAN_POINT('Ctrl Pts',(18.4419412840716,-21.4966721277451,-10.4479128513365));
#55198=CARTESIAN_POINT('Ctrl Pts',(18.3588567381415,-21.4843640206499,-10.4520915294204));
#55199=CARTESIAN_POINT('Ctrl Pts',(18.2742829614372,-21.4718352995807,-10.4563451073059));
#55200=CARTESIAN_POINT('Ctrl Pts',(18.1902413094004,-21.4550509150074,-10.4605986851913));
#55201=CARTESIAN_POINT('Ctrl Pts',(18.1071900176372,-21.4340776067662,-10.4648522630767));
#55202=CARTESIAN_POINT('Ctrl Pts',(18.0257488372261,-21.4135109070313,-10.4690233770547));
#55203=CARTESIAN_POINT('Ctrl Pts',(17.9452604262034,-21.3889163729565,-10.4731944910326));
#55204=CARTESIAN_POINT('Ctrl Pts',(17.8661476315627,-21.360408658554,-10.4773656050106));
#55205=CARTESIAN_POINT('Ctrl Pts',(17.7870613839843,-21.3319105101903,-10.481535319331));
#55206=CARTESIAN_POINT('Ctrl Pts',(17.7093502684721,-21.2995019451709,-10.4857050336513));
#55207=CARTESIAN_POINT('Ctrl Pts',(17.6334208106696,-21.2633471067784,-10.4898747479717));
#55208=CARTESIAN_POINT('Ctrl Pts',(17.5574940547628,-21.2271935549301,-10.4940443139158));
#55209=CARTESIAN_POINT('Ctrl Pts',(17.4833492454958,-21.1872941933041,-10.4982138798598));
#55210=CARTESIAN_POINT('Ctrl Pts',(17.4113705501161,-21.1438602460695,-10.5023834458039));
#55211=CARTESIAN_POINT('Ctrl Pts',(17.3368611726025,-21.0988992148319,-10.5066996085428));
#55212=CARTESIAN_POINT('Ctrl Pts',(17.2646735157618,-21.0501506938737,-10.5110157712817));
#55213=CARTESIAN_POINT('Ctrl Pts',(17.1952016813753,-20.9978982708331,-10.5153319340206));
#55214=CARTESIAN_POINT('Ctrl Pts',(17.1279928846869,-20.947347964977,-10.5195074982123));
#55215=CARTESIAN_POINT('Ctrl Pts',(17.0633260236107,-20.8935188682644,-10.523683062404));
#55216=CARTESIAN_POINT('Ctrl Pts',(17.0015232692729,-20.8367080350784,-10.5278586265957));
#55217=CARTESIAN_POINT('Ctrl Pts',(16.9365990047356,-20.7770278217632,-10.5322450886082));
#55218=CARTESIAN_POINT('Ctrl Pts',(16.8748361916356,-20.7140571577261,-10.5366315506207));
#55219=CARTESIAN_POINT('Ctrl Pts',(16.816561987441,-20.6481814372271,-10.5410180126333));
#55220=CARTESIAN_POINT('Ctrl Pts',(16.7582877832464,-20.5823057167281,-10.5454044746458));
#55221=CARTESIAN_POINT('Ctrl Pts',(16.7035024899564,-20.513525441,-10.5497909366584));
#55222=CARTESIAN_POINT('Ctrl Pts',(16.6524807786035,-20.4422609606901,-10.5541773986709));
#55223=CARTESIAN_POINT('Ctrl Pts',(16.6033728384837,-20.3736695367859,-10.5583993290636));
#55224=CARTESIAN_POINT('Ctrl Pts',(16.55756917535,-20.302523084569,-10.5626212594563));
#55225=CARTESIAN_POINT('Ctrl Pts',(16.5153433201942,-20.2291697370175,-10.5668431898491));
#55226=CARTESIAN_POINT('Ctrl Pts',(16.4731798646836,-20.1559247880487,-10.5710588812454));
#55227=CARTESIAN_POINT('Ctrl Pts',(16.4345839361667,-20.0804798079436,-10.5752745726417));
#55228=CARTESIAN_POINT('Ctrl Pts',(16.3997870211452,-20.0032134746785,-10.579490264038));
#55229=CARTESIAN_POINT('Ctrl Pts',(16.3650317212897,-19.9260395476307,-10.583700913703));
#55230=CARTESIAN_POINT('Ctrl Pts',(16.3340665899187,-19.8470490030815,-10.587911563368));
#55231=CARTESIAN_POINT('Ctrl Pts',(16.3070776023617,-19.7666457364042,-10.5921222130329));
#55232=CARTESIAN_POINT('Ctrl Pts',(16.2801155537111,-19.686322723796,-10.5963286598616));
#55233=CARTESIAN_POINT('Ctrl Pts',(16.2571218975387,-19.6045902181233,-10.6005351066902));
#55234=CARTESIAN_POINT('Ctrl Pts',(16.2382342921444,-19.5218715043693,-10.6047415535189));
#55235=CARTESIAN_POINT('Ctrl Pts',(16.2193575415102,-19.439200329293,-10.6089455828907));
#55236=CARTESIAN_POINT('Ctrl Pts',(16.2045822501753,-19.3555445100533,-10.6131496122625));
#55237=CARTESIAN_POINT('Ctrl Pts',(16.1939957867901,-19.271340878805,-10.6173536416343));
#55238=CARTESIAN_POINT('Ctrl Pts',(16.1834116610727,-19.1871558411241,-10.6215567426862));
#55239=CARTESIAN_POINT('Ctrl Pts',(16.1770145819502,-19.1024236771961,-10.6257598437382));
#55240=CARTESIAN_POINT('Ctrl Pts',(16.1748403468597,-19.0175886403178,-10.6299629447901));
#55241=CARTESIAN_POINT('Ctrl Pts',(16.1742666403856,-18.9952035679304,-10.6310719997839));
#55242=CARTESIAN_POINT('Ctrl Pts',(16.1739866695752,-18.9728113543428,-10.6321810547777));
#55243=CARTESIAN_POINT('Ctrl Pts',(16.1740004874608,-18.9504201902088,-10.6332901097715));
#55244=CARTESIAN_POINT('Ctrl Pts',(16.1772048604514,-18.9504028912009,-10.6332910657491));
#55245=CARTESIAN_POINT('Ctrl Pts',(16.1753928930938,-18.6273578295265,-10.6493117789502));
#55246=CARTESIAN_POINT('Ctrl Pts',(16.3822354976306,-17.4517521542537,-10.7077244277117));
#55247=CARTESIAN_POINT('Ctrl Pts',(18.037362949687,-16.0748525964386,-10.8021586297865));
#55248=CARTESIAN_POINT('Ctrl Pts',(19.7177437303012,-16.4853660561861,-10.8805721186601));
#55249=CARTESIAN_POINT('Ctrl Pts',(20.2948050591539,-16.920183071726,-10.9165936719733));
#55250=CARTESIAN_POINT('',(16.1739802850659,-18.9533010441961,-10.5667098967402));
#55251=CARTESIAN_POINT('Ctrl Pts',(16.1705864007212,-18.9532806854788,-10.5667109992167));
#55252=CARTESIAN_POINT('Ctrl Pts',(16.1754042043383,-18.178366800346,-10.6053965865579));
#55253=CARTESIAN_POINT('Ctrl Pts',(16.9631831042392,-16.5458334607307,-10.6864741094597));
#55254=CARTESIAN_POINT('Ctrl Pts',(19.090228029654,-16.2028738910185,-10.7809759400466));
#55255=CARTESIAN_POINT('Ctrl Pts',(20.0792749286077,-16.7569204692939,-10.8367921832923));
#55256=CARTESIAN_POINT('Ctrl Pts',(20.2922820154255,-16.9234654489969,-10.8502164909775));
#55257=CARTESIAN_POINT('Ctrl Pts',(20.293535888361,-16.9218650751948,-10.0501312781553));
#55258=CARTESIAN_POINT('Ctrl Pts',(20.3598785012909,-16.972829020757,-10.0543142412582));
#55259=CARTESIAN_POINT('Ctrl Pts',(20.4238373170522,-17.0271382723338,-10.0584972043611));
#55260=CARTESIAN_POINT('Ctrl Pts',(20.4850560926825,-17.0845411489729,-10.0626801674639));
#55261=CARTESIAN_POINT('Ctrl Pts',(20.5461929679461,-17.1418672302726,-10.0668575344697));
#55262=CARTESIAN_POINT('Ctrl Pts',(20.6045967518193,-17.2022784029154,-10.0710349014755));
#55263=CARTESIAN_POINT('Ctrl Pts',(20.6599429831436,-17.2654818039286,-10.0752122684813));
#55264=CARTESIAN_POINT('Ctrl Pts',(20.7152315991736,-17.3286194103528,-10.079385286858));
#55265=CARTESIAN_POINT('Ctrl Pts',(20.7674686870318,-17.3945431235226,-10.0835583052348));
#55266=CARTESIAN_POINT('Ctrl Pts',(20.8163664800914,-17.4629231575933,-10.0877313236115));
#55267=CARTESIAN_POINT('Ctrl Pts',(20.8652367031686,-17.5312646370337,-10.0919019891204));
#55268=CARTESIAN_POINT('Ctrl Pts',(20.9107711025747,-17.6020593143187,-10.0960726546294));
#55269=CARTESIAN_POINT('Ctrl Pts',(20.9527228017081,-17.674945134624,-10.1002433201383));
#55270=CARTESIAN_POINT('Ctrl Pts',(20.9946634319104,-17.7478117240485,-10.1044128852196));
#55271=CARTESIAN_POINT('Ctrl Pts',(21.0330230101449,-17.8227679620443,-10.1085824503009));
#55272=CARTESIAN_POINT('Ctrl Pts',(21.0675992713509,-17.8994248526825,-10.1127520153822));
#55273=CARTESIAN_POINT('Ctrl Pts',(21.1021767816142,-17.9760845125284,-10.1169217310878));
#55274=CARTESIAN_POINT('Ctrl Pts',(21.1329705155016,-18.0544445271115,-10.1210914467934));
#55275=CARTESIAN_POINT('Ctrl Pts',(21.1598258291851,-18.1340947203628,-10.125261162499));
#55276=CARTESIAN_POINT('Ctrl Pts',(21.1867086002934,-18.2138263496091,-10.1294351414077));
#55277=CARTESIAN_POINT('Ctrl Pts',(21.2096447612378,-18.2948503552936,-10.1336091203163));
#55278=CARTESIAN_POINT('Ctrl Pts',(21.2285293388216,-18.3767405995915,-10.137783099225));
#55279=CARTESIAN_POINT('Ctrl Pts',(21.2474234560288,-18.4586722110889,-10.1419591866365));
#55280=CARTESIAN_POINT('Ctrl Pts',(21.2622618321363,-18.5414704795095,-10.1461352740481));
#55281=CARTESIAN_POINT('Ctrl Pts',(21.2729909705675,-18.6247006700641,-10.1503113614597));
#55282=CARTESIAN_POINT('Ctrl Pts',(21.283739223649,-18.7080791405565,-10.1544948888396));
#55283=CARTESIAN_POINT('Ctrl Pts',(21.2903635759395,-18.7918906111061,-10.1586784162195));
#55284=CARTESIAN_POINT('Ctrl Pts',(21.2928626078116,-18.8756969571784,-10.1628619435994));
#55285=CARTESIAN_POINT('Ctrl Pts',(21.2950932319719,-18.9505021096975,-10.1665961405712));
#55286=CARTESIAN_POINT('Ctrl Pts',(21.294037851978,-19.0253029473734,-10.170330337543));
#55287=CARTESIAN_POINT('Ctrl Pts',(21.2897303495757,-19.0997916785801,-10.1740645345148));
#55288=CARTESIAN_POINT('Ctrl Pts',(21.2849032547983,-19.1832656112237,-10.1782491689078));
#55289=CARTESIAN_POINT('Ctrl Pts',(21.2759733033623,-19.2666581465938,-10.1824338033009));
#55290=CARTESIAN_POINT('Ctrl Pts',(21.262945864237,-19.3495334146438,-10.1866184376939));
#55291=CARTESIAN_POINT('Ctrl Pts',(21.2499369680589,-19.4322907200076,-10.1907971157779));
#55292=CARTESIAN_POINT('Ctrl Pts',(21.232842239734,-19.514531769942,-10.1949757938618));
#55293=CARTESIAN_POINT('Ctrl Pts',(21.2117189811603,-19.595823462137,-10.1991544719458));
#55294=CARTESIAN_POINT('Ctrl Pts',(21.1902171033577,-19.6785722494913,-10.2034080498312));
#55295=CARTESIAN_POINT('Ctrl Pts',(21.1645408797954,-19.7603368285348,-10.2076616277166));
#55296=CARTESIAN_POINT('Ctrl Pts',(21.1348056750072,-19.840668729535,-10.2119152056021));
#55297=CARTESIAN_POINT('Ctrl Pts',(21.1056469451873,-19.9194432398795,-10.21608631958));
#55298=CARTESIAN_POINT('Ctrl Pts',(21.0725853792787,-19.9968396756824,-10.220257433558));
#55299=CARTESIAN_POINT('Ctrl Pts',(21.0357801964354,-20.0724498771912,-10.2244285475359));
#55300=CARTESIAN_POINT('Ctrl Pts',(20.9989873639267,-20.1480347069666,-10.2285982618563));
#55301=CARTESIAN_POINT('Ctrl Pts',(20.9584536105076,-20.2218340795557,-10.2327679761767));
#55302=CARTESIAN_POINT('Ctrl Pts',(20.9143856152224,-20.2934613557353,-10.236937690497));
#55303=CARTESIAN_POINT('Ctrl Pts',(20.8703191880656,-20.3650860831091,-10.2411072564411));
#55304=CARTESIAN_POINT('Ctrl Pts',(20.8227190108796,-20.4345384763813,-10.2452768223851));
#55305=CARTESIAN_POINT('Ctrl Pts',(20.7718361823766,-20.5014591617067,-10.2494463883292));
#55306=CARTESIAN_POINT('Ctrl Pts',(20.7191643763941,-20.5707326957726,-10.2537625510681));
#55307=CARTESIAN_POINT('Ctrl Pts',(20.662975107358,-20.6372927599322,-10.258078713807));
#55308=CARTESIAN_POINT('Ctrl Pts',(20.6035924848957,-20.7007778419289,-10.2623948765459));
#55309=CARTESIAN_POINT('Ctrl Pts',(20.5461442451141,-20.7621949040571,-10.2665704407376));
#55310=CARTESIAN_POINT('Ctrl Pts',(20.4857078751412,-20.8207339487951,-10.2707460049293));
#55311=CARTESIAN_POINT('Ctrl Pts',(20.4226131812577,-20.8761064222342,-10.274921569121));
#55312=CARTESIAN_POINT('Ctrl Pts',(20.3563317243795,-20.9342756276711,-10.2793080311335));
#55313=CARTESIAN_POINT('Ctrl Pts',(20.2871168004274,-20.9889496060668,-10.283694493146));
#55314=CARTESIAN_POINT('Ctrl Pts',(20.2153865821741,-21.0398442935608,-10.2880809551586));
#55315=CARTESIAN_POINT('Ctrl Pts',(20.1436563639209,-21.0907389810548,-10.2924674171711));
#55316=CARTESIAN_POINT('Ctrl Pts',(20.0694113820225,-21.1378541309858,-10.2968538791837));
#55317=CARTESIAN_POINT('Ctrl Pts',(19.9930989518198,-21.1809616034213,-10.3012403411962));
#55318=CARTESIAN_POINT('Ctrl Pts',(19.9202977696528,-21.2220856371494,-10.3054249755892));
#55319=CARTESIAN_POINT('Ctrl Pts',(19.845344231219,-21.2597157589185,-10.3096096099823));
#55320=CARTESIAN_POINT('Ctrl Pts',(19.7686077403709,-21.2936205549928,-10.3137942443753));
#55321=CARTESIAN_POINT('Ctrl Pts',(19.6919804744194,-21.3274770917864,-10.3179729224593));
#55322=CARTESIAN_POINT('Ctrl Pts',(19.6135757141378,-21.3576186510692,-10.3221516005432));
#55323=CARTESIAN_POINT('Ctrl Pts',(19.5337886464593,-21.3838589846031,-10.3263302786272));
#55324=CARTESIAN_POINT('Ctrl Pts',(19.4525714529346,-21.4105696572571,-10.3305838565126));
#55325=CARTESIAN_POINT('Ctrl Pts',(19.369922328658,-21.43323763244,-10.334837434398));
#55326=CARTESIAN_POINT('Ctrl Pts',(19.2862808103367,-21.4517171653077,-10.3390910122835));
#55327=CARTESIAN_POINT('Ctrl Pts',(19.2042608460611,-21.4698384363709,-10.3432621262614));
#55328=CARTESIAN_POINT('Ctrl Pts',(19.1212870932382,-21.4839321143086,-10.3474332402394));
#55329=CARTESIAN_POINT('Ctrl Pts',(19.0377889319356,-21.4939111480997,-10.3516043542173));
#55330=CARTESIAN_POINT('Ctrl Pts',(18.9543187892475,-21.5038868333295,-10.3557740685377));
#55331=CARTESIAN_POINT('Ctrl Pts',(18.8703250439617,-21.5097505619763,-10.3599437828581));
#55332=CARTESIAN_POINT('Ctrl Pts',(18.7862446699246,-21.5114668379302,-10.3641134971784));
#55333=CARTESIAN_POINT('Ctrl Pts',(18.702167287828,-21.5131830528116,-10.3682830631225));
#55334=CARTESIAN_POINT('Ctrl Pts',(18.6180037430636,-21.510752099899,-10.3724526290665));
#55335=CARTESIAN_POINT('Ctrl Pts',(18.5341921271335,-21.5041905912256,-10.3766221950106));
#55336=CARTESIAN_POINT('Ctrl Pts',(18.44743379818,-21.4973983880018,-10.3809383577495));
#55337=CARTESIAN_POINT('Ctrl Pts',(18.3610531319648,-21.4861798052051,-10.3852545204884));
#55338=CARTESIAN_POINT('Ctrl Pts',(18.2755295374792,-21.4706116880131,-10.3895706832273));
#55339=CARTESIAN_POINT('Ctrl Pts',(18.1927918650886,-21.4555507006011,-10.393746247419));
#55340=CARTESIAN_POINT('Ctrl Pts',(18.1108567316687,-21.4364193523527,-10.3979218116107));
#55341=CARTESIAN_POINT('Ctrl Pts',(18.0301452832767,-21.413338769399,-10.4020973758024));
#55342=CARTESIAN_POINT('Ctrl Pts',(17.9453572914997,-21.3890924410691,-10.4064838378149));
#55343=CARTESIAN_POINT('Ctrl Pts',(17.8619204024431,-21.3604876310562,-10.4108702998275));
#55344=CARTESIAN_POINT('Ctrl Pts',(17.7802998178502,-21.3277221981047,-10.41525676184));
#55345=CARTESIAN_POINT('Ctrl Pts',(17.6986792332574,-21.2949567651532,-10.4196432238525));
#55346=CARTESIAN_POINT('Ctrl Pts',(17.6188754477654,-21.258031021948,-10.4240296858651));
#55347=CARTESIAN_POINT('Ctrl Pts',(17.5413224142635,-21.2171976020828,-10.4284161478776));
#55348=CARTESIAN_POINT('Ctrl Pts',(17.4673377107943,-21.1782429883953,-10.4326007822707));
#55349=CARTESIAN_POINT('Ctrl Pts',(17.3951258047344,-21.135587395429,-10.4367854166637));
#55350=CARTESIAN_POINT('Ctrl Pts',(17.3250812297128,-21.0894161734984,-10.4409700510568));
#55351=CARTESIAN_POINT('Ctrl Pts',(17.255136354474,-21.0433106705873,-10.4451487291407));
#55352=CARTESIAN_POINT('Ctrl Pts',(17.1873530634459,-20.9936997293727,-10.4493274072247));
#55353=CARTESIAN_POINT('Ctrl Pts',(17.1221018691138,-20.940814826887,-10.4535060853086));
#55354=CARTESIAN_POINT('Ctrl Pts',(17.0556810940184,-20.8869820005319,-10.457759663194));
#55355=CARTESIAN_POINT('Ctrl Pts',(16.9918845107681,-20.8297569115571,-10.4620132410795));
#55356=CARTESIAN_POINT('Ctrl Pts',(16.9310725805954,-20.7694302518554,-10.4662668189649));
#55357=CARTESIAN_POINT('Ctrl Pts',(16.8714396083538,-20.7102731421697,-10.4704379329429));
#55358=CARTESIAN_POINT('Ctrl Pts',(16.8146769368997,-20.6481339874867,-10.4746090469208));
#55359=CARTESIAN_POINT('Ctrl Pts',(16.7610901776525,-20.5833267094255,-10.4787801608988));
#55360=CARTESIAN_POINT('Ctrl Pts',(16.70752139996,-20.5185411780723,-10.4829498752191));
#55361=CARTESIAN_POINT('Ctrl Pts',(16.6571267108674,-20.4510896556874,-10.4871195895395));
#55362=CARTESIAN_POINT('Ctrl Pts',(16.6101724826409,-20.3813203547519,-10.4912893038599));
#55363=CARTESIAN_POINT('Ctrl Pts',(16.5632199252473,-20.3115535365076,-10.4954588698039));
#55364=CARTESIAN_POINT('Ctrl Pts',(16.5197078414471,-20.2394694858256,-10.499628435748));
#55365=CARTESIAN_POINT('Ctrl Pts',(16.4798593937702,-20.1654455601081,-10.503798001692));
#55366=CARTESIAN_POINT('Ctrl Pts',(16.4386099238314,-20.0888190444807,-10.5081141644309));
#55367=CARTESIAN_POINT('Ctrl Pts',(16.4012867603007,-20.0101141681399,-10.5124303271699));
#55368=CARTESIAN_POINT('Ctrl Pts',(16.3680847835395,-19.9297756330165,-10.5167464899088));
#55369=CARTESIAN_POINT('Ctrl Pts',(16.3359643576791,-19.8520541172246,-10.5209220541005));
#55370=CARTESIAN_POINT('Ctrl Pts',(16.307700860257,-19.7728042005823,-10.5250976182921));
#55371=CARTESIAN_POINT('Ctrl Pts',(16.2834204017388,-19.6924455635533,-10.5292731824838));
#55372=CARTESIAN_POINT('Ctrl Pts',(16.257913594982,-19.6080282028025,-10.5336596444963));
#55373=CARTESIAN_POINT('Ctrl Pts',(16.236802907853,-19.522387742153,-10.5380461065089));
#55374=CARTESIAN_POINT('Ctrl Pts',(16.2201737773397,-19.4360224398369,-10.5424325685214));
#55375=CARTESIAN_POINT('Ctrl Pts',(16.2035446468265,-19.3496571375208,-10.546819030534));
#55376=CARTESIAN_POINT('Ctrl Pts',(16.1913970777482,-19.2625675787001,-10.5512054925465));
#55377=CARTESIAN_POINT('Ctrl Pts',(16.1837535357011,-19.1752553948527,-10.555591954559));
#55378=CARTESIAN_POINT('Ctrl Pts',(16.1772957565522,-19.1014881810632,-10.5592979331155));
#55379=CARTESIAN_POINT('Ctrl Pts',(16.174038011382,-19.0274367677245,-10.563003911672));
#55380=CARTESIAN_POINT('Ctrl Pts',(16.1740003306697,-18.9533011644427,-10.5667098902285));
#55381=CARTESIAN_POINT('Origin',(18.734,-18.952,1.76670989022851));
#55382=CARTESIAN_POINT('',(20.293535888361,-16.9218650751948,-9.25004024798509));
#55383=CARTESIAN_POINT('',(20.2929505583931,-16.9226084740133,-9.31680761620569));
#55384=CARTESIAN_POINT('',(20.293535888361,-16.9218650751948,1.76670989022851));
#55385=CARTESIAN_POINT('',(16.1740007840082,-18.9540035272626,-9.83329010977151));
#55386=CARTESIAN_POINT('Ctrl Pts',(20.2929505583934,-16.9226084740135,-9.31680761620571));
#55387=CARTESIAN_POINT('Ctrl Pts',(20.7827497190878,-17.3064746480848,-9.34773679031647));
#55388=CARTESIAN_POINT('Ctrl Pts',(21.6282768182897,-18.6405174171462,-9.42105789998771));
#55389=CARTESIAN_POINT('Ctrl Pts',(20.8151679945063,-21.1501879698607,-9.53677094521946));
#55390=CARTESIAN_POINT('Ctrl Pts',(18.0121685510886,-21.8917703875575,-9.66394675190086));
#55391=CARTESIAN_POINT('Ctrl Pts',(16.3483940953146,-20.372000527443,-9.76278617059769));
#55392=CARTESIAN_POINT('Ctrl Pts',(16.174290432163,-19.2372014285682,-9.81923365373404));
#55393=CARTESIAN_POINT('Ctrl Pts',(16.1763511785197,-18.9540199907297,-9.8332892013099));
#55394=CARTESIAN_POINT('Ctrl Pts',(16.1740007840082,-18.9540035272626,-9.83329010977151));
#55395=CARTESIAN_POINT('Ctrl Pts',(16.1739350379054,-18.8699966984849,-9.83745593779553));
#55396=CARTESIAN_POINT('Ctrl Pts',(16.1780086491546,-18.7859395799201,-9.84162176581955));
#55397=CARTESIAN_POINT('Ctrl Pts',(16.186209790272,-18.7022700514274,-9.84578759384357));
#55398=CARTESIAN_POINT('Ctrl Pts',(16.1944094741073,-18.6186153903909,-9.84995268163077));
#55399=CARTESIAN_POINT('Ctrl Pts',(16.2067351859308,-18.5353486407625,-9.85411776941798));
#55400=CARTESIAN_POINT('Ctrl Pts',(16.2231231591269,-18.4529033260309,-9.85828285720518));
#55401=CARTESIAN_POINT('Ctrl Pts',(16.2395131466374,-18.3704478776005,-9.86244845694076));
#55402=CARTESIAN_POINT('Ctrl Pts',(16.2599662961797,-18.2888145159801,-9.86661405667633));
#55403=CARTESIAN_POINT('Ctrl Pts',(16.284367851052,-18.2084259721855,-9.87077965641191));
#55404=CARTESIAN_POINT('Ctrl Pts',(16.308796991805,-18.127946549396,-9.87494996534484));
#55405=CARTESIAN_POINT('Ctrl Pts',(16.3371833166001,-18.0487151959129,-9.87912027427777));
#55406=CARTESIAN_POINT('Ctrl Pts',(16.3693624790262,-17.971138442795,-9.8832905832107));
#55407=CARTESIAN_POINT('Ctrl Pts',(16.4015603628991,-17.8935165564619,-9.88746331837885));
#55408=CARTESIAN_POINT('Ctrl Pts',(16.4375552801455,-17.8175516031283,-9.89163605354699));
#55409=CARTESIAN_POINT('Ctrl Pts',(16.4771361744291,-17.7436268486807,-9.89580878871514));
#55410=CARTESIAN_POINT('Ctrl Pts',(16.5167895617088,-17.6695666999467,-9.89998916630976));
#55411=CARTESIAN_POINT('Ctrl Pts',(16.5600418069661,-17.5975546086437,-9.90416954390437));
#55412=CARTESIAN_POINT('Ctrl Pts',(16.606637749578,-17.5279459787355,-9.90834992149899));
#55413=CARTESIAN_POINT('Ctrl Pts',(16.6436006876738,-17.4727278774588,-9.91166606942058));
#55414=CARTESIAN_POINT('Ctrl Pts',(16.6826668124626,-17.4190216712155,-9.91498221734216));
#55415=CARTESIAN_POINT('Ctrl Pts',(16.7236914224215,-17.3669891410737,-9.91829836526375));
#55416=CARTESIAN_POINT('Ctrl Pts',(16.7754602209958,-17.3013294900759,-9.9224829996568));
#55417=CARTESIAN_POINT('Ctrl Pts',(16.8305455538228,-17.2380865845811,-9.92666763404985));
#55418=CARTESIAN_POINT('Ctrl Pts',(16.8886933634202,-17.1776146368405,-9.93085226844289));
#55419=CARTESIAN_POINT('Ctrl Pts',(16.9467584068079,-17.1172287634326,-9.93503094652683));
#55420=CARTESIAN_POINT('Ctrl Pts',(17.0078769523774,-17.0596063422906,-9.93920962461077));
#55421=CARTESIAN_POINT('Ctrl Pts',(17.0717539579496,-17.0050695709174,-9.94338830269471));
#55422=CARTESIAN_POINT('Ctrl Pts',(17.1367759129392,-16.9495552671121,-9.94764188058015));
#55423=CARTESIAN_POINT('Ctrl Pts',(17.2046558928938,-16.897238700291,-9.95189545846559));
#55424=CARTESIAN_POINT('Ctrl Pts',(17.2750424589415,-16.8484214078413,-9.95614903635103));
#55425=CARTESIAN_POINT('Ctrl Pts',(17.3440644440582,-16.8005505338648,-9.96032015032898));
#55426=CARTESIAN_POINT('Ctrl Pts',(17.4154962970279,-16.7560447387742,-9.96449126430693));
#55427=CARTESIAN_POINT('Ctrl Pts',(17.4889737195061,-16.7151473984906,-9.96866237828488));
#55428=CARTESIAN_POINT('Ctrl Pts',(17.5624264859256,-16.6742637817044,-9.97283209260526));
#55429=CARTESIAN_POINT('Ctrl Pts',(17.6379230570026,-16.6369864384996,-9.97700180692564));
#55430=CARTESIAN_POINT('Ctrl Pts',(17.7150725574695,-16.6035139202332,-9.98117152124602));
#55431=CARTESIAN_POINT('Ctrl Pts',(17.7922193126262,-16.5700425930627,-9.98534108719006));
#55432=CARTESIAN_POINT('Ctrl Pts',(17.8710184578639,-16.5403760039564,-9.98951065313411));
#55433=CARTESIAN_POINT('Ctrl Pts',(17.9510583236146,-16.5146649119625,-9.99368021907816));
#55434=CARTESIAN_POINT('Ctrl Pts',(18.0339122923051,-16.4880498496922,-9.99799638181708));
#55435=CARTESIAN_POINT('Ctrl Pts',(18.1180953501449,-16.4656737716515,-10.002312544556));
#55436=CARTESIAN_POINT('Ctrl Pts',(18.2031347548814,-16.4476473707712,-10.0066287072949));
#55437=CARTESIAN_POINT('Ctrl Pts',(18.2854040099531,-16.4302081780035,-10.0108042714866));
#55438=CARTESIAN_POINT('Ctrl Pts',(18.3684742051326,-16.4168396609884,-10.0149798356783));
#55439=CARTESIAN_POINT('Ctrl Pts',(18.4519097174451,-16.4075894449818,-10.01915539987));
#55440=CARTESIAN_POINT('Ctrl Pts',(18.5395593591353,-16.397872022555,-10.0235418618825));
#55441=CARTESIAN_POINT('Ctrl Pts',(18.6276116092813,-16.3926998996315,-10.027928323895));
#55442=CARTESIAN_POINT('Ctrl Pts',(18.7155609817199,-16.3920664066025,-10.0323147859076));
#55443=CARTESIAN_POINT('Ctrl Pts',(18.8035103541586,-16.3914329135735,-10.0367012479201));
#55444=CARTESIAN_POINT('Ctrl Pts',(18.8913562726232,-16.395337948682,-10.0410877099327));
#55445=CARTESIAN_POINT('Ctrl Pts',(18.9786013944251,-16.403712308658,-10.0454741719452));
#55446=CARTESIAN_POINT('Ctrl Pts',(19.0618259169023,-16.4117007450961,-10.0496584884871));
#55447=CARTESIAN_POINT('Ctrl Pts',(19.1448135519499,-16.4237853774933,-10.0538428050291));
#55448=CARTESIAN_POINT('Ctrl Pts',(19.2271290458148,-16.4399443190539,-10.058027121571));
#55449=CARTESIAN_POINT('Ctrl Pts',(19.3093328037822,-16.4560813263011,-10.0622057582786));
#55450=CARTESIAN_POINT('Ctrl Pts',(19.3908657848188,-16.476281573038,-10.0663843949863));
#55451=CARTESIAN_POINT('Ctrl Pts',(19.4712973833537,-16.5004713812603,-10.0705630316939));
#55452=CARTESIAN_POINT('Ctrl Pts',(19.5516353626652,-16.5246330334953,-10.0747368046325));
#55453=CARTESIAN_POINT('Ctrl Pts',(19.6308740694797,-16.5527748851346,-10.078910577571));
#55454=CARTESIAN_POINT('Ctrl Pts',(19.7085941104905,-16.5847724402168,-10.0830843505096));
#55455=CARTESIAN_POINT('Ctrl Pts',(19.7862608039805,-16.6167480319776,-10.0872552585443));
#55456=CARTESIAN_POINT('Ctrl Pts',(19.8624104781156,-16.6525738957064,-10.0914261665791));
#55457=CARTESIAN_POINT('Ctrl Pts',(19.9366409846827,-16.6920764035124,-10.0955970746139));
#55458=CARTESIAN_POINT('Ctrl Pts',(20.0108540887567,-16.7315696504074,-10.099767004827));
#55459=CARTESIAN_POINT('Ctrl Pts',(20.0831485098601,-16.7747376197254,-10.1039369350401));
#55460=CARTESIAN_POINT('Ctrl Pts',(20.153145166604,-16.8213599562328,-10.1081068652532));
#55461=CARTESIAN_POINT('Ctrl Pts',(20.2010560885864,-16.8532717536092,-10.1109610758742));
#55462=CARTESIAN_POINT('Ctrl Pts',(20.2478909735988,-16.8868009610696,-10.1138152864951));
#55463=CARTESIAN_POINT('Ctrl Pts',(20.293535888361,-16.9218650751947,-10.1166694971161));
#55464=CARTESIAN_POINT('',(16.1740010233873,-18.9497109517325,-9.7667098901893));
#55465=CARTESIAN_POINT('Ctrl Pts',(16.174001023388,-18.9497109509451,-9.76670989022852));
#55466=CARTESIAN_POINT('Ctrl Pts',(16.1741079389015,-18.8301400729777,-9.7726651119283));
#55467=CARTESIAN_POINT('Ctrl Pts',(16.18259555166,-18.7109297707787,-9.77862033362807));
#55468=CARTESIAN_POINT('Ctrl Pts',(16.1992930219765,-18.5930285031387,-9.78457555532785));
#55469=CARTESIAN_POINT('Ctrl Pts',(16.2067339930636,-18.5404876147875,-9.78722940837539));
#55470=CARTESIAN_POINT('Ctrl Pts',(16.2158047738385,-18.4882062515533,-9.78988326142292));
#55471=CARTESIAN_POINT('Ctrl Pts',(16.2264874578014,-18.4362666864388,-9.79253711447045));
#55472=CARTESIAN_POINT('Ctrl Pts',(16.2433320704913,-18.3543676186888,-9.7967217488635));
#55473=CARTESIAN_POINT('Ctrl Pts',(16.2642246666771,-18.2731422629635,-9.80090638325655));
#55474=CARTESIAN_POINT('Ctrl Pts',(16.2890969179466,-18.193021133782,-9.80509101764959));
#55475=CARTESIAN_POINT('Ctrl Pts',(16.3139337666449,-18.1130140471109,-9.80926969573354));
#55476=CARTESIAN_POINT('Ctrl Pts',(16.3427388836329,-18.0341085006258,-9.81344837381748));
#55477=CARTESIAN_POINT('Ctrl Pts',(16.3753929533287,-17.9567247619916,-9.81762705190143));
#55478=CARTESIAN_POINT('Ctrl Pts',(16.4086323237558,-17.8779539754572,-9.82188062978686));
#55479=CARTESIAN_POINT('Ctrl Pts',(16.4458598919279,-17.8007605624573,-9.8261342076723));
#55480=CARTESIAN_POINT('Ctrl Pts',(16.4868966678982,-17.7255716022299,-9.83038778555773));
#55481=CARTESIAN_POINT('Ctrl Pts',(16.5271378658896,-17.6518403267158,-9.83455889953568));
#55482=CARTESIAN_POINT('Ctrl Pts',(16.5710416613175,-17.5800368994831,-9.83873001351364));
#55483=CARTESIAN_POINT('Ctrl Pts',(16.618391498167,-17.5105421730166,-9.8429011274916));
#55484=CARTESIAN_POINT('Ctrl Pts',(16.6657254463214,-17.4410707661768,-9.84707084181197));
#55485=CARTESIAN_POINT('Ctrl Pts',(16.7165028805482,-17.3739069013823,-9.85124055613234));
#55486=CARTESIAN_POINT('Ctrl Pts',(16.7704633948898,-17.3094032751791,-9.85541027045272));
#55487=CARTESIAN_POINT('Ctrl Pts',(16.8244219890848,-17.2449019442917,-9.85957983639676));
#55488=CARTESIAN_POINT('Ctrl Pts',(16.8815631423607,-17.1830610160833,-9.86374940234081));
#55489=CARTESIAN_POINT('Ctrl Pts',(16.9415864376593,-17.1241997862083,-9.86791896828485));
#55490=CARTESIAN_POINT('Ctrl Pts',(17.0037200779738,-17.0632690681041,-9.87223513102377));
#55491=CARTESIAN_POINT('Ctrl Pts',(17.0689419268744,-17.0055318485509,-9.87655129376269));
#55492=CARTESIAN_POINT('Ctrl Pts',(17.1368790142893,-16.9512989836053,-9.88086745650161));
#55493=CARTESIAN_POINT('Ctrl Pts',(17.2026030582275,-16.8988327485311,-9.88504302069329));
#55494=CARTESIAN_POINT('Ctrl Pts',(17.2708677497022,-16.8496463025101,-9.88921858488496));
#55495=CARTESIAN_POINT('Ctrl Pts',(17.3413050297814,-16.8039774861683,-9.89339414907664));
#55496=CARTESIAN_POINT('Ctrl Pts',(17.4152999294287,-16.7560020464804,-9.89778061108918));
#55497=CARTESIAN_POINT('Ctrl Pts',(17.4916921547951,-16.7119092180967,-9.90216707310172));
#55498=CARTESIAN_POINT('Ctrl Pts',(17.5700268579948,-16.6719196231952,-9.90655353511426));
#55499=CARTESIAN_POINT('Ctrl Pts',(17.6483615611944,-16.6319300282936,-9.91093999712679));
#55500=CARTESIAN_POINT('Ctrl Pts',(17.7286381814853,-16.5960438342244,-9.91532645913933));
#55501=CARTESIAN_POINT('Ctrl Pts',(17.8103811197834,-16.5644221134993,-9.91971292115187));
#55502=CARTESIAN_POINT('Ctrl Pts',(17.8883629443183,-16.5342553550193,-9.92389755554492));
#55503=CARTESIAN_POINT('Ctrl Pts',(17.967969380348,-16.5078569775931,-9.92808218993797));
#55504=CARTESIAN_POINT('Ctrl Pts',(18.0488014484187,-16.4854025571831,-9.93226682433102));
#55505=CARTESIAN_POINT('Ctrl Pts',(18.1295184620454,-16.4629800978612,-9.93644550241496));
#55506=CARTESIAN_POINT('Ctrl Pts',(18.2114572030593,-16.4444905669892,-9.9406241804989));
#55507=CARTESIAN_POINT('Ctrl Pts',(18.2941997096014,-16.4300611219609,-9.94480285858285));
#55508=CARTESIAN_POINT('Ctrl Pts',(18.3784253161073,-16.4153730395006,-9.94905643646828));
#55509=CARTESIAN_POINT('Ctrl Pts',(18.4634833368927,-16.404892202575,-9.95331001435371));
#55510=CARTESIAN_POINT('Ctrl Pts',(18.5489177820416,-16.3986992788558,-9.95756359223915));
#55511=CARTESIAN_POINT('Ctrl Pts',(18.6326959137598,-16.3926264170474,-9.9617347062171));
#55512=CARTESIAN_POINT('Ctrl Pts',(18.7168355246874,-16.3906767277746,-9.96590582019505));
#55513=CARTESIAN_POINT('Ctrl Pts',(18.8008991604927,-16.3928742699263,-9.97007693417301));
#55514=CARTESIAN_POINT('Ctrl Pts',(18.8849345879332,-16.3950710746715,-9.97424664849338));
#55515=CARTESIAN_POINT('Ctrl Pts',(18.96889363139,-16.4014123350032,-9.97841636281375));
#55516=CARTESIAN_POINT('Ctrl Pts',(19.0523387760777,-16.4118699986722,-9.98258607713412));
#55517=CARTESIAN_POINT('Ctrl Pts',(19.1357809514291,-16.4223272902127,-9.98675564307817));
#55518=CARTESIAN_POINT('Ctrl Pts',(19.2187088080139,-16.4369006358009,-9.99092520902221));
#55519=CARTESIAN_POINT('Ctrl Pts',(19.3006912586604,-16.4555102609148,-9.99509477496626));
#55520=CARTESIAN_POINT('Ctrl Pts',(19.3855561111354,-16.4747741774902,-9.99941093770518));
#55521=CARTESIAN_POINT('Ctrl Pts',(19.4694073254463,-16.498363368963,-10.0037271004441));
#55522=CARTESIAN_POINT('Ctrl Pts',(19.5517816392175,-16.5261324870145,-10.008043263183));
#55523=CARTESIAN_POINT('Ctrl Pts',(19.6314726183819,-16.5529970289662,-10.0122188273747));
#55524=CARTESIAN_POINT('Ctrl Pts',(19.7097810183148,-16.5837731410383,-10.0163943915664));
#55525=CARTESIAN_POINT('Ctrl Pts',(19.7863076293696,-16.6182800825355,-10.0205699557581));
#55526=CARTESIAN_POINT('Ctrl Pts',(19.866699417624,-16.6545298876152,-10.0249564177706));
#55527=CARTESIAN_POINT('Ctrl Pts',(19.9451241711511,-16.6948970480992,-10.0293428797831));
#55528=CARTESIAN_POINT('Ctrl Pts',(20.0211501810795,-16.739118527497,-10.0337293417957));
#55529=CARTESIAN_POINT('Ctrl Pts',(20.097176191008,-16.7833400068949,-10.0381158038082));
#55530=CARTESIAN_POINT('Ctrl Pts',(20.1708030131039,-16.8314154242948,-10.0425022658208));
#55531=CARTESIAN_POINT('Ctrl Pts',(20.2416377781113,-16.8830320616279,-10.0468887278333));
#55532=CARTESIAN_POINT('Ctrl Pts',(20.2590918819294,-16.8957507054557,-10.0479695779407));
#55533=CARTESIAN_POINT('Ctrl Pts',(20.2763933942624,-16.9086963274252,-10.049050428048));
#55534=CARTESIAN_POINT('Ctrl Pts',(20.293535888361,-16.9218650751948,-10.0501312781553));
#55535=CARTESIAN_POINT('Ctrl Pts',(20.293535888361,-16.9218650751948,-9.2500402479851));
#55536=CARTESIAN_POINT('Ctrl Pts',(20.3602016707525,-16.9730772773468,-9.25421688807687));
#55537=CARTESIAN_POINT('Ctrl Pts',(20.4242843944649,-17.0275322155205,-9.25839352816864));
#55538=CARTESIAN_POINT('Ctrl Pts',(20.4854677358751,-17.0849272188293,-9.26257016826041));
#55539=CARTESIAN_POINT('Ctrl Pts',(20.5467562454808,-17.1424208785499,-9.26675398758907));
#55540=CARTESIAN_POINT('Ctrl Pts',(20.6051351000148,-17.2028643650392,-9.27093780691774));
#55541=CARTESIAN_POINT('Ctrl Pts',(20.660326284079,-17.2659196201644,-9.2751216262464));
#55542=CARTESIAN_POINT('Ctrl Pts',(20.6986357799563,-17.3096877522896,-9.2780257134125));
#55543=CARTESIAN_POINT('Ctrl Pts',(20.735410269639,-17.3547135411918,-9.2809298005786));
#55544=CARTESIAN_POINT('Ctrl Pts',(20.7705691100608,-17.4008758076974,-9.2838338877447));
#55545=CARTESIAN_POINT('Ctrl Pts',(20.8212311199914,-17.4673931665203,-9.28801852213775));
#55546=CARTESIAN_POINT('Ctrl Pts',(20.8687251499199,-17.5365189656784,-9.2922031565308));
#55547=CARTESIAN_POINT('Ctrl Pts',(20.9127716012343,-17.6079187860643,-9.29638779092385));
#55548=CARTESIAN_POINT('Ctrl Pts',(20.9567553578771,-17.6792169776433,-9.30056646900779));
#55549=CARTESIAN_POINT('Ctrl Pts',(20.9973010436861,-17.7527823729939,-9.30474514709174));
#55550=CARTESIAN_POINT('Ctrl Pts',(21.0341702903065,-17.8282488551323,-9.30892382517568));
#55551=CARTESIAN_POINT('Ctrl Pts',(21.0717003916751,-17.9050680197263,-9.31317740306112));
#55552=CARTESIAN_POINT('Ctrl Pts',(21.1054206649962,-17.98385671187,-9.31743098094655));
#55553=CARTESIAN_POINT('Ctrl Pts',(21.1351268232139,-18.0641993586154,-9.32168455883198));
#55554=CARTESIAN_POINT('Ctrl Pts',(21.1642570695877,-18.1429844063778,-9.32585567280993));
#55555=CARTESIAN_POINT('Ctrl Pts',(21.1895272879509,-18.223263242189,-9.33002678678789));
#55556=CARTESIAN_POINT('Ctrl Pts',(21.2107927216344,-18.3046223559168,-9.33419790076584));
#55557=CARTESIAN_POINT('Ctrl Pts',(21.2320510194963,-18.3859541688082,-9.33836761508621));
#55558=CARTESIAN_POINT('Ctrl Pts',(21.2493070853372,-18.4683650949799,-9.34253732940659));
#55559=CARTESIAN_POINT('Ctrl Pts',(21.2624662014641,-18.5514270752364,-9.34670704372696));
#55560=CARTESIAN_POINT('Ctrl Pts',(21.2756248493332,-18.6344860997912,-9.350876609671));
#55561=CARTESIAN_POINT('Ctrl Pts',(21.284686766209,-18.7181956778687,-9.35504617561505));
#55562=CARTESIAN_POINT('Ctrl Pts',(21.2896087040397,-18.8021195415124,-9.35921574155909));
#55563=CARTESIAN_POINT('Ctrl Pts',(21.2947036911327,-18.8889940646705,-9.36353190429801));
#55564=CARTESIAN_POINT('Ctrl Pts',(21.2953621283496,-18.9760976958014,-9.36784806703693));
#55565=CARTESIAN_POINT('Ctrl Pts',(21.2915948078576,-19.0629450261169,-9.37216422977585));
#55566=CARTESIAN_POINT('Ctrl Pts',(21.2879502074343,-19.1469633137822,-9.37633979396753));
#55567=CARTESIAN_POINT('Ctrl Pts',(21.2801638500694,-19.2307412775515,-9.38051535815922));
#55568=CARTESIAN_POINT('Ctrl Pts',(21.2682983360669,-19.313845193154,-9.3846909223509));
#55569=CARTESIAN_POINT('Ctrl Pts',(21.2558335231597,-19.4011464899728,-9.38907738436344));
#55570=CARTESIAN_POINT('Ctrl Pts',(21.2388667599596,-19.487703283801,-9.39346384637597));
#55571=CARTESIAN_POINT('Ctrl Pts',(21.2175306593405,-19.5730277482655,-9.39785030838851));
#55572=CARTESIAN_POINT('Ctrl Pts',(21.1961945587214,-19.6583522127299,-9.40223677040106));
#55573=CARTESIAN_POINT('Ctrl Pts',(21.1704893630394,-19.7424438151945,-9.4066232324136));
#55574=CARTESIAN_POINT('Ctrl Pts',(21.1406062076889,-19.8248382216158,-9.41100969442614));
#55575=CARTESIAN_POINT('Ctrl Pts',(21.1120980206135,-19.9034415392599,-9.41519432881918));
#55576=CARTESIAN_POINT('Ctrl Pts',(21.0796817805212,-19.9807929863463,-9.41937896321223));
#55577=CARTESIAN_POINT('Ctrl Pts',(21.0434873395327,-20.0564764499699,-9.42356359760528));
#55578=CARTESIAN_POINT('Ctrl Pts',(21.007344416851,-20.1320521875507,-9.42774227568923));
#55579=CARTESIAN_POINT('Ctrl Pts',(20.967434172056,-20.2059642460473,-9.43192095377317));
#55580=CARTESIAN_POINT('Ctrl Pts',(20.9239354273224,-20.2778140232168,-9.43609963185711));
#55581=CARTESIAN_POINT('Ctrl Pts',(20.8796569988514,-20.3509516560045,-9.44035320974255));
#55582=CARTESIAN_POINT('Ctrl Pts',(20.8316603217325,-20.4219518942303,-9.44460678762799));
#55583=CARTESIAN_POINT('Ctrl Pts',(20.7801842503405,-20.4904180230543,-9.44886036551342));
#55584=CARTESIAN_POINT('Ctrl Pts',(20.7297061430398,-20.5575568023704,-9.45303147949137));
#55585=CARTESIAN_POINT('Ctrl Pts',(20.6758826364362,-20.6222584681312,-9.45720259346932));
#55586=CARTESIAN_POINT('Ctrl Pts',(20.6189830730721,-20.6841774776944,-9.46137370744728));
#55587=CARTESIAN_POINT('Ctrl Pts',(20.562102602906,-20.746075709736,-9.46554342176765));
#55588=CARTESIAN_POINT('Ctrl Pts',(20.5021484369599,-20.8051928015664,-9.46971313608802));
#55589=CARTESIAN_POINT('Ctrl Pts',(20.4394292363847,-20.8612174102717,-9.47388285040839));
#55590=CARTESIAN_POINT('Ctrl Pts',(20.3767122676277,-20.9172400253809,-9.47805241635244));
#55591=CARTESIAN_POINT('Ctrl Pts',(20.3112308035245,-20.9701700703296,-9.48222198229648));
#55592=CARTESIAN_POINT('Ctrl Pts',(20.2433282670354,-21.0197350367801,-9.48639154824052));
#55593=CARTESIAN_POINT('Ctrl Pts',(20.1730383611302,-21.0710426463059,-9.49070771097945));
#55594=CARTESIAN_POINT('Ctrl Pts',(20.1001543913748,-21.1187438312855,-9.49502387371837));
#55595=CARTESIAN_POINT('Ctrl Pts',(20.0250903513379,-21.162584923653,-9.49934003645729));
#55596=CARTESIAN_POINT('Ctrl Pts',(19.9524715145099,-21.2049978970479,-9.50351560064897));
#55597=CARTESIAN_POINT('Ctrl Pts',(19.8778128975685,-21.2437982255353,-9.50769116484065));
#55598=CARTESIAN_POINT('Ctrl Pts',(19.8015130783443,-21.2788037793428,-9.51186672903233));
#55599=CARTESIAN_POINT('Ctrl Pts',(19.7213595366366,-21.3155773804553,-9.51625319104487));
#55600=CARTESIAN_POINT('Ctrl Pts',(19.6393951838166,-21.3481625684723,-9.52063965305741));
#55601=CARTESIAN_POINT('Ctrl Pts',(19.5561019854972,-21.3764067986709,-9.52502611506995));
#55602=CARTESIAN_POINT('Ctrl Pts',(19.4728087871779,-21.4046510288695,-9.5294125770825));
#55603=CARTESIAN_POINT('Ctrl Pts',(19.3881873224047,-21.428554216727,-9.53379903909504));
#55604=CARTESIAN_POINT('Ctrl Pts',(19.3027314805895,-21.4480257416514,-9.53818550110758));
#55605=CARTESIAN_POINT('Ctrl Pts',(19.2212075887321,-21.4666013528504,-9.54237013550063));
#55606=CARTESIAN_POINT('Ctrl Pts',(19.1386209669249,-21.4812132961356,-9.54655476989367));
#55607=CARTESIAN_POINT('Ctrl Pts',(19.0553917867601,-21.4917455225678,-9.55073940428672));
#55608=CARTESIAN_POINT('Ctrl Pts',(18.9722810730316,-21.5022627576793,-9.55491808237067));
#55609=CARTESIAN_POINT('Ctrl Pts',(18.8885300701229,-21.508711753151,-9.55909676045461));
#55610=CARTESIAN_POINT('Ctrl Pts',(18.8045707324918,-21.5110271142986,-9.56327543853855));
#55611=CARTESIAN_POINT('Ctrl Pts',(18.7191064840742,-21.5133839766308,-9.56752901642399));
#55612=CARTESIAN_POINT('Ctrl Pts',(18.6334268287621,-21.5114574491382,-9.57178259430942));
#55613=CARTESIAN_POINT('Ctrl Pts',(18.5479946282973,-21.5052336363321,-9.57603617219486));
#55614=CARTESIAN_POINT('Ctrl Pts',(18.4642186977458,-21.499130484282,-9.58020728617281));
#55615=CARTESIAN_POINT('Ctrl Pts',(18.3806811928206,-21.4888952174951,-9.58437840015076));
#55616=CARTESIAN_POINT('Ctrl Pts',(18.2978184502102,-21.4745672747467,-9.58854951412871));
#55617=CARTESIAN_POINT('Ctrl Pts',(18.2149835129934,-21.4602441398778,-9.59271922844908));
#55618=CARTESIAN_POINT('Ctrl Pts',(18.1328233413407,-21.4418311348332,-9.59688894276945));
#55619=CARTESIAN_POINT('Ctrl Pts',(18.0517667977985,-21.4194192707795,-9.60105865708982));
#55620=CARTESIAN_POINT('Ctrl Pts',(17.9707131385959,-21.3970082042361,-9.60522822303387));
#55621=CARTESIAN_POINT('Ctrl Pts',(17.8907634725904,-21.3705986850247,-9.60939778897791));
#55622=CARTESIAN_POINT('Ctrl Pts',(17.8123328245034,-21.3403319739124,-9.61356735492196));
#55623=CARTESIAN_POINT('Ctrl Pts',(17.7311446515844,-21.3090011225754,-9.61788351766088));
#55624=CARTESIAN_POINT('Ctrl Pts',(17.651584793418,-21.2735369848544,-9.6221996803998));
#55625=CARTESIAN_POINT('Ctrl Pts',(17.5740906315704,-21.2341503581117,-9.62651584313872));
#55626=CARTESIAN_POINT('Ctrl Pts',(17.499120833894,-21.1960467465924,-9.6306914073304));
#55627=CARTESIAN_POINT('Ctrl Pts',(17.4260846045835,-21.1542725466308,-9.63486697152208));
#55628=CARTESIAN_POINT('Ctrl Pts',(17.3553508285749,-21.1090643157145,-9.63904253571376));
#55629=CARTESIAN_POINT('Ctrl Pts',(17.2810444576936,-21.061572724527,-9.6434289977263));
#55630=CARTESIAN_POINT('Ctrl Pts',(17.2092797216846,-21.010291419192,-9.64781545973884));
#55631=CARTESIAN_POINT('Ctrl Pts',(17.1404457653641,-20.9555430869522,-9.65220192175138));
#55632=CARTESIAN_POINT('Ctrl Pts',(17.0716118090436,-20.9007947547124,-9.65658838376392));
#55633=CARTESIAN_POINT('Ctrl Pts',(17.0057090169082,-20.8425798367027,-9.66097484577646));
#55634=CARTESIAN_POINT('Ctrl Pts',(16.9430809195061,-20.7812645645512,-9.665361307789));
#55635=CARTESIAN_POINT('Ctrl Pts',(16.8827886985014,-20.7222362035939,-9.66958416538901));
#55636=CARTESIAN_POINT('Ctrl Pts',(16.8252872091303,-20.6600954577447,-9.67380702298902));
#55637=CARTESIAN_POINT('Ctrl Pts',(16.7709203169311,-20.5951427685755,-9.67802988058904));
#55638=CARTESIAN_POINT('Ctrl Pts',(16.7179063153622,-20.5318063918538,-9.68214765466763));
#55639=CARTESIAN_POINT('Ctrl Pts',(16.6678730797622,-20.4657967543979,-9.68626542874624));
#55640=CARTESIAN_POINT('Ctrl Pts',(16.6211045875939,-20.3974317611818,-9.69038320282483));
#55641=CARTESIAN_POINT('Ctrl Pts',(16.57438033231,-20.329131432319,-9.69449708202704));
#55642=CARTESIAN_POINT('Ctrl Pts',(16.530914960773,-20.2584805564846,-9.69861096122925));
#55643=CARTESIAN_POINT('Ctrl Pts',(16.4909521572678,-20.1858299620347,-9.70272484043146));
#55644=CARTESIAN_POINT('Ctrl Pts',(16.4510143565681,-20.11322482157,-9.70683614577718));
#55645=CARTESIAN_POINT('Ctrl Pts',(16.4145750025456,-20.0386228602468,-9.71094745112289));
#55646=CARTESIAN_POINT('Ctrl Pts',(16.3818335581792,-19.9624024099199,-9.71505875646861));
#55647=CARTESIAN_POINT('Ctrl Pts',(16.3475554603697,-19.8826047069797,-9.719363017612));
#55648=CARTESIAN_POINT('Ctrl Pts',(16.3173311789842,-19.8010333411257,-9.72366727875539));
#55649=CARTESIAN_POINT('Ctrl Pts',(16.2913340385439,-19.718148158481,-9.72797153989879));
#55650=CARTESIAN_POINT('Ctrl Pts',(16.2665001036005,-19.6389715567965,-9.73208321292913));
#55651=CARTESIAN_POINT('Ctrl Pts',(16.245523244682,-19.5585966865051,-9.73619488595948));
#55652=CARTESIAN_POINT('Ctrl Pts',(16.2285034541843,-19.4774398718271,-9.74030655898983));
#55653=CARTESIAN_POINT('Ctrl Pts',(16.2114791195104,-19.3962613887933,-9.74441932981084));
#55654=CARTESIAN_POINT('Ctrl Pts',(16.1984140354436,-19.3143010135803,-9.74853210063185));
#55655=CARTESIAN_POINT('Ctrl Pts',(16.1893567554131,-19.2319834955465,-9.75264487145287));
#55656=CARTESIAN_POINT('Ctrl Pts',(16.1802905487374,-19.1495848472745,-9.75676169572549));
#55657=CARTESIAN_POINT('Ctrl Pts',(16.1752400549859,-19.0668288268568,-9.76087851999812));
#55658=CARTESIAN_POINT('Ctrl Pts',(16.1742017924823,-18.9841424452887,-9.76499534427075));
#55659=CARTESIAN_POINT('Ctrl Pts',(16.1740576564023,-18.9726635650768,-9.76556685957694));
#55660=CARTESIAN_POINT('Ctrl Pts',(16.1739907628404,-18.9611860219109,-9.76613837488311));
#55661=CARTESIAN_POINT('Ctrl Pts',(16.1740010233873,-18.9497109517325,-9.7667098901893));
#55662=CARTESIAN_POINT('Origin',(18.734,-18.952,1.76670989022851));
#55663=CARTESIAN_POINT('',(20.293535888361,-16.9218650751948,-8.45013430445441));
#55664=CARTESIAN_POINT('',(20.293535888361,-16.9218650751948,-8.5166771521069));
#55665=CARTESIAN_POINT('',(20.293535888361,-16.9218650751948,1.76670989022851));
#55666=CARTESIAN_POINT('',(16.1736699172806,-18.9526425113319,-9.03329016588271));
#55667=CARTESIAN_POINT('Ctrl Pts',(20.293535888361,-16.9218650751948,-8.5166771521069));
#55668=CARTESIAN_POINT('Ctrl Pts',(20.3077409125195,-16.9327772784673,-8.51757293199392));
#55669=CARTESIAN_POINT('Ctrl Pts',(20.3218260021905,-16.9438344322647,-8.51846871188095));
#55670=CARTESIAN_POINT('Ctrl Pts',(20.3357880909559,-16.9550335727229,-8.51936449176797));
#55671=CARTESIAN_POINT('Ctrl Pts',(20.4010119675945,-17.0073503405056,-8.52354912616102));
#55672=CARTESIAN_POINT('Ctrl Pts',(20.4637914133142,-17.0629632902855,-8.52773376055407));
#55673=CARTESIAN_POINT('Ctrl Pts',(20.5237743555655,-17.1216154075823,-8.53191839494712));
#55674=CARTESIAN_POINT('Ctrl Pts',(20.5836719195229,-17.1801840408498,-8.53609707303107));
#55675=CARTESIAN_POINT('Ctrl Pts',(20.6407805603835,-17.2417829302056,-8.54027575111501));
#55676=CARTESIAN_POINT('Ctrl Pts',(20.6947805623985,-17.3061143459765,-8.54445442919896));
#55677=CARTESIAN_POINT('Ctrl Pts',(20.7497484756404,-17.3715988561409,-8.54870800708439));
#55678=CARTESIAN_POINT('Ctrl Pts',(20.8014948330692,-17.4399145156592,-8.55296158496982));
#55679=CARTESIAN_POINT('Ctrl Pts',(20.8497210505507,-17.5107073731346,-8.55721516285526));
#55680=CARTESIAN_POINT('Ctrl Pts',(20.8970123087006,-17.580127772927,-8.56138627683321));
#55681=CARTESIAN_POINT('Ctrl Pts',(20.9409184275292,-17.6519297794779,-8.56555739081116));
#55682=CARTESIAN_POINT('Ctrl Pts',(20.9811990900048,-17.7257470693688,-8.56972850478912));
#55683=CARTESIAN_POINT('Ctrl Pts',(21.0214662359151,-17.7995395891552,-8.57389821910949));
#55684=CARTESIAN_POINT('Ctrl Pts',(21.0581101213991,-17.8753456457564,-8.57806793342987));
#55685=CARTESIAN_POINT('Ctrl Pts',(21.0909354749526,-17.9527727150892,-8.58223764775024));
#55686=CARTESIAN_POINT('Ctrl Pts',(21.1237596604391,-18.0301970292346,-8.58640721369428));
#55687=CARTESIAN_POINT('Ctrl Pts',(21.152765405382,-18.109241817549,-8.59057677963833));
#55688=CARTESIAN_POINT('Ctrl Pts',(21.1778054030265,-18.1894941625544,-8.59474634558237));
#55689=CARTESIAN_POINT('Ctrl Pts',(21.2037257760979,-18.2725680810081,-8.59906250832129));
#55690=CARTESIAN_POINT('Ctrl Pts',(21.2253961847597,-18.3569355479855,-8.60337867106021));
#55691=CARTESIAN_POINT('Ctrl Pts',(21.2427098983461,-18.4421229109478,-8.60769483379913));
#55692=CARTESIAN_POINT('Ctrl Pts',(21.2594596195335,-18.5245353045218,-8.61187039799081));
#55693=CARTESIAN_POINT('Ctrl Pts',(21.2721321012069,-18.60771452538,-8.61604596218248));
#55694=CARTESIAN_POINT('Ctrl Pts',(21.2806833673555,-18.6912245670413,-8.62022152637416));
#55695=CARTESIAN_POINT('Ctrl Pts',(21.2896665376286,-18.7789525023806,-8.6246079883867));
#55696=CARTESIAN_POINT('Ctrl Pts',(21.2941011966021,-18.8670449731774,-8.62899445039924));
#55697=CARTESIAN_POINT('Ctrl Pts',(21.2939982462078,-18.9549965668355,-8.63338091241178));
#55698=CARTESIAN_POINT('Ctrl Pts',(21.2938952958136,-19.0429481604935,-8.63776737442432));
#55699=CARTESIAN_POINT('Ctrl Pts',(21.2892548426303,-19.1307583016183,-8.64215383643686));
#55700=CARTESIAN_POINT('Ctrl Pts',(21.2801502518719,-19.2179302444115,-8.6465402984494));
#55701=CARTESIAN_POINT('Ctrl Pts',(21.2714645768305,-19.301091276897,-8.65072493284245));
#55702=CARTESIAN_POINT('Ctrl Pts',(21.2586842102674,-19.3839810906174,-8.65490956723549));
#55703=CARTESIAN_POINT('Ctrl Pts',(21.2418346904937,-19.4661645312117,-8.65909420162854));
#55704=CARTESIAN_POINT('Ctrl Pts',(21.2250091539259,-19.5482309938506,-8.66327287971248));
#55705=CARTESIAN_POINT('Ctrl Pts',(21.2041260603601,-19.6295926336689,-8.66745155779643));
#55706=CARTESIAN_POINT('Ctrl Pts',(21.1792626972637,-19.7098194648929,-8.67163023588037));
#55707=CARTESIAN_POINT('Ctrl Pts',(21.1539536762528,-19.7914843044085,-8.6758838137658));
#55708=CARTESIAN_POINT('Ctrl Pts',(21.1245203396143,-19.8719727727559,-8.68013739165124));
#55709=CARTESIAN_POINT('Ctrl Pts',(21.0910986865303,-19.9508422207522,-8.68439096953668));
#55710=CARTESIAN_POINT('Ctrl Pts',(21.0583249774083,-20.028182630598,-8.68856208351463));
#55711=CARTESIAN_POINT('Ctrl Pts',(21.0217164021894,-20.1039657925521,-8.69273319749258));
#55712=CARTESIAN_POINT('Ctrl Pts',(20.9814509018454,-20.1777913541034,-8.69690431147053));
#55713=CARTESIAN_POINT('Ctrl Pts',(20.9411989129789,-20.2515921427745,-8.70107402579091));
#55714=CARTESIAN_POINT('Ctrl Pts',(20.897292656152,-20.3234362321085,-8.70524374011128));
#55715=CARTESIAN_POINT('Ctrl Pts',(20.849956485239,-20.3929469638315,-8.70941345443165));
#55716=CARTESIAN_POINT('Ctrl Pts',(20.80262199875,-20.4624552220643,-8.7135830203757));
#55717=CARTESIAN_POINT('Ctrl Pts',(20.7518581004867,-20.5296299080143,-8.71775258631974));
#55718=CARTESIAN_POINT('Ctrl Pts',(20.6979322543499,-20.594123655613,-8.72192215226378));
#55719=CARTESIAN_POINT('Ctrl Pts',(20.6421104419878,-20.6608849238157,-8.7262383150027));
#55720=CARTESIAN_POINT('Ctrl Pts',(20.5829005348977,-20.7247728178031,-8.73055447774162));
#55721=CARTESIAN_POINT('Ctrl Pts',(20.5206430286226,-20.7854412148401,-8.73487064048054));
#55722=CARTESIAN_POINT('Ctrl Pts',(20.4604135540661,-20.8441333452248,-8.73904620467222));
#55723=CARTESIAN_POINT('Ctrl Pts',(20.3973323666986,-20.8998122314802,-8.7432217688639));
#55724=CARTESIAN_POINT('Ctrl Pts',(20.3317422755908,-20.9522048947021,-8.74739733305558));
#55725=CARTESIAN_POINT('Ctrl Pts',(20.2628393849067,-21.0072437867916,-8.75178379506812));
#55726=CARTESIAN_POINT('Ctrl Pts',(20.1911679546946,-21.0586554168247,-8.75617025708066));
#55727=CARTESIAN_POINT('Ctrl Pts',(20.1171588579738,-21.1061753813487,-8.76055671909321));
#55728=CARTESIAN_POINT('Ctrl Pts',(20.043149761253,-21.1536953458726,-8.76494318110575));
#55729=CARTESIAN_POINT('Ctrl Pts',(19.9668035395282,-21.1973234230529,-8.76932964311829));
#55730=CARTESIAN_POINT('Ctrl Pts',(19.8885775886028,-21.2368524223451,-8.77371610513083));
#55731=CARTESIAN_POINT('Ctrl Pts',(19.8139509296381,-21.2745626337838,-8.77790073952388));
#55732=CARTESIAN_POINT('Ctrl Pts',(19.7373359438749,-21.3086830520783,-8.78208537391693));
#55733=CARTESIAN_POINT('Ctrl Pts',(19.6591123506694,-21.3389996101045,-8.78627000830997));
#55734=CARTESIAN_POINT('Ctrl Pts',(19.5810000990668,-21.3692730162627,-8.79044868639392));
#55735=CARTESIAN_POINT('Ctrl Pts',(19.5012842132702,-21.3957531518832,-8.79462736447786));
#55736=CARTESIAN_POINT('Ctrl Pts',(19.4203680775091,-21.4182722603509,-8.7988060425618));
#55737=CARTESIAN_POINT('Ctrl Pts',(19.3380015781678,-21.4411950076538,-8.80305962044724));
#55738=CARTESIAN_POINT('Ctrl Pts',(19.2543918069889,-21.4600131107992,-8.80731319833268));
#55739=CARTESIAN_POINT('Ctrl Pts',(19.1699845756622,-21.4746013259698,-8.81156677621811));
#55740=CARTESIAN_POINT('Ctrl Pts',(19.0872137432219,-21.4889067201227,-8.81573789019606));
#55741=CARTESIAN_POINT('Ctrl Pts',(19.0036765695344,-21.4991446900207,-8.81990900417402));
#55742=CARTESIAN_POINT('Ctrl Pts',(18.9198060037776,-21.5052481526401,-8.82408011815197));
#55743=CARTESIAN_POINT('Ctrl Pts',(18.8359635815991,-21.5113495671838,-8.82824983247234));
#55744=CARTESIAN_POINT('Ctrl Pts',(18.7517884479705,-21.5133191964338,-8.83241954679272));
#55745=CARTESIAN_POINT('Ctrl Pts',(18.6677187513895,-21.5111418085137,-8.83658926111309));
#55746=CARTESIAN_POINT('Ctrl Pts',(18.5836520463691,-21.5089644980744,-8.84075882705713));
#55747=CARTESIAN_POINT('Ctrl Pts',(18.4996912307932,-21.502640476632,-8.84492839300118));
#55748=CARTESIAN_POINT('Ctrl Pts',(18.4162731576902,-21.4922066163357,-8.84909795894522));
#55749=CARTESIAN_POINT('Ctrl Pts',(18.3299222080443,-21.481405914383,-8.85341412168414));
#55750=CARTESIAN_POINT('Ctrl Pts',(18.2441533999762,-21.4662010579768,-8.85773028442306));
#55751=CARTESIAN_POINT('Ctrl Pts',(18.1594420717103,-21.4466910003124,-8.86204644716198));
#55752=CARTESIAN_POINT('Ctrl Pts',(18.0774902060527,-21.4278164807242,-8.86622201135366));
#55753=CARTESIAN_POINT('Ctrl Pts',(17.996528423794,-21.404913110059,-8.87039757554534));
#55754=CARTESIAN_POINT('Ctrl Pts',(17.916971813041,-21.3781213781908,-8.87457313973702));
#55755=CARTESIAN_POINT('Ctrl Pts',(17.8333969870066,-21.3499764596372,-8.87895960174956));
#55756=CARTESIAN_POINT('Ctrl Pts',(17.7513735563979,-21.3175402693169,-8.88334606376211));
#55757=CARTESIAN_POINT('Ctrl Pts',(17.6713570660693,-21.2810319866776,-8.88773252577465));
#55758=CARTESIAN_POINT('Ctrl Pts',(17.5913405757408,-21.2445237040383,-8.89211898778719));
#55759=CARTESIAN_POINT('Ctrl Pts',(17.513331505326,-21.203943664325,-8.89650544979973));
#55760=CARTESIAN_POINT('Ctrl Pts',(17.4377516489576,-21.159564316712,-8.90089191181227));
#55761=CARTESIAN_POINT('Ctrl Pts',(17.3656493338169,-21.1172269286685,-8.90507654620532));
#55762=CARTESIAN_POINT('Ctrl Pts',(17.295489223029,-21.0712745855039,-8.90926118059836));
#55763=CARTESIAN_POINT('Ctrl Pts',(17.227656848054,-21.0219107006307,-8.91344581499141));
#55764=CARTESIAN_POINT('Ctrl Pts',(17.1599210240689,-20.9726170791376,-8.91762449307535));
#55765=CARTESIAN_POINT('Ctrl Pts',(17.0945067235341,-20.919921829671,-8.9218031711593));
#55766=CARTESIAN_POINT('Ctrl Pts',(17.0317733474473,-20.8640733310569,-8.92598184924324));
#55767=CARTESIAN_POINT('Ctrl Pts',(16.9679155206798,-20.8072237882428,-8.93023542712867));
#55768=CARTESIAN_POINT('Ctrl Pts',(16.9068360906094,-20.7471070845336,-8.93448900501411));
#55769=CARTESIAN_POINT('Ctrl Pts',(16.8488816768787,-20.6840302849062,-8.93874258289955));
#55770=CARTESIAN_POINT('Ctrl Pts',(16.7920508225469,-20.6221763521239,-8.9429136968775));
#55771=CARTESIAN_POINT('Ctrl Pts',(16.7382252223473,-20.5574764280243,-8.94708481085545));
#55772=CARTESIAN_POINT('Ctrl Pts',(16.6876956296652,-20.4902582435822,-8.9512559248334));
#55773=CARTESIAN_POINT('Ctrl Pts',(16.6371829926759,-20.423062614851,-8.95542563915378));
#55774=CARTESIAN_POINT('Ctrl Pts',(16.5899644428517,-20.3533507714291,-8.95959535347415));
#55775=CARTESIAN_POINT('Ctrl Pts',(16.546289949262,-20.2814828821387,-8.96376506779452));
#55776=CARTESIAN_POINT('Ctrl Pts',(16.5026170097982,-20.2096175502162,-8.96793463373857));
#55777=CARTESIAN_POINT('Ctrl Pts',(16.4624881140047,-20.1355967185418,-8.97210419968261));
#55778=CARTESIAN_POINT('Ctrl Pts',(16.426108718498,-20.0598076695739,-8.97627376562665));
#55779=CARTESIAN_POINT('Ctrl Pts',(16.388450268324,-19.9813539711403,-8.98058992836557));
#55780=CARTESIAN_POINT('Ctrl Pts',(16.3548101172678,-19.9010058763734,-8.98490609110449));
#55781=CARTESIAN_POINT('Ctrl Pts',(16.3253623529171,-19.8192166309839,-8.98922225384341));
#55782=CARTESIAN_POINT('Ctrl Pts',(16.2968738463928,-19.7400916616603,-8.99339781803509));
#55783=CARTESIAN_POINT('Ctrl Pts',(16.2723088794103,-19.6596184551162,-8.99757338222677));
#55784=CARTESIAN_POINT('Ctrl Pts',(16.2517740015378,-19.5782220792646,-9.00174894641845));
#55785=CARTESIAN_POINT('Ctrl Pts',(16.230201955801,-19.4927145659702,-9.00613540843099));
#55786=CARTESIAN_POINT('Ctrl Pts',(16.213077931431,-19.4061887466983,-9.01052187044353));
#55787=CARTESIAN_POINT('Ctrl Pts',(16.2004642109875,-19.3191463002578,-9.01490833245608));
#55788=CARTESIAN_POINT('Ctrl Pts',(16.1878504905441,-19.2321038538173,-9.01929479446862));
#55789=CARTESIAN_POINT('Ctrl Pts',(16.179747051756,-19.144545364966,-9.02368125648116));
#55790=CARTESIAN_POINT('Ctrl Pts',(16.1761531171477,-19.0569729673897,-9.0280677184937));
#55791=CARTESIAN_POINT('Ctrl Pts',(16.1747268399112,-19.022219269613,-9.0298085155863));
#55792=CARTESIAN_POINT('Ctrl Pts',(16.1740088273484,-18.9874363059254,-9.0315493126789));
#55793=CARTESIAN_POINT('Ctrl Pts',(16.1740000808904,-18.9526435515772,-9.0332901097715));
#55794=CARTESIAN_POINT('Ctrl Pts',(16.1699656690245,-18.9526308403706,-9.03329079541859));
#55795=CARTESIAN_POINT('Ctrl Pts',(16.1727141322405,-18.1388729144851,-9.07394170533744));
#55796=CARTESIAN_POINT('Ctrl Pts',(17.0319371704071,-16.4715241260563,-9.15698455081677));
#55797=CARTESIAN_POINT('Ctrl Pts',(19.1726622426421,-16.2273768357865,-9.25149015774581));
#55798=CARTESIAN_POINT('Ctrl Pts',(20.1114245041509,-16.7803425872416,-9.305344854756));
#55799=CARTESIAN_POINT('Ctrl Pts',(20.2929505583934,-16.9226084740135,-9.31680761620571));
#55800=CARTESIAN_POINT('',(16.174000001606,-18.9519093211995,-8.96670989026365));
#55801=CARTESIAN_POINT('Ctrl Pts',(16.174000001606,-18.9519093211995,-8.96670989026365));
#55802=CARTESIAN_POINT('Ctrl Pts',(16.1740031377284,-18.8633718327363,-8.97108917708311));
#55803=CARTESIAN_POINT('Ctrl Pts',(16.1786036643305,-18.7749281972307,-8.97546846390257));
#55804=CARTESIAN_POINT('Ctrl Pts',(16.1877467776185,-18.6870575014995,-8.97984775072203));
#55805=CARTESIAN_POINT('Ctrl Pts',(16.1969159526897,-18.5989363367042,-8.9842395203819));
#55806=CARTESIAN_POINT('Ctrl Pts',(16.2106535575188,-18.5113917635125,-8.98863129004177));
#55807=CARTESIAN_POINT('Ctrl Pts',(16.2288531973792,-18.4248951742598,-8.99302305970163));
#55808=CARTESIAN_POINT('Ctrl Pts',(16.2470794228643,-18.3382722327341,-8.99742124475989));
#55809=CARTESIAN_POINT('Ctrl Pts',(16.2697805833342,-18.2527007028955,-9.00181942981814));
#55810=CARTESIAN_POINT('Ctrl Pts',(16.2968004138022,-18.1686366251622,-9.00621761487639));
#55811=CARTESIAN_POINT('Ctrl Pts',(16.323895396912,-18.0843387325822,-9.01062803299535));
#55812=CARTESIAN_POINT('Ctrl Pts',(16.3553329301084,-18.0015570394279,-9.0150384511143));
#55813=CARTESIAN_POINT('Ctrl Pts',(16.3909082116846,-17.9207285170583,-9.01944886923326));
#55814=CARTESIAN_POINT('Ctrl Pts',(16.4178853374885,-17.8594353629383,-9.02279333761612));
#55815=CARTESIAN_POINT('Ctrl Pts',(16.4472408225495,-17.7992649146788,-9.02613780599898));
#55816=CARTESIAN_POINT('Ctrl Pts',(16.4788683829461,-17.7403971815138,-9.02948227438184));
#55817=CARTESIAN_POINT('Ctrl Pts',(16.5184411227219,-17.6667412480013,-9.03366690877489));
#55818=CARTESIAN_POINT('Ctrl Pts',(16.5616998679758,-17.5948890389389,-9.03785154316794));
#55819=CARTESIAN_POINT('Ctrl Pts',(16.6084559713663,-17.5252335221418,-9.04203617756098));
#55820=CARTESIAN_POINT('Ctrl Pts',(16.6551455232309,-17.4556771513513,-9.04621485564493));
#55821=CARTESIAN_POINT('Ctrl Pts',(16.7053222910481,-17.3883116408714,-9.05039353372887));
#55822=CARTESIAN_POINT('Ctrl Pts',(16.7587517035101,-17.3235055519856,-9.05457221181281));
#55823=CARTESIAN_POINT('Ctrl Pts',(16.8131387997914,-17.2575378605319,-9.05882578969825));
#55824=CARTESIAN_POINT('Ctrl Pts',(16.8708960667841,-17.1942226731586,-9.06307936758369));
#55825=CARTESIAN_POINT('Ctrl Pts',(16.9317298045576,-17.1339180044288,-9.06733294546913));
#55826=CARTESIAN_POINT('Ctrl Pts',(16.9913841616171,-17.0747824593773,-9.07150405944708));
#55827=CARTESIAN_POINT('Ctrl Pts',(17.053996425417,-17.0185420838703,-9.07567517342503));
#55828=CARTESIAN_POINT('Ctrl Pts',(17.1192501263854,-16.9654998500726,-9.07984628740298));
#55829=CARTESIAN_POINT('Ctrl Pts',(17.1844819308442,-16.9124754151088,-9.08401600172335));
#55830=CARTESIAN_POINT('Ctrl Pts',(17.2523530554691,-16.8626472804565,-9.08818571604372));
#55831=CARTESIAN_POINT('Ctrl Pts',(17.3225130695871,-16.8162788933773,-9.09235543036409));
#55832=CARTESIAN_POINT('Ctrl Pts',(17.3926705871107,-16.7699121562843,-9.09652499630814));
#55833=CARTESIAN_POINT('Ctrl Pts',(17.4651164479272,-16.7270051749184,-9.10069456225218));
#55834=CARTESIAN_POINT('Ctrl Pts',(17.5394714392694,-16.6877779442822,-9.10486412819622));
#55835=CARTESIAN_POINT('Ctrl Pts',(17.6164406603804,-16.6471715326089,-9.10918029093514));
#55836=CARTESIAN_POINT('Ctrl Pts',(17.6954552934391,-16.6105086923157,-9.11349645367407));
#55837=CARTESIAN_POINT('Ctrl Pts',(17.7760690203241,-16.5779805733362,-9.11781261641299));
#55838=CARTESIAN_POINT('Ctrl Pts',(17.8540567635348,-16.5465120544111,-9.12198818060466));
#55839=CARTESIAN_POINT('Ctrl Pts',(17.933540559028,-16.5189131263825,-9.12616374479634));
#55840=CARTESIAN_POINT('Ctrl Pts',(18.0140996850992,-16.4953063812095,-9.13033930898802));
#55841=CARTESIAN_POINT('Ctrl Pts',(18.0987276611172,-16.4705073154576,-9.13472577100056));
#55842=CARTESIAN_POINT('Ctrl Pts',(18.1845418843913,-16.4501144565313,-9.13911223301311));
#55843=CARTESIAN_POINT('Ctrl Pts',(18.271043398772,-16.4342090663879,-9.14349869502565));
#55844=CARTESIAN_POINT('Ctrl Pts',(18.3575449131528,-16.4183036762444,-9.14788515703819));
#55845=CARTESIAN_POINT('Ctrl Pts',(18.4447331334585,-16.406885754803,-9.15227161905073));
#55846=CARTESIAN_POINT('Ctrl Pts',(18.5321062576864,-16.3999735665917,-9.15665808106327));
#55847=CARTESIAN_POINT('Ctrl Pts',(18.6154380422939,-16.3933810933995,-9.1608416525087));
#55848=CARTESIAN_POINT('Ctrl Pts',(18.699248101493,-16.3908622168774,-9.16502522395412));
#55849=CARTESIAN_POINT('Ctrl Pts',(18.7831042309695,-16.392470985806,-9.16920879539955));
#55850=CARTESIAN_POINT('Ctrl Pts',(18.8668503855916,-16.3940776448814,-9.17338688021372));
#55851=CARTESIAN_POINT('Ctrl Pts',(18.9506420350365,-16.3998011941729,-9.17756496502789));
#55852=CARTESIAN_POINT('Ctrl Pts',(19.0340424954886,-16.4096439075336,-9.18174304984206));
#55853=CARTESIAN_POINT('Ctrl Pts',(19.1173586063387,-16.4194766661656,-9.18591690902259));
#55854=CARTESIAN_POINT('Ctrl Pts',(19.2002838596478,-16.4334202620667,-9.19009076820312));
#55855=CARTESIAN_POINT('Ctrl Pts',(19.282383581627,-16.45142497665,-9.19426462738365));
#55856=CARTESIAN_POINT('Ctrl Pts',(19.3644249023165,-16.4694168836558,-9.19843551750712));
#55857=CARTESIAN_POINT('Ctrl Pts',(19.4456414103866,-16.4914640715301,-9.20260640763059));
#55858=CARTESIAN_POINT('Ctrl Pts',(19.5256069084354,-16.5174654443781,-9.20677729775406));
#55859=CARTESIAN_POINT('Ctrl Pts',(19.6055553058994,-16.5434612568444,-9.21094729593461));
#55860=CARTESIAN_POINT('Ctrl Pts',(19.6842527850318,-16.5734094406313,-9.21511729411516));
#55861=CARTESIAN_POINT('Ctrl Pts',(19.7612877178884,-16.6071588657916,-9.2192872922957));
#55862=CARTESIAN_POINT('Ctrl Pts',(19.8383126150258,-16.6409038942485,-9.22345674723009));
#55863=CARTESIAN_POINT('Ctrl Pts',(19.9136749774788,-16.6784489895465,-9.22762620216448));
#55864=CARTESIAN_POINT('Ctrl Pts',(19.986984126806,-16.7195952925215,-9.23179565709887));
#55865=CARTESIAN_POINT('Ctrl Pts',(20.0603319682237,-16.7607633122466,-9.23596731264437));
#55866=CARTESIAN_POINT('Ctrl Pts',(20.1316240343953,-16.8055361040649,-9.24013896818987));
#55867=CARTESIAN_POINT('Ctrl Pts',(20.2004959726216,-16.8536698157143,-9.24431062373536));
#55868=CARTESIAN_POINT('Ctrl Pts',(20.2320270456839,-16.8757064770579,-9.24622049848527));
#55869=CARTESIAN_POINT('Ctrl Pts',(20.2630512663503,-16.8984469952002,-9.24813037323518));
#55870=CARTESIAN_POINT('Ctrl Pts',(20.293535888361,-16.9218650751948,-9.2500402479851));
#55871=CARTESIAN_POINT('Ctrl Pts',(20.293535888361,-16.9218650751948,-8.45013430445441));
#55872=CARTESIAN_POINT('Ctrl Pts',(20.3602160824505,-16.9730883483156,-8.45430378930826));
#55873=CARTESIAN_POINT('Ctrl Pts',(20.4243834050837,-17.0276105723033,-8.4584732741621));
#55874=CARTESIAN_POINT('Ctrl Pts',(20.4857033632667,-17.085148284646,-8.46264275901595));
#55875=CARTESIAN_POINT('Ctrl Pts',(20.5470302074154,-17.1426924582246,-8.46681271208489));
#55876=CARTESIAN_POINT('Ctrl Pts',(20.6055087176485,-17.2032524768093,-8.47098266515382));
#55877=CARTESIAN_POINT('Ctrl Pts',(20.6608405118462,-17.266507299954,-8.47515261822275));
#55878=CARTESIAN_POINT('Ctrl Pts',(20.7162314123542,-17.3298296929158,-8.47932702570247));
#55879=CARTESIAN_POINT('Ctrl Pts',(20.7684685826588,-17.3958522904954,-8.48350143318219));
#55880=CARTESIAN_POINT('Ctrl Pts',(20.8172936355307,-17.4642205714028,-8.48767584066191));
#55881=CARTESIAN_POINT('Ctrl Pts',(20.8661466876126,-17.5326280587777,-8.49185264199692));
#55882=CARTESIAN_POINT('Ctrl Pts',(20.9115834780555,-17.6033835204386,-8.49602944333194));
#55883=CARTESIAN_POINT('Ctrl Pts',(20.9533900376111,-17.6761050744858,-8.50020624466695));
#55884=CARTESIAN_POINT('Ctrl Pts',(20.9952677497756,-17.7489503968688,-8.5043901547025));
#55885=CARTESIAN_POINT('Ctrl Pts',(21.0335026842567,-17.8237680837989,-8.50857406473805));
#55886=CARTESIAN_POINT('Ctrl Pts',(21.0679278703286,-17.9001536727719,-8.5127579747736));
#55887=CARTESIAN_POINT('Ctrl Pts',(21.0899269831306,-17.9489672125086,-8.51543166573444));
#55888=CARTESIAN_POINT('Ctrl Pts',(21.1103712768816,-17.9984206443933,-8.51810535669527));
#55889=CARTESIAN_POINT('Ctrl Pts',(21.1292278697973,-18.0484052613331,-8.5207790476561));
#55890=CARTESIAN_POINT('Ctrl Pts',(21.1587406102024,-18.1266369456353,-8.52496368204915));
#55891=CARTESIAN_POINT('Ctrl Pts',(21.1844714983967,-18.2064616309202,-8.5291483164422));
#55892=CARTESIAN_POINT('Ctrl Pts',(21.2062483053235,-18.2874788815808,-8.53333295083525));
#55893=CARTESIAN_POINT('Ctrl Pts',(21.2279941156611,-18.3683808142128,-8.53751162891918));
#55894=CARTESIAN_POINT('Ctrl Pts',(21.2457969056055,-18.4504715000486,-8.54169030700312));
#55895=CARTESIAN_POINT('Ctrl Pts',(21.2595330219156,-18.5333319271619,-8.54586898508706));
#55896=CARTESIAN_POINT('Ctrl Pts',(21.2735153482386,-18.6176775678805,-8.5501225629725));
#55897=CARTESIAN_POINT('Ctrl Pts',(21.2832836065124,-18.7028203654202,-8.55437614085793));
#55898=CARTESIAN_POINT('Ctrl Pts',(21.288760950006,-18.7883036704005,-8.55862971874337));
#55899=CARTESIAN_POINT('Ctrl Pts',(21.2941321045079,-18.8721297147068,-8.56280083272132));
#55900=CARTESIAN_POINT('Ctrl Pts',(21.2953772042646,-18.9562827012369,-8.56697194669927));
#55901=CARTESIAN_POINT('Ctrl Pts',(21.2924758541409,-19.0403249895433,-8.57114306067723));
#55902=CARTESIAN_POINT('Ctrl Pts',(21.2895754775933,-19.1243390766482,-8.5753127749976));
#55903=CARTESIAN_POINT('Ctrl Pts',(21.2825314303294,-19.2082420799253,-8.57948248931797));
#55904=CARTESIAN_POINT('Ctrl Pts',(21.2713754270314,-19.2915967348151,-8.58365220363835));
#55905=CARTESIAN_POINT('Ctrl Pts',(21.2602198207119,-19.3749484235886,-8.5878217695824));
#55906=CARTESIAN_POINT('Ctrl Pts',(21.2449526111524,-19.4577513469166,-8.59199133552645));
#55907=CARTESIAN_POINT('Ctrl Pts',(21.2256571796747,-19.539575100711,-8.5961609014705));
#55908=CARTESIAN_POINT('Ctrl Pts',(21.2056833446298,-19.6242756767481,-8.60047706420942));
#55909=CARTESIAN_POINT('Ctrl Pts',(21.1813928737509,-19.7079264335901,-8.60479322694834));
#55910=CARTESIAN_POINT('Ctrl Pts',(21.1529349892685,-19.7900653421378,-8.60910938968726));
#55911=CARTESIAN_POINT('Ctrl Pts',(21.1254041173799,-19.8695285843792,-8.61328495387894));
#55912=CARTESIAN_POINT('Ctrl Pts',(21.0939733891635,-19.9475765433411,-8.61746051807061));
#55913=CARTESIAN_POINT('Ctrl Pts',(21.058826881657,-20.0238115367569,-8.62163608226229));
#55914=CARTESIAN_POINT('Ctrl Pts',(21.0219052076091,-20.1038969784586,-8.62602254427483));
#55915=CARTESIAN_POINT('Ctrl Pts',(20.98088279295,-20.1819809787842,-8.63040900628737));
#55916=CARTESIAN_POINT('Ctrl Pts',(20.9360262797509,-20.2576340464641,-8.63479546829991));
#55917=CARTESIAN_POINT('Ctrl Pts',(20.8911697665518,-20.3332871141441,-8.63918193031245));
#55918=CARTESIAN_POINT('Ctrl Pts',(20.8424795394309,-20.4065088081494,-8.64356839232499));
#55919=CARTESIAN_POINT('Ctrl Pts',(20.790271595083,-20.4769088914603,-8.64795485433753));
#55920=CARTESIAN_POINT('Ctrl Pts',(20.7404658156452,-20.5440697625802,-8.65213948873058));
#55921=CARTESIAN_POINT('Ctrl Pts',(20.6872735296056,-20.6089129557,-8.65632412312363));
#55922=CARTESIAN_POINT('Ctrl Pts',(20.6309382156177,-20.6710769052399,-8.66050875751668));
#55923=CARTESIAN_POINT('Ctrl Pts',(20.5746830879764,-20.7331523720919,-8.66468743560061));
#55924=CARTESIAN_POINT('Ctrl Pts',(20.5152941248615,-20.7925558323524,-8.66886611368455));
#55925=CARTESIAN_POINT('Ctrl Pts',(20.4530567178388,-20.8489565100058,-8.67304479176848));
#55926=CARTESIAN_POINT('Ctrl Pts',(20.3897037500243,-20.9063681292718,-8.67729836965392));
#55927=CARTESIAN_POINT('Ctrl Pts',(20.3233995043672,-20.960667870067,-8.68155194753935));
#55928=CARTESIAN_POINT('Ctrl Pts',(20.2544863550521,-21.0115439408035,-8.68580552542479));
#55929=CARTESIAN_POINT('Ctrl Pts',(20.1869092216095,-21.0614336796322,-8.68997663940274));
#55930=CARTESIAN_POINT('Ctrl Pts',(20.1168238263198,-21.1080310270074,-8.6941477533807));
#55931=CARTESIAN_POINT('Ctrl Pts',(20.0445871160411,-21.1510819473742,-8.69831886735865));
#55932=CARTESIAN_POINT('Ctrl Pts',(19.9723746454881,-21.1941184215889,-8.70248858167902));
#55933=CARTESIAN_POINT('Ctrl Pts',(19.8980126884871,-21.2336105969123,-8.7066582959994));
#55934=CARTESIAN_POINT('Ctrl Pts',(19.82188608189,-21.2693484573603,-8.71082801031978));
#55935=CARTESIAN_POINT('Ctrl Pts',(19.7457621842044,-21.3050850461018,-8.71499757626382));
#55936=CARTESIAN_POINT('Ctrl Pts',(19.6678741785634,-21.3370673908662,-8.71916714220786));
#55937=CARTESIAN_POINT('Ctrl Pts',(19.5886290994203,-21.3651326325803,-8.7233367081519));
#55938=CARTESIAN_POINT('Ctrl Pts',(19.5065978610537,-21.3941846135709,-8.72765287089082));
#55939=CARTESIAN_POINT('Ctrl Pts',(19.4231128413873,-21.4190387397286,-8.73196903362974));
#55940=CARTESIAN_POINT('Ctrl Pts',(19.3386433049389,-21.4395703957461,-8.73628519636867));
#55941=CARTESIAN_POINT('Ctrl Pts',(19.2569253547557,-21.4594332352284,-8.74046076056034));
#55942=CARTESIAN_POINT('Ctrl Pts',(19.1742865155734,-21.4752508467085,-8.74463632475203));
#55943=CARTESIAN_POINT('Ctrl Pts',(19.0911608126529,-21.4869627519759,-8.7488118889437));
#55944=CARTESIAN_POINT('Ctrl Pts',(19.0038366280904,-21.4992661977359,-8.75319835095625));
#55945=CARTESIAN_POINT('Ctrl Pts',(18.9159756858741,-21.5070382273415,-8.75758481296879));
#55946=CARTESIAN_POINT('Ctrl Pts',(18.8280834484891,-21.5102705690994,-8.76197127498134));
#55947=CARTESIAN_POINT('Ctrl Pts',(18.740191211104,-21.5135029108574,-8.76635773699389));
#55948=CARTESIAN_POINT('Ctrl Pts',(18.6522682575723,-21.5121956494501,-8.77074419900643));
#55949=CARTESIAN_POINT('Ctrl Pts',(18.5648137584889,-21.5064032601928,-8.77513066101898));
#55950=CARTESIAN_POINT('Ctrl Pts',(18.4813831705471,-21.5008773873516,-8.77931529541202));
#55951=CARTESIAN_POINT('Ctrl Pts',(18.3980683312294,-21.4912494832414,-8.78349992980507));
#55952=CARTESIAN_POINT('Ctrl Pts',(18.3153050503467,-21.4775285662876,-8.78768456419811));
#55953=CARTESIAN_POINT('Ctrl Pts',(18.2326595727504,-21.4638271793609,-8.79186324228205));
#55954=CARTESIAN_POINT('Ctrl Pts',(18.1505645441393,-21.4460444262517,-8.79604192036599));
#55955=CARTESIAN_POINT('Ctrl Pts',(18.0694525718378,-21.4242412333191,-8.80022059844993));
#55956=CARTESIAN_POINT('Ctrl Pts',(17.9868867257269,-21.4020472338228,-8.80447417633536));
#55957=CARTESIAN_POINT('Ctrl Pts',(17.9053400062238,-21.3756872759159,-8.8087277542208));
#55958=CARTESIAN_POINT('Ctrl Pts',(17.8252599013641,-21.3452804752329,-8.81298133210624));
#55959=CARTESIAN_POINT('Ctrl Pts',(17.7467323056007,-21.3154631697152,-8.81715244608419));
#55960=CARTESIAN_POINT('Ctrl Pts',(17.6696154154526,-21.2817547038764,-8.82132356006214));
#55961=CARTESIAN_POINT('Ctrl Pts',(17.5943160431837,-21.2443177089085,-8.82549467404009));
#55962=CARTESIAN_POINT('Ctrl Pts',(17.5190419383466,-21.2068932762859,-8.82966438836045));
#55963=CARTESIAN_POINT('Ctrl Pts',(17.4455845517335,-21.1657430039572,-8.83383410268082));
#55964=CARTESIAN_POINT('Ctrl Pts',(17.3743287784402,-21.1210768011442,-8.83800381700118));
#55965=CARTESIAN_POINT('Ctrl Pts',(17.3030755407331,-21.0764121877464,-8.84217338294522));
#55966=CARTESIAN_POINT('Ctrl Pts',(17.2340241499114,-21.0282321376744,-8.84634294888926));
#55967=CARTESIAN_POINT('Ctrl Pts',(17.1675318647123,-20.9767907499611,-8.85051251483329));
#55968=CARTESIAN_POINT('Ctrl Pts',(17.0987017927924,-20.9235407465156,-8.85482867757222));
#55969=CARTESIAN_POINT('Ctrl Pts',(17.0326145482177,-20.8667961238603,-8.85914484031114));
#55970=CARTESIAN_POINT('Ctrl Pts',(16.9696289167238,-20.8068840072896,-8.86346100305007));
#55971=CARTESIAN_POINT('Ctrl Pts',(16.908695035551,-20.7489235216147,-8.86763656724175));
#55972=CARTESIAN_POINT('Ctrl Pts',(16.8506640912076,-20.6879991088316,-8.87181213143344));
#55973=CARTESIAN_POINT('Ctrl Pts',(16.7958218659397,-20.6244429797905,-8.87598769562512));
#55974=CARTESIAN_POINT('Ctrl Pts',(16.7382096902485,-20.5576767817619,-8.88037415763767));
#55975=CARTESIAN_POINT('Ctrl Pts',(16.6841171816934,-20.4880064858708,-8.88476061965021));
#55976=CARTESIAN_POINT('Ctrl Pts',(16.6338248927157,-20.4158526287654,-8.88914708166276));
#55977=CARTESIAN_POINT('Ctrl Pts',(16.583532603738,-20.3436987716601,-8.89353354367531));
#55978=CARTESIAN_POINT('Ctrl Pts',(16.537040776547,-20.2690618860433,-8.89792000568785));
#55979=CARTESIAN_POINT('Ctrl Pts',(16.4945737975988,-20.192391181845,-8.9023064677004));
#55980=CARTESIAN_POINT('Ctrl Pts',(16.4520961746315,-20.115701260729,-8.90669402914565));
#55981=CARTESIAN_POINT('Ctrl Pts',(16.4134992022811,-20.0367143701648,-8.91108159059091));
#55982=CARTESIAN_POINT('Ctrl Pts',(16.3790251742675,-19.955839414531,-8.91546915203616));
#55983=CARTESIAN_POINT('Ctrl Pts',(16.3446454932948,-19.8751857940064,-8.91984470579147));
#55984=CARTESIAN_POINT('Ctrl Pts',(16.3143664333075,-19.7926547636182,-8.92422025954678));
#55985=CARTESIAN_POINT('Ctrl Pts',(16.288384114166,-19.7086788876112,-8.9285958133021));
#55986=CARTESIAN_POINT('Ctrl Pts',(16.262443998658,-19.624839415405,-8.93296425975242));
#55987=CARTESIAN_POINT('Ctrl Pts',(16.2407868563188,-19.5395601416143,-8.93733270620274));
#55988=CARTESIAN_POINT('Ctrl Pts',(16.2235607960526,-19.4532933305799,-8.94170115265305));
#55989=CARTESIAN_POINT('Ctrl Pts',(16.2063704951608,-19.3672055997965,-8.94606053069714));
#55990=CARTESIAN_POINT('Ctrl Pts',(16.193593030381,-19.2801348014828,-8.95041990874123));
#55991=CARTESIAN_POINT('Ctrl Pts',(16.1853263642748,-19.1925466660734,-8.95477928678532));
#55992=CARTESIAN_POINT('Ctrl Pts',(16.1777850503447,-19.1126438833577,-8.95875615459972));
#55993=CARTESIAN_POINT('Ctrl Pts',(16.1739971536887,-19.0323109723967,-8.96273302241411));
#55994=CARTESIAN_POINT('Ctrl Pts',(16.174000001606,-18.95190932191,-8.96670989022851));
#55995=CARTESIAN_POINT('Origin',(18.734,-18.952,1.76670989022851));
#55996=CARTESIAN_POINT('',(20.2947700633212,-16.9202870453763,-7.65021348571703));
#55997=CARTESIAN_POINT('',(20.2923705334705,-16.9234130561299,-7.71658757622639));
#55998=CARTESIAN_POINT('',(20.293535888361,-16.9218650751948,1.76670989022851));
#55999=CARTESIAN_POINT('',(16.1740010826189,-18.9496456407634,-8.23329012251336));
#56000=CARTESIAN_POINT('Ctrl Pts',(20.2923705334702,-16.9234130561297,-7.71658757622637));
#56001=CARTESIAN_POINT('Ctrl Pts',(20.5052428179242,-17.0840214782408,-7.72982826804403));
#56002=CARTESIAN_POINT('Ctrl Pts',(21.2942513355713,-17.8922292565335,-7.78546089542218));
#56003=CARTESIAN_POINT('Ctrl Pts',(21.5288884325279,-20.114707711301,-7.88348545836079));
#56004=CARTESIAN_POINT('Ctrl Pts',(19.2691669165561,-21.9314105027038,-8.01066126504223));
#56005=CARTESIAN_POINT('Ctrl Pts',(16.7471750902531,-21.0909114965219,-8.12726281551246));
#56006=CARTESIAN_POINT('Ctrl Pts',(16.1802303010149,-19.5894613347174,-8.20147243042223));
#56007=CARTESIAN_POINT('Ctrl Pts',(16.1744184492745,-18.9496462808249,-8.23329010977151));
#56008=CARTESIAN_POINT('Ctrl Pts',(16.1740010826189,-18.9496456407634,-8.23329012251336));
#56009=CARTESIAN_POINT('Ctrl Pts',(16.1741014808467,-18.8404782076363,-8.23871812867226));
#56010=CARTESIAN_POINT('Ctrl Pts',(16.1811885397045,-18.7316228555833,-8.24414613483116));
#56011=CARTESIAN_POINT('Ctrl Pts',(16.1951208364064,-18.6238345041446,-8.24957414099005));
#56012=CARTESIAN_POINT('Ctrl Pts',(16.2083299266979,-18.5216412981712,-8.25472038679507));
#56013=CARTESIAN_POINT('Ctrl Pts',(16.2276915596983,-18.4204066645004,-8.25986663260008));
#56014=CARTESIAN_POINT('Ctrl Pts',(16.253046772176,-18.32075434152,-8.2650128784051));
#56015=CARTESIAN_POINT('Ctrl Pts',(16.2736641888711,-18.2397227402536,-8.26919751279815));
#56016=CARTESIAN_POINT('Ctrl Pts',(16.2982940662941,-18.1595514977397,-8.27338214719119));
#56017=CARTESIAN_POINT('Ctrl Pts',(16.3268482220626,-18.0806675043515,-8.27756678158424));
#56018=CARTESIAN_POINT('Ctrl Pts',(16.3553617345247,-18.0018957925641,-8.28174545966817));
#56019=CARTESIAN_POINT('Ctrl Pts',(16.3877882750862,-17.9244081193638,-8.28592413775211));
#56020=CARTESIAN_POINT('Ctrl Pts',(16.4239892031397,-17.8486187792114,-8.29010281583605));
#56021=CARTESIAN_POINT('Ctrl Pts',(16.4608390068116,-17.7714709696054,-8.29435639372148));
#56022=CARTESIAN_POINT('Ctrl Pts',(16.5015997218016,-17.6960834444034,-8.29860997160692));
#56023=CARTESIAN_POINT('Ctrl Pts',(16.5460727818104,-17.6228745401938,-8.30286354949236));
#56024=CARTESIAN_POINT('Ctrl Pts',(16.5896836447688,-17.5510849334478,-8.30703466347031));
#56025=CARTESIAN_POINT('Ctrl Pts',(16.636863945312,-17.4813906391621,-8.31120577744826));
#56026=CARTESIAN_POINT('Ctrl Pts',(16.687379731032,-17.4141620778998,-8.31537689142621));
#56027=CARTESIAN_POINT('Ctrl Pts',(16.7378785656923,-17.3469560758304,-8.31954660574659));
#56028=CARTESIAN_POINT('Ctrl Pts',(16.7917103865527,-17.2822145310262,-8.32371632006696));
#56029=CARTESIAN_POINT('Ctrl Pts',(16.8485987415143,-17.220277708609,-8.32788603438733));
#56030=CARTESIAN_POINT('Ctrl Pts',(16.9054850721441,-17.1583430901697,-8.33205560033138));
#56031=CARTESIAN_POINT('Ctrl Pts',(16.9654274088045,-17.0992133339121,-8.33622516627543));
#56032=CARTESIAN_POINT('Ctrl Pts',(17.0281108772058,-17.0431934878745,-8.34039473221947));
#56033=CARTESIAN_POINT('Ctrl Pts',(17.0929982190277,-16.9852040531582,-8.34471089495839));
#56034=CARTESIAN_POINT('Ctrl Pts',(17.160822642128,-16.9305476379184,-8.34902705769731));
#56035=CARTESIAN_POINT('Ctrl Pts',(17.2311971876102,-16.8795175013831,-8.35334322043623));
#56036=CARTESIAN_POINT('Ctrl Pts',(17.2992792896755,-16.8301496661781,-8.35751878462791));
#56037=CARTESIAN_POINT('Ctrl Pts',(17.3697475047295,-16.7841757035315,-8.3616943488196));
#56038=CARTESIAN_POINT('Ctrl Pts',(17.4422231594135,-16.7418161628216,-8.36586991301128));
#56039=CARTESIAN_POINT('Ctrl Pts',(17.5183593871211,-16.6973171424108,-8.37025637502382));
#56040=CARTESIAN_POINT('Ctrl Pts',(17.5967106568092,-16.6568075367651,-8.37464283703636));
#56041=CARTESIAN_POINT('Ctrl Pts',(17.6768123961765,-16.6204866780732,-8.3790292990489));
#56042=CARTESIAN_POINT('Ctrl Pts',(17.7569141355438,-16.5841658193814,-8.38341576106144));
#56043=CARTESIAN_POINT('Ctrl Pts',(17.8387657767031,-16.5520338488593,-8.38780222307398));
#56044=CARTESIAN_POINT('Ctrl Pts',(17.921884774769,-16.524229652346,-8.39218868508653));
#56045=CARTESIAN_POINT('Ctrl Pts',(18.0011804710186,-16.4977043913048,-8.39637337892849));
#56046=CARTESIAN_POINT('Ctrl Pts',(18.0819246518065,-16.4750187798312,-8.40055807277046));
#56047=CARTESIAN_POINT('Ctrl Pts',(18.1637106209523,-16.4563297445084,-8.40474276661243));
#56048=CARTESIAN_POINT('Ctrl Pts',(18.2453798597927,-16.437667383404,-8.40892148778458));
#56049=CARTESIAN_POINT('Ctrl Pts',(18.3280874888044,-16.4229903695745,-8.41310020895672));
#56050=CARTESIAN_POINT('Ctrl Pts',(18.4114100949884,-16.4124063803072,-8.41727893012886));
#56051=CARTESIAN_POINT('Ctrl Pts',(18.4946347461072,-16.4018348337058,-8.42145273874578));
#56052=CARTESIAN_POINT('Ctrl Pts',(18.5784724833057,-16.3953468042856,-8.42562654736271));
#56053=CARTESIAN_POINT('Ctrl Pts',(18.6624895012295,-16.3929989744891,-8.42980035597963));
#56054=CARTESIAN_POINT('Ctrl Pts',(18.7464521744712,-16.3906526633381,-8.43397146485419));
#56055=CARTESIAN_POINT('Ctrl Pts',(18.8305934396788,-16.3924412477091,-8.43814257372876));
#56056=CARTESIAN_POINT('Ctrl Pts',(18.9144752300249,-16.398369507672,-8.44231368260332));
#56057=CARTESIAN_POINT('Ctrl Pts',(18.9983279261208,-16.4042957114284,-8.44648334473617));
#56058=CARTESIAN_POINT('Ctrl Pts',(19.0819208676515,-16.4143587064509,-8.45065300686901));
#56059=CARTESIAN_POINT('Ctrl Pts',(19.1648182224782,-16.4285112127888,-8.45482266900186));
#56060=CARTESIAN_POINT('Ctrl Pts',(19.2477116915594,-16.4426630557395,-8.45899213568521));
#56061=CARTESIAN_POINT('Ctrl Pts',(19.3299091855245,-16.4609039503774,-8.46316160236856));
#56062=CARTESIAN_POINT('Ctrl Pts',(19.4109835709542,-16.4831352315977,-8.46733106905191));
#56063=CARTESIAN_POINT('Ctrl Pts',(19.4921313337444,-16.5053866335099,-8.47150430936189));
#56064=CARTESIAN_POINT('Ctrl Pts',(19.5721535125707,-16.5316355155387,-8.47567754967187));
#56065=CARTESIAN_POINT('Ctrl Pts',(19.6506371967137,-16.5617330170877,-8.47985078998185));
#56066=CARTESIAN_POINT('Ctrl Pts',(19.7291549023695,-16.591843565457,-8.48402583932959));
#56067=CARTESIAN_POINT('Ctrl Pts',(19.8061323627794,-16.6258058722132,-8.48820088867733));
#56068=CARTESIAN_POINT('Ctrl Pts',(19.8811779671305,-16.6634234310973,-8.49237593802507));
#56069=CARTESIAN_POINT('Ctrl Pts',(19.9563509512674,-16.7011048407111,-8.49655807395564));
#56070=CARTESIAN_POINT('Ctrl Pts',(20.0295851250235,-16.7424536740936,-8.50074020988622));
#56071=CARTESIAN_POINT('Ctrl Pts',(20.1005148650005,-16.7872281589662,-8.50492234581679));
#56072=CARTESIAN_POINT('Ctrl Pts',(20.1669693727351,-16.8291776480275,-8.50884061458016));
#56073=CARTESIAN_POINT('Ctrl Pts',(20.231401090238,-16.8741335444452,-8.51275888334353));
#56074=CARTESIAN_POINT('Ctrl Pts',(20.293535888361,-16.9218650751948,-8.5166771521069));
#56075=CARTESIAN_POINT('',(16.1740010575059,-18.9543268925436,-8.16670989022852));
#56076=CARTESIAN_POINT('Ctrl Pts',(16.1740010575059,-18.9543268925436,-8.16670989022852));
#56077=CARTESIAN_POINT('Ctrl Pts',(16.173925195224,-18.8708647825268,-8.17086478789788));
#56078=CARTESIAN_POINT('Ctrl Pts',(16.1779353066412,-18.7872780169979,-8.17501968556725));
#56079=CARTESIAN_POINT('Ctrl Pts',(16.1860403077383,-18.7040052286649,-8.17917458323661));
#56080=CARTESIAN_POINT('Ctrl Pts',(16.1940671586084,-18.621535375116,-8.18328941845664));
#56081=CARTESIAN_POINT('Ctrl Pts',(16.2061102365111,-18.539373952273,-8.18740425367668));
#56082=CARTESIAN_POINT('Ctrl Pts',(16.2221259449782,-18.4579466307084,-8.19151908889671));
#56083=CARTESIAN_POINT('Ctrl Pts',(16.238134689091,-18.3765547174256,-8.1956321348003));
#56084=CARTESIAN_POINT('Ctrl Pts',(16.2581125446655,-18.2958967363639,-8.19974518070389));
#56085=CARTESIAN_POINT('Ctrl Pts',(16.2819644394348,-18.216390314281,-8.20385822660748));
#56086=CARTESIAN_POINT('Ctrl Pts',(16.3058135810414,-18.136893069419,-8.2079707977528));
#56087=CARTESIAN_POINT('Ctrl Pts',(16.3335357367832,-18.0585475732033,-8.21208336889813));
#56088=CARTESIAN_POINT('Ctrl Pts',(16.3649858005362,-17.9817568744182,-8.21619594004345));
#56089=CARTESIAN_POINT('Ctrl Pts',(16.3969970744395,-17.9035958852594,-8.2203818978976));
#56090=CARTESIAN_POINT('Ctrl Pts',(16.4328704281987,-17.8270462022341,-8.22456785575175));
#56091=CARTESIAN_POINT('Ctrl Pts',(16.4724022025116,-17.7525103575288,-8.2287538136059));
#56092=CARTESIAN_POINT('Ctrl Pts',(16.5112918107485,-17.6791852955861,-8.23287177349699));
#56093=CARTESIAN_POINT('Ctrl Pts',(16.553721559467,-17.6078095092637,-8.23698973338808));
#56094=CARTESIAN_POINT('Ctrl Pts',(16.5994527799561,-17.5387384653211,-8.24110769327917));
#56095=CARTESIAN_POINT('Ctrl Pts',(16.6463167081173,-17.467956614176,-8.24532765011484));
#56096=CARTESIAN_POINT('Ctrl Pts',(16.6966475137941,-17.3995956231065,-8.24954760695052));
#56097=CARTESIAN_POINT('Ctrl Pts',(16.7501447185243,-17.3340017854889,-8.25376756378619));
#56098=CARTESIAN_POINT('Ctrl Pts',(16.8036419232545,-17.2684079478714,-8.25798752062187));
#56099=CARTESIAN_POINT('Ctrl Pts',(16.8603051182412,-17.2055816046286,-8.26220747745754));
#56100=CARTESIAN_POINT('Ctrl Pts',(16.9197953580223,-17.1458268308308,-8.26642743429322));
#56101=CARTESIAN_POINT('Ctrl Pts',(16.9787876447051,-17.0865722243692,-8.27061206868627));
#56102=CARTESIAN_POINT('Ctrl Pts',(17.040795780927,-17.0301005497847,-8.27479670307932));
#56103=CARTESIAN_POINT('Ctrl Pts',(17.1055265727615,-16.9767343731087,-8.27898133747237));
#56104=CARTESIAN_POINT('Ctrl Pts',(17.170165228326,-16.9234441565798,-8.28316001555632));
#56105=CARTESIAN_POINT('Ctrl Pts',(17.2375184898921,-16.8732509480031,-8.28733869364027));
#56106=CARTESIAN_POINT('Ctrl Pts',(17.3072561423607,-16.8264407877718,-8.29151737172421));
#56107=CARTESIAN_POINT('Ctrl Pts',(17.3782437921301,-16.7787915890601,-8.29577094960965));
#56108=CARTESIAN_POINT('Ctrl Pts',(17.4517018138304,-16.7346482555832,-8.30002452749508));
#56109=CARTESIAN_POINT('Ctrl Pts',(17.5272463530814,-16.6942698045053,-8.30427810538052));
#56110=CARTESIAN_POINT('Ctrl Pts',(17.601326314026,-16.6546741684936,-8.30844921935847));
#56111=CARTESIAN_POINT('Ctrl Pts',(17.6774121876526,-16.6186989652307,-8.31262033333642));
#56112=CARTESIAN_POINT('Ctrl Pts',(17.7551140500802,-16.5865439557984,-8.31679144731437));
#56113=CARTESIAN_POINT('Ctrl Pts',(17.8327898388975,-16.5543997362901,-8.32096116163475));
#56114=CARTESIAN_POINT('Ctrl Pts',(17.912080114858,-16.5260733404924,-8.32513087595512));
#56115=CARTESIAN_POINT('Ctrl Pts',(17.9925737212262,-16.5017169401998,-8.32930059027549));
#56116=CARTESIAN_POINT('Ctrl Pts',(18.0730644632864,-16.4773614066125,-8.33347015621953));
#56117=CARTESIAN_POINT('Ctrl Pts',(18.1547580100543,-16.4569757200691,-8.33763972216357));
#56118=CARTESIAN_POINT('Ctrl Pts',(18.2372280581077,-16.4406621816752,-8.34180928810761));
#56119=CARTESIAN_POINT('Ctrl Pts',(18.3225976513131,-16.4237750793962,-8.34612545084653));
#56120=CARTESIAN_POINT('Ctrl Pts',(18.4087988479272,-16.4112519089494,-8.35044161358545));
#56121=CARTESIAN_POINT('Ctrl Pts',(18.4953492973481,-16.4031481325656,-8.35475777632437));
#56122=CARTESIAN_POINT('Ctrl Pts',(18.5790803749826,-16.3953083358451,-8.35893334051605));
#56123=CARTESIAN_POINT('Ctrl Pts',(18.6631378283657,-16.3916044048151,-8.36310890470773));
#56124=CARTESIAN_POINT('Ctrl Pts',(18.7470834485356,-16.392033433153,-8.36728446889941));
#56125=CARTESIAN_POINT('Ctrl Pts',(18.8352689624185,-16.3924841306923,-8.37167093091196));
#56126=CARTESIAN_POINT('Ctrl Pts',(18.9233304658569,-16.3974962383813,-8.3760573929245));
#56127=CARTESIAN_POINT('Ctrl Pts',(19.0107666109435,-16.4070048638422,-8.38044385493704));
#56128=CARTESIAN_POINT('Ctrl Pts',(19.0982027560302,-16.4165134893031,-8.38483031694958));
#56129=CARTESIAN_POINT('Ctrl Pts',(19.1850129820694,-16.4305184650313,-8.38921677896212));
#56130=CARTESIAN_POINT('Ctrl Pts',(19.2707112385804,-16.4488937205181,-8.39360324097467));
#56131=CARTESIAN_POINT('Ctrl Pts',(19.3524727077245,-16.4664248576225,-8.39778819867499));
#56132=CARTESIAN_POINT('Ctrl Pts',(19.433526484304,-16.4879988204599,-8.40197315637532));
#56133=CARTESIAN_POINT('Ctrl Pts',(19.5134425416023,-16.5135436595377,-8.40615811407565));
#56134=CARTESIAN_POINT('Ctrl Pts',(19.5932250321228,-16.5390458045443,-8.41033607729535));
#56135=CARTESIAN_POINT('Ctrl Pts',(19.6718731494991,-16.5685054918704,-8.41451404051504));
#56136=CARTESIAN_POINT('Ctrl Pts',(19.7489678548332,-16.6017999545453,-8.41869200373474));
#56137=CARTESIAN_POINT('Ctrl Pts',(19.8259879712294,-16.6350622049094,-8.4228659247853));
#56138=CARTESIAN_POINT('Ctrl Pts',(19.9014572393312,-16.6721516838604,-8.42703984583586));
#56139=CARTESIAN_POINT('Ctrl Pts',(19.9749733693939,-16.7128963631723,-8.43121376688642));
#56140=CARTESIAN_POINT('Ctrl Pts',(20.0484374966371,-16.7536122210786,-8.43538473544664));
#56141=CARTESIAN_POINT('Ctrl Pts',(20.1199508294567,-16.7979779202083,-8.43955570400687));
#56142=CARTESIAN_POINT('Ctrl Pts',(20.1891338986594,-16.8457746234146,-8.4437266725671));
#56143=CARTESIAN_POINT('Ctrl Pts',(20.2245612927115,-16.8702504476067,-8.44586254986287));
#56144=CARTESIAN_POINT('Ctrl Pts',(20.2593780205127,-16.8956252326461,-8.44799842715864));
#56145=CARTESIAN_POINT('Ctrl Pts',(20.293535888361,-16.9218650751948,-8.45013430445441));
#56146=CARTESIAN_POINT('Ctrl Pts',(20.2947700633212,-16.9202870453763,-7.65021348571703));
#56147=CARTESIAN_POINT('Ctrl Pts',(20.8607342530498,-17.3635946506649,-7.68605039300052));
#56148=CARTESIAN_POINT('Ctrl Pts',(21.6914150266576,-18.8744582227272,-7.76427923584449));
#56149=CARTESIAN_POINT('Ctrl Pts',(20.547911124632,-21.3754310952809,-7.88490001424893));
#56150=CARTESIAN_POINT('Ctrl Pts',(17.6781136533722,-21.788969486026,-8.01207582093036));
#56151=CARTESIAN_POINT('Ctrl Pts',(16.2739022033865,-20.1719439048314,-8.1060124462569));
#56152=CARTESIAN_POINT('Ctrl Pts',(16.1718447244466,-19.1382186602577,-8.15755713602294));
#56153=CARTESIAN_POINT('Ctrl Pts',(16.1735502429248,-18.9543273023083,-8.16670989022852));
#56154=CARTESIAN_POINT('Origin',(18.734,-18.952,1.76670989022851));
#56155=CARTESIAN_POINT('',(20.293535888361,-16.9218650751948,-6.85004462273915));
#56156=CARTESIAN_POINT('',(20.293535888361,-16.9218650751948,-6.91673142333303));
#56157=CARTESIAN_POINT('',(20.293535888361,-16.9218650751948,1.76670989022851));
#56158=CARTESIAN_POINT('',(16.1743644997381,-18.9525601738959,-7.4332900849458));
#56159=CARTESIAN_POINT('Ctrl Pts',(20.293535888361,-16.9218650751948,-6.91673142333303));
#56160=CARTESIAN_POINT('Ctrl Pts',(20.3602014303377,-16.9730770926618,-6.9209011201467));
#56161=CARTESIAN_POINT('Ctrl Pts',(20.4243665537901,-17.0275953336019,-6.92507081696036));
#56162=CARTESIAN_POINT('Ctrl Pts',(20.4856940849898,-17.0851395787013,-6.92924051377403));
#56163=CARTESIAN_POINT('Ctrl Pts',(20.5470198579879,-17.1426821740623,-6.93341009104649));
#56164=CARTESIAN_POINT('Ctrl Pts',(20.6055078656427,-17.2032502856324,-6.93757966831895));
#56165=CARTESIAN_POINT('Ctrl Pts',(20.6608565812866,-17.2665256705744,-6.94174924559141));
#56166=CARTESIAN_POINT('Ctrl Pts',(20.7178321198183,-17.3316608609927,-6.94604137609135));
#56167=CARTESIAN_POINT('Ctrl Pts',(20.7714805826835,-17.3996645851212,-6.9503335065913));
#56168=CARTESIAN_POINT('Ctrl Pts',(20.8215177102066,-17.4701532435594,-6.95462563709125));
#56169=CARTESIAN_POINT('Ctrl Pts',(20.8701964154299,-17.5387282556663,-6.95880124360044));
#56170=CARTESIAN_POINT('Ctrl Pts',(20.9154571739033,-17.6096545653463,-6.96297685010962));
#56171=CARTESIAN_POINT('Ctrl Pts',(20.9570834061099,-17.682551234008,-6.9671524566188));
#56172=CARTESIAN_POINT('Ctrl Pts',(21.0004520635259,-17.7584992716362,-6.97150284911413));
#56173=CARTESIAN_POINT('Ctrl Pts',(21.0398749862283,-17.836585743878,-6.97585324160946));
#56174=CARTESIAN_POINT('Ctrl Pts',(21.0751622352272,-17.9163555685729,-6.98020363410478));
#56175=CARTESIAN_POINT('Ctrl Pts',(21.110449484226,-17.9961253932677,-6.98455402660011));
#56176=CARTESIAN_POINT('Ctrl Pts',(21.1416009292668,-18.077578024238,-6.98890441909544));
#56177=CARTESIAN_POINT('Ctrl Pts',(21.1684852750765,-18.1602415485544,-6.99325481159076));
#56178=CARTESIAN_POINT('Ctrl Pts',(21.194345276957,-18.2397554377671,-6.99743944598381));
#56179=CARTESIAN_POINT('Ctrl Pts',(21.216353744912,-18.320685570143,-7.00162408037686));
#56180=CARTESIAN_POINT('Ctrl Pts',(21.2343571694271,-18.4026239673097,-7.00580871476991));
#56181=CARTESIAN_POINT('Ctrl Pts',(21.2523349682957,-18.4844457353101,-7.00998739285385));
#56182=CARTESIAN_POINT('Ctrl Pts',(21.2663189491973,-18.5672724719894,-7.0141660709378));
#56183=CARTESIAN_POINT('Ctrl Pts',(21.2762049862094,-18.6506798909933,-7.01834474902174));
#56184=CARTESIAN_POINT('Ctrl Pts',(21.2862682233301,-18.735582328039,-7.02259832690718));
#56185=CARTESIAN_POINT('Ctrl Pts',(21.2920850111441,-18.8210860111299,-7.02685190479261));
#56186=CARTESIAN_POINT('Ctrl Pts',(21.2935997221946,-18.9067312233284,-7.03110548267805));
#56187=CARTESIAN_POINT('Ctrl Pts',(21.2950850676156,-18.9907160359656,-7.035276596656));
#56188=CARTESIAN_POINT('Ctrl Pts',(21.2924336475012,-19.0748364579016,-7.03944771063394));
#56189=CARTESIAN_POINT('Ctrl Pts',(21.2856453456188,-19.1586543737303,-7.04361882461189));
#56190=CARTESIAN_POINT('Ctrl Pts',(21.2788593216167,-19.2424441636477,-7.04778853893226));
#56191=CARTESIAN_POINT('Ctrl Pts',(21.2679392098803,-19.325931190906,-7.05195825325263));
#56192=CARTESIAN_POINT('Ctrl Pts',(21.252936930744,-19.4086801275884,-7.05612796757299));
#56193=CARTESIAN_POINT('Ctrl Pts',(21.2379351854531,-19.4914261197086,-7.06029753351703));
#56194=CARTESIAN_POINT('Ctrl Pts',(21.2188516444825,-19.5734336209715,-7.06446709946108));
#56195=CARTESIAN_POINT('Ctrl Pts',(21.1957895218785,-19.6542765480702,-7.06863666540512));
#56196=CARTESIAN_POINT('Ctrl Pts',(21.1719165634939,-19.7379618127552,-7.07295282814404));
#56197=CARTESIAN_POINT('Ctrl Pts',(21.1437801888442,-19.8203985795363,-7.07726899088296));
#56198=CARTESIAN_POINT('Ctrl Pts',(21.1115508461405,-19.901132221567,-7.08158515362188));
#56199=CARTESIAN_POINT('Ctrl Pts',(21.0803713708855,-19.9792359737001,-7.08576071781356));
#56200=CARTESIAN_POINT('Ctrl Pts',(21.0453617283798,-20.0557454470086,-7.08993628200524));
#56201=CARTESIAN_POINT('Ctrl Pts',(21.0067242058649,-20.1302719058331,-7.09411184619692));
#56202=CARTESIAN_POINT('Ctrl Pts',(20.9661351939398,-20.2085625189232,-7.09849830820946));
#56203=CARTESIAN_POINT('Ctrl Pts',(20.9215424772638,-20.2846640250238,-7.10288477022201));
#56204=CARTESIAN_POINT('Ctrl Pts',(20.8732322919594,-20.3581597352499,-7.10727123223455));
#56205=CARTESIAN_POINT('Ctrl Pts',(20.8249221066551,-20.4316554454761,-7.1116576942471));
#56206=CARTESIAN_POINT('Ctrl Pts',(20.7728948573422,-20.5025449370743,-7.11604415625964));
#56207=CARTESIAN_POINT('Ctrl Pts',(20.7174842649082,-20.5704530178111,-7.12043061827219));
#56208=CARTESIAN_POINT('Ctrl Pts',(20.6646231959703,-20.6352365470891,-7.12461525266523));
#56209=CARTESIAN_POINT('Ctrl Pts',(20.6084865283938,-20.6975481314174,-7.12879988705828));
#56210=CARTESIAN_POINT('Ctrl Pts',(20.5493342156371,-20.7570378626326,-7.13298452145133));
#56211=CARTESIAN_POINT('Ctrl Pts',(20.490266098876,-20.8164429175788,-7.13716319953527));
#56212=CARTESIAN_POINT('Ctrl Pts',(20.4281911845787,-20.8730337741353,-7.14134187761922));
#56213=CARTESIAN_POINT('Ctrl Pts',(20.3634098690378,-20.9264932207233,-7.14552055570316));
#56214=CARTESIAN_POINT('Ctrl Pts',(20.2974673949733,-20.9809108894708,-7.1497741335886));
#56215=CARTESIAN_POINT('Ctrl Pts',(20.2287208456647,-21.0320834094472,-7.15402771147404));
#56216=CARTESIAN_POINT('Ctrl Pts',(20.1575266602173,-21.0797151707056,-7.15828128935947));
#56217=CARTESIAN_POINT('Ctrl Pts',(20.0877127129788,-21.1264234973262,-7.16245240333742));
#56218=CARTESIAN_POINT('Ctrl Pts',(20.0155455870562,-21.1697268615303,-7.16662351731537));
#56219=CARTESIAN_POINT('Ctrl Pts',(19.9413936052584,-21.2093880220248,-7.17079463129332));
#56220=CARTESIAN_POINT('Ctrl Pts',(19.8672665058742,-21.2490358738339,-7.1749643456137));
#56221=CARTESIAN_POINT('Ctrl Pts',(19.7911562786917,-21.2850437324071,-7.17913405993407));
#56222=CARTESIAN_POINT('Ctrl Pts',(19.713457069089,-21.3172196197841,-7.18330377425445));
#56223=CARTESIAN_POINT('Ctrl Pts',(19.6357606243576,-21.3493943622049,-7.18747334019849));
#56224=CARTESIAN_POINT('Ctrl Pts',(19.5564757349844,-21.3777372293228,-7.19164290614254));
#56225=CARTESIAN_POINT('Ctrl Pts',(19.4760165374071,-21.402104377004,-7.19581247208659));
#56226=CARTESIAN_POINT('Ctrl Pts',(19.3927284937003,-21.4273282435376,-7.2001286348255));
#56227=CARTESIAN_POINT('Ctrl Pts',(19.3081825327892,-21.4482914634566,-7.20444479756443));
#56228=CARTESIAN_POINT('Ctrl Pts',(19.2228531842897,-21.4648912758434,-7.20876096030335));
#56229=CARTESIAN_POINT('Ctrl Pts',(19.1403034303424,-21.4809503510877,-7.21293652449503));
#56230=CARTESIAN_POINT('Ctrl Pts',(19.0570210156986,-21.4929259089214,-7.2171120886867));
#56231=CARTESIAN_POINT('Ctrl Pts',(18.9734422997763,-21.5007776256625,-7.22128765287838));
#56232=CARTESIAN_POINT('Ctrl Pts',(18.8856422216022,-21.5090259139505,-7.22567411489092));
#56233=CARTESIAN_POINT('Ctrl Pts',(18.7975157065272,-21.5127227980494,-7.23006057690346));
#56234=CARTESIAN_POINT('Ctrl Pts',(18.7095680581453,-21.5118834114501,-7.234447038916));
#56235=CARTESIAN_POINT('Ctrl Pts',(18.6216204097634,-21.5110440248507,-7.23883350092854));
#56236=CARTESIAN_POINT('Ctrl Pts',(18.5338522025563,-21.5056684789459,-7.24321996294108));
#56237=CARTESIAN_POINT('Ctrl Pts',(18.4467595506041,-21.4958342957494,-7.24760642495362));
#56238=CARTESIAN_POINT('Ctrl Pts',(18.3636741606704,-21.4864525978996,-7.25179105934667));
#56239=CARTESIAN_POINT('Ctrl Pts',(18.2808942658294,-21.4729786230522,-7.25597569373971));
#56240=CARTESIAN_POINT('Ctrl Pts',(18.1988547913486,-21.4554415522751,-7.26016032813276));
#56241=CARTESIAN_POINT('Ctrl Pts',(18.1169320899053,-21.4379294433475,-7.26433900621671));
#56242=CARTESIAN_POINT('Ctrl Pts',(18.0357481614732,-21.4163658213152,-7.26851768430065));
#56243=CARTESIAN_POINT('Ctrl Pts',(17.955732329606,-21.3908315713102,-7.2726963623846));
#56244=CARTESIAN_POINT('Ctrl Pts',(17.874282271459,-21.3648396382251,-7.27694994027003));
#56245=CARTESIAN_POINT('Ctrl Pts',(17.7940430771264,-21.3347333841335,-7.28120351815547));
#56246=CARTESIAN_POINT('Ctrl Pts',(17.7154562415196,-21.3006525098576,-7.2854570960409));
#56247=CARTESIAN_POINT('Ctrl Pts',(17.6383929650706,-21.267232359833,-7.28962821001885));
#56248=CARTESIAN_POINT('Ctrl Pts',(17.5629189921768,-21.2299905173578,-7.2937993239968));
#56249=CARTESIAN_POINT('Ctrl Pts',(17.4894331713722,-21.1891082694137,-7.29797043797475));
#56250=CARTESIAN_POINT('Ctrl Pts',(17.4159720094442,-21.1482397399027,-7.30214015229513));
#56251=CARTESIAN_POINT('Ctrl Pts',(17.3444980763221,-21.1037334544494,-7.3063098666155));
#56252=CARTESIAN_POINT('Ctrl Pts',(17.2753861385067,-21.0558169129132,-7.31047958093588));
#56253=CARTESIAN_POINT('Ctrl Pts',(17.2062766599909,-21.0079020764533,-7.31464914687992));
#56254=CARTESIAN_POINT('Ctrl Pts',(17.13952938724,-20.9565774880023,-7.31881871282395));
#56255=CARTESIAN_POINT('Ctrl Pts',(17.0754894346057,-20.9021135106643,-7.32298827876799));
#56256=CARTESIAN_POINT('Ctrl Pts',(17.0091979162385,-20.8457346470716,-7.32730444150691));
#56257=CARTESIAN_POINT('Ctrl Pts',(16.9458080406879,-20.7859918669771,-7.33162060424583));
#56258=CARTESIAN_POINT('Ctrl Pts',(16.8856630675041,-20.7232285521557,-7.33593676698476));
#56259=CARTESIAN_POINT('Ctrl Pts',(16.8274773104957,-20.6625097457132,-7.34011233117643));
#56260=CARTESIAN_POINT('Ctrl Pts',(16.7723285700599,-20.5989645570466,-7.34428789536811));
#56261=CARTESIAN_POINT('Ctrl Pts',(16.7204869451086,-20.5329380689268,-7.34846345955979));
#56262=CARTESIAN_POINT('Ctrl Pts',(16.6660269229228,-20.4635767398551,-7.35284992157233));
#56263=CARTESIAN_POINT('Ctrl Pts',(16.6152172172816,-20.3914773402461,-7.35723638358488));
#56264=CARTESIAN_POINT('Ctrl Pts',(16.5683186145658,-20.317072941928,-7.36162284559742));
#56265=CARTESIAN_POINT('Ctrl Pts',(16.52142001185,-20.2426685436098,-7.36600930760997));
#56266=CARTESIAN_POINT('Ctrl Pts',(16.4784327293519,-20.1659596899256,-7.37039576962251));
#56267=CARTESIAN_POINT('Ctrl Pts',(16.4395601204679,-20.0874054955004,-7.37478223163505));
#56268=CARTESIAN_POINT('Ctrl Pts',(16.3997963941391,-20.0070505211682,-7.37926924910123));
#56269=CARTESIAN_POINT('Ctrl Pts',(16.3642056179145,-19.9244993534859,-7.38375626656741));
#56270=CARTESIAN_POINT('Ctrl Pts',(16.333017909016,-19.8401919830611,-7.38824328403359));
#56271=CARTESIAN_POINT('Ctrl Pts',(16.3019356806124,-19.7561697500662,-7.39271512587963));
#56272=CARTESIAN_POINT('Ctrl Pts',(16.2752269677052,-19.6704034844248,-7.39718696772568));
#56273=CARTESIAN_POINT('Ctrl Pts',(16.2530742870064,-19.5833537887801,-7.40165880957172));
#56274=CARTESIAN_POINT('Ctrl Pts',(16.2309688572623,-19.4964897673338,-7.40612111312307));
#56275=CARTESIAN_POINT('Ctrl Pts',(16.2134002030054,-19.408348109083,-7.41058341667443));
#56276=CARTESIAN_POINT('Ctrl Pts',(16.2005019648758,-19.3194067310513,-7.41504572022578));
#56277=CARTESIAN_POINT('Ctrl Pts',(16.1876417930136,-19.2307278436206,-7.41949485428542));
#56278=CARTESIAN_POINT('Ctrl Pts',(16.1794246278367,-19.1412542906273,-7.42394398834506));
#56279=CARTESIAN_POINT('Ctrl Pts',(16.175933399183,-19.0514749505386,-7.4283931224047));
#56280=CARTESIAN_POINT('Ctrl Pts',(16.1746525201579,-19.0185362676236,-7.43002544244505));
#56281=CARTESIAN_POINT('Ctrl Pts',(16.1740072831437,-18.9855565464226,-7.4316577624854));
#56282=CARTESIAN_POINT('Ctrl Pts',(16.1740000613162,-18.952560302501,-7.43329008252576));
#56283=CARTESIAN_POINT('Ctrl Pts',(16.1781030393919,-18.952558854618,-7.43329010977151));
#56284=CARTESIAN_POINT('Ctrl Pts',(16.1790025482941,-18.4906083143692,-7.4561794192865));
#56285=CARTESIAN_POINT('Ctrl Pts',(16.5197425194489,-17.1718695770502,-7.52146066436197));
#56286=CARTESIAN_POINT('Ctrl Pts',(18.3750628649076,-16.0796619494175,-7.61589315318027));
#56287=CARTESIAN_POINT('Ctrl Pts',(19.8237022844342,-16.5698110446498,-7.68743633248356));
#56288=CARTESIAN_POINT('Ctrl Pts',(20.2923705334702,-16.9234130561297,-7.71658757622637));
#56289=CARTESIAN_POINT('',(16.1738764939443,-18.9508698166505,-7.36670989022851));
#56290=CARTESIAN_POINT('Ctrl Pts',(16.170378839146,-18.9508682725878,-7.36670989022851));
#56291=CARTESIAN_POINT('Ctrl Pts',(16.1700290602903,-18.8875375837258,-7.36987218932674));
#56292=CARTESIAN_POINT('Ctrl Pts',(16.2008981559486,-17.9755793377669,-7.41542642398544));
#56293=CARTESIAN_POINT('Ctrl Pts',(17.2895132774888,-16.291783852743,-7.50337259420463));
#56294=CARTESIAN_POINT('Ctrl Pts',(19.3719151115967,-16.2958825772312,-7.59471149360257));
#56295=CARTESIAN_POINT('Ctrl Pts',(20.1912479809582,-16.8392004196504,-7.64365845744004));
#56296=CARTESIAN_POINT('Ctrl Pts',(20.2947700633212,-16.9202870453763,-7.65021348571703));
#56297=CARTESIAN_POINT('Ctrl Pts',(20.293535888361,-16.9218650751948,-6.85004462273914));
#56298=CARTESIAN_POINT('Ctrl Pts',(20.3601338996604,-16.9730252160533,-6.85422899536763));
#56299=CARTESIAN_POINT('Ctrl Pts',(20.4241220221326,-17.0273968372747,-6.85841336799612));
#56300=CARTESIAN_POINT('Ctrl Pts',(20.4851928160501,-17.0846693594828,-6.8625977406246));
#56301=CARTESIAN_POINT('Ctrl Pts',(20.5090109325979,-17.1070061185362,-6.86422968068222));
#56302=CARTESIAN_POINT('Ctrl Pts',(20.5323857251923,-17.1297837513318,-6.86586162073984));
#56303=CARTESIAN_POINT('Ctrl Pts',(20.5553006227462,-17.1529824788,-6.86749356079746));
#56304=CARTESIAN_POINT('Ctrl Pts',(20.6140591953844,-17.2124688504871,-6.87167819519051));
#56305=CARTESIAN_POINT('Ctrl Pts',(20.6700096812721,-17.2749476638323,-6.87586282958355));
#56306=CARTESIAN_POINT('Ctrl Pts',(20.7228319806688,-17.3401230342644,-6.8800474639766));
#56307=CARTESIAN_POINT('Ctrl Pts',(20.7755790940605,-17.4052056356238,-6.88422614206054));
#56308=CARTESIAN_POINT('Ctrl Pts',(20.8252065780214,-17.4729768158299,-6.88840482014449));
#56309=CARTESIAN_POINT('Ctrl Pts',(20.8714311671561,-17.5431039762745,-6.89258349822843));
#56310=CARTESIAN_POINT('Ctrl Pts',(20.9184842988301,-17.6144881156706,-6.89683707611387));
#56311=CARTESIAN_POINT('Ctrl Pts',(20.9620110031542,-17.6883131849442,-6.90109065399931));
#56312=CARTESIAN_POINT('Ctrl Pts',(21.0017554861493,-17.7641931743588,-6.90534423188474));
#56313=CARTESIAN_POINT('Ctrl Pts',(21.0407294447865,-17.838602082111,-6.90951534586269));
#56314=CARTESIAN_POINT('Ctrl Pts',(21.0760663016048,-17.9149865174727,-6.91368645984064));
#56315=CARTESIAN_POINT('Ctrl Pts',(21.1075695674518,-17.9929548975847,-6.9178575738186));
#56316=CARTESIAN_POINT('Ctrl Pts',(21.1390622620736,-18.0708971146537,-6.92202728813897));
#56317=CARTESIAN_POINT('Ctrl Pts',(21.1667237483346,-18.1504217947136,-6.92619700245934));
#56318=CARTESIAN_POINT('Ctrl Pts',(21.1904053024889,-18.2311165212712,-6.93036671677971));
#56319=CARTESIAN_POINT('Ctrl Pts',(21.214086013952,-18.3118083763641,-6.93453628272375));
#56320=CARTESIAN_POINT('Ctrl Pts',(21.2337869461661,-18.3936697535163,-6.9387058486678));
#56321=CARTESIAN_POINT('Ctrl Pts',(21.2494093711531,-18.4762735076587,-6.94287541461184));
#56322=CARTESIAN_POINT('Ctrl Pts',(21.2655810613302,-18.561781507894,-6.94719157735076));
#56323=CARTESIAN_POINT('Ctrl Pts',(21.2773820094429,-18.6480845421362,-6.95150774008968));
#56324=CARTESIAN_POINT('Ctrl Pts',(21.2847607940422,-18.7346998122938,-6.9558239028286));
#56325=CARTESIAN_POINT('Ctrl Pts',(21.2918992155093,-18.8184935991363,-6.95999946702028));
#56326=CARTESIAN_POINT('Ctrl Pts',(21.2948991834511,-18.9025791196893,-6.96417503121196));
#56327=CARTESIAN_POINT('Ctrl Pts',(21.2937672733171,-18.9865182046883,-6.96835059540364));
#56328=CARTESIAN_POINT('Ctrl Pts',(21.2925781930931,-19.0746968533244,-6.97273705741618));
#56329=CARTESIAN_POINT('Ctrl Pts',(21.2868289009943,-19.1627133020808,-6.97712351942873));
#56330=CARTESIAN_POINT('Ctrl Pts',(21.2765884850301,-19.250066763985,-6.98150998144127));
#56331=CARTESIAN_POINT('Ctrl Pts',(21.2663480690658,-19.3374202258893,-6.98589644345381));
#56332=CARTESIAN_POINT('Ctrl Pts',(21.2516167014297,-19.4241101416678,-6.99028290546635));
#56333=CARTESIAN_POINT('Ctrl Pts',(21.2325245180281,-19.5096515334976,-6.9946693674789));
#56334=CARTESIAN_POINT('Ctrl Pts',(21.2143107942863,-19.5912570390866,-6.99885400187194));
#56335=CARTESIAN_POINT('Ctrl Pts',(21.1920609365757,-19.6721211400212,-7.00303863626499));
#56336=CARTESIAN_POINT('Ctrl Pts',(21.1658504730776,-19.75181452637,-7.00722327065804));
#56337=CARTESIAN_POINT('Ctrl Pts',(21.1396773169301,-19.8313944790474,-7.01140194874198));
#56338=CARTESIAN_POINT('Ctrl Pts',(21.1095548952069,-19.9098065938023,-7.01558062682592));
#56339=CARTESIAN_POINT('Ctrl Pts',(21.0756095445167,-19.9866326599466,-7.01975930490986));
#56340=CARTESIAN_POINT('Ctrl Pts',(21.0410557478115,-20.0648357781127,-7.0240128827953));
#56341=CARTESIAN_POINT('Ctrl Pts',(21.0025407271242,-20.1413949579936,-7.02826646068074));
#56342=CARTESIAN_POINT('Ctrl Pts',(20.9602505991267,-20.215886177584,-7.03252003856617));
#56343=CARTESIAN_POINT('Ctrl Pts',(20.9187803477829,-20.2889332395249,-7.03669115254412));
#56344=CARTESIAN_POINT('Ctrl Pts',(20.8736802961219,-20.3599913900462,-7.04086226652207));
#56345=CARTESIAN_POINT('Ctrl Pts',(20.8251733475076,-20.4286834564909,-7.04503338050002));
#56346=CARTESIAN_POINT('Ctrl Pts',(20.7766826758684,-20.4973524726493,-7.0492030948204));
#56347=CARTESIAN_POINT('Ctrl Pts',(20.724787642863,-20.5636566060812,-7.05337280914077));
#56348=CARTESIAN_POINT('Ctrl Pts',(20.669754524153,-20.6272475704269,-7.05754252346114));
#56349=CARTESIAN_POINT('Ctrl Pts',(20.6147233637574,-20.6908362719332,-7.06171208940519));
#56350=CARTESIAN_POINT('Ctrl Pts',(20.556554641366,-20.7517116490139,-7.06588165534923));
#56351=CARTESIAN_POINT('Ctrl Pts',(20.4955540788024,-20.8095594815387,-7.07005122129327));
#56352=CARTESIAN_POINT('Ctrl Pts',(20.4324088117115,-20.8694411724922,-7.07436738403219));
#56353=CARTESIAN_POINT('Ctrl Pts',(20.3662292470559,-20.9260780978832,-7.07868354677112));
#56354=CARTESIAN_POINT('Ctrl Pts',(20.2973935081709,-20.9791656909609,-7.08299970951004));
#56355=CARTESIAN_POINT('Ctrl Pts',(20.2308000862399,-21.030523961278,-7.08717527370171));
#56356=CARTESIAN_POINT('Ctrl Pts',(20.1617212960249,-21.0785603570292,-7.09135083789339));
#56357=CARTESIAN_POINT('Ctrl Pts',(20.0905291277018,-21.1230432344144,-7.09552640208507));
#56358=CARTESIAN_POINT('Ctrl Pts',(20.0157412122,-21.1697728361884,-7.09991286409761));
#56359=CARTESIAN_POINT('Ctrl Pts',(19.9386213249318,-21.2125802257264,-7.10429932611016));
#56360=CARTESIAN_POINT('Ctrl Pts',(19.8596279445188,-21.2512524286207,-7.1086857881227));
#56361=CARTESIAN_POINT('Ctrl Pts',(19.7806345641058,-21.2899246315151,-7.11307225013524));
#56362=CARTESIAN_POINT('Ctrl Pts',(19.6997682540138,-21.3244614898292,-7.11745871214778));
#56363=CARTESIAN_POINT('Ctrl Pts',(19.6175072439402,-21.3547099179687,-7.12184517416032));
#56364=CARTESIAN_POINT('Ctrl Pts',(19.5390311848803,-21.3835665710906,-7.12602980855337));
#56365=CARTESIAN_POINT('Ctrl Pts',(19.4589938470389,-21.4086281659991,-7.13021444294642));
#56366=CARTESIAN_POINT('Ctrl Pts',(19.3777970941006,-21.429725832619,-7.13439907733946));
#56367=CARTESIAN_POINT('Ctrl Pts',(19.29671591469,-21.4507934693218,-7.13857775542341));
#56368=CARTESIAN_POINT('Ctrl Pts',(19.2144790396054,-21.4679082701427,-7.14275643350735));
#56369=CARTESIAN_POINT('Ctrl Pts',(19.1315065014624,-21.4809500946628,-7.1469351115913));
#56370=CARTESIAN_POINT('Ctrl Pts',(19.0470467402045,-21.4942256845145,-7.15118868947673));
#56371=CARTESIAN_POINT('Ctrl Pts',(18.9618251354747,-21.5032806792605,-7.15544226736217));
#56372=CARTESIAN_POINT('Ctrl Pts',(18.876298964101,-21.508042058499,-7.15969584524761));
#56373=CARTESIAN_POINT('Ctrl Pts',(18.7924308844499,-21.5127111291099,-7.16386695922556));
#56374=CARTESIAN_POINT('Ctrl Pts',(18.7082704224837,-21.5132515520536,-7.16803807320351));
#56375=CARTESIAN_POINT('Ctrl Pts',(18.624255374081,-21.5096465973785,-7.17220918718146));
#56376=CARTESIAN_POINT('Ctrl Pts',(18.5402685177392,-21.5060428523808,-7.17637890150184));
#56377=CARTESIAN_POINT('Ctrl Pts',(18.4564274372809,-21.4982965120596,-7.18054861582221));
#56378=CARTESIAN_POINT('Ctrl Pts',(18.3731691163824,-21.4864429513066,-7.18471833014259));
#56379=CARTESIAN_POINT('Ctrl Pts',(18.2899137581722,-21.4745898123542,-7.18888789608663));
#56380=CARTESIAN_POINT('Ctrl Pts',(18.2072415736112,-21.4586298092437,-7.19305746203067));
#56381=CARTESIAN_POINT('Ctrl Pts',(18.1255822535273,-21.4386499242509,-7.19722702797472));
#56382=CARTESIAN_POINT('Ctrl Pts',(18.0410518924869,-21.4179675711496,-7.20154319071364));
#56383=CARTESIAN_POINT('Ctrl Pts',(17.9576074580674,-21.3929775239273,-7.20585935345255));
#56384=CARTESIAN_POINT('Ctrl Pts',(17.8757097136974,-21.363832868264,-7.21017551619147));
#56385=CARTESIAN_POINT('Ctrl Pts',(17.7964797797361,-21.3356375966935,-7.21435108038315));
#56386=CARTESIAN_POINT('Ctrl Pts',(17.7186977338733,-21.303554456016,-7.21852664457484));
#56387=CARTESIAN_POINT('Ctrl Pts',(17.6427597031132,-21.2677708467054,-7.22270220876652));
#56388=CARTESIAN_POINT('Ctrl Pts',(17.562986222945,-21.2301798923558,-7.22708867077906));
#56389=CARTESIAN_POINT('Ctrl Pts',(17.4852484504759,-21.1885050997006,-7.2314751327916));
#56390=CARTESIAN_POINT('Ctrl Pts',(17.4099736292609,-21.1430166976971,-7.23586159480414));
#56391=CARTESIAN_POINT('Ctrl Pts',(17.334698808046,-21.0975282956936,-7.24024805681668));
#56392=CARTESIAN_POINT('Ctrl Pts',(17.2618873758782,-21.0482266726393,-7.24463451882922));
#56393=CARTESIAN_POINT('Ctrl Pts',(17.1919269101811,-20.9954310816997,-7.24902098084176));
#56394=CARTESIAN_POINT('Ctrl Pts',(17.1258771580207,-20.9455867065661,-7.25316224442402));
#56395=CARTESIAN_POINT('Ctrl Pts',(17.0621112325388,-20.892434299838,-7.25730350800628));
#56396=CARTESIAN_POINT('Ctrl Pts',(17.0009846311415,-20.8362127616859,-7.26144477158854));
#56397=CARTESIAN_POINT('Ctrl Pts',(16.9399453026366,-20.7800714932715,-7.26558012252322));
#56398=CARTESIAN_POINT('Ctrl Pts',(16.8815381604268,-20.7208701082194,-7.26971547345791));
#56399=CARTESIAN_POINT('Ctrl Pts',(16.8260879518442,-20.6588894564388,-7.27385082439259));
#56400=CARTESIAN_POINT('Ctrl Pts',(16.770701311821,-20.5969798597695,-7.27798143452813));
#56401=CARTESIAN_POINT('Ctrl Pts',(16.7182651826551,-20.5322976752766,-7.28211204466367));
#56402=CARTESIAN_POINT('Ctrl Pts',(16.6690684130046,-20.4651614391824,-7.2862426547992));
#56403=CARTESIAN_POINT('Ctrl Pts',(16.6199019406792,-20.3980665482496,-7.29037072114092));
#56404=CARTESIAN_POINT('Ctrl Pts',(16.5739711466917,-20.3285209831314,-7.29449878748264));
#56405=CARTESIAN_POINT('Ctrl Pts',(16.5315246255303,-20.2568763255016,-7.29862685382436));
#56406=CARTESIAN_POINT('Ctrl Pts',(16.4890908665707,-20.185253208944,-7.30275367899921));
#56407=CARTESIAN_POINT('Ctrl Pts',(16.4501395400175,-20.1115326575802,-7.30688050417406));
#56408=CARTESIAN_POINT('Ctrl Pts',(16.4148750854128,-20.0360939214575,-7.31100732934891));
#56409=CARTESIAN_POINT('Ctrl Pts',(16.3796101195077,-19.9606540915462,-7.31513421435872));
#56410=CARTESIAN_POINT('Ctrl Pts',(16.3480323287909,-19.8834964546655,-7.31926109936854));
#56411=CARTESIAN_POINT('Ctrl Pts',(16.320298833946,-19.8050220870468,-7.32338798437836));
#56412=CARTESIAN_POINT('Ctrl Pts',(16.2925397363851,-19.7264752742868,-7.32751867920247));
#56413=CARTESIAN_POINT('Ctrl Pts',(16.2686321752694,-19.646609748954,-7.33164937402659));
#56414=CARTESIAN_POINT('Ctrl Pts',(16.2486837569799,-19.5658429540043,-7.3357800688507));
#56415=CARTESIAN_POINT('Ctrl Pts',(16.2287250388403,-19.4850344572077,-7.33991289645232));
#56416=CARTESIAN_POINT('Ctrl Pts',(16.2127296214478,-19.4033242264923,-7.34404572405394));
#56417=CARTESIAN_POINT('Ctrl Pts',(16.2007537416511,-19.3211387199432,-7.34817855165555));
#56418=CARTESIAN_POINT('Ctrl Pts',(16.1887593096482,-19.2388258972814,-7.35231778154836));
#56419=CARTESIAN_POINT('Ctrl Pts',(16.180796886798,-19.1560367972438,-7.35645701144116));
#56420=CARTESIAN_POINT('Ctrl Pts',(16.176870697397,-19.0732011954116,-7.36059624133396));
#56421=CARTESIAN_POINT('Ctrl Pts',(16.1749377014765,-19.0324184251309,-7.36263412429881));
#56422=CARTESIAN_POINT('Ctrl Pts',(16.1739822581149,-18.9916243590029,-7.36467200726366));
#56423=CARTESIAN_POINT('Ctrl Pts',(16.1740002494514,-18.9508698712832,-7.36670989022851));
#56424=CARTESIAN_POINT('Origin',(18.734,-18.952,1.76670989022851));
#56425=CARTESIAN_POINT('',(20.293535888361,-16.9218650751948,-6.05008448366249));
#56426=CARTESIAN_POINT('',(20.2954006764134,-16.9194747298048,-6.11677130171703));
#56427=CARTESIAN_POINT('',(20.293535888361,-16.9218650751948,1.76670989022851));
#56428=CARTESIAN_POINT('',(16.1740008768645,-18.954118854712,-6.6332901097715));
#56429=CARTESIAN_POINT('Ctrl Pts',(20.2954006764134,-16.9194747298048,-6.11677130171703));
#56430=CARTESIAN_POINT('Ctrl Pts',(20.8926533917614,-17.3857070907967,-6.15458085831207));
#56431=CARTESIAN_POINT('Ctrl Pts',(21.7124083657865,-18.9714392500858,-6.23478235046759));
#56432=CARTESIAN_POINT('Ctrl Pts',(20.4337935871551,-21.4567938704141,-6.35737577818358));
#56433=CARTESIAN_POINT('Ctrl Pts',(17.5479307767974,-21.7370548235123,-6.48455158486502));
#56434=CARTESIAN_POINT('Ctrl Pts',(16.247850859816,-20.0919179750469,-6.57652302872766));
#56435=CARTESIAN_POINT('Ctrl Pts',(16.1710772471096,-19.0983559299756,-6.62610253702982));
#56436=CARTESIAN_POINT('Ctrl Pts',(16.1723626618067,-18.9541202106264,-6.6332901097715));
#56437=CARTESIAN_POINT('Ctrl Pts',(16.1740008768645,-18.954118854712,-6.6332901097715));
#56438=CARTESIAN_POINT('Ctrl Pts',(16.1739325519701,-18.8715687540989,-6.63740642252224));
#56439=CARTESIAN_POINT('Ctrl Pts',(16.1778613169669,-18.7888758591841,-6.64152273527298));
#56440=CARTESIAN_POINT('Ctrl Pts',(16.1858020059738,-18.7064659224448,-6.64563904802372));
#56441=CARTESIAN_POINT('Ctrl Pts',(16.1937337220434,-18.624149108506,-6.64975070936243));
#56442=CARTESIAN_POINT('Ctrl Pts',(16.2056683130375,-18.5421150878493,-6.65386237070115));
#56443=CARTESIAN_POINT('Ctrl Pts',(16.2215685692311,-18.4607889397778,-6.65797403203986));
#56444=CARTESIAN_POINT('Ctrl Pts',(16.2374592000152,-18.3795120234588,-6.6620832043354));
#56445=CARTESIAN_POINT('Ctrl Pts',(16.2573106430753,-18.2989425946372,-6.66619237663094));
#56446=CARTESIAN_POINT('Ctrl Pts',(16.2810340922893,-18.219498630985,-6.67030154892649));
#56447=CARTESIAN_POINT('Ctrl Pts',(16.3047507902538,-18.1400772755974,-6.67440955182854));
#56448=CARTESIAN_POINT('Ctrl Pts',(16.3323371713263,-18.0617812045222,-6.67851755473059));
#56449=CARTESIAN_POINT('Ctrl Pts',(16.3636541468014,-17.9850147176797,-6.68262555763264));
#56450=CARTESIAN_POINT('Ctrl Pts',(16.3949722554067,-17.9082454532245,-6.686733709173));
#56451=CARTESIAN_POINT('Ctrl Pts',(16.4300210447237,-17.8330063217983,-6.69084186071336));
#56452=CARTESIAN_POINT('Ctrl Pts',(16.4686133150906,-17.7596815996408,-6.69495001225373));
#56453=CARTESIAN_POINT('Ctrl Pts',(16.5072438266208,-17.6862842198592,-6.69906223457025));
#56454=CARTESIAN_POINT('Ctrl Pts',(16.5494246053548,-17.6148054564872,-6.70317445688677));
#56455=CARTESIAN_POINT('Ctrl Pts',(16.5949228757402,-17.5456042319217,-6.70728667920329));
#56456=CARTESIAN_POINT('Ctrl Pts',(16.6404458510681,-17.4763654320318,-6.71140113440064));
#56457=CARTESIAN_POINT('Ctrl Pts',(16.6892896206455,-17.4094070139063,-6.71551558959799));
#56458=CARTESIAN_POINT('Ctrl Pts',(16.7411800554791,-17.3450561090319,-6.71963004479534));
#56459=CARTESIAN_POINT('Ctrl Pts',(16.7931561866084,-17.2805989295773,-6.72375129495539));
#56460=CARTESIAN_POINT('Ctrl Pts',(16.8481887081044,-17.2187582108671,-6.72787254511545));
#56461=CARTESIAN_POINT('Ctrl Pts',(16.9059658904507,-17.1598249822285,-6.73199379527551));
#56462=CARTESIAN_POINT('Ctrl Pts',(16.9382542996129,-17.1268905239829,-6.73429692959297));
#56463=CARTESIAN_POINT('Ctrl Pts',(16.9713992632832,-17.0948633881751,-6.73660006391043));
#56464=CARTESIAN_POINT('Ctrl Pts',(17.0053421035808,-17.0637887096123,-6.73890319822789));
#56465=CARTESIAN_POINT('Ctrl Pts',(17.067013876621,-17.0073281863675,-6.74308783262094));
#56466=CARTESIAN_POINT('Ctrl Pts',(17.1315694533285,-16.9537872066973,-6.74727246701399));
#56467=CARTESIAN_POINT('Ctrl Pts',(17.1987010234279,-16.9034744198481,-6.75145710140704));
#56468=CARTESIAN_POINT('Ctrl Pts',(17.2657370400465,-16.8532332470235,-6.75563577949098));
#56469=CARTESIAN_POINT('Ctrl Pts',(17.3353414020479,-16.8062114135714,-6.75981445757493));
#56470=CARTESIAN_POINT('Ctrl Pts',(17.4071710083241,-16.7626793686515,-6.76399313565888));
#56471=CARTESIAN_POINT('Ctrl Pts',(17.4802881086698,-16.7183670431123,-6.76824671354431));
#56472=CARTESIAN_POINT('Ctrl Pts',(17.5557106573434,-16.6776711711575,-6.77250029142975));
#56473=CARTESIAN_POINT('Ctrl Pts',(17.6330432222704,-16.6408327248831,-6.77675386931519));
#56474=CARTESIAN_POINT('Ctrl Pts',(17.7088765445242,-16.604708463774,-6.78092498329314));
#56475=CARTESIAN_POINT('Ctrl Pts',(17.7865460506905,-16.5722936025648,-6.78509609727109));
#56476=CARTESIAN_POINT('Ctrl Pts',(17.8656529884828,-16.5437696398415,-6.78926721124905));
#56477=CARTESIAN_POINT('Ctrl Pts',(17.9447333811781,-16.5152552486094,-6.79343692556942));
#56478=CARTESIAN_POINT('Ctrl Pts',(18.0252498151569,-16.4906293187766,-6.79760663988979));
#56479=CARTESIAN_POINT('Ctrl Pts',(18.1067845307988,-16.4700248278448,-6.80177635421016));
#56480=CARTESIAN_POINT('Ctrl Pts',(18.1883163450857,-16.4494210701093,-6.80594592015421));
#56481=CARTESIAN_POINT('Ctrl Pts',(18.2708659227711,-16.4328385786397,-6.81011548609825));
#56482=CARTESIAN_POINT('Ctrl Pts',(18.354002682145,-16.4203598126071,-6.81428505204229));
#56483=CARTESIAN_POINT('Ctrl Pts',(18.4400624274181,-16.407442308555,-6.81860121478121));
#56484=CARTESIAN_POINT('Ctrl Pts',(18.5267508916661,-16.3989225513938,-6.82291737752013));
#56485=CARTESIAN_POINT('Ctrl Pts',(18.6135836740997,-16.3948336173693,-6.82723354025905));
#56486=CARTESIAN_POINT('Ctrl Pts',(18.6975878877789,-16.3908778799405,-6.83140910445074));
#56487=CARTESIAN_POINT('Ctrl Pts',(18.7817266907703,-16.3910686822566,-6.83558466864242));
#56488=CARTESIAN_POINT('Ctrl Pts',(18.8655624783158,-16.3953828377523,-6.8397602328341));
#56489=CARTESIAN_POINT('Ctrl Pts',(18.9536326121895,-16.3999148909862,-6.84414669484664));
#56490=CARTESIAN_POINT('Ctrl Pts',(19.0413677347567,-16.4089977253144,-6.84853315685917));
#56491=CARTESIAN_POINT('Ctrl Pts',(19.1282700391328,-16.4225433120446,-6.85291961887171));
#56492=CARTESIAN_POINT('Ctrl Pts',(19.215172343509,-16.4360888987749,-6.85730608088425));
#56493=CARTESIAN_POINT('Ctrl Pts',(19.3012412773527,-16.4540970446291,-6.86169254289679));
#56494=CARTESIAN_POINT('Ctrl Pts',(19.3859971465594,-16.4764193164273,-6.86607900490932));
#56495=CARTESIAN_POINT('Ctrl Pts',(19.4675566079707,-16.4978997458344,-6.87030003977797));
#56496=CARTESIAN_POINT('Ctrl Pts',(19.5482065113869,-16.5234553484004,-6.87452107464661));
#56497=CARTESIAN_POINT('Ctrl Pts',(19.6275095404914,-16.5529917255143,-6.87874210951525));
#56498=CARTESIAN_POINT('Ctrl Pts',(19.7060066097554,-16.5822279232523,-6.88292024583855));
#56499=CARTESIAN_POINT('Ctrl Pts',(19.7831836026446,-16.6153642261603,-6.88709838216186));
#56500=CARTESIAN_POINT('Ctrl Pts',(19.8586276869387,-16.6522581523634,-6.89127651848516));
#56501=CARTESIAN_POINT('Ctrl Pts',(19.9352336917231,-16.6897202849305,-6.89551900262647));
#56502=CARTESIAN_POINT('Ctrl Pts',(20.0100524891745,-16.7310566538662,-6.89976148676778));
#56503=CARTESIAN_POINT('Ctrl Pts',(20.0826708318901,-16.7760664102025,-6.90400397090909));
#56504=CARTESIAN_POINT('Ctrl Pts',(20.1552891746057,-16.8210761665388,-6.90824645505041));
#56505=CARTESIAN_POINT('Ctrl Pts',(20.2257066150957,-16.8697590872399,-6.91248893919172));
#56506=CARTESIAN_POINT('Ctrl Pts',(20.293535888361,-16.9218650751948,-6.91673142333303));
#56507=CARTESIAN_POINT('',(16.174000571626,-18.9502892327451,-6.56670989025839));
#56508=CARTESIAN_POINT('Ctrl Pts',(16.174000571626,-18.9502892327451,-6.56670989025839));
#56509=CARTESIAN_POINT('Ctrl Pts',(16.1740643617891,-18.8548333601137,-6.57143929947809));
#56510=CARTESIAN_POINT('Ctrl Pts',(16.1794711562484,-18.7595846663132,-6.57616870869779));
#56511=CARTESIAN_POINT('Ctrl Pts',(16.1901275024526,-18.6650980721186,-6.58089811791749));
#56512=CARTESIAN_POINT('Ctrl Pts',(16.2008364140088,-18.5701453968694,-6.585650856246));
#56513=CARTESIAN_POINT('Ctrl Pts',(16.2168466650978,-18.4759625571763,-6.59040359457451));
#56514=CARTESIAN_POINT('Ctrl Pts',(16.2380139506878,-18.3830943473309,-6.59515633290303));
#56515=CARTESIAN_POINT('Ctrl Pts',(16.2593038089219,-18.2896883688619,-6.59993659274351));
#56516=CARTESIAN_POINT('Ctrl Pts',(16.2858104835345,-18.19761248234,-6.604716852584));
#56517=CARTESIAN_POINT('Ctrl Pts',(16.3173390825673,-18.1073994967126,-6.60949711242449));
#56518=CARTESIAN_POINT('Ctrl Pts',(16.3253523527945,-18.0844710744544,-6.61071205742785));
#56519=CARTESIAN_POINT('Ctrl Pts',(16.333689786842,-18.0616628735359,-6.61192700243122));
#56520=CARTESIAN_POINT('Ctrl Pts',(16.3423477078173,-18.0389833992214,-6.61314194743458));
#56521=CARTESIAN_POINT('Ctrl Pts',(16.3721681801721,-17.9608684985717,-6.61732658182763));
#56522=CARTESIAN_POINT('Ctrl Pts',(16.405875193857,-17.8840707367779,-6.62151121622068));
#56523=CARTESIAN_POINT('Ctrl Pts',(16.4433319467771,-17.8090039939072,-6.62569585061373));
#56524=CARTESIAN_POINT('Ctrl Pts',(16.4807353846456,-17.7340440992537,-6.62987452869767));
#56525=CARTESIAN_POINT('Ctrl Pts',(16.5218777565726,-17.6608107375732,-6.63405320678161));
#56526=CARTESIAN_POINT('Ctrl Pts',(16.5665735905076,-17.5896994606788,-6.63823188486555));
#56527=CARTESIAN_POINT('Ctrl Pts',(16.6120705651436,-17.5173135652528,-6.64248546275099));
#56528=CARTESIAN_POINT('Ctrl Pts',(16.661249474465,-17.4471270300731,-6.64673904063642));
#56529=CARTESIAN_POINT('Ctrl Pts',(16.7138648542455,-17.3795325145214,-6.65099261852186));
#56530=CARTESIAN_POINT('Ctrl Pts',(16.7654601822184,-17.3132484505536,-6.65516373249981));
#56531=CARTESIAN_POINT('Ctrl Pts',(16.8203596287512,-17.2494571801029,-6.65933484647776));
#56532=CARTESIAN_POINT('Ctrl Pts',(16.8782881026493,-17.1884996869773,-6.66350596045572));
#56533=CARTESIAN_POINT('Ctrl Pts',(16.9361971380885,-17.1275626487273,-6.66767567477609));
#56534=CARTESIAN_POINT('Ctrl Pts',(16.99713286563,-17.0694578324917,-6.67184538909646));
#56535=CARTESIAN_POINT('Ctrl Pts',(17.060781453689,-17.0144913687209,-6.67601510341684));
#56536=CARTESIAN_POINT('Ctrl Pts',(17.1244277768581,-16.9595268608928,-6.68018466936088));
#56537=CARTESIAN_POINT('Ctrl Pts',(17.1907864198799,-16.9077007835217,-6.68435423530492));
#56538=CARTESIAN_POINT('Ctrl Pts',(17.2595094445542,-16.8592798558094,-6.68852380124897));
#56539=CARTESIAN_POINT('Ctrl Pts',(17.3306486859969,-16.8091565080125,-6.69283996398789));
#56540=CARTESIAN_POINT('Ctrl Pts',(17.4043212347439,-16.7626825189769,-6.69715612672681));
#56541=CARTESIAN_POINT('Ctrl Pts',(17.4801089073792,-16.7201045885064,-6.70147228946573));
#56542=CARTESIAN_POINT('Ctrl Pts',(17.55342780455,-16.6789136296426,-6.70564785365741));
#56543=CARTESIAN_POINT('Ctrl Pts',(17.6287256988456,-16.6413689670528,-6.70982341784909));
#56544=CARTESIAN_POINT('Ctrl Pts',(17.7056010183993,-16.6076460304291,-6.71399898204077));
#56545=CARTESIAN_POINT('Ctrl Pts',(17.78635912759,-16.5722198284453,-6.71838544405331));
#56546=CARTESIAN_POINT('Ctrl Pts',(17.8688576552586,-16.5410117758974,-6.72277190606585));
#56547=CARTESIAN_POINT('Ctrl Pts',(17.9526121488767,-16.5141663251737,-6.7271583680784));
#56548=CARTESIAN_POINT('Ctrl Pts',(18.0363666424947,-16.48732087445,-6.73154483009094));
#56549=CARTESIAN_POINT('Ctrl Pts',(18.1213765216826,-16.4648381003647,-6.73593129210348));
#56550=CARTESIAN_POINT('Ctrl Pts',(18.20714644876,-16.4468003401833,-6.74031775411602));
#56551=CARTESIAN_POINT('Ctrl Pts',(18.2889778682176,-16.4295908639743,-6.7445027922187));
#56552=CARTESIAN_POINT('Ctrl Pts',(18.3718056859211,-16.4163630651953,-6.74868783032138));
#56553=CARTESIAN_POINT('Ctrl Pts',(18.4552077229431,-16.4072259695106,-6.75287286842406));
#56554=CARTESIAN_POINT('Ctrl Pts',(18.5384664989632,-16.3981045687601,-6.75705071782041));
#56555=CARTESIAN_POINT('Ctrl Pts',(18.6222970795582,-16.3930599483572,-6.76122856721675));
#56556=CARTESIAN_POINT('Ctrl Pts',(18.7062667332562,-16.3921502259086,-6.7654064166131));
#56557=CARTESIAN_POINT('Ctrl Pts',(18.7901543122248,-16.391241392653,-6.76958018244063));
#56558=CARTESIAN_POINT('Ctrl Pts',(18.8741802371499,-16.3944594382537,-6.77375394826816));
#56559=CARTESIAN_POINT('Ctrl Pts',(18.9579070743402,-16.4018106693697,-6.7779277140957));
#56560=CARTESIAN_POINT('Ctrl Pts',(19.041577192961,-16.4091569205853,-6.78209865251406));
#56561=CARTESIAN_POINT('Ctrl Pts',(19.124948169362,-16.4206307562896,-6.78626959093242));
#56562=CARTESIAN_POINT('Ctrl Pts',(19.2075843584854,-16.4361864426397,-6.79044052935078));
#56563=CARTESIAN_POINT('Ctrl Pts',(19.2901893576105,-16.4517362576901,-6.79460989350049));
#56564=CARTESIAN_POINT('Ctrl Pts',(19.3720596691157,-16.471364776407,-6.7987792576502));
#56565=CARTESIAN_POINT('Ctrl Pts',(19.4527679051966,-16.4949748274673,-6.80294862179992));
#56566=CARTESIAN_POINT('Ctrl Pts',(19.5335042821171,-16.5185931107316,-6.80711943969727));
#56567=CARTESIAN_POINT('Ctrl Pts',(19.6130773298815,-16.5461955784803,-6.81129025759462));
#56568=CARTESIAN_POINT('Ctrl Pts',(19.6910737323175,-16.5776348488685,-6.81546107549197));
#56569=CARTESIAN_POINT('Ctrl Pts',(19.7690820104975,-16.6090789062047,-6.81963252843869));
#56570=CARTESIAN_POINT('Ctrl Pts',(19.8455127429621,-16.64436074602,-6.8238039813854));
#56571=CARTESIAN_POINT('Ctrl Pts',(19.9199734317183,-16.6832851613175,-6.82797543433211));
#56572=CARTESIAN_POINT('Ctrl Pts',(19.9945177108395,-16.7222532735795,-6.83215157019648));
#56573=CARTESIAN_POINT('Ctrl Pts',(20.0670871265703,-16.7648719041894,-6.83632770606085));
#56574=CARTESIAN_POINT('Ctrl Pts',(20.1373150369702,-16.8109005378046,-6.84050384192522));
#56575=CARTESIAN_POINT('Ctrl Pts',(20.1907958241465,-16.8459528061175,-6.84368410219653));
#56576=CARTESIAN_POINT('Ctrl Pts',(20.2429192181243,-16.8829816922142,-6.84686436246784));
#56577=CARTESIAN_POINT('Ctrl Pts',(20.293535888361,-16.9218650751948,-6.85004462273914));
#56578=CARTESIAN_POINT('Ctrl Pts',(20.293535888361,-16.9218650751948,-6.05008448366249));
#56579=CARTESIAN_POINT('Ctrl Pts',(20.3602243278818,-16.9730946824,-6.05425482454861));
#56580=CARTESIAN_POINT('Ctrl Pts',(20.4243678404919,-17.0275998935312,-6.05842516543473));
#56581=CARTESIAN_POINT('Ctrl Pts',(20.4856397847705,-17.0850886297391,-6.06259550632085));
#56582=CARTESIAN_POINT('Ctrl Pts',(20.5469803613649,-17.1426417605921,-6.06677051851546));
#56583=CARTESIAN_POINT('Ctrl Pts',(20.6054426153629,-17.20318476991,-6.07094553071006));
#56584=CARTESIAN_POINT('Ctrl Pts',(20.6607367305677,-17.2663886654744,-6.07512054290466));
#56585=CARTESIAN_POINT('Ctrl Pts',(20.7160670517863,-17.3296339462947,-6.07929828885399));
#56586=CARTESIAN_POINT('Ctrl Pts',(20.7682248206514,-17.3955432204527,-6.08347603480332));
#56587=CARTESIAN_POINT('Ctrl Pts',(20.8169619670476,-17.4637562552346,-6.08765378075265));
#56588=CARTESIAN_POINT('Ctrl Pts',(20.8657776958325,-17.5320792747738,-6.09183826278073));
#56589=CARTESIAN_POINT('Ctrl Pts',(20.9111615486972,-17.6027130808414,-6.09602274480881));
#56590=CARTESIAN_POINT('Ctrl Pts',(20.9529102925223,-17.6752709317405,-6.10020722683688));
#56591=CARTESIAN_POINT('Ctrl Pts',(20.9669828868101,-17.6997286065002,-6.1016177247942));
#56592=CARTESIAN_POINT('Ctrl Pts',(20.980642853236,-17.7244047147345,-6.10302822275152));
#56593=CARTESIAN_POINT('Ctrl Pts',(20.9938836431733,-17.7492839406918,-6.10443872070884));
#56594=CARTESIAN_POINT('Ctrl Pts',(21.0331661282527,-17.8230950824048,-6.10862335510189));
#56595=CARTESIAN_POINT('Ctrl Pts',(21.0689017421373,-17.8989701434485,-6.11280798949494));
#56596=CARTESIAN_POINT('Ctrl Pts',(21.1008684225543,-17.9765340240093,-6.11699262388799));
#56597=CARTESIAN_POINT('Ctrl Pts',(21.1327896023584,-18.0539875019867,-6.12117130197194));
#56598=CARTESIAN_POINT('Ctrl Pts',(21.1609523307068,-18.1331246030379,-6.12534998005589));
#56599=CARTESIAN_POINT('Ctrl Pts',(21.1851803441784,-18.2135455868415,-6.12952865813984));
#56600=CARTESIAN_POINT('Ctrl Pts',(21.2098426273792,-18.2954080589821,-6.13378223602527));
#56601=CARTESIAN_POINT('Ctrl Pts',(21.2304275222058,-18.3786004681764,-6.13803581391071));
#56602=CARTESIAN_POINT('Ctrl Pts',(21.2468003698023,-18.4626797556596,-6.14228939179614));
#56603=CARTESIAN_POINT('Ctrl Pts',(21.2628557977992,-18.5451290020877,-6.14646050577409));
#56604=CARTESIAN_POINT('Ctrl Pts',(21.2748609466779,-18.6284305735959,-6.15063161975205));
#56605=CARTESIAN_POINT('Ctrl Pts',(21.2827395777799,-18.7121530390891,-6.15480273373));
#56606=CARTESIAN_POINT('Ctrl Pts',(21.2906155651312,-18.7958474107005,-6.15897244805037));
#56607=CARTESIAN_POINT('Ctrl Pts',(21.2943677416632,-18.8799619381738,-6.16314216237074));
#56608=CARTESIAN_POINT('Ctrl Pts',(21.2939715980996,-18.9640588939549,-6.16731187669111));
#56609=CARTESIAN_POINT('Ctrl Pts',(21.2935754686324,-19.0481528572055,-6.17148144263516));
#56610=CARTESIAN_POINT('Ctrl Pts',(21.2890313155854,-19.1322287899834,-6.1756510085792));
#56611=CARTESIAN_POINT('Ctrl Pts',(21.2803667494581,-19.2158491562509,-6.17982057452325));
#56612=CARTESIAN_POINT('Ctrl Pts',(21.2713975478746,-19.3024095114395,-6.18413673726217));
#56613=CARTESIAN_POINT('Ctrl Pts',(21.2580128490967,-19.388481144016,-6.18845290000109));
#56614=CARTESIAN_POINT('Ctrl Pts',(21.2403015155518,-19.4735867263868,-6.19276906274001));
#56615=CARTESIAN_POINT('Ctrl Pts',(21.2231671268342,-19.5559200033636,-6.19694462693169));
#56616=CARTESIAN_POINT('Ctrl Pts',(21.2019838191122,-19.6373487577952,-6.20112019112337));
#56617=CARTESIAN_POINT('Ctrl Pts',(21.1768832583851,-19.7174550188626,-6.20529575531505));
#56618=CARTESIAN_POINT('Ctrl Pts',(21.1505149280065,-19.801607256742,-6.20968221732759));
#56619=CARTESIAN_POINT('Ctrl Pts',(21.1198234271564,-19.8842993445549,-6.21406867934013));
#56620=CARTESIAN_POINT('Ctrl Pts',(21.0850182368018,-19.965071197017,-6.21845514135266));
#56621=CARTESIAN_POINT('Ctrl Pts',(21.0502130464472,-20.045843049479,-6.2228416033652));
#56622=CARTESIAN_POINT('Ctrl Pts',(21.0112944915984,-20.1246941799628,-6.22722806537774));
#56623=CARTESIAN_POINT('Ctrl Pts',(20.9685260259017,-20.2011971179794,-6.23161452739027));
#56624=CARTESIAN_POINT('Ctrl Pts',(20.9277254007097,-20.2741800424132,-6.23579916178332));
#56625=CARTESIAN_POINT('Ctrl Pts',(20.883269491877,-20.3452977698653,-6.23998379617637));
#56626=CARTESIAN_POINT('Ctrl Pts',(20.8353535008893,-20.4141605466913,-6.24416843056941));
#56627=CARTESIAN_POINT('Ctrl Pts',(20.7875057123839,-20.482925305878,-6.24834710865336));
#56628=CARTESIAN_POINT('Ctrl Pts',(20.7362078848242,-20.5494411154157,-6.25252578673731));
#56629=CARTESIAN_POINT('Ctrl Pts',(20.6817007285136,-20.6133433938074,-6.25670446482125));
#56630=CARTESIAN_POINT('Ctrl Pts',(20.6262165705998,-20.6783910746135,-6.26095804270669));
#56631=CARTESIAN_POINT('Ctrl Pts',(20.5674071330978,-20.7407301867605,-6.26521162059212));
#56632=CARTESIAN_POINT('Ctrl Pts',(20.5055720700286,-20.8000076841547,-6.26946519847756));
#56633=CARTESIAN_POINT('Ctrl Pts',(20.4449358003181,-20.8581359715914,-6.27363631245551));
#56634=CARTESIAN_POINT('Ctrl Pts',(20.3813905208317,-20.9133199626604,-6.27780742643346));
#56635=CARTESIAN_POINT('Ctrl Pts',(20.3152577303048,-20.9652620272462,-6.28197854041141));
#56636=CARTESIAN_POINT('Ctrl Pts',(20.2491471312743,-21.0171866621706,-6.28614825473179));
#56637=CARTESIAN_POINT('Ctrl Pts',(20.1804511070729,-21.0658712472024,-6.29031796905216));
#56638=CARTESIAN_POINT('Ctrl Pts',(20.1095244508952,-21.1110582402958,-6.29448768337254));
#56639=CARTESIAN_POINT('Ctrl Pts',(20.0386003185924,-21.1562436254421,-6.29865724931658));
#56640=CARTESIAN_POINT('Ctrl Pts',(19.9654461005735,-21.1979314196438,-6.30282681526062));
#56641=CARTESIAN_POINT('Ctrl Pts',(19.8904446404442,-21.235908009003,-6.30699638120466));
#56642=CARTESIAN_POINT('Ctrl Pts',(19.812806221501,-21.2752198083949,-6.31131254394358));
#56643=CARTESIAN_POINT('Ctrl Pts',(19.7331887160477,-21.3105543371331,-6.3156287066825));
#56644=CARTESIAN_POINT('Ctrl Pts',(19.6520415805983,-21.3417279460835,-6.31994486942142));
#56645=CARTESIAN_POINT('Ctrl Pts',(19.573537804551,-21.3718860780012,-6.32412043361311));
#56646=CARTESIAN_POINT('Ctrl Pts',(19.493602985757,-21.3981501088936,-6.32829599780479));
#56647=CARTESIAN_POINT('Ctrl Pts',(19.4126598398381,-21.4204045093523,-6.33247156199647));
#56648=CARTESIAN_POINT('Ctrl Pts',(19.3276284480429,-21.4437829266734,-6.33685802400901));
#56649=CARTESIAN_POINT('Ctrl Pts',(19.2414847611989,-21.4627358902474,-6.34124448602155));
#56650=CARTESIAN_POINT('Ctrl Pts',(19.1547290262948,-21.4771905049784,-6.3456309480341));
#56651=CARTESIAN_POINT('Ctrl Pts',(19.0679732913907,-21.4916451197093,-6.35001741004664));
#56652=CARTESIAN_POINT('Ctrl Pts',(18.9806060935248,-21.5016013954773,-6.35440387205918));
#56653=CARTESIAN_POINT('Ctrl Pts',(18.8931294701917,-21.5070494734381,-6.35879033407172));
#56654=CARTESIAN_POINT('Ctrl Pts',(18.8096777759696,-21.512246877256,-6.36297496846477));
#56655=CARTESIAN_POINT('Ctrl Pts',(18.7258158815286,-21.5133611702432,-6.36715960285781));
#56656=CARTESIAN_POINT('Ctrl Pts',(18.6419771668657,-21.5103455197025,-6.37134423725086));
#56657=CARTESIAN_POINT('Ctrl Pts',(18.5582577862359,-21.5073341615672,-6.3755229153348));
#56658=CARTESIAN_POINT('Ctrl Pts',(18.4745619756521,-21.5002045527773,-6.37970159341874));
#56659=CARTESIAN_POINT('Ctrl Pts',(18.3913265823787,-21.4889617515555,-6.38388027150268));
#56660=CARTESIAN_POINT('Ctrl Pts',(18.306599254501,-21.4775174312019,-6.38813384938812));
#56661=CARTESIAN_POINT('Ctrl Pts',(18.2223494934531,-21.4618109801083,-6.39238742727355));
#56662=CARTESIAN_POINT('Ctrl Pts',(18.1390363521672,-21.4419032627308,-6.39664100515899));
#56663=CARTESIAN_POINT('Ctrl Pts',(18.0573383986974,-21.4223814953014,-6.40081211913694));
#56664=CARTESIAN_POINT('Ctrl Pts',(17.9765415407097,-21.3988200192303,-6.4049832331149));
#56665=CARTESIAN_POINT('Ctrl Pts',(17.8970700591984,-21.3713280625392,-6.40915434709285));
#56666=CARTESIAN_POINT('Ctrl Pts',(17.8176252451101,-21.3438453310398,-6.41332406141322));
#56667=CARTESIAN_POINT('Ctrl Pts',(17.739505358624,-21.3124348885694,-6.41749377573359));
#56668=CARTESIAN_POINT('Ctrl Pts',(17.6631189946706,-21.2772556574331,-6.42166349005396));
#56669=CARTESIAN_POINT('Ctrl Pts',(17.5867353488719,-21.2420776781248,-6.425833055998));
#56670=CARTESIAN_POINT('Ctrl Pts',(17.5120855204506,-21.2031313700067,-6.43000262194204));
#56671=CARTESIAN_POINT('Ctrl Pts',(17.4395563508724,-21.1606230188136,-6.43417218788608));
#56672=CARTESIAN_POINT('Ctrl Pts',(17.364477145166,-21.1166201264321,-6.438488350625));
#56673=CARTESIAN_POINT('Ctrl Pts',(17.291670952671,-21.068800314323,-6.44280451336393));
#56674=CARTESIAN_POINT('Ctrl Pts',(17.2215354755327,-21.0174420984932,-6.44712067610285));
#56675=CARTESIAN_POINT('Ctrl Pts',(17.1536846541853,-20.9677568711422,-6.45129624029452));
#56676=CARTESIAN_POINT('Ctrl Pts',(17.0883335592485,-20.9147605602812,-6.4554718044862));
#56677=CARTESIAN_POINT('Ctrl Pts',(17.0258081406203,-20.8587460689743,-6.45964736867787));
#56678=CARTESIAN_POINT('Ctrl Pts',(16.9601247117371,-20.7999024188732,-6.46403383069042));
#56679=CARTESIAN_POINT('Ctrl Pts',(16.8975603248984,-20.7377280904825,-6.46842029270297));
#56680=CARTESIAN_POINT('Ctrl Pts',(16.838447047551,-20.6726042556212,-6.47280675471551));
#56681=CARTESIAN_POINT('Ctrl Pts',(16.7793337702036,-20.6074804207598,-6.47719321672806));
#56682=CARTESIAN_POINT('Ctrl Pts',(16.7236719107426,-20.5394075767508,-6.48157967874061));
#56683=CARTESIAN_POINT('Ctrl Pts',(16.6717415022696,-20.4688025212726,-6.48596614075316));
#56684=CARTESIAN_POINT('Ctrl Pts',(16.6219091295864,-20.4010499743281,-6.49017538570612));
#56685=CARTESIAN_POINT('Ctrl Pts',(16.5753265021952,-20.3307132360493,-6.49438463065908));
#56686=CARTESIAN_POINT('Ctrl Pts',(16.532270626113,-20.2581346654013,-6.49859387561204));
#56687=CARTESIAN_POINT('Ctrl Pts',(16.489277141859,-20.1856612676153,-6.50279702099133));
#56688=CARTESIAN_POINT('Ctrl Pts',(16.4498004872776,-20.110952875341,-6.50700016637061));
#56689=CARTESIAN_POINT('Ctrl Pts',(16.4140760664827,-20.0343829926109,-6.5112033117499));
#56690=CARTESIAN_POINT('Ctrl Pts',(16.3783931208862,-19.9579020056842,-6.51540157737789));
#56691=CARTESIAN_POINT('Ctrl Pts',(16.3464539443372,-19.8795642299173,-6.51959984300589));
#56692=CARTESIAN_POINT('Ctrl Pts',(16.3184487740251,-19.7997689984254,-6.52379810863388));
#56693=CARTESIAN_POINT('Ctrl Pts',(16.2904693914727,-19.7200472440891,-6.52799250840909));
#56694=CARTESIAN_POINT('Ctrl Pts',(16.2664169618497,-19.6388711282231,-6.5321869081843));
#56695=CARTESIAN_POINT('Ctrl Pts',(16.2464336691667,-19.5566600282013,-6.53638130795952));
#56696=CARTESIAN_POINT('Ctrl Pts',(16.2264610773219,-19.4744929513394,-6.54057346167876));
#56697=CARTESIAN_POINT('Ctrl Pts',(16.210553397436,-19.3912924312907,-6.54476561539801));
#56698=CARTESIAN_POINT('Ctrl Pts',(16.1988026788696,-19.3074919730929,-6.54895776911726));
#56699=CARTESIAN_POINT('Ctrl Pts',(16.1870533030452,-19.2237010906829,-6.55314944380363));
#56700=CARTESIAN_POINT('Ctrl Pts',(16.1794600117858,-19.1393108539568,-6.55734111849));
#56701=CARTESIAN_POINT('Ctrl Pts',(16.1760633700115,-19.0547628189716,-6.56153279317637));
#56702=CARTESIAN_POINT('Ctrl Pts',(16.1746649834927,-19.0199546642812,-6.56325849219375));
#56703=CARTESIAN_POINT('Ctrl Pts',(16.173977295445,-18.9851198216844,-6.56498419121113));
#56704=CARTESIAN_POINT('Ctrl Pts',(16.1740005716256,-18.9502892333483,-6.5667098902285));
#56705=CARTESIAN_POINT('Origin',(18.734,-18.952,1.76670989022851));
#56706=CARTESIAN_POINT('',(20.293535888361,-16.9218650751948,-5.25018234329749));
#56707=CARTESIAN_POINT('',(20.293535888361,-16.9218650751948,-5.31661775147474));
#56708=CARTESIAN_POINT('',(20.293535888361,-16.9218650751948,1.76670989022851));
#56709=CARTESIAN_POINT('',(16.1740005630998,-18.9503020392334,-5.8332901097715));
#56710=CARTESIAN_POINT('Ctrl Pts',(20.293535888361,-16.9218650751948,-5.31661775147473));
#56711=CARTESIAN_POINT('Ctrl Pts',(20.3601996645773,-16.9730757362167,-5.32080132225747));
#56712=CARTESIAN_POINT('Ctrl Pts',(20.424260063449,-17.0275132017657,-5.32498489304021));
#56713=CARTESIAN_POINT('Ctrl Pts',(20.4854058706178,-17.0848691860597,-5.32916846382294));
#56714=CARTESIAN_POINT('Ctrl Pts',(20.5380265777208,-17.1342284567911,-5.33276875079266));
#56715=CARTESIAN_POINT('Ctrl Pts',(20.5884892430759,-17.185748417461,-5.33636903776239));
#56716=CARTESIAN_POINT('Ctrl Pts',(20.6366195645771,-17.239213150305,-5.33996932473211));
#56717=CARTESIAN_POINT('Ctrl Pts',(20.6925617159657,-17.3013555188871,-5.34415395912515));
#56718=CARTESIAN_POINT('Ctrl Pts',(20.7455602793472,-17.3663571440021,-5.3483385935182));
#56719=CARTESIAN_POINT('Ctrl Pts',(20.7953091936645,-17.4339076417706,-5.35252322791125));
#56720=CARTESIAN_POINT('Ctrl Pts',(20.8449872965599,-17.5013619897667,-5.35670190599519));
#56721=CARTESIAN_POINT('Ctrl Pts',(20.8914246675681,-17.5713576368076,-5.36088058407914));
#56722=CARTESIAN_POINT('Ctrl Pts',(20.934353739878,-17.6435492292773,-5.36505926216309));
#56723=CARTESIAN_POINT('Ctrl Pts',(20.9780522849565,-17.7170348041588,-5.36931284004852));
#56724=CARTESIAN_POINT('Ctrl Pts',(21.0181151991573,-17.7927954651137,-5.37356641793396));
#56725=CARTESIAN_POINT('Ctrl Pts',(21.0543048298795,-17.8704337762126,-5.37781999581939));
#56726=CARTESIAN_POINT('Ctrl Pts',(21.089792853992,-17.9465669171521,-5.38199110979734));
#56727=CARTESIAN_POINT('Ctrl Pts',(21.1215562334332,-18.0245051179384,-5.38616222377529));
#56728=CARTESIAN_POINT('Ctrl Pts',(21.1494168148284,-18.1038481205325,-5.39033333775325));
#56729=CARTESIAN_POINT('Ctrl Pts',(21.1772680473364,-18.1831644988157,-5.39450305207362));
#56730=CARTESIAN_POINT('Ctrl Pts',(21.2012189304412,-18.2638843090192,-5.39867276639399));
#56731=CARTESIAN_POINT('Ctrl Pts',(21.2211399893044,-18.3455886927152,-5.40284248071437));
#56732=CARTESIAN_POINT('Ctrl Pts',(21.2410603392909,-18.4272901690186,-5.40701204665841));
#56733=CARTESIAN_POINT('Ctrl Pts',(21.2569510420043,-18.5099757020134,-5.41118161260245));
#56734=CARTESIAN_POINT('Ctrl Pts',(21.2687332465284,-18.5932140346339,-5.4153511785465));
#56735=CARTESIAN_POINT('Ctrl Pts',(21.2809296988287,-18.6793789243438,-5.41966734128542));
#56736=CARTESIAN_POINT('Ctrl Pts',(21.2887232939913,-18.7661356875971,-5.42398350402433));
#56737=CARTESIAN_POINT('Ctrl Pts',(21.2920850129342,-18.8529996636308,-5.42829966676325));
#56738=CARTESIAN_POINT('Ctrl Pts',(21.2953372242362,-18.9370340547817,-5.43247523095493));
#56739=CARTESIAN_POINT('Ctrl Pts',(21.2944419142066,-19.0211683105535,-5.43665079514661));
#56740=CARTESIAN_POINT('Ctrl Pts',(21.2894259327675,-19.1049650356758,-5.44082635933829));
#56741=CARTESIAN_POINT('Ctrl Pts',(21.2841566060302,-19.1929941341762,-5.44521282135083));
#56742=CARTESIAN_POINT('Ctrl Pts',(21.2743394628619,-19.2806501283313,-5.44959928336338));
#56743=CARTESIAN_POINT('Ctrl Pts',(21.2600666971253,-19.3674359657934,-5.45398574537592));
#56744=CARTESIAN_POINT('Ctrl Pts',(21.2457939313886,-19.4542218032555,-5.45837220738846));
#56745=CARTESIAN_POINT('Ctrl Pts',(21.2270657409798,-19.5401369333207,-5.462758669401));
#56746=CARTESIAN_POINT('Ctrl Pts',(21.2040345704695,-19.6247029215675,-5.46714513141354));
#56747=CARTESIAN_POINT('Ctrl Pts',(21.1820630982548,-19.7053779033381,-5.47132976580658));
#56748=CARTESIAN_POINT('Ctrl Pts',(21.1560941354244,-19.7851254547589,-5.47551440019963));
#56749=CARTESIAN_POINT('Ctrl Pts',(21.1262230006563,-19.8635202220089,-5.47969903459268));
#56750=CARTESIAN_POINT('Ctrl Pts',(21.0963943837511,-19.9418034040111,-5.48387771267662));
#56751=CARTESIAN_POINT('Ctrl Pts',(21.0626747898134,-20.0187372003264,-5.48805639076056));
#56752=CARTESIAN_POINT('Ctrl Pts',(21.0252097777407,-20.0939096962481,-5.49223506884451));
#56753=CARTESIAN_POINT('Ctrl Pts',(20.9870732322522,-20.1704296051336,-5.49648864672994));
#56754=CARTESIAN_POINT('Ctrl Pts',(20.9450558013773,-20.2451239847431,-5.50074222461538));
#56755=CARTESIAN_POINT('Ctrl Pts',(20.8993630289916,-20.3175778823181,-5.50499580250082));
#56756=CARTESIAN_POINT('Ctrl Pts',(20.8545561001607,-20.3886271197065,-5.50916691647877));
#56757=CARTESIAN_POINT('Ctrl Pts',(20.8062153221385,-20.4575215650235,-5.51333803045672));
#56758=CARTESIAN_POINT('Ctrl Pts',(20.7545808175508,-20.5238947673893,-5.51750914443467));
#56759=CARTESIAN_POINT('Ctrl Pts',(20.7029636394197,-20.5902456975861,-5.52167885875505));
#56760=CARTESIAN_POINT('Ctrl Pts',(20.6480552119857,-20.6540767022586,-5.52584857307542));
#56761=CARTESIAN_POINT('Ctrl Pts',(20.5901376466264,-20.7150521934351,-5.53001828739579));
#56762=CARTESIAN_POINT('Ctrl Pts',(20.5322221422225,-20.776025514842,-5.53418785333984));
#56763=CARTESIAN_POINT('Ctrl Pts',(20.4712980302309,-20.8341431918207,-5.53835741928388));
#56764=CARTESIAN_POINT('Ctrl Pts',(20.4076852490905,-20.8891054919588,-5.54252698522792));
#56765=CARTESIAN_POINT('Ctrl Pts',(20.34183592104,-20.9460001987665,-5.54684314796684));
#56766=CARTESIAN_POINT('Ctrl Pts',(20.2731057379437,-20.999513169412,-5.55115931070577));
#56767=CARTESIAN_POINT('Ctrl Pts',(20.2018865153254,-21.0493576657609,-5.55547547344469));
#56768=CARTESIAN_POINT('Ctrl Pts',(20.1329872513929,-21.0975784828839,-5.55965103763637));
#56769=CARTESIAN_POINT('Ctrl Pts',(20.0617590424853,-21.1423659457519,-5.56382660182805));
#56770=CARTESIAN_POINT('Ctrl Pts',(19.9885842021594,-21.1835058771359,-5.56800216601973));
#56771=CARTESIAN_POINT('Ctrl Pts',(19.9117134746052,-21.2267236886533,-5.57238862803227));
#56772=CARTESIAN_POINT('Ctrl Pts',(19.8326948219823,-21.2659155519541,-5.57677509004481));
#56773=CARTESIAN_POINT('Ctrl Pts',(19.7519960894443,-21.3008899424784,-5.58116155205735));
#56774=CARTESIAN_POINT('Ctrl Pts',(19.6712973569064,-21.3358643330026,-5.5855480140699));
#56775=CARTESIAN_POINT('Ctrl Pts',(19.5889191146256,-21.3666211190642,-5.58993447608244));
#56776=CARTESIAN_POINT('Ctrl Pts',(19.5053461655913,-21.393029514944,-5.59432093809498));
#56777=CARTESIAN_POINT('Ctrl Pts',(19.4256185318269,-21.4182228213827,-5.59850557248803));
#56778=CARTESIAN_POINT('Ctrl Pts',(19.3445069543659,-21.4395528703719,-5.60269020688107));
#56779=CARTESIAN_POINT('Ctrl Pts',(19.2624206826504,-21.4568695738795,-5.60687484127412));
#56780=CARTESIAN_POINT('Ctrl Pts',(19.1804512505824,-21.4741616292031,-5.61105351935807));
#56781=CARTESIAN_POINT('Ctrl Pts',(19.0975103262627,-21.4874515917235,-5.61523219744201));
#56782=CARTESIAN_POINT('Ctrl Pts',(19.0140230530432,-21.4966388918203,-5.61941087552595));
#56783=CARTESIAN_POINT('Ctrl Pts',(18.9290393304525,-21.5059908676685,-5.62366445341139));
#56784=CARTESIAN_POINT('Ctrl Pts',(18.8434899394337,-21.511091508697,-5.62791803129682));
#56785=CARTESIAN_POINT('Ctrl Pts',(18.7578350465906,-21.5118890387191,-5.63217160918226));
#56786=CARTESIAN_POINT('Ctrl Pts',(18.673840740987,-21.5126711070654,-5.63634272316021));
#56787=CARTESIAN_POINT('Ctrl Pts',(18.5897454689698,-21.5093154194064,-5.64051383713816));
#56788=CARTESIAN_POINT('Ctrl Pts',(18.5059873315596,-21.5018255279589,-5.64468495111611));
#56789=CARTESIAN_POINT('Ctrl Pts',(18.4222573000014,-21.4943381498168,-5.64885466543648));
#56790=CARTESIAN_POINT('Ctrl Pts',(18.3388646361979,-21.4827193639703,-5.65302437975686));
#56791=CARTESIAN_POINT('Ctrl Pts',(18.2562442180637,-21.4670247340387,-5.65719409407723));
#56792=CARTESIAN_POINT('Ctrl Pts',(18.1736267399184,-21.4513306625893,-5.66136366002127));
#56793=CARTESIAN_POINT('Ctrl Pts',(18.0917819045973,-21.4315611221138,-5.66553322596531));
#56794=CARTESIAN_POINT('Ctrl Pts',(18.0111349162342,-21.4078228907379,-5.66970279190935));
#56795=CARTESIAN_POINT('Ctrl Pts',(17.9276524792491,-21.3832500524311,-5.67401895464827));
#56796=CARTESIAN_POINT('Ctrl Pts',(17.8454541950085,-21.354424401291,-5.6783351173872));
#56797=CARTESIAN_POINT('Ctrl Pts',(17.7649932472177,-21.3215201862534,-5.68265128012612));
#56798=CARTESIAN_POINT('Ctrl Pts',(17.6871533063382,-21.2896878225597,-5.6868268443178));
#56799=CARTESIAN_POINT('Ctrl Pts',(17.6109396593041,-21.2540387751658,-5.69100240850948));
#56800=CARTESIAN_POINT('Ctrl Pts',(17.5367393343476,-21.2147785791989,-5.69517797270115));
#56801=CARTESIAN_POINT('Ctrl Pts',(17.458791327372,-21.173535444066,-5.6995644347137));
#56802=CARTESIAN_POINT('Ctrl Pts',(17.3830658746254,-21.1283070744553,-5.70395089672624));
#56803=CARTESIAN_POINT('Ctrl Pts',(17.3099772536615,-21.0793831854912,-5.70833735873878));
#56804=CARTESIAN_POINT('Ctrl Pts',(17.2368886326976,-21.0304592965271,-5.71272382075132));
#56805=CARTESIAN_POINT('Ctrl Pts',(17.1664372628671,-20.977840296355,-5.71711028276386));
#56806=CARTESIAN_POINT('Ctrl Pts',(17.0989955289256,-20.9218630357379,-5.72149674477641));
#56807=CARTESIAN_POINT('Ctrl Pts',(17.0355419517776,-20.8691959820086,-5.72562381401755));
#56808=CARTESIAN_POINT('Ctrl Pts',(16.9745020021859,-20.8133485129554,-5.72975088325869));
#56809=CARTESIAN_POINT('Ctrl Pts',(16.9162185170907,-20.7545732940416,-5.73387795249984));
#56810=CARTESIAN_POINT('Ctrl Pts',(16.8577217299027,-20.6955829734197,-5.73802012571949));
#56811=CARTESIAN_POINT('Ctrl Pts',(16.8020020379165,-20.6336436795684,-5.74216229893914));
#56812=CARTESIAN_POINT('Ctrl Pts',(16.7493744028763,-20.5690532580101,-5.7463044721588));
#56813=CARTESIAN_POINT('Ctrl Pts',(16.6970742796337,-20.5048647949489,-5.75042086784547));
#56814=CARTESIAN_POINT('Ctrl Pts',(16.6478281605157,-20.4380584608901,-5.75453726353214));
#56815=CARTESIAN_POINT('Ctrl Pts',(16.6019085746493,-20.3689637094668,-5.75865365921882));
#56816=CARTESIAN_POINT('Ctrl Pts',(16.5560170315913,-20.2999111537828,-5.76276754104799));
#56817=CARTESIAN_POINT('Ctrl Pts',(16.5134482524877,-20.2285733472958,-5.76688142287716));
#56818=CARTESIAN_POINT('Ctrl Pts',(16.4744330306069,-20.1553108953332,-5.77099530470634));
#56819=CARTESIAN_POINT('Ctrl Pts',(16.4354291736147,-20.0820697842618,-5.77510798818763));
#56820=CARTESIAN_POINT('Ctrl Pts',(16.3999770407453,-20.0069055590536,-5.77922067166892));
#56821=CARTESIAN_POINT('Ctrl Pts',(16.3682620211175,-19.9302043831803,-5.78333335515021));
#56822=CARTESIAN_POINT('Ctrl Pts',(16.3361584999705,-19.852563635971,-5.78749641803532));
#56823=CARTESIAN_POINT('Ctrl Pts',(16.3078844956127,-19.7733484709671,-5.79165948092042));
#56824=CARTESIAN_POINT('Ctrl Pts',(16.2835818660734,-19.6929797358388,-5.79582254380553));
#56825=CARTESIAN_POINT('Ctrl Pts',(16.2595524301165,-19.6135144512041,-5.79993880837768));
#56826=CARTESIAN_POINT('Ctrl Pts',(16.2394055983612,-19.5329218806178,-5.80405507294983));
#56827=CARTESIAN_POINT('Ctrl Pts',(16.2232275631065,-19.4516216269696,-5.80817133752197));
#56828=CARTESIAN_POINT('Ctrl Pts',(16.2067736327737,-19.3689349046017,-5.81235779956356));
#56829=CARTESIAN_POINT('Ctrl Pts',(16.1944252132089,-19.2855166404035,-5.81654426160515));
#56830=CARTESIAN_POINT('Ctrl Pts',(16.186218055036,-19.2018142528269,-5.82073072364674));
#56831=CARTESIAN_POINT('Ctrl Pts',(16.1780108968631,-19.1181118652502,-5.82491718568833));
#56832=CARTESIAN_POINT('Ctrl Pts',(16.1739449655996,-19.0341258661345,-5.82910364772991));
#56833=CARTESIAN_POINT('Ctrl Pts',(16.1740005630998,-18.9503020392334,-5.8332901097715));
#56834=CARTESIAN_POINT('Ctrl Pts',(16.1712326851452,-18.9503002033939,-5.8332901097715));
#56835=CARTESIAN_POINT('Ctrl Pts',(16.1704460832798,-18.847523176255,-5.83841759033362));
#56836=CARTESIAN_POINT('Ctrl Pts',(16.2227680109981,-17.8958349863275,-5.88593700645621));
#56837=CARTESIAN_POINT('Ctrl Pts',(17.4141948925089,-16.2277744127114,-5.97584835813928));
#56838=CARTESIAN_POINT('Ctrl Pts',(19.4492535155253,-16.3260866525647,-6.06521460822567));
#56839=CARTESIAN_POINT('Ctrl Pts',(20.2230158476471,-16.8629690852954,-6.11218892275159));
#56840=CARTESIAN_POINT('Ctrl Pts',(20.2954006764134,-16.9194747298048,-6.11677130171703));
#56841=CARTESIAN_POINT('',(16.1740007055014,-18.9539005700932,-5.76670989019962));
#56842=CARTESIAN_POINT('Ctrl Pts',(16.174000705501,-18.9539005695105,-5.76670989022851));
#56843=CARTESIAN_POINT('Ctrl Pts',(16.1739381768052,-18.8696766480678,-5.77088500205647));
#56844=CARTESIAN_POINT('Ctrl Pts',(16.1780364138872,-18.7854119279347,-5.77506011388444));
#56845=CARTESIAN_POINT('Ctrl Pts',(16.1862808495761,-18.7015461508315,-5.7792352257124));
#56846=CARTESIAN_POINT('Ctrl Pts',(16.1945245019764,-18.617688341661,-5.78340994087069));
#56847=CARTESIAN_POINT('Ctrl Pts',(16.2069135252697,-18.5342298557721,-5.78758465602899));
#56848=CARTESIAN_POINT('Ctrl Pts',(16.2233814427541,-18.4516056954636,-5.79175937118728));
#56849=CARTESIAN_POINT('Ctrl Pts',(16.2398526754154,-18.3689649019825,-5.79593492676267));
#56850=CARTESIAN_POINT('Ctrl Pts',(16.2604043427349,-18.2871592164315,-5.80011048233807));
#56851=CARTESIAN_POINT('Ctrl Pts',(16.2849190524512,-18.2066125085881,-5.80428603791346));
#56852=CARTESIAN_POINT('Ctrl Pts',(16.3094630809747,-18.1259694694634,-5.80846658731951));
#56853=CARTESIAN_POINT('Ctrl Pts',(16.3379794801119,-18.0465888526479,-5.81264713672555));
#56854=CARTESIAN_POINT('Ctrl Pts',(16.370301376024,-17.9688780263803,-5.8168276861316));
#56855=CARTESIAN_POINT('Ctrl Pts',(16.4026440716432,-17.8911171918327,-5.82101092579452));
#56856=CARTESIAN_POINT('Ctrl Pts',(16.4387969424267,-17.815028700182,-5.82519416545745));
#56857=CARTESIAN_POINT('Ctrl Pts',(16.4785465454209,-17.7409964020585,-5.82937740512037));
#56858=CARTESIAN_POINT('Ctrl Pts',(16.5183679957913,-17.6668302906143,-5.8335682059857));
#56859=CARTESIAN_POINT('Ctrl Pts',(16.5617989238527,-17.5947281861652,-5.83775900685103));
#56860=CARTESIAN_POINT('Ctrl Pts',(16.6085819963934,-17.5250457926251,-5.84194980771636));
#56861=CARTESIAN_POINT('Ctrl Pts',(16.6388616407137,-17.4799449051204,-5.84466224092623));
#56862=CARTESIAN_POINT('Ctrl Pts',(16.67054468148,-17.4358570345709,-5.8473746741361));
#56863=CARTESIAN_POINT('Ctrl Pts',(16.7035527014987,-17.392870830236,-5.85008710734598));
#56864=CARTESIAN_POINT('Ctrl Pts',(16.754476165831,-17.3265534188316,-5.85427174173903));
#56865=CARTESIAN_POINT('Ctrl Pts',(16.8087468503131,-17.262610070515,-5.85845637613208));
#56866=CARTESIAN_POINT('Ctrl Pts',(16.8661152556941,-17.201398222899,-5.86264101052513));
#56867=CARTESIAN_POINT('Ctrl Pts',(16.9234020042507,-17.1402735027716,-5.86681968860906));
#56868=CARTESIAN_POINT('Ctrl Pts',(16.9837774037102,-17.081872893435,-5.870998366693));
#56869=CARTESIAN_POINT('Ctrl Pts',(17.0469505633854,-17.0265223453859,-5.87517704477694));
#56870=CARTESIAN_POINT('Ctrl Pts',(17.1112560565461,-16.9701796785426,-5.87943062266237));
#56871=CARTESIAN_POINT('Ctrl Pts',(17.1784603025299,-16.916997875599,-5.88368420054781));
#56872=CARTESIAN_POINT('Ctrl Pts',(17.248215753932,-16.8672829510612,-5.88793777843324));
#56873=CARTESIAN_POINT('Ctrl Pts',(17.316618859792,-16.8185318473463,-5.8921088924112));
#56874=CARTESIAN_POINT('Ctrl Pts',(17.3874747417493,-16.7731146765033,-5.89628000638915));
#56875=CARTESIAN_POINT('Ctrl Pts',(17.4604222489452,-16.7312794610716,-5.9004511203671));
#56876=CARTESIAN_POINT('Ctrl Pts',(17.5333452779006,-16.6894582838505,-5.90462083468747));
#56877=CARTESIAN_POINT('Ctrl Pts',(17.6083581394473,-16.6512169036016,-5.90879054900784));
#56878=CARTESIAN_POINT('Ctrl Pts',(17.6850725337909,-16.616758862423,-5.91296026332821));
#56879=CARTESIAN_POINT('Ctrl Pts',(17.7617841983071,-16.5823020474093,-5.91712982927226));
#56880=CARTESIAN_POINT('Ctrl Pts',(17.8401968552427,-16.5516284915074,-5.9212993952163));
#56881=CARTESIAN_POINT('Ctrl Pts',(17.9199007999992,-16.5248942147986,-5.92546896116034));
#56882=CARTESIAN_POINT('Ctrl Pts',(18.0024070371279,-16.497219993901,-5.92978512389926));
#56883=CARTESIAN_POINT('Ctrl Pts',(18.0862965548752,-16.4737673840698,-5.93410128663819));
#56884=CARTESIAN_POINT('Ctrl Pts',(18.17109806773,-16.454653124885,-5.93841744937711));
#56885=CARTESIAN_POINT('Ctrl Pts',(18.2531371802229,-16.4361615106827,-5.94259301356879));
#56886=CARTESIAN_POINT('Ctrl Pts',(18.3360293116297,-16.4217299783602,-5.94676857776046));
#56887=CARTESIAN_POINT('Ctrl Pts',(18.4193394847876,-16.4114117295071,-5.95094414195214));
#56888=CARTESIAN_POINT('Ctrl Pts',(18.5068574567408,-16.4005723304336,-5.95533060396469));
#56889=CARTESIAN_POINT('Ctrl Pts',(18.5948362284715,-16.3942727005954,-5.95971706597723));
#56890=CARTESIAN_POINT('Ctrl Pts',(18.6827702698547,-16.3925126461048,-5.96410352798978));
#56891=CARTESIAN_POINT('Ctrl Pts',(18.7707043112378,-16.3907525916143,-5.96848999000232));
#56892=CARTESIAN_POINT('Ctrl Pts',(18.8585930447508,-16.3935320181048,-5.97287645201487));
#56893=CARTESIAN_POINT('Ctrl Pts',(18.9459382820312,-16.4007880988421,-5.97726291402741));
#56894=CARTESIAN_POINT('Ctrl Pts',(19.0292570355294,-16.4077096851946,-5.98144716675294));
#56895=CARTESIAN_POINT('Ctrl Pts',(19.1123913980881,-16.418730040739,-5.98563141947846));
#56896=CARTESIAN_POINT('Ctrl Pts',(19.194905891231,-16.4338328571303,-5.98981567220399));
#56897=CARTESIAN_POINT('Ctrl Pts',(19.2773086561184,-16.4489152236435,-5.99399425926716));
#56898=CARTESIAN_POINT('Ctrl Pts',(19.3590927697209,-16.4680689925776,-5.99817284633033));
#56899=CARTESIAN_POINT('Ctrl Pts',(19.4398267332537,-16.4912260114703,-6.0023514333935));
#56900=CARTESIAN_POINT('Ctrl Pts',(19.5204679325001,-16.5143564226722,-6.00652521921033));
#56901=CARTESIAN_POINT('Ctrl Pts',(19.6000609401166,-16.5414808153857,-6.01069900502716));
#56902=CARTESIAN_POINT('Ctrl Pts',(19.6781847982246,-16.5724800764016,-6.01487279084399));
#56903=CARTESIAN_POINT('Ctrl Pts',(19.756255136842,-16.6034581010796,-6.01904371736923));
#56904=CARTESIAN_POINT('Ctrl Pts',(19.8328578987203,-16.638305552342,-6.02321464389447));
#56905=CARTESIAN_POINT('Ctrl Pts',(19.9075887387112,-16.6768539668034,-6.02738557041971));
#56906=CARTESIAN_POINT('Ctrl Pts',(19.9823054028888,-16.715395068954,-6.03155570575518));
#56907=CARTESIAN_POINT('Ctrl Pts',(20.0551504373947,-16.7576355380431,-6.03572584109066));
#56908=CARTESIAN_POINT('Ctrl Pts',(20.1257419130199,-16.8033598608553,-6.03989597642613));
#56909=CARTESIAN_POINT('Ctrl Pts',(20.1832317946324,-16.8405978684476,-6.04329214550492));
#56910=CARTESIAN_POINT('Ctrl Pts',(20.2392273264478,-16.8801456060531,-6.04668831458371));
#56911=CARTESIAN_POINT('Ctrl Pts',(20.293535888361,-16.9218650751948,-6.05008448366249));
#56912=CARTESIAN_POINT('Ctrl Pts',(20.293535888361,-16.9218650751948,-5.25018234329749));
#56913=CARTESIAN_POINT('Ctrl Pts',(20.3601377623853,-16.9730281833724,-5.25435377502357));
#56914=CARTESIAN_POINT('Ctrl Pts',(20.4242724026374,-17.0275130355736,-5.25852520674965));
#56915=CARTESIAN_POINT('Ctrl Pts',(20.4855962926596,-17.0850478239813,-5.26269663847572));
#56916=CARTESIAN_POINT('Ctrl Pts',(20.5468968472374,-17.1425607188029,-5.2668664828561));
#56917=CARTESIAN_POINT('Ctrl Pts',(20.6053884404635,-17.2031209306373,-5.27103632723647));
#56918=CARTESIAN_POINT('Ctrl Pts',(20.6607620047844,-17.2664175555852,-5.27520617161685));
#56919=CARTESIAN_POINT('Ctrl Pts',(20.716131108673,-17.3297090818852,-5.27937568010935));
#56920=CARTESIAN_POINT('Ctrl Pts',(20.7683823803764,-17.3957362366199,-5.28354518860186));
#56921=CARTESIAN_POINT('Ctrl Pts',(20.817245809119,-17.4641536037655,-5.28771469709437));
#56922=CARTESIAN_POINT('Ctrl Pts',(20.8661199594387,-17.5325859829986,-5.29188512045731));
#56923=CARTESIAN_POINT('Ctrl Pts',(20.9116045244801,-17.6034092410065,-5.29605554382025));
#56924=CARTESIAN_POINT('Ctrl Pts',(20.9534725337246,-17.6762485853261,-5.3002259671832));
#56925=CARTESIAN_POINT('Ctrl Pts',(20.9953878213432,-17.7491701816048,-5.30440109988962));
#56926=CARTESIAN_POINT('Ctrl Pts',(21.033678175198,-17.824112007304,-5.30857623259604));
#56927=CARTESIAN_POINT('Ctrl Pts',(21.0681626420736,-17.9006747599586,-5.31275136530246));
#56928=CARTESIAN_POINT('Ctrl Pts',(21.1026701970053,-17.9772887729425,-5.31692929334565));
#56929=CARTESIAN_POINT('Ctrl Pts',(21.1333666264305,-18.0555254448552,-5.32110722138883));
#56930=CARTESIAN_POINT('Ctrl Pts',(21.1601200340366,-18.1349678216579,-5.32528514943202));
#56931=CARTESIAN_POINT('Ctrl Pts',(21.1869161602422,-18.2145370483607,-5.32946974859679));
#56932=CARTESIAN_POINT('Ctrl Pts',(21.2097565782892,-18.2953153796072,-5.33365434776156));
#56933=CARTESIAN_POINT('Ctrl Pts',(21.228560024071,-18.3768736779567,-5.33783894692634));
#56934=CARTESIAN_POINT('Ctrl Pts',(21.2338697296436,-18.3999040605933,-5.33902059149097));
#56935=CARTESIAN_POINT('Ctrl Pts',(21.2388578513853,-18.4229965973846,-5.34020223605561));
#56936=CARTESIAN_POINT('Ctrl Pts',(21.2435233083642,-18.4461415565825,-5.34138388062024));
#56937=CARTESIAN_POINT('Ctrl Pts',(21.2600453931921,-18.528106298929,-5.34556851501329));
#56938=CARTESIAN_POINT('Ctrl Pts',(21.2725783676242,-18.6110338790214,-5.34975314940634));
#56939=CARTESIAN_POINT('Ctrl Pts',(21.2810167729394,-18.6945013429835,-5.35393778379939));
#56940=CARTESIAN_POINT('Ctrl Pts',(21.2894431672292,-18.7778500013417,-5.35811646188332));
#56941=CARTESIAN_POINT('Ctrl Pts',(21.2937865229904,-18.8617365633854,-5.36229513996726));
#56942=CARTESIAN_POINT('Ctrl Pts',(21.293992315731,-18.9457275683921,-5.3664738180512));
#56943=CARTESIAN_POINT('Ctrl Pts',(21.2942017971586,-19.0312240518004,-5.37072739593664));
#56944=CARTESIAN_POINT('Ctrl Pts',(21.2901238296771,-19.1168282866478,-5.37498097382208));
#56945=CARTESIAN_POINT('Ctrl Pts',(21.2817561480521,-19.202077208203,-5.37923455170751));
#56946=CARTESIAN_POINT('Ctrl Pts',(21.2735506902637,-19.2856734130643,-5.38340566568546));
#56947=CARTESIAN_POINT('Ctrl Pts',(21.2612204100085,-19.3689274796566,-5.38757677966342));
#56948=CARTESIAN_POINT('Ctrl Pts',(21.2448156932502,-19.4514041995501,-5.39174789364137));
#56949=CARTESIAN_POINT('Ctrl Pts',(21.2284164812531,-19.5338532435837,-5.39591760796174));
#56950=CARTESIAN_POINT('Ctrl Pts',(21.2079456377351,-19.6155250081443,-5.40008732228211));
#56951=CARTESIAN_POINT('Ctrl Pts',(21.1835049170499,-19.695993051949,-5.40425703660248));
#56952=CARTESIAN_POINT('Ctrl Pts',(21.1590650660704,-19.7764582323555,-5.40842660254653));
#56953=CARTESIAN_POINT('Ctrl Pts',(21.1306557533066,-19.855719337241,-5.41259616849058));
#56954=CARTESIAN_POINT('Ctrl Pts',(21.0984286192895,-19.9333650209198,-5.41676573443462));
#56955=CARTESIAN_POINT('Ctrl Pts',(21.0650684189968,-20.0137406310503,-5.42108189717355));
#56956=CARTESIAN_POINT('Ctrl Pts',(21.0276171353222,-20.0923846228544,-5.42539805991247));
#56957=CARTESIAN_POINT('Ctrl Pts',(20.9862964849991,-20.1688650474316,-5.42971422265139));
#56958=CARTESIAN_POINT('Ctrl Pts',(20.946321850514,-20.2428541302226,-5.43388978684307));
#56959=CARTESIAN_POINT('Ctrl Pts',(20.9027263517804,-20.314818059135,-5.43806535103475));
#56960=CARTESIAN_POINT('Ctrl Pts',(20.8557557370743,-20.3843940073151,-5.44224091522644));
#56961=CARTESIAN_POINT('Ctrl Pts',(20.8064127482816,-20.4574840712366,-5.44662737723898));
#56962=CARTESIAN_POINT('Ctrl Pts',(20.7533450801509,-20.5279381144881,-5.45101383925152));
#56963=CARTESIAN_POINT('Ctrl Pts',(20.6968850924152,-20.5953752200804,-5.45540030126406));
#56964=CARTESIAN_POINT('Ctrl Pts',(20.6404251046795,-20.6628123256726,-5.4597867632766));
#56965=CARTESIAN_POINT('Ctrl Pts',(20.5805732479923,-20.7272321203106,-5.46417322528913));
#56966=CARTESIAN_POINT('Ctrl Pts',(20.5177042670233,-20.788300380603,-5.46855968730167));
#56967=CARTESIAN_POINT('Ctrl Pts',(20.4577279810629,-20.8465587997145,-5.47274432169472));
#56968=CARTESIAN_POINT('Ctrl Pts',(20.3947828711327,-20.9019841740837,-5.47692895608777));
#56969=CARTESIAN_POINT('Ctrl Pts',(20.3291674917033,-20.9542588927042,-5.48111359048082));
#56970=CARTESIAN_POINT('Ctrl Pts',(20.2636455076449,-21.0064592047331,-5.48529226856476));
#56971=CARTESIAN_POINT('Ctrl Pts',(20.1954611603976,-21.0555174845772,-5.4894709466487));
#56972=CARTESIAN_POINT('Ctrl Pts',(20.124949408759,-21.1011532616994,-5.49364962473264));
#56973=CARTESIAN_POINT('Ctrl Pts',(20.0531737846481,-21.1476070273286,-5.49790320261808));
#56974=CARTESIAN_POINT('Ctrl Pts',(19.9789868438524,-21.1905140507392,-5.50215678050351));
#56975=CARTESIAN_POINT('Ctrl Pts',(19.9027767244008,-21.2296217790711,-5.50641035838895));
#56976=CARTESIAN_POINT('Ctrl Pts',(19.8280440868267,-21.2679713277768,-5.5105814723669));
#56977=CARTESIAN_POINT('Ctrl Pts',(19.7513664452244,-21.3026673605995,-5.51475258634485));
#56978=CARTESIAN_POINT('Ctrl Pts',(19.6731370139766,-21.3335166740922,-5.5189237003228));
#56979=CARTESIAN_POINT('Ctrl Pts',(19.5949338333701,-21.3643556357998,-5.52309341464318));
#56980=CARTESIAN_POINT('Ctrl Pts',(19.5151803248755,-21.3913502731114,-5.52726312896355));
#56981=CARTESIAN_POINT('Ctrl Pts',(19.4342901358277,-21.4143553207574,-5.53143284328392));
#56982=CARTESIAN_POINT('Ctrl Pts',(19.3534028252,-21.4373595497851,-5.53560240922797));
#56983=CARTESIAN_POINT('Ctrl Pts',(19.2713793571593,-21.4563743463907,-5.53977197517202));
#56984=CARTESIAN_POINT('Ctrl Pts',(19.1886476884737,-21.4713045626453,-5.54394154111606));
#56985=CARTESIAN_POINT('Ctrl Pts',(19.1030072763778,-21.486759706885,-5.54825770385498));
#56986=CARTESIAN_POINT('Ctrl Pts',(19.0166084554189,-21.4978376052711,-5.5525738665939));
#56987=CARTESIAN_POINT('Ctrl Pts',(18.9299344373273,-21.5044908807416,-5.55689002933282));
#56988=CARTESIAN_POINT('Ctrl Pts',(18.8460838162585,-21.5109274264636,-5.5610655935245));
#56989=CARTESIAN_POINT('Ctrl Pts',(18.7619761239715,-21.5132232209822,-5.56524115771618));
#56990=CARTESIAN_POINT('Ctrl Pts',(18.6780494593124,-21.511388508413,-5.56941672190786));
#56991=CARTESIAN_POINT('Ctrl Pts',(18.589883858338,-21.5094611288736,-5.5738031839204));
#56992=CARTESIAN_POINT('Ctrl Pts',(18.5019186353064,-21.5029750554617,-5.57818964593294));
#56993=CARTESIAN_POINT('Ctrl Pts',(18.4146539811436,-21.492003566974,-5.58257610794548));
#56994=CARTESIAN_POINT('Ctrl Pts',(18.3273893269809,-21.4810320784863,-5.58696256995802));
#56995=CARTESIAN_POINT('Ctrl Pts',(18.2408257994993,-21.4655753517935,-5.59134903197056));
#56996=CARTESIAN_POINT('Ctrl Pts',(18.1554472698611,-21.4457675790757,-5.59573549398311));
#56997=CARTESIAN_POINT('Ctrl Pts',(18.073997132933,-21.4268711913428,-5.59992012837615));
#56998=CARTESIAN_POINT('Ctrl Pts',(17.9933221701875,-21.4039450190917,-5.60410476276919));
#56999=CARTESIAN_POINT('Ctrl Pts',(17.9138510440903,-21.3770681825714,-5.60828939716223));
#57000=CARTESIAN_POINT('Ctrl Pts',(17.8344930353043,-21.3502296019011,-5.61246807524618));
#57001=CARTESIAN_POINT('Ctrl Pts',(17.7563358916499,-21.3194516726888,-5.61664675333012));
#57002=CARTESIAN_POINT('Ctrl Pts',(17.6797967513075,-21.2848642288925,-5.62082543141407));
#57003=CARTESIAN_POINT('Ctrl Pts',(17.6018857018822,-21.2496568300238,-5.62507900929951));
#57004=CARTESIAN_POINT('Ctrl Pts',(17.5256517013915,-21.2105021111286,-5.62933258718494));
#57005=CARTESIAN_POINT('Ctrl Pts',(17.4515171985767,-21.167589732792,-5.63358616507038));
#57006=CARTESIAN_POINT('Ctrl Pts',(17.3788199377604,-21.1255092946461,-5.63775727904834));
#57007=CARTESIAN_POINT('Ctrl Pts',(17.3081419118298,-21.079815837063,-5.64192839302629));
#57008=CARTESIAN_POINT('Ctrl Pts',(17.2398584137962,-21.0307354137495,-5.64609950700425));
#57009=CARTESIAN_POINT('Ctrl Pts',(17.17159782895,-20.9816714598462,-5.65026922132462));
#57010=CARTESIAN_POINT('Ctrl Pts',(17.1057305494617,-20.9292230656517,-5.65443893564499));
#57011=CARTESIAN_POINT('Ctrl Pts',(17.0426026198914,-20.8736594137781,-5.65860864996536));
#57012=CARTESIAN_POINT('Ctrl Pts',(16.9794769366837,-20.8180977390976,-5.66277821590941));
#57013=CARTESIAN_POINT('Ctrl Pts',(16.9190907543429,-20.759421331729,-5.66694778185345));
#57014=CARTESIAN_POINT('Ctrl Pts',(16.8617557221014,-20.6979385338196,-5.6711173477975));
#57015=CARTESIAN_POINT('Ctrl Pts',(16.8024048608569,-20.6342940765829,-5.67543351053642));
#57016=CARTESIAN_POINT('Ctrl Pts',(16.7463240583277,-20.5676425973537,-5.67974967327534));
#57017=CARTESIAN_POINT('Ctrl Pts',(16.6938147044704,-20.4983647564223,-5.68406583601426));
#57018=CARTESIAN_POINT('Ctrl Pts',(16.643015837292,-20.4313436338724,-5.68824140020594));
#57019=CARTESIAN_POINT('Ctrl Pts',(16.5955595388127,-20.3618650450196,-5.69241696439762));
#57020=CARTESIAN_POINT('Ctrl Pts',(16.5516743299489,-20.2903029066083,-5.6965925285893));
#57021=CARTESIAN_POINT('Ctrl Pts',(16.5055725835126,-20.2151263347087,-5.70097899060184));
#57022=CARTESIAN_POINT('Ctrl Pts',(16.4634124379741,-20.1376507144176,-5.70536545261438));
#57023=CARTESIAN_POINT('Ctrl Pts',(16.4254030213234,-20.0583362915701,-5.70975191462692));
#57024=CARTESIAN_POINT('Ctrl Pts',(16.3873936046726,-19.9790218687225,-5.71413837663946));
#57025=CARTESIAN_POINT('Ctrl Pts',(16.3535350701226,-19.897869208087,-5.718524838652));
#57026=CARTESIAN_POINT('Ctrl Pts',(16.323976493569,-19.8153578044185,-5.72291130066454));
#57027=CARTESIAN_POINT('Ctrl Pts',(16.2911969765866,-19.7238552940422,-5.72777574688618));
#57028=CARTESIAN_POINT('Ctrl Pts',(16.2636032939182,-19.630402505787,-5.73264019310782));
#57029=CARTESIAN_POINT('Ctrl Pts',(16.2413973788046,-19.5355513454785,-5.73750463932946));
#57030=CARTESIAN_POINT('Ctrl Pts',(16.2191773325018,-19.4406398246901,-5.74237218114115));
#57031=CARTESIAN_POINT('Ctrl Pts',(16.2023520711407,-19.3443282665182,-5.74723972295285));
#57032=CARTESIAN_POINT('Ctrl Pts',(16.1910760934491,-19.2471914725933,-5.75210726476454));
#57033=CARTESIAN_POINT('Ctrl Pts',(16.1798001157575,-19.1500546786684,-5.75697480657623));
#57034=CARTESIAN_POINT('Ctrl Pts',(16.1740736044194,-19.0520927805192,-5.76184234838793));
#57035=CARTESIAN_POINT('Ctrl Pts',(16.1740007055014,-18.9539005700933,-5.76670989019962));
#57036=CARTESIAN_POINT('Origin',(18.734,-18.952,1.76670989022851));
#57037=CARTESIAN_POINT('',(20.2961058236219,-16.9185141606304,-4.4501059332472));
#57038=CARTESIAN_POINT('',(20.2910030755688,-16.9251725897442,-4.51667470355372));
#57039=CARTESIAN_POINT('',(20.293535888361,-16.9218650751948,1.76670989022851));
#57040=CARTESIAN_POINT('',(16.1741505039397,-18.9508032548666,-5.03329016024815));
#57041=CARTESIAN_POINT('Ctrl Pts',(20.2910030755688,-16.9251725897442,-4.51667470355372));
#57042=CARTESIAN_POINT('Ctrl Pts',(20.612749297949,-17.1716047206165,-4.53675463058365));
#57043=CARTESIAN_POINT('Ctrl Pts',(21.4403820710291,-18.1629200661967,-4.59922649317405));
#57044=CARTESIAN_POINT('Ctrl Pts',(21.3050298972618,-20.5498409932103,-4.70409029132494));
#57045=CARTESIAN_POINT('Ctrl Pts',(18.7821183084785,-21.9787102934683,-4.83126609800637));
#57046=CARTESIAN_POINT('Ctrl Pts',(16.5671405548292,-20.815635979695,-4.94099937082189));
#57047=CARTESIAN_POINT('Ctrl Pts',(16.1797898378084,-19.4541224957223,-5.00834070807693));
#57048=CARTESIAN_POINT('Ctrl Pts',(16.1776748285763,-18.9508059208577,-5.0332901097715));
#57049=CARTESIAN_POINT('Ctrl Pts',(16.1740002797795,-18.9508031412289,-5.03329016239971));
#57050=CARTESIAN_POINT('Ctrl Pts',(16.1740435234788,-18.8583078019676,-5.03786858507912));
#57051=CARTESIAN_POINT('Ctrl Pts',(16.1791038614083,-18.7659792628304,-5.04244700775854));
#57052=CARTESIAN_POINT('Ctrl Pts',(16.1891023385012,-18.6743385289637,-5.04702543043795));
#57053=CARTESIAN_POINT('Ctrl Pts',(16.1991318881351,-18.5824130006799,-5.05161808160685));
#57054=CARTESIAN_POINT('Ctrl Pts',(16.2141301908472,-18.4911798450087,-5.05621073277575));
#57055=CARTESIAN_POINT('Ctrl Pts',(16.2339673694791,-18.401148979913,-5.06080338394464));
#57056=CARTESIAN_POINT('Ctrl Pts',(16.253896242195,-18.3107019620039,-5.06541726388551));
#57057=CARTESIAN_POINT('Ctrl Pts',(16.2787086950666,-18.2214686541854,-5.07003114382637));
#57058=CARTESIAN_POINT('Ctrl Pts',(16.3082244096464,-18.1339457320907,-5.07464502376723));
#57059=CARTESIAN_POINT('Ctrl Pts',(16.3316224115872,-18.064563657823,-5.07830258630123));
#57060=CARTESIAN_POINT('Ctrl Pts',(16.3579750606108,-17.996256071474,-5.08196014883524));
#57061=CARTESIAN_POINT('Ctrl Pts',(16.3871718743356,-17.9292596866308,-5.08561771136924));
#57062=CARTESIAN_POINT('Ctrl Pts',(16.4205760854036,-17.8526088095457,-5.08980234576229));
#57063=CARTESIAN_POINT('Ctrl Pts',(16.4578017058021,-17.7774535557437,-5.09398698015534));
#57064=CARTESIAN_POINT('Ctrl Pts',(16.4986929228155,-17.7042010295369,-5.09817161454839));
#57065=CARTESIAN_POINT('Ctrl Pts',(16.5395259362428,-17.6310527692343,-5.10235029263233));
#57066=CARTESIAN_POINT('Ctrl Pts',(16.5840139603303,-17.559802255246,-5.10652897071626));
#57067=CARTESIAN_POINT('Ctrl Pts',(16.6319534129312,-17.4908360304906,-5.1107076488002));
#57068=CARTESIAN_POINT('Ctrl Pts',(16.6807521457665,-17.4206336357216,-5.11496122668564));
#57069=CARTESIAN_POINT('Ctrl Pts',(16.7331270652481,-17.3527986694292,-5.11921480457108));
#57070=CARTESIAN_POINT('Ctrl Pts',(16.7888147952352,-17.2877120083459,-5.12346838245651));
#57071=CARTESIAN_POINT('Ctrl Pts',(16.8434229099109,-17.2238871791938,-5.12763949643446));
#57072=CARTESIAN_POINT('Ctrl Pts',(16.9012162179242,-17.1627054093257,-5.13181061041241));
#57073=CARTESIAN_POINT('Ctrl Pts',(16.961904139826,-17.1044945839445,-5.13598172439036));
#57074=CARTESIAN_POINT('Ctrl Pts',(17.0225716973095,-17.046303291768,-5.14015143871074));
#57075=CARTESIAN_POINT('Ctrl Pts',(17.0861316079121,-16.9910812823427,-5.14432115303111));
#57076=CARTESIAN_POINT('Ctrl Pts',(17.1522562065725,-16.9391198316955,-5.14849086735148));
#57077=CARTESIAN_POINT('Ctrl Pts',(17.218378452236,-16.8871602300597,-5.15266043329552));
#57078=CARTESIAN_POINT('Ctrl Pts',(17.2870648422621,-16.838461240085,-5.15682999923957));
#57079=CARTESIAN_POINT('Ctrl Pts',(17.3579554657569,-16.7932731901003,-5.16099956518361));
#57080=CARTESIAN_POINT('Ctrl Pts',(17.4313385161206,-16.7464963840237,-5.16531572792253));
#57081=CARTESIAN_POINT('Ctrl Pts',(17.5070832408524,-16.7034822843461,-5.16963189066145));
#57082=CARTESIAN_POINT('Ctrl Pts',(17.5847604857695,-16.6644579700187,-5.17394805340038));
#57083=CARTESIAN_POINT('Ctrl Pts',(17.6599074026035,-16.6267048686258,-5.17812361759205));
#57084=CARTESIAN_POINT('Ctrl Pts',(17.7368624194977,-16.5926857570979,-5.18229918178373));
#57085=CARTESIAN_POINT('Ctrl Pts',(17.8152162748901,-16.5625572895604,-5.18647474597541));
#57086=CARTESIAN_POINT('Ctrl Pts',(17.8975275972498,-16.5309071047512,-5.19086120798795));
#57087=CARTESIAN_POINT('Ctrl Pts',(17.9813822273943,-16.5035511069692,-5.1952476700005));
#57088=CARTESIAN_POINT('Ctrl Pts',(18.0662895457779,-16.4806111699446,-5.19963413201304));
#57089=CARTESIAN_POINT('Ctrl Pts',(18.1511968641614,-16.4576712329201,-5.20402059402558));
#57090=CARTESIAN_POINT('Ctrl Pts',(18.2371562875636,-16.439147404523,-5.20840705603812));
#57091=CARTESIAN_POINT('Ctrl Pts',(18.3236691980734,-16.4250990060965,-5.21279351805067));
#57092=CARTESIAN_POINT('Ctrl Pts',(18.408989825773,-16.4112442165067,-5.21711952777667));
#57093=CARTESIAN_POINT('Ctrl Pts',(18.4951771225028,-16.4016888928814,-5.22144553750267));
#57094=CARTESIAN_POINT('Ctrl Pts',(18.5817594763928,-16.3965308017955,-5.22577154722868));
#57095=CARTESIAN_POINT('Ctrl Pts',(18.6653746429516,-16.3915494790907,-5.22994930409856));
#57096=CARTESIAN_POINT('Ctrl Pts',(18.7493577227615,-16.3906689763753,-5.23412706096844));
#57097=CARTESIAN_POINT('Ctrl Pts',(18.8332735543601,-16.3939255754758,-5.23830481783833));
#57098=CARTESIAN_POINT('Ctrl Pts',(18.9171071872597,-16.3971789846156,-5.24247848243894));
#57099=CARTESIAN_POINT('Ctrl Pts',(19.0008732457144,-16.4045614313944,-5.24665214703955));
#57100=CARTESIAN_POINT('Ctrl Pts',(19.0841345041026,-16.4160572110087,-5.25082581164016));
#57101=CARTESIAN_POINT('Ctrl Pts',(19.1673391847203,-16.4275451789998,-5.25499664014818));
#57102=CARTESIAN_POINT('Ctrl Pts',(19.2500392922831,-16.4431408649386,-5.2591674686562));
#57103=CARTESIAN_POINT('Ctrl Pts',(19.3318020312623,-16.4627766810873,-5.26333829716423));
#57104=CARTESIAN_POINT('Ctrl Pts',(19.413533738698,-16.4824050448233,-5.26750754271101));
#57105=CARTESIAN_POINT('Ctrl Pts',(19.4943283380498,-16.5060703831817,-5.2716767882578));
#57106=CARTESIAN_POINT('Ctrl Pts',(19.5737638927826,-16.5336541594762,-5.27584603380458));
#57107=CARTESIAN_POINT('Ctrl Pts',(19.6532187797483,-16.561244648835,-5.28001629402076));
#57108=CARTESIAN_POINT('Ctrl Pts',(19.7313135247755,-16.5927553354863,-5.28418655423693));
#57109=CARTESIAN_POINT('Ctrl Pts',(19.8076429176265,-16.6280183121568,-5.2883568144531));
#57110=CARTESIAN_POINT('Ctrl Pts',(19.8839842511284,-16.6632868052199,-5.29252772704734));
#57111=CARTESIAN_POINT('Ctrl Pts',(19.9585592703134,-16.7023085526977,-5.29669863964157));
#57112=CARTESIAN_POINT('Ctrl Pts',(20.0309859639485,-16.7448689641708,-5.3008695522358));
#57113=CARTESIAN_POINT('Ctrl Pts',(20.1034742983524,-16.7874655978756,-5.30504401460217));
#57114=CARTESIAN_POINT('Ctrl Pts',(20.1738102696017,-16.8336066600712,-5.30921847696853));
#57115=CARTESIAN_POINT('Ctrl Pts',(20.2416402523474,-16.8830338645831,-5.31339293933489));
#57116=CARTESIAN_POINT('Ctrl Pts',(20.2591066893483,-16.895761527466,-5.31446787671484));
#57117=CARTESIAN_POINT('Ctrl Pts',(20.2764071271508,-16.9087068769371,-5.31554281409479));
#57118=CARTESIAN_POINT('Ctrl Pts',(20.293535888361,-16.9218650751948,-5.31661775147473));
#57119=CARTESIAN_POINT('',(16.1737368696253,-18.9528355653615,-4.96670989022851));
#57120=CARTESIAN_POINT('Ctrl Pts',(16.1740001363332,-18.952835479442,-4.96670989022851));
#57121=CARTESIAN_POINT('Ctrl Pts',(16.1739730621524,-18.8698772454868,-4.97085977152528));
#57122=CARTESIAN_POINT('Ctrl Pts',(16.1779827035226,-18.7867551328103,-4.97500965282205));
#57123=CARTESIAN_POINT('Ctrl Pts',(16.1860506816107,-18.7038986680416,-4.97915953411883));
#57124=CARTESIAN_POINT('Ctrl Pts',(16.194107496698,-18.6211568449803,-4.98330367356457));
#57125=CARTESIAN_POINT('Ctrl Pts',(16.2062114544436,-18.5386804021303,-4.98744781301032));
#57126=CARTESIAN_POINT('Ctrl Pts',(16.2223321624274,-18.4568993297282,-4.99159195245607));
#57127=CARTESIAN_POINT('Ctrl Pts',(16.2384354396283,-18.3752066844675,-4.99573161098228));
#57128=CARTESIAN_POINT('Ctrl Pts',(16.258546748188,-18.2942083730103,-4.99987126950849));
#57129=CARTESIAN_POINT('Ctrl Pts',(16.2825840079951,-18.2143282341429,-5.0040109280347));
#57130=CARTESIAN_POINT('Ctrl Pts',(16.3066073287289,-18.1344944173239,-5.00814818599595));
#57131=CARTESIAN_POINT('Ctrl Pts',(16.33455194816,-18.0557779336924,-5.0122854439572));
#57132=CARTESIAN_POINT('Ctrl Pts',(16.3662852025775,-17.9785902003439,-5.01642270191845));
#57133=CARTESIAN_POINT('Ctrl Pts',(16.3980099615293,-17.9014231313034,-5.020558852274));
#57134=CARTESIAN_POINT('Ctrl Pts',(16.4335211635118,-17.8257844328042,-5.02469500262956));
#57135=CARTESIAN_POINT('Ctrl Pts',(16.4726375176037,-17.7520667838541,-5.02883115298511));
#57136=CARTESIAN_POINT('Ctrl Pts',(16.5117556109323,-17.6783458571842,-5.03296748724699));
#57137=CARTESIAN_POINT('Ctrl Pts',(16.5544789534253,-17.6065465624547,-5.03710382150887));
#57138=CARTESIAN_POINT('Ctrl Pts',(16.6005803897996,-17.5370368319944,-5.04124015577075));
#57139=CARTESIAN_POINT('Ctrl Pts',(16.646728500548,-17.4674567279532,-5.04538067777228));
#57140=CARTESIAN_POINT('Ctrl Pts',(16.6962612737695,-17.4001712070013,-5.04952119977381));
#57141=CARTESIAN_POINT('Ctrl Pts',(16.7489086678727,-17.3355185113609,-5.05366172177533));
#57142=CARTESIAN_POINT('Ctrl Pts',(16.8015842228024,-17.2708312333184,-5.05780445852127));
#57143=CARTESIAN_POINT('Ctrl Pts',(16.8573774008556,-17.2087799314012,-5.06194719526721));
#57144=CARTESIAN_POINT('Ctrl Pts',(16.9159800655235,-17.1496672011401,-5.06608993201314));
#57145=CARTESIAN_POINT('Ctrl Pts',(16.9746826938398,-17.0904536371675,-5.07023973538449));
#57146=CARTESIAN_POINT('Ctrl Pts',(17.0362040315237,-17.0341889688223,-5.07438953875584));
#57147=CARTESIAN_POINT('Ctrl Pts',(17.1002018437186,-16.9811363353769,-5.07853934212719));
#57148=CARTESIAN_POINT('Ctrl Pts',(17.1438608301676,-16.9449440949669,-5.08137031717058));
#57149=CARTESIAN_POINT('Ctrl Pts',(17.1886716656529,-16.910245843732,-5.08420129221397));
#57150=CARTESIAN_POINT('Ctrl Pts',(17.2345184376715,-16.8771132454428,-5.08703226725736));
#57151=CARTESIAN_POINT('Ctrl Pts',(17.302287307428,-16.8281379601765,-5.09121690165041));
#57152=CARTESIAN_POINT('Ctrl Pts',(17.3725842232475,-16.78239517261,-5.09540153604346));
#57153=CARTESIAN_POINT('Ctrl Pts',(17.4450678487465,-16.7401559934152,-5.09958617043651));
#57154=CARTESIAN_POINT('Ctrl Pts',(17.5174483027761,-16.697976936464,-5.10376484852044));
#57155=CARTESIAN_POINT('Ctrl Pts',(17.5920088899902,-16.6592918118672,-5.10794352660438));
#57156=CARTESIAN_POINT('Ctrl Pts',(17.668377621725,-16.6243297168801,-5.11212220468831));
#57157=CARTESIAN_POINT('Ctrl Pts',(17.7461152080911,-16.5887409514671,-5.11637578257375));
#57158=CARTESIAN_POINT('Ctrl Pts',(17.8257260077699,-16.5570102814917,-5.12062936045919));
#57159=CARTESIAN_POINT('Ctrl Pts',(17.9067894477686,-16.5293314914588,-5.12488293834462));
#57160=CARTESIAN_POINT('Ctrl Pts',(17.9862813148006,-16.5021893087815,-5.12905405232258));
#57161=CARTESIAN_POINT('Ctrl Pts',(18.0671695448446,-16.4789434563412,-5.13322516630053));
#57162=CARTESIAN_POINT('Ctrl Pts',(18.1490371223199,-16.4597282588497,-5.13739628027848));
#57163=CARTESIAN_POINT('Ctrl Pts',(18.230877228339,-16.4405195092033,-5.14156599459885));
#57164=CARTESIAN_POINT('Ctrl Pts',(18.3136955816367,-16.4253388333998,-5.14573570891923));
#57165=CARTESIAN_POINT('Ctrl Pts',(18.3970618790067,-16.4142701675274,-5.1499054232396));
#57166=CARTESIAN_POINT('Ctrl Pts',(18.4804252098461,-16.4032018955256,-5.15407498918365));
#57167=CARTESIAN_POINT('Ctrl Pts',(18.5643359898473,-16.3962454022305,-5.1582445551277));
#57168=CARTESIAN_POINT('Ctrl Pts',(18.6483570024151,-16.3934329641448,-5.16241412107174));
#57169=CARTESIAN_POINT('Ctrl Pts',(18.7353320901336,-16.3905216442056,-5.16673028381067));
#57170=CARTESIAN_POINT('Ctrl Pts',(18.822424779069,-16.3920512290412,-5.17104644654959));
#57171=CARTESIAN_POINT('Ctrl Pts',(18.909150084646,-16.3979987376964,-5.17536260928851));
#57172=CARTESIAN_POINT('Ctrl Pts',(18.9930503225157,-16.4037525068826,-5.17953817348019));
#57173=CARTESIAN_POINT('Ctrl Pts',(19.0766062822588,-16.4136406900189,-5.18371373767187));
#57174=CARTESIAN_POINT('Ctrl Pts',(19.1593859487959,-16.427589812537,-5.18788930186354));
#57175=CARTESIAN_POINT('Ctrl Pts',(19.2463466194998,-16.4422434720726,-5.19227576387609));
#57176=CARTESIAN_POINT('Ctrl Pts',(19.3324499449361,-16.4613789616179,-5.19666222588863));
#57177=CARTESIAN_POINT('Ctrl Pts',(19.4172115835232,-16.4848514572204,-5.20104868790118));
#57178=CARTESIAN_POINT('Ctrl Pts',(19.5019732221104,-16.5083239528229,-5.20543514991372));
#57179=CARTESIAN_POINT('Ctrl Pts',(19.5853926474676,-16.5361331988246,-5.20982161192626));
#57180=CARTESIAN_POINT('Ctrl Pts',(19.6670104728637,-16.5680764572817,-5.21420807393881));
#57181=CARTESIAN_POINT('Ctrl Pts',(19.7448664736167,-16.5985474278376,-5.21839236074251));
#57182=CARTESIAN_POINT('Ctrl Pts',(19.821373063144,-16.6328931302869,-5.22257664754621));
#57183=CARTESIAN_POINT('Ctrl Pts',(19.8961176236036,-16.6709733388428,-5.22676093434992));
#57184=CARTESIAN_POINT('Ctrl Pts',(19.9707478771494,-16.7089953113065,-5.2309388221206));
#57185=CARTESIAN_POINT('Ctrl Pts',(20.0436210503407,-16.7507402336343,-5.23511670989127));
#57186=CARTESIAN_POINT('Ctrl Pts',(20.1143433780762,-16.7960194438258,-5.23929459766195));
#57187=CARTESIAN_POINT('Ctrl Pts',(20.1757784666028,-16.8353525989353,-5.24292384620713));
#57188=CARTESIAN_POINT('Ctrl Pts',(20.2355906143445,-16.877351908466,-5.24655309475231));
#57189=CARTESIAN_POINT('Ctrl Pts',(20.293535888361,-16.9218650751948,-5.25018234329749));
#57190=CARTESIAN_POINT('Ctrl Pts',(20.2961058236222,-16.9185141606307,-4.45010593324722));
#57191=CARTESIAN_POINT('Ctrl Pts',(20.3016500329822,-16.9227661777456,-4.45045503344821));
#57192=CARTESIAN_POINT('Ctrl Pts',(20.9781025678406,-17.4463824914852,-4.49319606920968));
#57193=CARTESIAN_POINT('Ctrl Pts',(21.7484972529808,-19.2278589375158,-4.57832904053163));
#57194=CARTESIAN_POINT('Ctrl Pts',(20.1337364777487,-21.6360323460232,-4.70550484721307));
#57195=CARTESIAN_POINT('Ctrl Pts',(17.2348043616254,-21.581772666889,-4.8326806538945));
#57196=CARTESIAN_POINT('Ctrl Pts',(16.1917618388527,-19.8928505847622,-4.91974900156632));
#57197=CARTESIAN_POINT('Ctrl Pts',(16.1699049957539,-18.998574246681,-4.96442541367765));
#57198=CARTESIAN_POINT('Ctrl Pts',(16.1700997034774,-18.952836752384,-4.96670989022851));
#57199=CARTESIAN_POINT('Origin',(18.734,-18.952,1.76670989022851));
#57200=CARTESIAN_POINT('',(20.293535888361,-16.9218650751948,-3.65004596076623));
#57201=CARTESIAN_POINT('',(20.293535888361,-16.9218650751948,-3.71676815356108));
#57202=CARTESIAN_POINT('',(20.293535888361,-16.9218650751948,1.76670989022851));
#57203=CARTESIAN_POINT('',(16.1740009581142,-18.9542148462772,-4.23329008724971));
#57204=CARTESIAN_POINT('Ctrl Pts',(20.293535888361,-16.9218650751948,-3.71676815356108));
#57205=CARTESIAN_POINT('Ctrl Pts',(20.360101304459,-16.9730001766405,-3.72094076536866));
#57206=CARTESIAN_POINT('Ctrl Pts',(20.4242136557516,-17.0274621982811,-3.72511337717624));
#57207=CARTESIAN_POINT('Ctrl Pts',(20.4855270207266,-17.0849828346625,-3.72928598898382));
#57208=CARTESIAN_POINT('Ctrl Pts',(20.5468084015455,-17.1424734653673,-3.73345642414578));
#57209=CARTESIAN_POINT('Ctrl Pts',(20.6052933602042,-17.203019228744,-3.73762685930775));
#57210=CARTESIAN_POINT('Ctrl Pts',(20.6606699271548,-17.2663123089381,-3.74179729446971));
#57211=CARTESIAN_POINT('Ctrl Pts',(20.716034218668,-17.3295913588252,-3.74596680516274));
#57212=CARTESIAN_POINT('Ctrl Pts',(20.7682911845239,-17.3956161695929,-3.75013631585578));
#57213=CARTESIAN_POINT('Ctrl Pts',(20.8171674786023,-17.4640439334128,-3.75430582654881));
#57214=CARTESIAN_POINT('Ctrl Pts',(20.8660475997594,-17.5324770552174,-3.75847566372006));
#57215=CARTESIAN_POINT('Ctrl Pts',(20.9115462572013,-17.6033131285658,-3.76264550089132));
#57216=CARTESIAN_POINT('Ctrl Pts',(20.9534327836276,-17.6761794330866,-3.76681533806257));
#57217=CARTESIAN_POINT('Ctrl Pts',(20.9953632082252,-17.7491221033938,-3.77098954533186));
#57218=CARTESIAN_POINT('Ctrl Pts',(21.0336737129171,-17.8240988539095,-3.77516375260116));
#57219=CARTESIAN_POINT('Ctrl Pts',(21.0681793259974,-17.9007118025554,-3.77933795987045));
#57220=CARTESIAN_POINT('Ctrl Pts',(21.1027036747927,-17.977366350183,-3.78351443363353));
#57221=CARTESIAN_POINT('Ctrl Pts',(21.133418850014,-18.0556584365516,-3.78769090739661));
#57222=CARTESIAN_POINT('Ctrl Pts',(21.1601887465462,-18.1351718870334,-3.79186738115969));
#57223=CARTESIAN_POINT('Ctrl Pts',(21.1870051419978,-18.214823451218,-3.79605110939672));
#57224=CARTESIAN_POINT('Ctrl Pts',(21.2098624458985,-18.2957001737844,-3.80023483763376));
#57225=CARTESIAN_POINT('Ctrl Pts',(21.2286750199151,-18.3773726903361,-3.80441856587079));
#57226=CARTESIAN_POINT('Ctrl Pts',(21.2428259543193,-18.4388072618799,-3.80756559209883));
#57227=CARTESIAN_POINT('Ctrl Pts',(21.2546893789919,-18.5006918342718,-3.81071261832686));
#57228=CARTESIAN_POINT('Ctrl Pts',(21.2642482087236,-18.5628419315355,-3.8138596445549));
#57229=CARTESIAN_POINT('Ctrl Pts',(21.2769586867287,-18.645483579777,-3.818044278948));
#57230=CARTESIAN_POINT('Ctrl Pts',(21.285639763102,-18.7289023900137,-3.82222891334111));
#57231=CARTESIAN_POINT('Ctrl Pts',(21.2902056694013,-18.8126709803349,-3.82641354773422));
#57232=CARTESIAN_POINT('Ctrl Pts',(21.2947650766981,-18.8963203364363,-3.83059222581822));
#57233=CARTESIAN_POINT('Ctrl Pts',(21.2952209238071,-18.9803180282763,-3.83477090390223));
#57234=CARTESIAN_POINT('Ctrl Pts',(21.2915388082527,-19.0642285359494,-3.83894958198624));
#57235=CARTESIAN_POINT('Ctrl Pts',(21.2877906934233,-19.1496430791655,-3.84320315987166));
#57236=CARTESIAN_POINT('Ctrl Pts',(21.2797547375529,-19.2349668053837,-3.84745673775708));
#57237=CARTESIAN_POINT('Ctrl Pts',(21.2674501116906,-19.3197370413421,-3.8517103156425));
#57238=CARTESIAN_POINT('Ctrl Pts',(21.2553840350109,-19.4028638408624,-3.85588142962051));
#57239=CARTESIAN_POINT('Ctrl Pts',(21.2392133934507,-19.485457943358,-3.86005254359853));
#57240=CARTESIAN_POINT('Ctrl Pts',(21.2190086634415,-19.567086939075,-3.86422365757654));
#57241=CARTESIAN_POINT('Ctrl Pts',(21.1988107133246,-19.6486885433942,-3.86839337189698));
#57242=CARTESIAN_POINT('Ctrl Pts',(21.1745814736227,-19.7293252379224,-3.87256308621741));
#57243=CARTESIAN_POINT('Ctrl Pts',(21.1464423282955,-19.8085757483423,-3.87673280053785));
#57244=CARTESIAN_POINT('Ctrl Pts',(21.1183041842798,-19.8878234386891,-3.88090236648196));
#57245=CARTESIAN_POINT('Ctrl Pts',(21.0862565659974,-19.9656846097694,-3.88507193242607));
#57246=CARTESIAN_POINT('Ctrl Pts',(21.0504699913871,-20.0417553757623,-3.88924149837017));
#57247=CARTESIAN_POINT('Ctrl Pts',(21.0134252049623,-20.1205006960415,-3.89355766110902));
#57248=CARTESIAN_POINT('Ctrl Pts',(20.9723738713786,-20.1973268901843,-3.89787382384787));
#57249=CARTESIAN_POINT('Ctrl Pts',(20.9275574633283,-20.2718127348517,-3.90218998658671));
#57250=CARTESIAN_POINT('Ctrl Pts',(20.884200945055,-20.3438722109659,-3.90636555077845));
#57251=CARTESIAN_POINT('Ctrl Pts',(20.8373211816341,-20.4137411050184,-3.9105411149702));
#57252=CARTESIAN_POINT('Ctrl Pts',(20.7871804520946,-20.4810683539778,-3.91471667916194));
#57253=CARTESIAN_POINT('Ctrl Pts',(20.7345072335068,-20.5517961422236,-3.91910314117434));
#57254=CARTESIAN_POINT('Ctrl Pts',(20.6782353411156,-20.6197183310686,-3.92348960318673));
#57255=CARTESIAN_POINT('Ctrl Pts',(20.6187144099125,-20.684469795716,-3.92787606519913));
#57256=CARTESIAN_POINT('Ctrl Pts',(20.5591934787094,-20.7492212603633,-3.93226252721153));
#57257=CARTESIAN_POINT('Ctrl Pts',(20.4964239761435,-20.8108016487773,-3.93664898922393));
#57258=CARTESIAN_POINT('Ctrl Pts',(20.4307957154099,-20.8688944415817,-3.94103545123633));
#57259=CARTESIAN_POINT('Ctrl Pts',(20.3681871082353,-20.9243142988764,-3.94522008562936));
#57260=CARTESIAN_POINT('Ctrl Pts',(20.3027439921319,-20.9767667301135,-3.94940472002239));
#57261=CARTESIAN_POINT('Ctrl Pts',(20.2347793028206,-21.025948283884,-3.95358935441541));
#57262=CARTESIAN_POINT('Ctrl Pts',(20.1669113528321,-21.0750598338002,-3.95776803249935));
#57263=CARTESIAN_POINT('Ctrl Pts',(20.0965293283134,-21.1209094865297,-3.96194671058328));
#57264=CARTESIAN_POINT('Ctrl Pts',(20.0239808111748,-21.1632325763702,-3.96612538866721));
#57265=CARTESIAN_POINT('Ctrl Pts',(19.9501319140058,-21.2063142771792,-3.97037896655265));
#57266=CARTESIAN_POINT('Ctrl Pts',(19.8740384525298,-21.2457414247198,-3.97463254443809));
#57267=CARTESIAN_POINT('Ctrl Pts',(19.7960998386656,-21.2812797025489,-3.97888612232353));
#57268=CARTESIAN_POINT('Ctrl Pts',(19.7196722169164,-21.3161290015149,-3.98305723630146));
#57269=CARTESIAN_POINT('Ctrl Pts',(19.6414707859433,-21.3472386721819,-3.98722835027939));
#57270=CARTESIAN_POINT('Ctrl Pts',(19.5618972814746,-21.3744339188772,-3.99139946425732));
#57271=CARTESIAN_POINT('Ctrl Pts',(19.4823504786638,-21.4016200399449,-3.99556917857768));
#57272=CARTESIAN_POINT('Ctrl Pts',(19.4014329516939,-21.4248941970684,-3.99973889289803));
#57273=CARTESIAN_POINT('Ctrl Pts',(19.319564628433,-21.4441304271503,-4.00390860721839));
#57274=CARTESIAN_POINT('Ctrl Pts',(19.2376992183983,-21.4633659727245,-4.00807817316242));
#57275=CARTESIAN_POINT('Ctrl Pts',(19.1548835273736,-21.4785637725469,-4.01224773910645));
#57276=CARTESIAN_POINT('Ctrl Pts',(19.0715494575443,-21.4896485894843,-4.01641730505048));
#57277=CARTESIAN_POINT('Ctrl Pts',(18.9852854646228,-21.5011231349107,-4.02073346778942));
#57278=CARTESIAN_POINT('Ctrl Pts',(18.8984664850867,-21.5081900216474,-4.02504963052836));
#57279=CARTESIAN_POINT('Ctrl Pts',(18.8115774056926,-21.5108242898109,-4.0293657932673));
#57280=CARTESIAN_POINT('Ctrl Pts',(18.7275187289215,-21.5133727469659,-4.03354135745896));
#57281=CARTESIAN_POINT('Ctrl Pts',(18.6433949192222,-21.5117729919952,-4.03771692165062));
#57282=CARTESIAN_POINT('Ctrl Pts',(18.5596431317113,-21.5060555362953,-4.04189248584229));
#57283=CARTESIAN_POINT('Ctrl Pts',(18.471661240513,-21.5000493054998,-4.04627894785487));
#57284=CARTESIAN_POINT('Ctrl Pts',(18.3840905205394,-21.4894985417946,-4.05066540986745));
#57285=CARTESIAN_POINT('Ctrl Pts',(18.2974272347522,-21.474499597749,-4.05505187188003));
#57286=CARTESIAN_POINT('Ctrl Pts',(18.210763948965,-21.4595006537034,-4.05943833389261));
#57287=CARTESIAN_POINT('Ctrl Pts',(18.1250086463917,-21.440053731818,-4.06382479590519));
#57288=CARTESIAN_POINT('Ctrl Pts',(18.0406384682269,-21.4163152773655,-4.06821125791777));
#57289=CARTESIAN_POINT('Ctrl Pts',(17.9601502870268,-21.3936690643915,-4.07239589231081));
#57290=CARTESIAN_POINT('Ctrl Pts',(17.8806229756134,-21.3670332665356,-4.07658052670385));
#57291=CARTESIAN_POINT('Ctrl Pts',(17.8024810747699,-21.3365067607239,-4.08076516109689));
#57292=CARTESIAN_POINT('Ctrl Pts',(17.7244503992504,-21.306023705615,-4.08494383918082));
#57293=CARTESIAN_POINT('Ctrl Pts',(17.6478016421986,-21.2716611086066,-4.08912251726475));
#57294=CARTESIAN_POINT('Ctrl Pts',(17.5729454850813,-21.2335679725546,-4.09330119534867));
#57295=CARTESIAN_POINT('Ctrl Pts',(17.4967475851455,-21.1947920444157,-4.09755477323411));
#57296=CARTESIAN_POINT('Ctrl Pts',(17.422407646075,-21.1521506525344,-4.10180835111955));
#57297=CARTESIAN_POINT('Ctrl Pts',(17.3503388850133,-21.1058528080799,-4.10606192900499));
#57298=CARTESIAN_POINT('Ctrl Pts',(17.2796673175155,-21.0604525376831,-4.11023304298293));
#57299=CARTESIAN_POINT('Ctrl Pts',(17.2111800563182,-21.0115365845697,-4.11440415696087));
#57300=CARTESIAN_POINT('Ctrl Pts',(17.1452415288503,-20.959348131329,-4.11857527093882));
#57301=CARTESIAN_POINT('Ctrl Pts',(17.0793251276922,-20.9071771904278,-4.12274498525918));
#57302=CARTESIAN_POINT('Ctrl Pts',(17.01595612214,-20.8517362155439,-4.12691469957954));
#57303=CARTESIAN_POINT('Ctrl Pts',(16.9554677262149,-20.7933101181237,-4.1310844138999));
#57304=CARTESIAN_POINT('Ctrl Pts',(16.8949814827263,-20.7348860997546,-4.13525397984395));
#57305=CARTESIAN_POINT('Ctrl Pts',(16.8373759753517,-20.6734774902646,-4.139423545788));
#57306=CARTESIAN_POINT('Ctrl Pts',(16.7829482470746,-20.6094067266084,-4.14359311173204));
#57307=CARTESIAN_POINT('Ctrl Pts',(16.7266069070151,-20.5430833139417,-4.14790927447097));
#57308=CARTESIAN_POINT('Ctrl Pts',(16.6736713066581,-20.47390746331,-4.1522254372099));
#57309=CARTESIAN_POINT('Ctrl Pts',(16.6244248933205,-20.4022733774286,-4.15654159994883));
#57310=CARTESIAN_POINT('Ctrl Pts',(16.5767826767178,-20.3329727643605,-4.1607171641405));
#57311=CARTESIAN_POINT('Ctrl Pts',(16.5325931948253,-20.2613720362608,-4.16489272833218));
#57312=CARTESIAN_POINT('Ctrl Pts',(16.4920674161606,-20.1878552866412,-4.16906829252386));
#57313=CARTESIAN_POINT('Ctrl Pts',(16.4494947767562,-20.1106253807675,-4.17345475453641));
#57314=CARTESIAN_POINT('Ctrl Pts',(16.4109659295264,-20.0312813353545,-4.17784121654897));
#57315=CARTESIAN_POINT('Ctrl Pts',(16.3766684749372,-19.9502925828358,-4.18222767856152));
#57316=CARTESIAN_POINT('Ctrl Pts',(16.342371020348,-19.8693038303171,-4.18661414057408));
#57317=CARTESIAN_POINT('Ctrl Pts',(16.3123050853067,-19.7866709419478,-4.19100060258663));
#57318=CARTESIAN_POINT('Ctrl Pts',(16.2865973915759,-19.702879798822,-4.19538706459919));
#57319=CARTESIAN_POINT('Ctrl Pts',(16.2566341527394,-19.6052182170345,-4.2004996433589));
#57320=CARTESIAN_POINT('Ctrl Pts',(16.2324986213406,-19.5056900725379,-4.20561222211862));
#57321=CARTESIAN_POINT('Ctrl Pts',(16.2143850329185,-19.404924295726,-4.21072480087833));
#57322=CARTESIAN_POINT('Ctrl Pts',(16.1965183144937,-19.3055318551339,-4.21576770033015));
#57323=CARTESIAN_POINT('Ctrl Pts',(16.1845105456257,-19.2049352741343,-4.22081059978196));
#57324=CARTESIAN_POINT('Ctrl Pts',(16.1785021632643,-19.1037590407164,-4.22585349923378));
#57325=CARTESIAN_POINT('Ctrl Pts',(16.1755487125963,-19.0540253526453,-4.22833236190576));
#57326=CARTESIAN_POINT('Ctrl Pts',(16.174044162412,-19.0041519285503,-4.23081122457773));
#57327=CARTESIAN_POINT('Ctrl Pts',(16.1740009581142,-18.9542148462772,-4.23329008724971));
#57328=CARTESIAN_POINT('Ctrl Pts',(16.1756127776244,-18.9542129983521,-4.2332901097715));
#57329=CARTESIAN_POINT('Ctrl Pts',(16.1805387770827,-18.3551144017957,-4.26304769694121));
#57330=CARTESIAN_POINT('Ctrl Pts',(16.6895187238437,-16.8950156783259,-4.3351972196714));
#57331=CARTESIAN_POINT('Ctrl Pts',(18.6971963271545,-16.1157768135428,-4.42965875093214));
#57332=CARTESIAN_POINT('Ctrl Pts',(19.9334915941914,-16.6513471023293,-4.49436269502317));
#57333=CARTESIAN_POINT('Ctrl Pts',(20.2910030755688,-16.9251725897442,-4.51667470355372));
#57334=CARTESIAN_POINT('',(16.1740010840393,-18.9496440968074,-4.16670989022851));
#57335=CARTESIAN_POINT('Ctrl Pts',(16.174088184599,-18.9496434116999,-4.16670992829755));
#57336=CARTESIAN_POINT('Ctrl Pts',(16.1722334877636,-18.748007243103,-4.17674049236081));
#57337=CARTESIAN_POINT('Ctrl Pts',(16.2862273000593,-17.6962739531831,-4.22916299198455));
#57338=CARTESIAN_POINT('Ctrl Pts',(17.7316712464,-16.0996999541064,-4.32362832696778));
#57339=CARTESIAN_POINT('Ctrl Pts',(19.6284056027312,-16.406435236022,-4.40806309788774));
#57340=CARTESIAN_POINT('Ctrl Pts',(20.2961058236222,-16.9185141606307,-4.45010593324722));
#57341=CARTESIAN_POINT('Ctrl Pts',(20.293535888361,-16.9218650751948,-3.65004596076623));
#57342=CARTESIAN_POINT('Ctrl Pts',(20.3602232257825,-16.9730938357748,-3.65422168175373));
#57343=CARTESIAN_POINT('Ctrl Pts',(20.4243341343203,-17.02757381297,-3.65839740274122));
#57344=CARTESIAN_POINT('Ctrl Pts',(20.485549918636,-17.0850043164147,-3.66257312372872));
#57345=CARTESIAN_POINT('Ctrl Pts',(20.5479163710248,-17.1435143363186,-3.66682733540086));
#57346=CARTESIAN_POINT('Ctrl Pts',(20.6072773997898,-17.2050865762893,-3.67108154707301));
#57347=CARTESIAN_POINT('Ctrl Pts',(20.6633380137791,-17.2693666981226,-3.67533575874516));
#57348=CARTESIAN_POINT('Ctrl Pts',(20.7193986277684,-17.3336468199559,-3.67958997041731));
#57349=CARTESIAN_POINT('Ctrl Pts',(20.7721585715388,-17.4006343914317,-3.68384418208945));
#57350=CARTESIAN_POINT('Ctrl Pts',(20.8213695361432,-17.4699445288447,-3.6880983937616));
#57351=CARTESIAN_POINT('Ctrl Pts',(20.8697756595073,-17.5381211047148,-3.69228302815506));
#57352=CARTESIAN_POINT('Ctrl Pts',(20.914928230553,-17.6087985715452,-3.69646766254852));
#57353=CARTESIAN_POINT('Ctrl Pts',(20.956559006204,-17.6816333348432,-3.70065229694198));
#57354=CARTESIAN_POINT('Ctrl Pts',(20.9981305255987,-17.7543644268708,-3.70483097502633));
#57355=CARTESIAN_POINT('Ctrl Pts',(21.0361899803433,-17.8292463201213,-3.70900965311069));
#57356=CARTESIAN_POINT('Ctrl Pts',(21.0705113959643,-17.905905120685,-3.71318833119505));
#57357=CARTESIAN_POINT('Ctrl Pts',(21.1054479982896,-17.9839379751455,-3.71744190908038));
#57358=CARTESIAN_POINT('Ctrl Pts',(21.1365109555626,-18.0638116724909,-3.72169548696571));
#57359=CARTESIAN_POINT('Ctrl Pts',(21.1635100116305,-18.1451040318682,-3.72594906485105));
#57360=CARTESIAN_POINT('Ctrl Pts',(21.1899856383155,-18.22482038024,-3.73012017882942));
#57361=CARTESIAN_POINT('Ctrl Pts',(21.2125533792703,-18.3059004177639,-3.7342912928078));
#57362=CARTESIAN_POINT('Ctrl Pts',(21.2310824062636,-18.3879260187451,-3.73846240678618));
#57363=CARTESIAN_POINT('Ctrl Pts',(21.249605215663,-18.4699240952438,-3.74263212110699));
#57364=CARTESIAN_POINT('Ctrl Pts',(21.2640919013283,-18.5528666566977,-3.74680183542779));
#57365=CARTESIAN_POINT('Ctrl Pts',(21.2744621331457,-18.6363227121685,-3.75097154974859));
#57366=CARTESIAN_POINT('Ctrl Pts',(21.2848319959458,-18.7197757979147,-3.75514111569307));
#57367=CARTESIAN_POINT('Ctrl Pts',(21.2910856402585,-18.8037418847205,-3.75931068163754));
#57368=CARTESIAN_POINT('Ctrl Pts',(21.293194451632,-18.887783501059,-3.76348024758202));
#57369=CARTESIAN_POINT('Ctrl Pts',(21.2953774062114,-18.9747799169322,-3.76779641032044));
#57370=CARTESIAN_POINT('Ctrl Pts',(21.293118626995,-19.0618567451373,-3.77211257305885));
#57371=CARTESIAN_POINT('Ctrl Pts',(21.2864451550249,-19.148529210526,-3.77642873579727));
#57372=CARTESIAN_POINT('Ctrl Pts',(21.2799890707009,-19.2323783294897,-3.78060429998939));
#57373=CARTESIAN_POINT('Ctrl Pts',(21.2694016000863,-19.3158485639548,-3.78477986418151));
#57374=CARTESIAN_POINT('Ctrl Pts',(21.2547598325397,-19.3985085292069,-3.78895542837363));
#57375=CARTESIAN_POINT('Ctrl Pts',(21.2393785441268,-19.48534345277,-3.7933418903852));
#57376=CARTESIAN_POINT('Ctrl Pts',(21.2195227615801,-19.571283533682,-3.79772835239677));
#57377=CARTESIAN_POINT('Ctrl Pts',(21.1953413592831,-19.6558456599868,-3.80211481440833));
#57378=CARTESIAN_POINT('Ctrl Pts',(21.1711599569862,-19.7404077862916,-3.8065012764199));
#57379=CARTESIAN_POINT('Ctrl Pts',(21.1426531949957,-19.8235914337675,-3.81088773843147));
#57380=CARTESIAN_POINT('Ctrl Pts',(21.1100276507034,-19.9049389293616,-3.81527420044303));
#57381=CARTESIAN_POINT('Ctrl Pts',(21.0789032560606,-19.9825435061126,-3.81945883483597));
#57382=CARTESIAN_POINT('Ctrl Pts',(21.0439149217344,-20.058766045094,-3.8236434692289));
#57383=CARTESIAN_POINT('Ctrl Pts',(21.0052063614282,-20.1331950151471,-3.82782810362184));
#57384=CARTESIAN_POINT('Ctrl Pts',(20.9665528979664,-20.2075180447737,-3.83200678170567));
#57385=CARTESIAN_POINT('Ctrl Pts',(20.9241899370651,-20.2800521717354,-3.8361854597895));
#57386=CARTESIAN_POINT('Ctrl Pts',(20.8783095486357,-20.3504050055795,-3.84036413787333));
#57387=CARTESIAN_POINT('Ctrl Pts',(20.8316067872157,-20.422018863411,-3.84461771575879));
#57388=CARTESIAN_POINT('Ctrl Pts',(20.7812594376514,-20.4913720121106,-3.84887129364426));
#57389=CARTESIAN_POINT('Ctrl Pts',(20.7275195051817,-20.5580759578738,-3.85312487152972));
#57390=CARTESIAN_POINT('Ctrl Pts',(20.6748214261695,-20.6234867174841,-3.85729598550756));
#57391=CARTESIAN_POINT('Ctrl Pts',(20.6188614359627,-20.6863497027061,-3.86146709948541));
#57392=CARTESIAN_POINT('Ctrl Pts',(20.5599202972603,-20.7463285841932,-3.86563821346325));
#57393=CARTESIAN_POINT('Ctrl Pts',(20.5009989368264,-20.8062873391872,-3.8698079277835));
#57394=CARTESIAN_POINT('Ctrl Pts',(20.4390987367875,-20.8633635846449,-3.87397764210375));
#57395=CARTESIAN_POINT('Ctrl Pts',(20.3745386111499,-20.9172564884326,-3.87814735642401));
#57396=CARTESIAN_POINT('Ctrl Pts',(20.3099807828387,-20.9711474744794,-3.88231692236793));
#57397=CARTESIAN_POINT('Ctrl Pts',(20.2427635708238,-21.0218550499287,-3.88648648831186));
#57398=CARTESIAN_POINT('Ctrl Pts',(20.1732393309683,-21.0691183595147,-3.89065605425578));
#57399=CARTESIAN_POINT('Ctrl Pts',(20.1012707046024,-21.118043388763,-3.89497221699484));
#57400=CARTESIAN_POINT('Ctrl Pts',(20.0268302379305,-21.1632771484777,-3.89928837973389));
#57401=CARTESIAN_POINT('Ctrl Pts',(19.9503401869381,-21.2045799763026,-3.90360454247295));
#57402=CARTESIAN_POINT('Ctrl Pts',(19.876341791316,-21.2445373688529,-3.90778010666452));
#57403=CARTESIAN_POINT('Ctrl Pts',(19.8004257365565,-21.280815836347,-3.91195567085608));
#57404=CARTESIAN_POINT('Ctrl Pts',(19.7229964759441,-21.3132466983715,-3.91613123504764));
#57405=CARTESIAN_POINT('Ctrl Pts',(19.6416564474416,-21.3473155661428,-3.92051769706045));
#57406=CARTESIAN_POINT('Ctrl Pts',(19.5586468811864,-21.3771377310941,-3.92490415907325));
#57407=CARTESIAN_POINT('Ctrl Pts',(19.4744545807604,-21.4025768736832,-3.92929062108606));
#57408=CARTESIAN_POINT('Ctrl Pts',(19.3902622803343,-21.4280160162723,-3.93367708309886));
#57409=CARTESIAN_POINT('Ctrl Pts',(19.3048878272885,-21.4490720714144,-3.93806354511167));
#57410=CARTESIAN_POINT('Ctrl Pts',(19.2188278686569,-21.4656710082613,-3.94245000712447));
#57411=CARTESIAN_POINT('Ctrl Pts',(19.1367276562992,-21.4815062034173,-3.94663464151748));
#57412=CARTESIAN_POINT('Ctrl Pts',(19.0536980417282,-21.4933443659488,-3.95081927591048));
#57413=CARTESIAN_POINT('Ctrl Pts',(18.9701628470242,-21.5010835823263,-3.95500391030349));
#57414=CARTESIAN_POINT('Ctrl Pts',(18.8867465543302,-21.5088117828872,-3.9591825883874));
#57415=CARTESIAN_POINT('Ctrl Pts',(18.8028265650696,-21.5124525840588,-3.96336126647131));
#57416=CARTESIAN_POINT('Ctrl Pts',(18.7188367813161,-21.511955092731,-3.96753994455521));
#57417=CARTESIAN_POINT('Ctrl Pts',(18.6333415410503,-21.5114486842286,-3.97179352244066));
#57418=CARTESIAN_POINT('Ctrl Pts',(18.5477744529621,-21.5066540748901,-3.9760471003261));
#57419=CARTESIAN_POINT('Ctrl Pts',(18.4625985845166,-21.4975728769127,-3.98030067821155));
#57420=CARTESIAN_POINT('Ctrl Pts',(18.3790740164893,-21.4886677356787,-3.98447179218945));
#57421=CARTESIAN_POINT('Ctrl Pts',(18.2959261128658,-21.4756407813846,-3.98864290616735));
#57422=CARTESIAN_POINT('Ctrl Pts',(18.2135896449255,-21.4585460423322,-3.99281402014525));
#57423=CARTESIAN_POINT('Ctrl Pts',(18.1312808057821,-21.4414570395846,-3.99698373446557));
#57424=CARTESIAN_POINT('Ctrl Pts',(18.0497833116117,-21.4203030563997,-4.00115344878589));
#57425=CARTESIAN_POINT('Ctrl Pts',(17.9695227367341,-21.3951894142595,-4.00532316310622));
#57426=CARTESIAN_POINT('Ctrl Pts',(17.8892650178723,-21.3700766657704,-4.00949272905021));
#57427=CARTESIAN_POINT('Ctrl Pts',(17.8102445695778,-21.3410046766648,-4.0136622949942));
#57428=CARTESIAN_POINT('Ctrl Pts',(17.7328714533936,-21.3081285264539,-4.0178318609382));
#57429=CARTESIAN_POINT('Ctrl Pts',(17.6527779938924,-21.2740964913578,-4.02214802367717));
#57430=CARTESIAN_POINT('Ctrl Pts',(17.5744503476374,-21.2359880155536,-4.02646418641615));
#57431=CARTESIAN_POINT('Ctrl Pts',(17.498318591899,-21.1940284248139,-4.03078034915512));
#57432=CARTESIAN_POINT('Ctrl Pts',(17.424666820098,-21.1534356633302,-4.03495591334675));
#57433=CARTESIAN_POINT('Ctrl Pts',(17.3530704495471,-21.1092391216314,-4.03913147753838));
#57434=CARTESIAN_POINT('Ctrl Pts',(17.2838902366715,-21.0616875774151,-4.04330704173));
#57435=CARTESIAN_POINT('Ctrl Pts',(17.2112158957012,-21.0117343177416,-4.04769350374265));
#57436=CARTESIAN_POINT('Ctrl Pts',(17.1412086706267,-20.9580785813371,-4.0520799657553));
#57437=CARTESIAN_POINT('Ctrl Pts',(17.074246682156,-20.9010559057928,-4.05646642776795));
#57438=CARTESIAN_POINT('Ctrl Pts',(17.0072846936853,-20.8440332302485,-4.0608528897806));
#57439=CARTESIAN_POINT('Ctrl Pts',(16.9433683113268,-20.7836440693276,-4.06523935179325));
#57440=CARTESIAN_POINT('Ctrl Pts',(16.8828286089282,-20.7202659530956,-4.0696258138059));
#57441=CARTESIAN_POINT('Ctrl Pts',(16.8258191500137,-20.66058359639,-4.07375648865202));
#57442=CARTESIAN_POINT('Ctrl Pts',(16.7715797255597,-20.5980163329693,-4.07788716349815));
#57443=CARTESIAN_POINT('Ctrl Pts',(16.720421868205,-20.5328551822216,-4.08201783834428));
#57444=CARTESIAN_POINT('Ctrl Pts',(16.6693300782615,-20.467778183328,-4.08614317866297));
#57445=CARTESIAN_POINT('Ctrl Pts',(16.6213122506322,-20.4001143092104,-4.09026851898165));
#57446=CARTESIAN_POINT('Ctrl Pts',(16.5766430483355,-20.3301911997632,-4.09439385930034));
#57447=CARTESIAN_POINT('Ctrl Pts',(16.5320173182039,-20.2603361396388,-4.09851518482882));
#57448=CARTESIAN_POINT('Ctrl Pts',(16.4907340001793,-20.1882266026471,-4.1026365103573));
#57449=CARTESIAN_POINT('Ctrl Pts',(16.4530264539488,-20.1142218730582,-4.10675783588578));
#57450=CARTESIAN_POINT('Ctrl Pts',(16.4153436115611,-20.0402656271648,-4.11087646135585));
#57451=CARTESIAN_POINT('Ctrl Pts',(16.3812321043791,-19.9644170734852,-4.11499508682592));
#57452=CARTESIAN_POINT('Ctrl Pts',(16.3508802454214,-19.8870616211443,-4.11911371229599));
#57453=CARTESIAN_POINT('Ctrl Pts',(16.3205285952527,-19.8097067009281,-4.12323230943423));
#57454=CARTESIAN_POINT('Ctrl Pts',(16.2939367323083,-19.7308453355426,-4.12735090657246));
#57455=CARTESIAN_POINT('Ctrl Pts',(16.2712450678812,-19.6508834983921,-4.13146950371069));
#57456=CARTESIAN_POINT('Ctrl Pts',(16.2485547151173,-19.570926283335,-4.1355878627786));
#57457=CARTESIAN_POINT('Ctrl Pts',(16.2297642345971,-19.4898691801182,-4.1397062218465));
#57458=CARTESIAN_POINT('Ctrl Pts',(16.2149637529308,-19.4081319830394,-4.14382458091441));
#57459=CARTESIAN_POINT('Ctrl Pts',(16.2001500672816,-19.3263218655941,-4.14794661410208));
#57460=CARTESIAN_POINT('Ctrl Pts',(16.1893335672674,-19.2438309098088,-4.15206864728976));
#57461=CARTESIAN_POINT('Ctrl Pts',(16.1825528364004,-19.1610869947166,-4.15619068047744));
#57462=CARTESIAN_POINT('Ctrl Pts',(16.1767848147302,-19.0907009692733,-4.1596970837278));
#57463=CARTESIAN_POINT('Ctrl Pts',(16.1739362156169,-19.020132176051,-4.16320348697815));
#57464=CARTESIAN_POINT('Ctrl Pts',(16.1740010840393,-18.9496440968074,-4.16670989022851));
#57465=CARTESIAN_POINT('Origin',(18.734,-18.952,1.76670989022851));
#57466=CARTESIAN_POINT('',(20.2912842963712,-16.9247659399654,-2.85017128767263));
#57467=CARTESIAN_POINT('',(20.293535888361,-16.9218650751948,-2.91665631152786));
#57468=CARTESIAN_POINT('',(20.293535888361,-16.9218650751948,1.76670989022851));
#57469=CARTESIAN_POINT('',(16.1740000028035,-18.9521198080497,-3.43329010980363));
#57470=CARTESIAN_POINT('Ctrl Pts',(20.293535888361,-16.9218650751948,-2.91665631152786));
#57471=CARTESIAN_POINT('Ctrl Pts',(20.3304359427923,-16.950211446889,-2.91898054028019));
#57472=CARTESIAN_POINT('Ctrl Pts',(20.3665290689409,-16.9795381976313,-2.92130476903252));
#57473=CARTESIAN_POINT('Ctrl Pts',(20.401762322946,-17.0097927931959,-2.92362899778485));
#57474=CARTESIAN_POINT('Ctrl Pts',(20.4651976823984,-17.0642643769006,-2.92781363217406));
#57475=CARTESIAN_POINT('Ctrl Pts',(20.5260796023552,-17.1219484370562,-2.93199826656327));
#57476=CARTESIAN_POINT('Ctrl Pts',(20.5840648143939,-17.1825763134451,-2.93618290095248));
#57477=CARTESIAN_POINT('Ctrl Pts',(20.6419674916593,-17.243117893555,-2.94036157903251));
#57478=CARTESIAN_POINT('Ctrl Pts',(20.6969813355446,-17.3065946373119,-2.94454025711253));
#57479=CARTESIAN_POINT('Ctrl Pts',(20.7487967797138,-17.3726982756753,-2.94871893519256));
#57480=CARTESIAN_POINT('Ctrl Pts',(20.8015409785421,-17.439986774327,-2.95297251307897));
#57481=CARTESIAN_POINT('Ctrl Pts',(20.8509706214137,-17.5099969539569,-2.95722609096537));
#57482=CARTESIAN_POINT('Ctrl Pts',(20.8967991444563,-17.5823650629678,-2.96147966885178));
#57483=CARTESIAN_POINT('Ctrl Pts',(20.9417391920986,-17.6533301748853,-2.96565078282566));
#57484=CARTESIAN_POINT('Ctrl Pts',(20.9832162459024,-17.7265621993701,-2.96982189679953));
#57485=CARTESIAN_POINT('Ctrl Pts',(21.0210023907229,-17.801686970939,-2.97399301077341));
#57486=CARTESIAN_POINT('Ctrl Pts',(21.0587758560372,-17.8767865336643,-2.97816272508966));
#57487=CARTESIAN_POINT('Ctrl Pts',(21.0928606655495,-17.953777171463,-2.9823324394059));
#57488=CARTESIAN_POINT('Ctrl Pts',(21.1230748017627,-18.0322600413256,-2.98650215372215));
#57489=CARTESIAN_POINT('Ctrl Pts',(21.153287862827,-18.11074011843,-2.99067171966202));
#57490=CARTESIAN_POINT('Ctrl Pts',(21.1796303599629,-18.190711892398,-2.99484128560189));
#57491=CARTESIAN_POINT('Ctrl Pts',(21.2019688964371,-18.2717577444622,-2.99901085154177));
#57492=CARTESIAN_POINT('Ctrl Pts',(21.2250928283449,-18.3556530688812,-3.00332701428548));
#57493=CARTESIAN_POINT('Ctrl Pts',(21.2439258622492,-18.4406988974017,-3.00764317702919));
#57494=CARTESIAN_POINT('Ctrl Pts',(21.2583771885884,-18.5264182690313,-3.0119593397729));
#57495=CARTESIAN_POINT('Ctrl Pts',(21.2723577644625,-18.6093453409698,-3.01613490396034));
#57496=CARTESIAN_POINT('Ctrl Pts',(21.2822377087348,-18.6929022752308,-3.02031046814777));
#57497=CARTESIAN_POINT('Ctrl Pts',(21.2879876706469,-18.7766518372396,-3.02448603233521));
#57498=CARTESIAN_POINT('Ctrl Pts',(21.2940280494849,-18.8646313908058,-3.02887249435706));
#57499=CARTESIAN_POINT('Ctrl Pts',(21.295510260803,-18.9528229589747,-3.0332589563789));
#57500=CARTESIAN_POINT('Ctrl Pts',(21.2924621252161,-19.0407217776803,-3.03764541840075));
#57501=CARTESIAN_POINT('Ctrl Pts',(21.2894139896292,-19.128620596386,-3.0420318804226));
#57502=CARTESIAN_POINT('Ctrl Pts',(21.2818356329246,-19.2162260941259,-3.04641834244444));
#57503=CARTESIAN_POINT('Ctrl Pts',(21.2698170137414,-19.303044260485,-3.05080480446629));
#57504=CARTESIAN_POINT('Ctrl Pts',(21.2583513890591,-19.3858677941968,-3.05498943886226));
#57505=CARTESIAN_POINT('Ctrl Pts',(21.2428024516836,-19.4682831419495,-3.05917407325824));
#57506=CARTESIAN_POINT('Ctrl Pts',(21.2232102976567,-19.5498562486417,-3.06335870765421));
#57507=CARTESIAN_POINT('Ctrl Pts',(21.2036460306358,-19.6313132461141,-3.06753738574112));
#57508=CARTESIAN_POINT('Ctrl Pts',(21.1800500847572,-19.7119299402854,-3.07171606382802));
#57509=CARTESIAN_POINT('Ctrl Pts',(21.1525141031144,-19.7912791746712,-3.07589474191493));
#57510=CARTESIAN_POINT('Ctrl Pts',(21.1244845588152,-19.8720506869848,-3.08014831979963));
#57511=CARTESIAN_POINT('Ctrl Pts',(21.0923724052599,-19.951508376567,-3.08440189768433));
#57512=CARTESIAN_POINT('Ctrl Pts',(21.0563283883887,-20.0292143967122,-3.08865547556903));
#57513=CARTESIAN_POINT('Ctrl Pts',(21.0209831550867,-20.1054139340948,-3.09282658955003));
#57514=CARTESIAN_POINT('Ctrl Pts',(20.981857354168,-20.1799286784576,-3.09699770353102));
#57515=CARTESIAN_POINT('Ctrl Pts',(20.9391422334474,-20.252364460552,-3.10116881751202));
#57516=CARTESIAN_POINT('Ctrl Pts',(20.8964414461978,-20.3247759361205,-3.10533853183546));
#57517=CARTESIAN_POINT('Ctrl Pts',(20.8501539646467,-20.3951094389618,-3.1095082461589));
#57518=CARTESIAN_POINT('Ctrl Pts',(20.8005166300294,-20.4629960350087,-3.11367796048233));
#57519=CARTESIAN_POINT('Ctrl Pts',(20.7508810617213,-20.5308802153594,-3.11784752642946));
#57520=CARTESIAN_POINT('Ctrl Pts',(20.6978961495658,-20.5963172911853,-3.12201709237659));
#57521=CARTESIAN_POINT('Ctrl Pts',(20.6418408397362,-20.6589690478256,-3.12618665832372));
#57522=CARTESIAN_POINT('Ctrl Pts',(20.5838146944558,-20.7238235628383,-3.13050282105905));
#57523=CARTESIAN_POINT('Ctrl Pts',(20.5224985756086,-20.7856928577379,-3.13481898379438));
#57524=CARTESIAN_POINT('Ctrl Pts',(20.4582443784124,-20.8442424061186,-3.13913514652972));
#57525=CARTESIAN_POINT('Ctrl Pts',(20.3960832548337,-20.9008847092082,-3.1433107107245));
#57526=CARTESIAN_POINT('Ctrl Pts',(20.3311729226015,-20.9544199625776,-3.14748627491928));
#57527=CARTESIAN_POINT('Ctrl Pts',(20.2638651397916,-21.0045868201006,-3.15166183911406));
#57528=CARTESIAN_POINT('Ctrl Pts',(20.1931578010452,-21.0572874862143,-3.15604830111967));
#57529=CARTESIAN_POINT('Ctrl Pts',(20.1198049419666,-21.1062702143003,-3.16043476312528));
#57530=CARTESIAN_POINT('Ctrl Pts',(20.0442460480198,-21.1512851778813,-3.16482122513089));
#57531=CARTESIAN_POINT('Ctrl Pts',(19.968687154073,-21.1963001414623,-3.1692076871365));
#57532=CARTESIAN_POINT('Ctrl Pts',(19.8909227738874,-21.2373471369618,-3.17359414914211));
#57533=CARTESIAN_POINT('Ctrl Pts',(19.8114169849418,-21.2742344068933,-3.17798061114772));
#57534=CARTESIAN_POINT('Ctrl Pts',(19.7355693750926,-21.3094244389056,-3.18216524554016));
#57535=CARTESIAN_POINT('Ctrl Pts',(19.6578547653244,-21.3409601078314,-3.1863498799326));
#57536=CARTESIAN_POINT('Ctrl Pts',(19.578659830513,-21.3686401823022,-3.19053451432504));
#57537=CARTESIAN_POINT('Ctrl Pts',(19.4995776198891,-21.3962808576131,-3.19471319240837));
#57538=CARTESIAN_POINT('Ctrl Pts',(19.4190197000618,-21.4200766888,-3.1988918704917));
#57539=CARTESIAN_POINT('Ctrl Pts',(19.3373948467031,-21.4398735214983,-3.20307054857503));
#57540=CARTESIAN_POINT('Ctrl Pts',(19.2543069264955,-21.4600251981986,-3.20732412646062));
#57541=CARTESIAN_POINT('Ctrl Pts',(19.1701138843276,-21.4760328992744,-3.21157770434621));
#57542=CARTESIAN_POINT('Ctrl Pts',(19.0852654759068,-21.4877863800873,-3.2158312822318));
#57543=CARTESIAN_POINT('Ctrl Pts',(19.0020620194665,-21.4993119967374,-3.22000239620914));
#57544=CARTESIAN_POINT('Ctrl Pts',(18.9182288577839,-21.5067468078097,-3.22417351018648));
#57545=CARTESIAN_POINT('Ctrl Pts',(18.8342009436325,-21.5100382661124,-3.22834462416381));
#57546=CARTESIAN_POINT('Ctrl Pts',(18.7502012258592,-21.5133286199344,-3.23251433848358));
#57547=CARTESIAN_POINT('Ctrl Pts',(18.6660073447033,-21.5124783642369,-3.23668405280334));
#57548=CARTESIAN_POINT('Ctrl Pts',(18.5820577129981,-21.5074869480044,-3.2408537671231));
#57549=CARTESIAN_POINT('Ctrl Pts',(18.4981110685809,-21.5024957093878,-3.24502333306653));
#57550=CARTESIAN_POINT('Ctrl Pts',(18.414409115505,-21.4933636313811,-3.24919289900997));
#57551=CARTESIAN_POINT('Ctrl Pts',(18.3313872270487,-21.4801421943903,-3.2533624649534));
#57552=CARTESIAN_POINT('Ctrl Pts',(18.2454463913858,-21.4664559079809,-3.25767862769305));
#57553=CARTESIAN_POINT('Ctrl Pts',(18.1602348531239,-21.4483874314135,-3.2619947904327));
#57554=CARTESIAN_POINT('Ctrl Pts',(18.0762243702397,-21.4260515800794,-3.26631095317234));
#57555=CARTESIAN_POINT('Ctrl Pts',(17.9949505200244,-21.4044433167599,-3.27048651736342));
#57556=CARTESIAN_POINT('Ctrl Pts',(17.9148011124187,-21.378841616957,-3.2746620815545));
#57557=CARTESIAN_POINT('Ctrl Pts',(17.8361862981299,-21.349400791844,-3.27883764574558));
#57558=CARTESIAN_POINT('Ctrl Pts',(17.7536008364223,-21.3184729806292,-3.28322410775951));
#57559=CARTESIAN_POINT('Ctrl Pts',(17.6727096022459,-21.2833082561226,-3.28761056977344));
#57560=CARTESIAN_POINT('Ctrl Pts',(17.5939605452813,-21.2441409297172,-3.29199703178737));
#57561=CARTESIAN_POINT('Ctrl Pts',(17.5152114883168,-21.2049736033118,-3.2963834938013));
#57562=CARTESIAN_POINT('Ctrl Pts',(17.4386050767024,-21.161804026126,-3.30076995581523));
#57563=CARTESIAN_POINT('Ctrl Pts',(17.364553744478,-21.1149186191895,-3.30515641782916));
#57564=CARTESIAN_POINT('Ctrl Pts',(17.2939096238495,-21.070190479346,-3.30934105222176));
#57565=CARTESIAN_POINT('Ctrl Pts',(17.2253276726157,-21.0219144506012,-3.31352568661436));
#57566=CARTESIAN_POINT('Ctrl Pts',(17.1591863942882,-20.97030674261,-3.31771032100696));
#57567=CARTESIAN_POINT('Ctrl Pts',(17.093139259884,-20.9187724918035,-3.32188899909045));
#57568=CARTESIAN_POINT('Ctrl Pts',(17.0295262575255,-20.8639162618917,-3.32606767717394));
#57569=CARTESIAN_POINT('Ctrl Pts',(16.9686982691563,-20.8059983276908,-3.33024635525743));
#57570=CARTESIAN_POINT('Ctrl Pts',(16.9067799828036,-20.7470422561362,-3.33449993314298));
#57571=CARTESIAN_POINT('Ctrl Pts',(16.8477479425957,-20.6849138964936,-3.33875351102853));
#57572=CARTESIAN_POINT('Ctrl Pts',(16.7919382910611,-20.6199317488055,-3.34300708891408));
#57573=CARTESIAN_POINT('Ctrl Pts',(16.7372106185328,-20.5562094068615,-3.34717820289155));
#57574=CARTESIAN_POINT('Ctrl Pts',(16.6855818186072,-20.4897433069906,-3.35134931686903));
#57575=CARTESIAN_POINT('Ctrl Pts',(16.6373315068437,-20.420870732844,-3.35552043084651));
#57576=CARTESIAN_POINT('Ctrl Pts',(16.5890973859384,-20.352021269555,-3.3596901451664));
#57577=CARTESIAN_POINT('Ctrl Pts',(16.544239765417,-20.2807673121879,-3.36385985948629));
#57578=CARTESIAN_POINT('Ctrl Pts',(16.5029964131481,-20.207477198301,-3.36802957380618));
#57579=CARTESIAN_POINT('Ctrl Pts',(16.4617545284946,-20.1341896923911,-3.37219913974973));
#57580=CARTESIAN_POINT('Ctrl Pts',(16.4241268812486,-20.0588665753509,-3.37636870569329));
#57581=CARTESIAN_POINT('Ctrl Pts',(16.3903058438335,-19.9819017925758,-3.38053827163684));
#57582=CARTESIAN_POINT('Ctrl Pts',(16.3552957004569,-19.9022310229649,-3.38485443437632));
#57583=CARTESIAN_POINT('Ctrl Pts',(16.3243650403573,-19.8208014806367,-3.3891705971158));
#57584=CARTESIAN_POINT('Ctrl Pts',(16.2976726756056,-19.7380719867858,-3.39348675985528));
#57585=CARTESIAN_POINT('Ctrl Pts',(16.2718498118347,-19.6580373975154,-3.39766232404646));
#57586=CARTESIAN_POINT('Ctrl Pts',(16.2499934356292,-19.5767867151056,-3.40183788823764));
#57587=CARTESIAN_POINT('Ctrl Pts',(16.2321958025117,-19.4947483371048,-3.40601345242882));
#57588=CARTESIAN_POINT('Ctrl Pts',(16.2134992532485,-19.4085663956273,-3.41039991444245));
#57589=CARTESIAN_POINT('Ctrl Pts',(16.1992823307861,-19.3215156705806,-3.41478637645608));
#57590=CARTESIAN_POINT('Ctrl Pts',(16.1895904829899,-19.2340996450696,-3.41917283846971));
#57591=CARTESIAN_POINT('Ctrl Pts',(16.1798986351937,-19.1466836195585,-3.42355930048334));
#57592=CARTESIAN_POINT('Ctrl Pts',(16.174731820223,-19.0589028772671,-3.42794576249697));
#57593=CARTESIAN_POINT('Ctrl Pts',(16.1740724460423,-18.9712592442245,-3.43233222451059));
#57594=CARTESIAN_POINT('Ctrl Pts',(16.1740244495167,-18.9648795739235,-3.43265151959756));
#57595=CARTESIAN_POINT('Ctrl Pts',(16.1740003013853,-18.958499723977,-3.43297081468453));
#57596=CARTESIAN_POINT('Ctrl Pts',(16.1740000028035,-18.9521198086917,-3.4332901097715));
#57597=CARTESIAN_POINT('Ctrl Pts',(16.1740000028035,-18.9521198080497,-3.43329010980363));
#57598=CARTESIAN_POINT('Ctrl Pts',(16.173996094898,-18.8686175883754,-3.43746913841141));
#57599=CARTESIAN_POINT('Ctrl Pts',(16.1780820066338,-18.7849577973269,-3.4416481670192));
#57600=CARTESIAN_POINT('Ctrl Pts',(16.1862780259001,-18.7015748760835,-3.44582719562698));
#57601=CARTESIAN_POINT('Ctrl Pts',(16.1944623792895,-18.6183106386623,-3.45000027597724));
#57602=CARTESIAN_POINT('Ctrl Pts',(16.2067451760218,-18.5353229435673,-3.45417335632751));
#57603=CARTESIAN_POINT('Ctrl Pts',(16.2230946976723,-18.4530465324877,-3.45834643667777));
#57604=CARTESIAN_POINT('Ctrl Pts',(16.2396087147061,-18.369942324114,-3.46256150311587));
#57605=CARTESIAN_POINT('Ctrl Pts',(16.2602717621694,-18.2875642714266,-3.46677656955396));
#57606=CARTESIAN_POINT('Ctrl Pts',(16.2849973159137,-18.2063554108437,-3.47099163599205));
#57607=CARTESIAN_POINT('Ctrl Pts',(16.3094325809408,-18.1260999774803,-3.47515721572334));
#57608=CARTESIAN_POINT('Ctrl Pts',(16.3378353258575,-18.0469868800097,-3.47932279545462));
#57609=CARTESIAN_POINT('Ctrl Pts',(16.3700710228284,-17.9694320426107,-3.4834883751859));
#57610=CARTESIAN_POINT('Ctrl Pts',(16.4022960455082,-17.8919028861488,-3.48765257555781));
#57611=CARTESIAN_POINT('Ctrl Pts',(16.4383513227395,-17.8159313907882,-3.49181677592972));
#57612=CARTESIAN_POINT('Ctrl Pts',(16.4780536821042,-17.7419147919373,-3.49598097630164));
#57613=CARTESIAN_POINT('Ctrl Pts',(16.5177548909312,-17.667900338019,-3.50014505599887));
#57614=CARTESIAN_POINT('Ctrl Pts',(16.561102752779,-17.5958410741347,-3.50430913569611));
#57615=CARTESIAN_POINT('Ctrl Pts',(16.6078681568274,-17.5261096166088,-3.50847321539335));
#57616=CARTESIAN_POINT('Ctrl Pts',(16.6556310871524,-17.4548907569615,-3.51272611670991));
#57617=CARTESIAN_POINT('Ctrl Pts',(16.7069587733462,-17.3861005826234,-3.51697901802647));
#57618=CARTESIAN_POINT('Ctrl Pts',(16.7615616490752,-17.320103265583,-3.52123191934302));
#57619=CARTESIAN_POINT('Ctrl Pts',(16.815101261178,-17.255391092332,-3.52540200532769));
#57620=CARTESIAN_POINT('Ctrl Pts',(16.8717892886061,-17.1933642853471,-3.52957209131236));
#57621=CARTESIAN_POINT('Ctrl Pts',(16.9313144499797,-17.134329840772,-3.53374217729703));
#57622=CARTESIAN_POINT('Ctrl Pts',(16.9926128107595,-17.0735368147895,-3.53803648627953));
#57623=CARTESIAN_POINT('Ctrl Pts',(17.0569196193486,-17.0159176096088,-3.54233079526203));
#57624=CARTESIAN_POINT('Ctrl Pts',(17.1238587796064,-16.9617625140729,-3.54662510424453));
#57625=CARTESIAN_POINT('Ctrl Pts',(17.1907979398642,-16.9076074185369,-3.55091941322703));
#57626=CARTESIAN_POINT('Ctrl Pts',(17.2603689845986,-16.8569166856669,-3.55521372220953));
#57627=CARTESIAN_POINT('Ctrl Pts',(17.3321657913458,-16.809930708066,-3.55950803119203));
#57628=CARTESIAN_POINT('Ctrl Pts',(17.4021289421208,-16.7641447297734,-3.56369266558497));
#57629=CARTESIAN_POINT('Ctrl Pts',(17.4744678068902,-16.7217048000894,-3.5678772999779));
#57630=CARTESIAN_POINT('Ctrl Pts',(17.5488288662328,-16.6828659396842,-3.57206193437084));
#57631=CARTESIAN_POINT('Ctrl Pts',(17.6230840818116,-16.6440823615896,-3.57624061245467));
#57632=CARTESIAN_POINT('Ctrl Pts',(17.6993553703909,-16.6088898827214,-3.5804192905385));
#57633=CARTESIAN_POINT('Ctrl Pts',(17.7772605377961,-16.5775001365631,-3.58459796862233));
#57634=CARTESIAN_POINT('Ctrl Pts',(17.8565620993404,-16.5455477517632,-3.58885154650779));
#57635=CARTESIAN_POINT('Ctrl Pts',(17.9375562869753,-16.5175360325719,-3.59310512439325));
#57636=CARTESIAN_POINT('Ctrl Pts',(18.0198140087904,-16.4936390887504,-3.59735870227872));
#57637=CARTESIAN_POINT('Ctrl Pts',(18.1004770041527,-16.4702054338167,-3.60152981625656));
#57638=CARTESIAN_POINT('Ctrl Pts',(18.1823545166279,-16.4507285663625,-3.60570093023439));
#57639=CARTESIAN_POINT('Ctrl Pts',(18.2650237601176,-16.4353233647475,-3.60987204421223));
#57640=CARTESIAN_POINT('Ctrl Pts',(18.3476652631443,-16.4199233324967,-3.61404175853249));
#57641=CARTESIAN_POINT('Ctrl Pts',(18.4310975176832,-16.408592336823,-3.61821147285275));
#57642=CARTESIAN_POINT('Ctrl Pts',(18.5148867965882,-16.4013943064263,-3.622381187173));
#57643=CARTESIAN_POINT('Ctrl Pts',(18.5986730939111,-16.3941965321664,-3.62655075311693));
#57644=CARTESIAN_POINT('Ctrl Pts',(18.6828159319225,-16.3911314692988,-3.63072031906085));
#57645=CARTESIAN_POINT('Ctrl Pts',(18.7668770686618,-16.3922111223079,-3.63488988500478));
#57646=CARTESIAN_POINT('Ctrl Pts',(18.8538936912734,-16.3933287345849,-3.63920604774383));
#57647=CARTESIAN_POINT('Ctrl Pts',(18.9408222331034,-16.398887935209,-3.64352221048289));
#57648=CARTESIAN_POINT('Ctrl Pts',(19.0271792931089,-16.4088433193977,-3.64783837322195));
#57649=CARTESIAN_POINT('Ctrl Pts',(19.110723280963,-16.418474407993,-3.65201393741352));
#57650=CARTESIAN_POINT('Ctrl Pts',(19.1937319902678,-16.4322195436239,-3.65618950160508));
#57651=CARTESIAN_POINT('Ctrl Pts',(19.2757772698984,-16.4499853338117,-3.66036506579665));
#57652=CARTESIAN_POINT('Ctrl Pts',(19.3619664615664,-16.4686484318293,-3.66475152780945));
#57653=CARTESIAN_POINT('Ctrl Pts',(19.4470917766263,-16.4917488722623,-3.66913798982225));
#57654=CARTESIAN_POINT('Ctrl Pts',(19.5306760960808,-16.5191195676866,-3.67352445183505));
#57655=CARTESIAN_POINT('Ctrl Pts',(19.6142604155353,-16.5464902631109,-3.67791091384785));
#57656=CARTESIAN_POINT('Ctrl Pts',(19.6963032254016,-16.578130933778,-3.68229737586066));
#57657=CARTESIAN_POINT('Ctrl Pts',(19.7763550154477,-16.6138177954293,-3.68668383787346));
#57658=CARTESIAN_POINT('Ctrl Pts',(19.8527263004242,-16.6478638983275,-3.69086862549939));
#57659=CARTESIAN_POINT('Ctrl Pts',(19.9275699049938,-16.6857190326234,-3.69505341312532));
#57660=CARTESIAN_POINT('Ctrl Pts',(20.0004799995,-16.7272239638861,-3.69923820075125));
#57661=CARTESIAN_POINT('Ctrl Pts',(20.0732773467746,-16.7686647124574,-3.70341651707547));
#57662=CARTESIAN_POINT('Ctrl Pts',(20.1441467296561,-16.8137438158313,-3.70759483339969));
#57663=CARTESIAN_POINT('Ctrl Pts',(20.2127034231806,-16.8622545163887,-3.71177314972391));
#57664=CARTESIAN_POINT('Ctrl Pts',(20.2400223175747,-16.8815853597736,-3.71343815100296));
#57665=CARTESIAN_POINT('Ctrl Pts',(20.2669742267315,-16.901460586774,-3.71510315228202));
#57666=CARTESIAN_POINT('Ctrl Pts',(20.293535888361,-16.9218650751948,-3.71676815356108));
#57667=CARTESIAN_POINT('',(16.1743944592445,-18.9523823947444,-3.36670986511428));
#57668=CARTESIAN_POINT('Ctrl Pts',(16.1740000284928,-18.9523819467095,-3.3667098902285));
#57669=CARTESIAN_POINT('Ctrl Pts',(16.1739869935966,-18.8650154810558,-3.37103154303558));
#57670=CARTESIAN_POINT('Ctrl Pts',(16.1784506871914,-18.7777135371325,-3.37535319584266));
#57671=CARTESIAN_POINT('Ctrl Pts',(16.1873453738309,-18.6909440385447,-3.37967484864975));
#57672=CARTESIAN_POINT('Ctrl Pts',(16.1966194662204,-18.6004733587883,-3.38418084296216));
#57673=CARTESIAN_POINT('Ctrl Pts',(16.2107109130556,-18.5105820575904,-3.38868683727458));
#57674=CARTESIAN_POINT('Ctrl Pts',(16.2295088315793,-18.4217887333309,-3.39319283158699));
#57675=CARTESIAN_POINT('Ctrl Pts',(16.2475982064586,-18.3363422660913,-3.39752898296558));
#57676=CARTESIAN_POINT('Ctrl Pts',(16.2700454505065,-18.2519128648082,-3.40186513434417));
#57677=CARTESIAN_POINT('Ctrl Pts',(16.296700996459,-18.1689459997304,-3.40620128572276));
#57678=CARTESIAN_POINT('Ctrl Pts',(16.3233900671469,-18.0858747870546,-3.41054289068792));
#57679=CARTESIAN_POINT('Ctrl Pts',(16.3542978445813,-18.0042701592832,-3.41488449565309));
#57680=CARTESIAN_POINT('Ctrl Pts',(16.3892268388776,-17.9245571437398,-3.41922610061825));
#57681=CARTESIAN_POINT('Ctrl Pts',(16.4242296046626,-17.8446757709924,-3.42357687523365));
#57682=CARTESIAN_POINT('Ctrl Pts',(16.4632703651625,-17.7666943545301,-3.42792764984905));
#57683=CARTESIAN_POINT('Ctrl Pts',(16.5061059491331,-17.6910130460184,-3.43227842446446));
#57684=CARTESIAN_POINT('Ctrl Pts',(16.5109248522389,-17.6824990756499,-3.43276787644255));
#57685=CARTESIAN_POINT('Ctrl Pts',(16.515791737601,-17.6740141830169,-3.43325732842064));
#57686=CARTESIAN_POINT('Ctrl Pts',(16.5207062260025,-17.6655589131312,-3.43374678039873));
#57687=CARTESIAN_POINT('Ctrl Pts',(16.5627232942887,-17.5932694654538,-3.43793141479117));
#57688=CARTESIAN_POINT('Ctrl Pts',(16.608363899273,-17.5229061642045,-3.44211604918361));
#57689=CARTESIAN_POINT('Ctrl Pts',(16.6574263400684,-17.4548554395523,-3.44630068357605));
#57690=CARTESIAN_POINT('Ctrl Pts',(16.7064189465521,-17.3869015766835,-3.4504793616594));
#57691=CARTESIAN_POINT('Ctrl Pts',(16.7588234476463,-17.3212541220954,-3.45465803974274));
#57692=CARTESIAN_POINT('Ctrl Pts',(16.8143930615577,-17.2582735752536,-3.45883671782609));
#57693=CARTESIAN_POINT('Ctrl Pts',(16.8709587208714,-17.1941641473616,-3.46309029571167));
#57694=CARTESIAN_POINT('Ctrl Pts',(16.930803836094,-17.1328185931037,-3.46734387359726));
#57695=CARTESIAN_POINT('Ctrl Pts',(16.9936228831504,-17.0745848910946,-3.47159745148285));
#57696=CARTESIAN_POINT('Ctrl Pts',(17.0552240603871,-17.0174801630431,-3.47576856546019));
#57697=CARTESIAN_POINT('Ctrl Pts',(17.1196845346186,-16.9633680324693,-3.47993967943753));
#57698=CARTESIAN_POINT('Ctrl Pts',(17.1866778681087,-16.9125407039709,-3.48411079341487));
#57699=CARTESIAN_POINT('Ctrl Pts',(17.2536487213389,-16.8617304310734,-3.48828050773464));
#57700=CARTESIAN_POINT('Ctrl Pts',(17.3231503796757,-16.8142030489941,-3.49245022205441));
#57701=CARTESIAN_POINT('Ctrl Pts',(17.394823786903,-16.7702101223364,-3.49661993637418));
#57702=CARTESIAN_POINT('Ctrl Pts',(17.4664946436829,-16.726218761136,-3.50078950231762));
#57703=CARTESIAN_POINT('Ctrl Pts',(17.5403367031862,-16.685761845216,-3.50495906826106));
#57704=CARTESIAN_POINT('Ctrl Pts',(17.6159635983351,-16.649046547463,-3.50912863420449));
#57705=CARTESIAN_POINT('Ctrl Pts',(17.694249441846,-16.6110403851223,-3.51344479694413));
#57706=CARTESIAN_POINT('Ctrl Pts',(17.7744474914061,-16.5770440773058,-3.51776095968377));
#57707=CARTESIAN_POINT('Ctrl Pts',(17.8561052781563,-16.5472337208454,-3.52207712242341));
#57708=CARTESIAN_POINT('Ctrl Pts',(17.9351030710676,-16.5183944336202,-3.52625268661449));
#57709=CARTESIAN_POINT('Ctrl Pts',(18.0154664958611,-16.4934726654684,-3.53042825080558));
#57710=CARTESIAN_POINT('Ctrl Pts',(18.0967709615464,-16.4725768508479,-3.53460381499666));
#57711=CARTESIAN_POINT('Ctrl Pts',(18.1821819225493,-16.4506256382959,-3.53899027701058));
#57712=CARTESIAN_POINT('Ctrl Pts',(18.2686309144574,-16.4331178853206,-3.54337673902449));
#57713=CARTESIAN_POINT('Ctrl Pts',(18.3556165397335,-16.4201180997138,-3.54776320103841));
#57714=CARTESIAN_POINT('Ctrl Pts',(18.4426021650097,-16.407118314107,-3.55214966305233));
#57715=CARTESIAN_POINT('Ctrl Pts',(18.5301238388031,-16.3986264761921,-3.55653612506624));
#57716=CARTESIAN_POINT('Ctrl Pts',(18.6176794289204,-16.3946440363642,-3.56092258708016));
#57717=CARTESIAN_POINT('Ctrl Pts',(18.7011876748678,-16.3908456887753,-3.56510628052802));
#57718=CARTESIAN_POINT('Ctrl Pts',(18.7850375342268,-16.3911349078501,-3.56928997397587));
#57719=CARTESIAN_POINT('Ctrl Pts',(18.868795197093,-16.3955512414991,-3.57347366742373));
#57720=CARTESIAN_POINT('Ctrl Pts',(18.9524422754803,-16.3999617443031,-3.57765183717926));
#57721=CARTESIAN_POINT('Ctrl Pts',(19.0359969440168,-16.4084885197953,-3.58183000693479));
#57722=CARTESIAN_POINT('Ctrl Pts',(19.1190226609994,-16.4211192144795,-3.58600817669031));
#57723=CARTESIAN_POINT('Ctrl Pts',(19.2019636761046,-16.4337370234749,-3.59018208392532));
#57724=CARTESIAN_POINT('Ctrl Pts',(19.2843763591288,-16.4504503679969,-3.59435599116033));
#57725=CARTESIAN_POINT('Ctrl Pts',(19.3658279303816,-16.4711949962986,-3.59852989839534));
#57726=CARTESIAN_POINT('Ctrl Pts',(19.4496036347878,-16.4925315503012,-3.60282290359291));
#57727=CARTESIAN_POINT('Ctrl Pts',(19.5323620461702,-16.5181329092784,-3.60711590879049));
#57728=CARTESIAN_POINT('Ctrl Pts',(19.613642592643,-16.5478725264229,-3.61140891398806));
#57729=CARTESIAN_POINT('Ctrl Pts',(19.6925889893505,-16.5767581050134,-3.6155786360938));
#57730=CARTESIAN_POINT('Ctrl Pts',(19.7701408045475,-16.6095472854996,-3.61974835819955));
#57731=CARTESIAN_POINT('Ctrl Pts',(19.8458923492031,-16.6460738511861,-3.62391808030529));
#57732=CARTESIAN_POINT('Ctrl Pts',(19.9250034287628,-16.6842203478312,-3.62827272704878));
#57733=CARTESIAN_POINT('Ctrl Pts',(20.002150345742,-16.7264432362292,-3.63262737379227));
#57734=CARTESIAN_POINT('Ctrl Pts',(20.0768973717721,-16.7724985320291,-3.63698202053576));
#57735=CARTESIAN_POINT('Ctrl Pts',(20.1516443978023,-16.8185538278289,-3.64133666727925));
#57736=CARTESIAN_POINT('Ctrl Pts',(20.2239910606285,-16.8684412099267,-3.64569131402274));
#57737=CARTESIAN_POINT('Ctrl Pts',(20.293535888361,-16.9218650751948,-3.65004596076623));
#57738=CARTESIAN_POINT('Ctrl Pts',(20.2912842963712,-16.9247659399654,-2.85017128767263));
#57739=CARTESIAN_POINT('Ctrl Pts',(20.689119003359,-17.2333456259195,-2.87512870967275));
#57740=CARTESIAN_POINT('Ctrl Pts',(21.5323502495748,-18.3705873153274,-2.94247806723335));
#57741=CARTESIAN_POINT('Ctrl Pts',(21.1037095629711,-20.8355520758667,-3.05221936035442));
#57742=CARTESIAN_POINT('Ctrl Pts',(18.4329096239604,-21.9640817435474,-3.17939516703586));
#57743=CARTESIAN_POINT('Ctrl Pts',(16.4590845454477,-20.6164716802603,-3.28422525531007));
#57744=CARTESIAN_POINT('Ctrl Pts',(16.1776267599649,-19.3569817996596,-3.34666340802382));
#57745=CARTESIAN_POINT('Ctrl Pts',(16.1781627867106,-18.9523866751972,-3.36670962517707));
#57746=CARTESIAN_POINT('Origin',(18.734,-18.952,1.76670989022851));
#57747=CARTESIAN_POINT('',(20.293535888361,-16.9218650751948,-2.05017637630343));
#57748=CARTESIAN_POINT('',(20.293535888361,-16.9218650751948,-2.11663751779963));
#57749=CARTESIAN_POINT('',(20.293535888361,-16.9218650751948,1.76670989022851));
#57750=CARTESIAN_POINT('',(16.1740010149448,-18.9497204131756,-2.63329010980609));
#57751=CARTESIAN_POINT('Ctrl Pts',(20.293535888361,-16.9218650751948,-2.11663751779963));
#57752=CARTESIAN_POINT('Ctrl Pts',(20.3602472256299,-16.9731122722949,-2.12081218273854));
#57753=CARTESIAN_POINT('Ctrl Pts',(20.4243917162535,-17.0276218213591,-2.12498684767744));
#57754=CARTESIAN_POINT('Ctrl Pts',(20.4856474637794,-17.0850958346409,-2.12916151261635));
#57755=CARTESIAN_POINT('Ctrl Pts',(20.5469405643417,-17.1426048949019,-2.13333872321698));
#57756=CARTESIAN_POINT('Ctrl Pts',(20.6053410960536,-17.2030816868678,-2.1375159338176));
#57757=CARTESIAN_POINT('Ctrl Pts',(20.6605654848026,-17.2661929431968,-2.14169314441823));
#57758=CARTESIAN_POINT('Ctrl Pts',(20.7158816143227,-17.3294090422494,-2.14587729435364));
#57759=CARTESIAN_POINT('Ctrl Pts',(20.768010782938,-17.3952679817225,-2.15006144428905));
#57760=CARTESIAN_POINT('Ctrl Pts',(20.8167112396531,-17.4634053969523,-2.15424559422446));
#57761=CARTESIAN_POINT('Ctrl Pts',(20.8412645289459,-17.4977582096496,-2.15635511538172));
#57762=CARTESIAN_POINT('Ctrl Pts',(20.8649469915942,-17.5326897523485,-2.15846463653898));
#57763=CARTESIAN_POINT('Ctrl Pts',(20.8877320902557,-17.5681509896658,-2.16057415769624));
#57764=CARTESIAN_POINT('Ctrl Pts',(20.9329306422981,-17.638495059893,-2.16475879183927));
#57765=CARTESIAN_POINT('Ctrl Pts',(20.9747633711847,-17.7111867434279,-2.16894342598229));
#57766=CARTESIAN_POINT('Ctrl Pts',(21.0129782252709,-17.7858703979656,-2.17312806012532));
#57767=CARTESIAN_POINT('Ctrl Pts',(21.0511386851992,-17.8604477494804,-2.17730673795485));
#57768=CARTESIAN_POINT('Ctrl Pts',(21.0856912912936,-17.9370110341171,-2.18148541578439));
#57769=CARTESIAN_POINT('Ctrl Pts',(21.116427617672,-18.0151762991077,-2.18566409361392));
#57770=CARTESIAN_POINT('Ctrl Pts',(21.1477148729796,-18.0947426263206,-2.18991767156241));
#57771=CARTESIAN_POINT('Ctrl Pts',(21.1750474280233,-18.1759685243987,-2.1941712495109));
#57772=CARTESIAN_POINT('Ctrl Pts',(21.1982547719715,-18.2584234585746,-2.19842482745939));
#57773=CARTESIAN_POINT('Ctrl Pts',(21.2210121944976,-18.33927983665,-2.20259594117397));
#57774=CARTESIAN_POINT('Ctrl Pts',(21.2398027993344,-18.421317558152,-2.20676705488855));
#57775=CARTESIAN_POINT('Ctrl Pts',(21.2545152522161,-18.504112889953,-2.21093816860314));
#57776=CARTESIAN_POINT('Ctrl Pts',(21.2692227681819,-18.5868804389239,-2.21510788265736));
#57777=CARTESIAN_POINT('Ctrl Pts',(21.2798547695695,-18.6704046407403,-2.21927759671159));
#57778=CARTESIAN_POINT('Ctrl Pts',(21.2863509615978,-18.7542512482192,-2.22344731076582));
#57779=CARTESIAN_POINT('Ctrl Pts',(21.2928469224598,-18.838094872027,-2.22761687644128));
#57780=CARTESIAN_POINT('Ctrl Pts',(21.2952073318929,-18.9222604199623,-2.23178644211675));
#57781=CARTESIAN_POINT('Ctrl Pts',(21.2934238553148,-19.0063095649563,-2.23595600779222));
#57782=CARTESIAN_POINT('Ctrl Pts',(21.2915776736488,-19.0933137860529,-2.24027217084101));
#57783=CARTESIAN_POINT('Ctrl Pts',(21.2852907961481,-19.1801927391156,-2.24458833388979));
#57784=CARTESIAN_POINT('Ctrl Pts',(21.2746126736341,-19.2664634200821,-2.24890449693858));
#57785=CARTESIAN_POINT('Ctrl Pts',(21.2642823912523,-19.3499238312634,-2.25308006085834));
#57786=CARTESIAN_POINT('Ctrl Pts',(21.2498426885289,-19.4328145349077,-2.25725562477811));
#57787=CARTESIAN_POINT('Ctrl Pts',(21.2313905396645,-19.514708176939,-2.26143118869787));
#57788=CARTESIAN_POINT('Ctrl Pts',(21.2120064127097,-19.6007380895305,-2.26581765131117));
#57789=CARTESIAN_POINT('Ctrl Pts',(21.1881940056838,-19.6856670076433,-2.27020411392447));
#57790=CARTESIAN_POINT('Ctrl Pts',(21.1601243952761,-19.7690192278313,-2.27459057653778));
#57791=CARTESIAN_POINT('Ctrl Pts',(21.1320547848685,-19.8523714480192,-2.27897703915108));
#57792=CARTESIAN_POINT('Ctrl Pts',(21.0997282551218,-19.9341464586593,-2.28336350176438));
#57793=CARTESIAN_POINT('Ctrl Pts',(21.0633723464422,-20.0138966388639,-2.28774996437768));
#57794=CARTESIAN_POINT('Ctrl Pts',(21.0286892306353,-20.089977387114,-2.29193459890685));
#57795=CARTESIAN_POINT('Ctrl Pts',(20.9902102866637,-20.1644987286812,-2.29611923343602));
#57796=CARTESIAN_POINT('Ctrl Pts',(20.948098122754,-20.2370562255471,-2.30030386796519));
#57797=CARTESIAN_POINT('Ctrl Pts',(20.906045900278,-20.30951044583,-2.30448254618695));
#57798=CARTESIAN_POINT('Ctrl Pts',(20.8603709589155,-20.380005979264,-2.30866122440872));
#57799=CARTESIAN_POINT('Ctrl Pts',(20.8112833253055,-20.4481597462864,-2.31283990263049));
#57800=CARTESIAN_POINT('Ctrl Pts',(20.761315833192,-20.5175351177548,-2.31709348048168));
#57801=CARTESIAN_POINT('Ctrl Pts',(20.7078123007176,-20.5844835062303,-2.32134705833287));
#57802=CARTESIAN_POINT('Ctrl Pts',(20.6510424452111,-20.6486284988939,-2.32560063618407));
#57803=CARTESIAN_POINT('Ctrl Pts',(20.5953731818007,-20.7115299183389,-2.32977175030303));
#57804=CARTESIAN_POINT('Ctrl Pts',(20.5365634319266,-20.7717353099771,-2.33394286442199));
#57805=CARTESIAN_POINT('Ctrl Pts',(20.4749092250507,-20.8289217005868,-2.33811397854095));
#57806=CARTESIAN_POINT('Ctrl Pts',(20.4132757068255,-20.8860889017635,-2.34228369300321));
#57807=CARTESIAN_POINT('Ctrl Pts',(20.3487999642225,-20.940238801272,-2.34645340746548));
#57808=CARTESIAN_POINT('Ctrl Pts',(20.2818144940605,-20.9910856509662,-2.35062312192774));
#57809=CARTESIAN_POINT('Ctrl Pts',(20.2148314075177,-21.0419306913198,-2.35479268801438));
#57810=CARTESIAN_POINT('Ctrl Pts',(20.1453391379196,-21.0894726380872,-2.35896225410102));
#57811=CARTESIAN_POINT('Ctrl Pts',(20.0737017376896,-21.1334672250647,-2.36313182018765));
#57812=CARTESIAN_POINT('Ctrl Pts',(19.999545660235,-21.179008604135,-2.36744798276027));
#57813=CARTESIAN_POINT('Ctrl Pts',(19.9230912497087,-21.2207482563567,-2.3717641453329));
#57814=CARTESIAN_POINT('Ctrl Pts',(19.8447714026877,-21.2584663212307,-2.37608030790552));
#57815=CARTESIAN_POINT('Ctrl Pts',(19.7690028109338,-21.294955726763,-2.38025587224007));
#57816=CARTESIAN_POINT('Ctrl Pts',(19.6914889015738,-21.3276813875219,-2.38443143657462));
#57817=CARTESIAN_POINT('Ctrl Pts',(19.6126415021176,-21.3564935247899,-2.38860700090917));
#57818=CARTESIAN_POINT('Ctrl Pts',(19.5298117168502,-21.3867608913672,-2.39299346260083));
#57819=CARTESIAN_POINT('Ctrl Pts',(19.4455107504569,-21.4127088296375,-2.39737992429249));
#57820=CARTESIAN_POINT('Ctrl Pts',(19.3602311944397,-21.4342236988456,-2.40176638598414));
#57821=CARTESIAN_POINT('Ctrl Pts',(19.2749516384225,-21.4557385680537,-2.4061528476758));
#57822=CARTESIAN_POINT('Ctrl Pts',(19.1886940767213,-21.4728203301028,-2.41053930936746));
#57823=CARTESIAN_POINT('Ctrl Pts',(19.1019580505853,-21.4854180217661,-2.41492577105912));
#57824=CARTESIAN_POINT('Ctrl Pts',(19.0192128717129,-21.4974360758147,-2.41911040544303));
#57825=CARTESIAN_POINT('Ctrl Pts',(18.9357242972402,-21.5054183621376,-2.42329503982695));
#57826=CARTESIAN_POINT('Ctrl Pts',(18.8519204122539,-21.5092826938713,-2.42747967421086));
#57827=CARTESIAN_POINT('Ctrl Pts',(18.7682358117207,-21.5131415252074,-2.4316583522859));
#57828=CARTESIAN_POINT('Ctrl Pts',(18.6842372477568,-21.5128940235269,-2.43583703036095));
#57829=CARTESIAN_POINT('Ctrl Pts',(18.6003605130588,-21.5085094342736,-2.44001570843599));
#57830=CARTESIAN_POINT('Ctrl Pts',(18.5149803479453,-21.5040462543973,-2.44426928632368));
#57831=CARTESIAN_POINT('Ctrl Pts',(18.4297268997696,-21.4952961442209,-2.44852286421137));
#57832=CARTESIAN_POINT('Ctrl Pts',(18.3450626650525,-21.4822821481969,-2.45277644209906));
#57833=CARTESIAN_POINT('Ctrl Pts',(18.2620398119429,-21.4695204539127,-2.45694755606873));
#57834=CARTESIAN_POINT('Ctrl Pts',(18.1795840056911,-21.4526587990536,-2.4611186700384));
#57835=CARTESIAN_POINT('Ctrl Pts',(18.0981270507746,-21.431771278252,-2.46528978400807));
#57836=CARTESIAN_POINT('Ctrl Pts',(18.0166974295212,-21.4108907664585,-2.46945949832042));
#57837=CARTESIAN_POINT('Ctrl Pts',(17.9362664391869,-21.3859871858385,-2.47362921263276));
#57838=CARTESIAN_POINT('Ctrl Pts',(17.857254322942,-21.3571854435283,-2.4777989269451));
#57839=CARTESIAN_POINT('Ctrl Pts',(17.7782450182823,-21.3283847261058,-2.48196849288138));
#57840=CARTESIAN_POINT('Ctrl Pts',(17.7006549192467,-21.2956862811424,-2.48613805881766));
#57841=CARTESIAN_POINT('Ctrl Pts',(17.6248864697078,-21.2592640024329,-2.49030762475394));
#57842=CARTESIAN_POINT('Ctrl Pts',(17.5464540946264,-21.2215611611785,-2.49462378750282));
#57843=CARTESIAN_POINT('Ctrl Pts',(17.4699743261967,-21.1798679825075,-2.49893995025171));
#57844=CARTESIAN_POINT('Ctrl Pts',(17.3958663510849,-21.1344294576552,-2.50325611300059));
#57845=CARTESIAN_POINT('Ctrl Pts',(17.3241724357536,-21.0904710881461,-2.50743167718525));
#57846=CARTESIAN_POINT('Ctrl Pts',(17.2546985266632,-21.0430079392874,-2.51160724136991));
#57847=CARTESIAN_POINT('Ctrl Pts',(17.1877934784102,-20.9923052204494,-2.51578280555457));
#57848=CARTESIAN_POINT('Ctrl Pts',(17.1175092148076,-20.9390416275035,-2.52016926758557));
#57849=CARTESIAN_POINT('Ctrl Pts',(17.0500605848374,-20.8822029788445,-2.52455572961657));
#57850=CARTESIAN_POINT('Ctrl Pts',(16.9858097729218,-20.8221419544912,-2.52894219164756));
#57851=CARTESIAN_POINT('Ctrl Pts',(16.9215589610062,-20.762080930138,-2.53332865367856));
#57852=CARTESIAN_POINT('Ctrl Pts',(16.8605063152545,-20.698798000471,-2.53771511570956));
#57853=CARTESIAN_POINT('Ctrl Pts',(16.802965079949,-20.6326856153201,-2.54210157774055));
#57854=CARTESIAN_POINT('Ctrl Pts',(16.7485317522925,-20.5701440813406,-2.54625111891253));
#57855=CARTESIAN_POINT('Ctrl Pts',(16.6970294692199,-20.5048282635504,-2.5504006600845));
#57856=CARTESIAN_POINT('Ctrl Pts',(16.6487573722081,-20.4370465256145,-2.55455020125647));
#57857=CARTESIAN_POINT('Ctrl Pts',(16.6005493742832,-20.3693547930394,-2.55869423237572));
#57858=CARTESIAN_POINT('Ctrl Pts',(16.5555633203296,-20.2992040148308,-2.56283826349496));
#57859=CARTESIAN_POINT('Ctrl Pts',(16.514059720175,-20.2269373137572,-2.5669822946142));
#57860=CARTESIAN_POINT('Ctrl Pts',(16.4725982721948,-20.154744008692,-2.5711221169438));
#57861=CARTESIAN_POINT('Ctrl Pts',(16.4346124893252,-20.0804394498693,-2.57526193927339));
#57862=CARTESIAN_POINT('Ctrl Pts',(16.4003201033268,-20.0043963796323,-2.57940176160299));
#57863=CARTESIAN_POINT('Ctrl Pts',(16.3660518421397,-19.9284068059566,-2.58353867155335));
#57864=CARTESIAN_POINT('Ctrl Pts',(16.3354720095443,-19.8506815753093,-2.58767558150371));
#57865=CARTESIAN_POINT('Ctrl Pts',(16.3087521158423,-19.7716174109842,-2.59181249145407));
#57866=CARTESIAN_POINT('Ctrl Pts',(16.2820372325143,-19.6925680723558,-2.59594862567282));
#57867=CARTESIAN_POINT('Ctrl Pts',(16.2591810094483,-19.6121807387927,-2.60008475989157));
#57868=CARTESIAN_POINT('Ctrl Pts',(16.2403061251851,-19.5308703297896,-2.60422089411032));
#57869=CARTESIAN_POINT('Ctrl Pts',(16.2214331728165,-19.4495682431231,-2.60835660498473));
#57870=CARTESIAN_POINT('Ctrl Pts',(16.2065408484312,-19.3673437264668,-2.61249231585914));
#57871=CARTESIAN_POINT('Ctrl Pts',(16.1957010120584,-19.2846232821293,-2.61662802673355));
#57872=CARTESIAN_POINT('Ctrl Pts',(16.1848552750847,-19.2018578094073,-2.62076598885772));
#57873=CARTESIAN_POINT('Ctrl Pts',(16.1780664813587,-19.1185963356398,-2.62490395098188));
#57874=CARTESIAN_POINT('Ctrl Pts',(16.1753546619781,-19.0352708485527,-2.62904191310604));
#57875=CARTESIAN_POINT('Ctrl Pts',(16.1744266413966,-19.0067557610314,-2.63045797866119));
#57876=CARTESIAN_POINT('Ctrl Pts',(16.1739756253558,-18.9782331861948,-2.63187404421635));
#57877=CARTESIAN_POINT('Ctrl Pts',(16.1740010149441,-18.949720413872,-2.6332901097715));
#57878=CARTESIAN_POINT('Ctrl Pts',(16.1740010149447,-18.9497204131756,-2.63329010980609));
#57879=CARTESIAN_POINT('Ctrl Pts',(16.1740928743929,-18.8465613267996,-2.63841342883191));
#57880=CARTESIAN_POINT('Ctrl Pts',(16.1804238944876,-18.7436786900648,-2.64353674785773));
#57881=CARTESIAN_POINT('Ctrl Pts',(16.1928719236877,-18.6417289897893,-2.64866006688355));
#57882=CARTESIAN_POINT('Ctrl Pts',(16.2055250386107,-18.5380996318225,-2.6538677944185));
#57883=CARTESIAN_POINT('Ctrl Pts',(16.2244983314994,-18.4354341185118,-2.65907552195346));
#57884=CARTESIAN_POINT('Ctrl Pts',(16.249614957165,-18.3343990293583,-2.66428324948841));
#57885=CARTESIAN_POINT('Ctrl Pts',(16.2576437833537,-18.3021019692125,-2.66594796113293));
#57886=CARTESIAN_POINT('Ctrl Pts',(16.2662999939976,-18.2699713447297,-2.66761267277746));
#57887=CARTESIAN_POINT('Ctrl Pts',(16.2755767948953,-18.2380284707337,-2.66927738442199));
#57888=CARTESIAN_POINT('Ctrl Pts',(16.2988961609904,-18.1577327328976,-2.67346201883521));
#57889=CARTESIAN_POINT('Ctrl Pts',(16.3261969265523,-18.0784312369418,-2.67764665324844));
#57890=CARTESIAN_POINT('Ctrl Pts',(16.3573766633345,-18.0005476808496,-2.68183128766167));
#57891=CARTESIAN_POINT('Ctrl Pts',(16.3885120196229,-17.9227749823538,-2.68600996576607));
#57892=CARTESIAN_POINT('Ctrl Pts',(16.4235152107073,-17.8464166382457,-2.69018864387046));
#57893=CARTESIAN_POINT('Ctrl Pts',(16.4622338002164,-17.7718820679608,-2.69436732197485));
#57894=CARTESIAN_POINT('Ctrl Pts',(16.5016463923759,-17.6960115195324,-2.69862089985521));
#57895=CARTESIAN_POINT('Ctrl Pts',(16.5449087556002,-17.6220312333017,-2.70287447773556));
#57896=CARTESIAN_POINT('Ctrl Pts',(16.5918084260802,-17.55035266182,-2.70712805561592));
#57897=CARTESIAN_POINT('Ctrl Pts',(16.6377988552168,-17.4800637188785,-2.71129916961483));
#57898=CARTESIAN_POINT('Ctrl Pts',(16.6872865541291,-17.4119884433508,-2.71547028361375));
#57899=CARTESIAN_POINT('Ctrl Pts',(16.7400252973108,-17.3464892136658,-2.71964139761266));
#57900=CARTESIAN_POINT('Ctrl Pts',(16.7927463434997,-17.2810119628776,-2.72381111195414));
#57901=CARTESIAN_POINT('Ctrl Pts',(16.8487159791043,-17.2181093992061,-2.72798082629562));
#57902=CARTESIAN_POINT('Ctrl Pts',(16.9076465125814,-17.1581123393607,-2.7321505406371));
#57903=CARTESIAN_POINT('Ctrl Pts',(16.9665749490588,-17.0981174144665,-2.73632010660236));
#57904=CARTESIAN_POINT('Ctrl Pts',(17.0284637509529,-17.0410281154314,-2.74048967256763));
#57905=CARTESIAN_POINT('Ctrl Pts',(17.0929880053966,-16.987138774985,-2.7446592385329));
#57906=CARTESIAN_POINT('Ctrl Pts',(17.1597808523048,-16.9313547524114,-2.74897540124711));
#57907=CARTESIAN_POINT('Ctrl Pts',(17.2293975200619,-16.8790002342604,-2.75329156396132));
#57908=CARTESIAN_POINT('Ctrl Pts',(17.3014414464083,-16.8303553571507,-2.75760772667553));
#57909=CARTESIAN_POINT('Ctrl Pts',(17.3711385501861,-16.7832950812868,-2.76178329088851));
#57910=CARTESIAN_POINT('Ctrl Pts',(17.4431067778018,-16.7397066785438,-2.76595885510149));
#57911=CARTESIAN_POINT('Ctrl Pts',(17.5169602827153,-16.6997978939377,-2.77013441931447));
#57912=CARTESIAN_POINT('Ctrl Pts',(17.5945439513522,-16.6578734121651,-2.7745208812793));
#57913=CARTESIAN_POINT('Ctrl Pts',(17.6742078257199,-16.6200102829154,-2.77890734324412));
#57914=CARTESIAN_POINT('Ctrl Pts',(17.7554809190364,-16.5863921694013,-2.78329380520895));
#57915=CARTESIAN_POINT('Ctrl Pts',(17.8367540123529,-16.5527740558871,-2.78768026717377));
#57916=CARTESIAN_POINT('Ctrl Pts',(17.9196357523207,-16.523401080228,-2.79206672913859));
#57917=CARTESIAN_POINT('Ctrl Pts',(18.0036392138267,-16.4983958913426,-2.79645319110342));
#57918=CARTESIAN_POINT('Ctrl Pts',(18.0837805456623,-16.4745403370102,-2.80063798179662));
#57919=CARTESIAN_POINT('Ctrl Pts',(18.1652410320983,-16.4545709643755,-2.80482277248982));
#57920=CARTESIAN_POINT('Ctrl Pts',(18.2476089212221,-16.4386310023227,-2.80900756318302));
#57921=CARTESIAN_POINT('Ctrl Pts',(18.3298587386536,-16.4227138896876,-2.81318635511476));
#57922=CARTESIAN_POINT('Ctrl Pts',(18.4130129271248,-16.4108148007751,-2.8173651470465));
#57923=CARTESIAN_POINT('Ctrl Pts',(18.4966446832037,-16.4030271767654,-2.82154393897824));
#57924=CARTESIAN_POINT('Ctrl Pts',(18.5801762046828,-16.3952488864037,-2.82571772253091));
#57925=CARTESIAN_POINT('Ctrl Pts',(18.6641837002162,-16.3915723068656,-2.82989150608357));
#57926=CARTESIAN_POINT('Ctrl Pts',(18.748231717209,-16.392039559246,-2.83406528963623));
#57927=CARTESIAN_POINT('Ctrl Pts',(18.8322246249333,-16.3925065052547,-2.83823633648948));
#57928=CARTESIAN_POINT('Ctrl Pts',(18.9162575426882,-16.3971118856053,-2.84240738334274));
#57929=CARTESIAN_POINT('Ctrl Pts',(18.999892508799,-16.4058458071506,-2.84657843019599));
#57930=CARTESIAN_POINT('Ctrl Pts',(19.083497725474,-16.41457662199,-2.85074799338403));
#57931=CARTESIAN_POINT('Ctrl Pts',(19.1667048146443,-16.4274330128491,-2.85491755657206));
#57932=CARTESIAN_POINT('Ctrl Pts',(19.2490798028144,-16.4443531355606,-2.8590871197601));
#57933=CARTESIAN_POINT('Ctrl Pts',(19.3314501999323,-16.4612723152533,-2.86325645056349));
#57934=CARTESIAN_POINT('Ctrl Pts',(19.4129881380691,-16.4822546823773,-2.86742578136688));
#57935=CARTESIAN_POINT('Ctrl Pts',(19.4932700684874,-16.5071873357864,-2.87159511217027));
#57936=CARTESIAN_POINT('Ctrl Pts',(19.5736163334742,-16.5321399691772,-2.87576778410031));
#57937=CARTESIAN_POINT('Ctrl Pts',(19.6527041405874,-16.5610490742656,-2.87994045603036));
#57938=CARTESIAN_POINT('Ctrl Pts',(19.7301259599796,-16.5937521182338,-2.8841131279604));
#57939=CARTESIAN_POINT('Ctrl Pts',(19.80758106589,-16.6264692224563,-2.88828759387722));
#57940=CARTESIAN_POINT('Ctrl Pts',(19.8833683419596,-16.6629833163712,-2.89246205979404));
#57941=CARTESIAN_POINT('Ctrl Pts',(19.957103132272,-16.7030849887498,-2.89663652571085));
#57942=CARTESIAN_POINT('Ctrl Pts',(20.0309449059727,-16.7432448455048,-2.90081704844978));
#57943=CARTESIAN_POINT('Ctrl Pts',(20.1027278532674,-16.7870024370963,-2.90499757118871));
#57944=CARTESIAN_POINT('Ctrl Pts',(20.1720950490366,-16.8341041975733,-2.90917809392763));
#57945=CARTESIAN_POINT('Ctrl Pts',(20.213456940573,-16.8621897773121,-2.91167083312771));
#57946=CARTESIAN_POINT('Ctrl Pts',(20.2539605186504,-16.891463544437,-2.91416357232779));
#57947=CARTESIAN_POINT('Ctrl Pts',(20.293535888361,-16.9218650751948,-2.91665631152786));
#57948=CARTESIAN_POINT('',(16.1740009418753,-18.9541959965583,-2.56670989022851));
#57949=CARTESIAN_POINT('Ctrl Pts',(16.172685086933,-18.9541844540912,-2.56671052146184));
#57950=CARTESIAN_POINT('Ctrl Pts',(16.1790130664392,-18.2584131946872,-2.60137099441126));
#57951=CARTESIAN_POINT('Ctrl Pts',(16.8320815170599,-16.7012241087188,-2.67842340292117));
#57952=CARTESIAN_POINT('Ctrl Pts',(18.9167593652634,-16.1584579179283,-2.77291032499143));
#57953=CARTESIAN_POINT('Ctrl Pts',(20.0133687891635,-16.7092013388142,-2.83273677411227));
#57954=CARTESIAN_POINT('Ctrl Pts',(20.2912842963712,-16.9247659399654,-2.85017128767263));
#57955=CARTESIAN_POINT('Ctrl Pts',(20.293535888361,-16.9218650751948,-2.05017637630343));
#57956=CARTESIAN_POINT('Ctrl Pts',(20.3599947739675,-16.972918340639,-2.05435390936659));
#57957=CARTESIAN_POINT('Ctrl Pts',(20.424037310397,-17.0273100671775,-2.05853144242976));
#57958=CARTESIAN_POINT('Ctrl Pts',(20.4853117242371,-17.0847808793423,-2.06270897549293));
#57959=CARTESIAN_POINT('Ctrl Pts',(20.5465213916427,-17.1421909641996,-2.06688209430953));
#57960=CARTESIAN_POINT('Ctrl Pts',(20.6049684159709,-17.2026733548758,-2.07105521312614));
#57961=CARTESIAN_POINT('Ctrl Pts',(20.6603338894341,-17.2659283092295,-2.07522833194274));
#57962=CARTESIAN_POINT('Ctrl Pts',(20.7156675790622,-17.3291469506085,-2.07939905508363));
#57963=CARTESIAN_POINT('Ctrl Pts',(20.7679229277693,-17.3951346502392,-2.08356977822452));
#57964=CARTESIAN_POINT('Ctrl Pts',(20.8168185234436,-17.4635555104741,-2.08774050136541));
#57965=CARTESIAN_POINT('Ctrl Pts',(20.8657007171828,-17.5319576170377,-2.09191008134074));
#57966=CARTESIAN_POINT('Ctrl Pts',(20.9112247197038,-17.6027911854591,-2.09607966131607));
#57967=CARTESIAN_POINT('Ctrl Pts',(20.9531508455286,-17.6756890955611,-2.1002492412914));
#57968=CARTESIAN_POINT('Ctrl Pts',(20.9950780564932,-17.7485888924203,-2.10441892918458));
#57969=CARTESIAN_POINT('Ctrl Pts',(21.0334069776191,-17.8235527376139,-2.10858861707775));
#57970=CARTESIAN_POINT('Ctrl Pts',(21.0679432156334,-17.9001877229283,-2.11275830497093));
#57971=CARTESIAN_POINT('Ctrl Pts',(21.1025145462378,-17.9769005777583,-2.11693222972244));
#57972=CARTESIAN_POINT('Ctrl Pts',(21.1332853065668,-18.0552875441195,-2.12110615447396));
#57973=CARTESIAN_POINT('Ctrl Pts',(21.1601089504552,-18.1349349104745,-2.12528007922547));
#57974=CARTESIAN_POINT('Ctrl Pts',(21.1869458980825,-18.2146217795823,-2.12945607412099));
#57975=CARTESIAN_POINT('Ctrl Pts',(21.2098317045075,-18.2955698507065,-2.13363206901651));
#57976=CARTESIAN_POINT('Ctrl Pts',(21.2286701992247,-18.3773517622928,-2.13780806391203));
#57977=CARTESIAN_POINT('Ctrl Pts',(21.2475424633262,-18.4592802739571,-2.14199154458485));
#57978=CARTESIAN_POINT('Ctrl Pts',(21.2623528380693,-18.5420451588483,-2.14617502525768));
#57979=CARTESIAN_POINT('Ctrl Pts',(21.273056640464,-18.6252105012155,-2.15035850593051));
#57980=CARTESIAN_POINT('Ctrl Pts',(21.2829756094017,-18.7022779224197,-2.15423524181513));
#57981=CARTESIAN_POINT('Ctrl Pts',(21.2893686864234,-18.7796888801639,-2.15811197769975));
#57982=CARTESIAN_POINT('Ctrl Pts',(21.2922402934534,-18.8570968865022,-2.16198871358438));
#57983=CARTESIAN_POINT('Ctrl Pts',(21.2953399702062,-18.9406528171088,-2.16617334886797));
#57984=CARTESIAN_POINT('Ctrl Pts',(21.2943475192283,-19.0245162609818,-2.17035798415156));
#57985=CARTESIAN_POINT('Ctrl Pts',(21.2892270081162,-19.1082527983545,-2.17454261943515));
#57986=CARTESIAN_POINT('Ctrl Pts',(21.2841137854036,-19.1918701473637,-2.17872129842001));
#57987=CARTESIAN_POINT('Ctrl Pts',(21.274884201526,-19.2753604934237,-2.18289997740487));
#57988=CARTESIAN_POINT('Ctrl Pts',(21.2615542857184,-19.3582872539799,-2.18707865638973));
#57989=CARTESIAN_POINT('Ctrl Pts',(21.2479854443897,-19.4427003944775,-2.19133223405123));
#57990=CARTESIAN_POINT('Ctrl Pts',(21.2301678127852,-19.5265290647065,-2.19558581171274));
#57991=CARTESIAN_POINT('Ctrl Pts',(21.208173766456,-19.6093158855382,-2.19983938937424));
#57992=CARTESIAN_POINT('Ctrl Pts',(21.1866061117414,-19.6904977444785,-2.20401050427198));
#57993=CARTESIAN_POINT('Ctrl Pts',(21.1610226544758,-19.7706773244638,-2.20818161916971));
#57994=CARTESIAN_POINT('Ctrl Pts',(21.1315432451786,-19.8494332217488,-2.21235273406745));
#57995=CARTESIAN_POINT('Ctrl Pts',(21.1020737279442,-19.9281626918327,-2.21652244931264));
#57996=CARTESIAN_POINT('Ctrl Pts',(21.0687110161701,-20.0054689975125,-2.22069216455782));
#57997=CARTESIAN_POINT('Ctrl Pts',(21.0316242449842,-20.0809476643586,-2.22486187980301));
#57998=CARTESIAN_POINT('Ctrl Pts',(20.9945387934706,-20.1564236454194,-2.22903144667569));
#57999=CARTESIAN_POINT('Ctrl Pts',(20.9537297496554,-20.2300717044421,-2.23320101354836));
#58000=CARTESIAN_POINT('Ctrl Pts',(20.9094130507601,-20.3015103032518,-2.23737058042103));
#58001=CARTESIAN_POINT('Ctrl Pts',(20.8635382531532,-20.3754605600038,-2.24168674207477));
#58002=CARTESIAN_POINT('Ctrl Pts',(20.8139048344501,-20.4470426505681,-2.2460029037285));
#58003=CARTESIAN_POINT('Ctrl Pts',(20.7608012117367,-20.515865994292,-2.25031906538223));
#58004=CARTESIAN_POINT('Ctrl Pts',(20.7094274096053,-20.582447456381,-2.25449463050257));
#58005=CARTESIAN_POINT('Ctrl Pts',(20.6548063539525,-20.6464468137819,-2.2586701956229));
#58006=CARTESIAN_POINT('Ctrl Pts',(20.5972390425424,-20.7075455762656,-2.26284576074324));
#58007=CARTESIAN_POINT('Ctrl Pts',(20.5367641853794,-20.7717302471062,-2.26723222066367));
#58008=CARTESIAN_POINT('Ctrl Pts',(20.4730380462215,-20.8327132050707,-2.2716186805841));
#58009=CARTESIAN_POINT('Ctrl Pts',(20.4064500165861,-20.8901720620268,-2.27600514050453));
#58010=CARTESIAN_POINT('Ctrl Pts',(20.3398619869507,-20.9476309189828,-2.28039160042496));
#58011=CARTESIAN_POINT('Ctrl Pts',(20.2704125717478,-21.0015653791251,-2.28477806034539));
#58012=CARTESIAN_POINT('Ctrl Pts',(20.1985254700657,-21.0517059669222,-2.28916452026582));
#58013=CARTESIAN_POINT('Ctrl Pts',(20.1299459675163,-21.0995395349505,-2.29334915467529));
#58014=CARTESIAN_POINT('Ctrl Pts',(20.0588929044663,-21.1440987240594,-2.29753378908477));
#58015=CARTESIAN_POINT('Ctrl Pts',(19.9857121094434,-21.1851181775877,-2.30171842349424));
#58016=CARTESIAN_POINT('Ctrl Pts',(19.9126354781746,-21.226079245029,-2.30589710159743));
#58017=CARTESIAN_POINT('Ctrl Pts',(19.8374375284691,-21.2635103616748,-2.31007577970061));
#58018=CARTESIAN_POINT('Ctrl Pts',(19.7604940332823,-21.2971886916911,-2.3142544578038));
#58019=CARTESIAN_POINT('Ctrl Pts',(19.6821713816853,-21.3314706813749,-2.31850803568478));
#58020=CARTESIAN_POINT('Ctrl Pts',(19.6020403867589,-21.3618637479467,-2.32276161356576));
#58021=CARTESIAN_POINT('Ctrl Pts',(19.5205248076212,-21.3881811769646,-2.32701519144673));
#58022=CARTESIAN_POINT('Ctrl Pts',(19.4405895664662,-21.413988391455,-2.33118630545076));
#58023=CARTESIAN_POINT('Ctrl Pts',(19.3593234056757,-21.4358764386427,-2.33535741945479));
#58024=CARTESIAN_POINT('Ctrl Pts',(19.2771455317525,-21.4537179959654,-2.33952853345882));
#58025=CARTESIAN_POINT('Ctrl Pts',(19.194995233359,-21.4715535663921,-2.34369824780777));
#58026=CARTESIAN_POINT('Ctrl Pts',(19.1119342786071,-21.485345246116,-2.34786796215672));
#58027=CARTESIAN_POINT('Ctrl Pts',(19.0283943159569,-21.4950163166469,-2.35203767650567));
#58028=CARTESIAN_POINT('Ctrl Pts',(18.9448573259675,-21.5046870430453,-2.35620724248077));
#58029=CARTESIAN_POINT('Ctrl Pts',(18.8608418190481,-21.5102373997256,-2.36037680845588));
#58030=CARTESIAN_POINT('Ctrl Pts',(18.7767854909901,-21.5116424363103,-2.36454637443098));
#58031=CARTESIAN_POINT('Ctrl Pts',(18.6897738473697,-21.5130968722274,-2.36886253714067));
#58032=CARTESIAN_POINT('Ctrl Pts',(18.6027189860106,-21.5101090568378,-2.37317869985036));
#58033=CARTESIAN_POINT('Ctrl Pts',(18.5161054386262,-21.5027100893915,-2.37749486256005));
#58034=CARTESIAN_POINT('Ctrl Pts',(18.4323133171285,-21.4955521424197,-2.3816704267887));
#58035=CARTESIAN_POINT('Ctrl Pts',(18.3489346599974,-21.4842661264524,-2.38584599101735));
#58036=CARTESIAN_POINT('Ctrl Pts',(18.266400191337,-21.4689327402492,-2.390021555246));
#58037=CARTESIAN_POINT('Ctrl Pts',(18.1796971048713,-21.452824901532,-2.39440801719621));
#58038=CARTESIAN_POINT('Ctrl Pts',(18.0939262957253,-21.4322502184638,-2.39879447914641));
#58039=CARTESIAN_POINT('Ctrl Pts',(18.0095696123222,-21.4073616054278,-2.40318094109662));
#58040=CARTESIAN_POINT('Ctrl Pts',(17.9252129289191,-21.3824729923918,-2.40756740304683));
#58041=CARTESIAN_POINT('Ctrl Pts',(17.8422708932844,-21.3532707138249,-2.41195386499704));
#58042=CARTESIAN_POINT('Ctrl Pts',(17.7611994326681,-21.3199651720832,-2.41634032694725));
#58043=CARTESIAN_POINT('Ctrl Pts',(17.6838581936353,-21.288192069127,-2.42052496109126));
#58044=CARTESIAN_POINT('Ctrl Pts',(17.6079312972239,-21.2525667345156,-2.42470959523527));
#58045=CARTESIAN_POINT('Ctrl Pts',(17.5338290567893,-21.2132363226944,-2.42889422937928));
#58046=CARTESIAN_POINT('Ctrl Pts',(17.4598322918057,-21.1739618928909,-2.4330729072098));
#58047=CARTESIAN_POINT('Ctrl Pts',(17.3876554268637,-21.1309930749775,-2.43725158504032));
#58048=CARTESIAN_POINT('Ctrl Pts',(17.3176892303927,-21.0845252176456,-2.44143026287085));
#58049=CARTESIAN_POINT('Ctrl Pts',(17.246468934763,-21.0372244537998,-2.44568384081909));
#58050=CARTESIAN_POINT('Ctrl Pts',(17.1775397859107,-20.9862981588104,-2.44993741876734));
#58051=CARTESIAN_POINT('Ctrl Pts',(17.1112881539936,-20.9320015820273,-2.45419099671558));
#58052=CARTESIAN_POINT('Ctrl Pts',(17.046320944286,-20.8787576544711,-2.4583621104312));
#58053=CARTESIAN_POINT('Ctrl Pts',(16.983928731977,-20.8222732634782,-2.46253322414681));
#58054=CARTESIAN_POINT('Ctrl Pts',(16.9244454837175,-20.762831978015,-2.46670433786243));
#58055=CARTESIAN_POINT('Ctrl Pts',(16.8649821956771,-20.7034106386898,-2.4708740519177));
#58056=CARTESIAN_POINT('Ctrl Pts',(16.8084262582069,-20.641034700359,-2.47504376597298));
#58057=CARTESIAN_POINT('Ctrl Pts',(16.7550758225426,-20.5760255847352,-2.47921348002825));
#58058=CARTESIAN_POINT('Ctrl Pts',(16.7017272853469,-20.5110187824527,-2.48338304570478));
#58059=CARTESIAN_POINT('Ctrl Pts',(16.651584314341,-20.4433793453335,-2.4875526113813));
#58060=CARTESIAN_POINT('Ctrl Pts',(16.6049048052798,-20.3734618010412,-2.49172217705783));
#58061=CARTESIAN_POINT('Ctrl Pts',(16.5565840957098,-20.3010860323251,-2.4960383401054));
#58062=CARTESIAN_POINT('Ctrl Pts',(16.5119752240842,-20.2262694173157,-2.50035450315297));
#58063=CARTESIAN_POINT('Ctrl Pts',(16.4713143087945,-20.1494362040685,-2.50467066620054));
#58064=CARTESIAN_POINT('Ctrl Pts',(16.4319779239082,-20.0751058347982,-2.50884623012138));
#58065=CARTESIAN_POINT('Ctrl Pts',(16.3963363916713,-19.9988886782757,-2.51302179404221));
#58066=CARTESIAN_POINT('Ctrl Pts',(16.3645549999889,-19.9211905859647,-2.51719735796305));
#58067=CARTESIAN_POINT('Ctrl Pts',(16.3311683990456,-19.8395681312915,-2.52158382057399));
#58068=CARTESIAN_POINT('Ctrl Pts',(16.3020423326888,-19.7563117555003,-2.52597028318493));
#58069=CARTESIAN_POINT('Ctrl Pts',(16.2773090396202,-19.6719093867897,-2.53035674579587));
#58070=CARTESIAN_POINT('Ctrl Pts',(16.2525757465516,-19.5875070180792,-2.53474320840681));
#58071=CARTESIAN_POINT('Ctrl Pts',(16.2322352869843,-19.5019592385255,-2.53912967101775));
#58072=CARTESIAN_POINT('Ctrl Pts',(16.2163575306375,-19.4157632978817,-2.54351613362869));
#58073=CARTESIAN_POINT('Ctrl Pts',(16.193544110504,-19.2919155599045,-2.54981867488562));
#58074=CARTESIAN_POINT('Ctrl Pts',(16.1798641823048,-19.1663368454762,-2.55612121614255));
#58075=CARTESIAN_POINT('Ctrl Pts',(16.1755170133934,-19.040118143674,-2.56242375739948));
#58076=CARTESIAN_POINT('Ctrl Pts',(16.1745315620426,-19.0115058691761,-2.56385246834249));
#58077=CARTESIAN_POINT('Ctrl Pts',(16.1740255308992,-18.9828608310217,-2.5652811792855));
#58078=CARTESIAN_POINT('Ctrl Pts',(16.1740009418753,-18.9541959965583,-2.56670989022851));
#58079=CARTESIAN_POINT('Origin',(18.734,-18.952,1.76670989022851));
#58080=CARTESIAN_POINT('',(20.293535888361,-16.9218650751948,-1.25003886335143));
#58081=CARTESIAN_POINT('',(20.2916962531304,-16.9242237737286,-1.31677679843946));
#58082=CARTESIAN_POINT('',(20.293535888361,-16.9218650751948,1.76670989022851));
#58083=CARTESIAN_POINT('',(16.1742339454204,-18.95300766776,-1.83329006740176));
#58084=CARTESIAN_POINT('Ctrl Pts',(20.2916962531305,-16.9242237737287,-1.31677679843947));
#58085=CARTESIAN_POINT('Ctrl Pts',(20.7197402889178,-17.2576788600888,-1.34369097149553));
#58086=CARTESIAN_POINT('Ctrl Pts',(21.5659317262182,-18.4571855196717,-1.41299708011206));
#58087=CARTESIAN_POINT('Ctrl Pts',(21.0139855935949,-20.9432205334647,-1.52469512428908));
#58088=CARTESIAN_POINT('Ctrl Pts',(18.2938122981759,-21.946916179492,-1.65187093097051));
#58089=CARTESIAN_POINT('Ctrl Pts',(16.4202753042621,-20.536339124494,-1.75473569408312));
#58090=CARTESIAN_POINT('Ctrl Pts',(16.1765569610219,-19.3178333678849,-1.81520852163526));
#58091=CARTESIAN_POINT('Ctrl Pts',(16.1778407221624,-18.9530194401788,-1.83328941362691));
#58092=CARTESIAN_POINT('Ctrl Pts',(16.174000198019,-18.953006904815,-1.8332901097715));
#58093=CARTESIAN_POINT('Ctrl Pts',(16.1739663681252,-18.8669962708809,-1.83754657623655));
#58094=CARTESIAN_POINT('Ctrl Pts',(16.1782715498346,-18.7810104795588,-1.8418030427016));
#58095=CARTESIAN_POINT('Ctrl Pts',(16.186881959491,-18.6955049947587,-1.84605950916664));
#58096=CARTESIAN_POINT('Ctrl Pts',(16.1954973714571,-18.6099498346313,-1.85031844847147));
#58097=CARTESIAN_POINT('Ctrl Pts',(16.2084229438518,-18.5248759665389,-1.85457738777631));
#58098=CARTESIAN_POINT('Ctrl Pts',(16.2255732751413,-18.4407316105854,-1.85883632708114));
#58099=CARTESIAN_POINT('Ctrl Pts',(16.242752034236,-18.3564477798121,-1.86310232585877));
#58100=CARTESIAN_POINT('Ctrl Pts',(16.2641694501873,-18.273096962922,-1.86736832463641));
#58101=CARTESIAN_POINT('Ctrl Pts',(16.2896893999554,-18.1911151923519,-1.87163432341404));
#58102=CARTESIAN_POINT('Ctrl Pts',(16.315231796287,-18.1090613131363,-1.87590407443307));
#58103=CARTESIAN_POINT('Ctrl Pts',(16.3448837660304,-18.02837928517,-1.88017382545211));
#58104=CARTESIAN_POINT('Ctrl Pts',(16.3784607475836,-17.9494857455749,-1.88444357647114));
#58105=CARTESIAN_POINT('Ctrl Pts',(16.4121081360754,-17.8704267756062,-1.88872228065047));
#58106=CARTESIAN_POINT('Ctrl Pts',(16.4496967908486,-17.7931641763823,-1.89300098482979));
#58107=CARTESIAN_POINT('Ctrl Pts',(16.4909957508862,-17.7180907900264,-1.89727968900912));
#58108=CARTESIAN_POINT('Ctrl Pts',(16.5197685295266,-17.6657875377064,-1.90026064078387));
#58109=CARTESIAN_POINT('Ctrl Pts',(16.550341278611,-17.6145463427439,-1.90324159255863));
#58110=CARTESIAN_POINT('Ctrl Pts',(16.582623920045,-17.5644910945881,-1.90622254433338));
#58111=CARTESIAN_POINT('Ctrl Pts',(16.6279420233621,-17.494223953898,-1.91040717962067));
#58112=CARTESIAN_POINT('Ctrl Pts',(16.6767906254559,-17.4260486191802,-1.91459181490796));
#58113=CARTESIAN_POINT('Ctrl Pts',(16.7289503547201,-17.3603417703656,-1.91877645019526));
#58114=CARTESIAN_POINT('Ctrl Pts',(16.7810358412116,-17.2947284469337,-1.92295512918387));
#58115=CARTESIAN_POINT('Ctrl Pts',(16.836422809856,-17.2315769875611,-1.92713380817248));
#58116=CARTESIAN_POINT('Ctrl Pts',(16.8948480567244,-17.1712360825911,-1.93131248716108));
#58117=CARTESIAN_POINT('Ctrl Pts',(16.9543205181339,-17.1098136268105,-1.93556606482166));
#58118=CARTESIAN_POINT('Ctrl Pts',(17.016940988381,-17.0513038784721,-1.93981964248223));
#58119=CARTESIAN_POINT('Ctrl Pts',(17.0823881640359,-16.9960403012068,-1.9440732201428));
#58120=CARTESIAN_POINT('Ctrl Pts',(17.146566536085,-16.94184810136,-1.94824433504437));
#58121=CARTESIAN_POINT('Ctrl Pts',(17.2134626230336,-16.8907776412551,-1.95241544994594));
#58122=CARTESIAN_POINT('Ctrl Pts',(17.282736811581,-16.8431057025209,-1.9565865648475));
#58123=CARTESIAN_POINT('Ctrl Pts',(17.3519877545945,-16.7954497605048,-1.96075628009654));
#58124=CARTESIAN_POINT('Ctrl Pts',(17.4236148357286,-16.7511903355776,-1.96492599534558));
#58125=CARTESIAN_POINT('Ctrl Pts',(17.4972477392747,-16.7105621031153,-1.96909571059463));
#58126=CARTESIAN_POINT('Ctrl Pts',(17.5708780227141,-16.6699353163424,-1.97326527747116));
#58127=CARTESIAN_POINT('Ctrl Pts',(17.6465135834571,-16.6329396866301,-1.97743484434769));
#58128=CARTESIAN_POINT('Ctrl Pts',(17.7237588789704,-16.5997642810762,-1.98160441122423));
#58129=CARTESIAN_POINT('Ctrl Pts',(17.8037199857111,-16.5654224855399,-1.98592057287344));
#58130=CARTESIAN_POINT('Ctrl Pts',(17.8854056436375,-16.5351747548242,-1.99023673452266));
#58131=CARTESIAN_POINT('Ctrl Pts',(17.9683557183502,-16.5091760534216,-1.99455289617187));
#58132=CARTESIAN_POINT('Ctrl Pts',(18.0486037412859,-16.4840242450154,-1.99872846129608));
#58133=CARTESIAN_POINT('Ctrl Pts',(18.1300346026624,-16.4628489694374,-2.00290402642029));
#58134=CARTESIAN_POINT('Ctrl Pts',(18.212219147317,-16.4457388919401,-2.0070795915445));
#58135=CARTESIAN_POINT('Ctrl Pts',(18.2985545773167,-16.4277646377265,-2.01146605145622));
#58136=CARTESIAN_POINT('Ctrl Pts',(18.3857212504153,-16.414277123386,-2.01585251136794));
#58137=CARTESIAN_POINT('Ctrl Pts',(18.4732153214912,-16.4053175793878,-2.02023897127966));
#58138=CARTESIAN_POINT('Ctrl Pts',(18.5607093925672,-16.3963580353896,-2.02462543119138));
#58139=CARTESIAN_POINT('Ctrl Pts',(18.6485302783096,-16.3919264150074,-2.0290118911031));
#58140=CARTESIAN_POINT('Ctrl Pts',(18.7361763184416,-16.3920009250709,-2.03339835101482));
#58141=CARTESIAN_POINT('Ctrl Pts',(18.8197745701694,-16.3920719940094,-2.03758222948031));
#58142=CARTESIAN_POINT('Ctrl Pts',(18.9035248815704,-16.3962424237147,-2.0417661079458));
#58143=CARTESIAN_POINT('Ctrl Pts',(18.9869920193069,-16.4045316413806,-2.04594998641129));
#58144=CARTESIAN_POINT('Ctrl Pts',(19.0703479391413,-16.4128098138685,-2.05012828996194));
#58145=CARTESIAN_POINT('Ctrl Pts',(19.1534209809421,-16.4251958328744,-2.05430659351258));
#58146=CARTESIAN_POINT('Ctrl Pts',(19.2357756009627,-16.4416571456714,-2.05848489706323));
#58147=CARTESIAN_POINT('Ctrl Pts',(19.318045201778,-16.4581014645496,-2.06265888712123));
#58148=CARTESIAN_POINT('Ctrl Pts',(19.3995974052575,-16.4786126315121,-2.06683287717923));
#58149=CARTESIAN_POINT('Ctrl Pts',(19.4800028447553,-16.5031064221537,-2.07100686723723));
#58150=CARTESIAN_POINT('Ctrl Pts',(19.5603542147999,-16.5275837416973,-2.07517805045328));
#58151=CARTESIAN_POINT('Ctrl Pts',(19.6395599135003,-16.5560382324505,-2.07934923366934));
#58152=CARTESIAN_POINT('Ctrl Pts',(19.7172030732731,-16.5883351090507,-2.08352041688539));
#58153=CARTESIAN_POINT('Ctrl Pts',(19.7948145897911,-16.6206188231483,-2.08768990014728));
#58154=CARTESIAN_POINT('Ctrl Pts',(19.8708644093497,-16.6567416327097,-2.09185938340917));
#58155=CARTESIAN_POINT('Ctrl Pts',(19.9449544117899,-16.6965201369627,-2.09602886667105));
#58156=CARTESIAN_POINT('Ctrl Pts',(20.0190582144982,-16.7363060505018,-2.10019912655576));
#58157=CARTESIAN_POINT('Ctrl Pts',(20.0912010629145,-16.7797488058117,-2.10436938644047));
#58158=CARTESIAN_POINT('Ctrl Pts',(20.1610091624569,-16.8266188929361,-2.10853964632518));
#58159=CARTESIAN_POINT('Ctrl Pts',(20.2061939577773,-16.8569565658888,-2.11123893681666));
#58160=CARTESIAN_POINT('Ctrl Pts',(20.2504011024562,-16.8887292250434,-2.11393822730815));
#58161=CARTESIAN_POINT('Ctrl Pts',(20.293535888361,-16.9218650751948,-2.11663751779963));
#58162=CARTESIAN_POINT('',(16.1740004726294,-18.9504444093098,-1.76670989019937));
#58163=CARTESIAN_POINT('Ctrl Pts',(16.1740004726298,-18.9504444087268,-1.7667098902285));
#58164=CARTESIAN_POINT('Ctrl Pts',(16.1740562220874,-18.8586988534878,-1.77129369133236));
#58165=CARTESIAN_POINT('Ctrl Pts',(16.1790436176654,-18.7671041921699,-1.77587749243622));
#58166=CARTESIAN_POINT('Ctrl Pts',(16.1889163327552,-18.6760486877659,-1.78046129354008));
#58167=CARTESIAN_POINT('Ctrl Pts',(16.1979293239818,-18.5929223689306,-1.78464593360694));
#58168=CARTESIAN_POINT('Ctrl Pts',(16.2110359189735,-18.510083390536,-1.78883057367379));
#58169=CARTESIAN_POINT('Ctrl Pts',(16.2282088655394,-18.4279668040492,-1.79301521374065));
#58170=CARTESIAN_POINT('Ctrl Pts',(16.24535736882,-18.3459670990266,-1.79719389755824));
#58171=CARTESIAN_POINT('Ctrl Pts',(16.2665606337553,-18.2646881899744,-1.80137258137583));
#58172=CARTESIAN_POINT('Ctrl Pts',(16.2917396797569,-18.184559755964,-1.80555126519342));
#58173=CARTESIAN_POINT('Ctrl Pts',(16.3173699983022,-18.1029952166205,-1.80980484165292));
#58174=CARTESIAN_POINT('Ctrl Pts',(16.3471199655449,-18.0226232777798,-1.81405841811242));
#58175=CARTESIAN_POINT('Ctrl Pts',(16.3808518405096,-17.9438860483621,-1.81831199457193));
#58176=CARTESIAN_POINT('Ctrl Pts',(16.4139298146452,-17.8666751598207,-1.82248311438838));
#58177=CARTESIAN_POINT('Ctrl Pts',(16.4508365039862,-17.7910366100589,-1.82665423420484));
#58178=CARTESIAN_POINT('Ctrl Pts',(16.4913923920135,-17.7173700487186,-1.8308253540213));
#58179=CARTESIAN_POINT('Ctrl Pts',(16.531934671396,-17.6437282064046,-1.83499507420651));
#58180=CARTESIAN_POINT('Ctrl Pts',(16.5761234959118,-17.5720574410135,-1.83916479439172));
#58181=CARTESIAN_POINT('Ctrl Pts',(16.6237330298035,-17.5027335253662,-1.84333451457693));
#58182=CARTESIAN_POINT('Ctrl Pts',(16.6713408697582,-17.4334120762489,-1.8475040864044));
#58183=CARTESIAN_POINT('Ctrl Pts',(16.7223689159663,-17.3664376895872,-1.85167365823187));
#58184=CARTESIAN_POINT('Ctrl Pts',(16.7765483383152,-17.3021566764789,-1.85584323005933));
#58185=CARTESIAN_POINT('Ctrl Pts',(16.8326324736236,-17.2356158223938,-1.86015938590618));
#58186=CARTESIAN_POINT('Ctrl Pts',(16.8920933527671,-17.1719616497153,-1.86447554175303));
#58187=CARTESIAN_POINT('Ctrl Pts',(16.9545891225287,-17.1115389357183,-1.86879169759988));
#58188=CARTESIAN_POINT('Ctrl Pts',(17.0150492806953,-17.0530843097644,-1.87296726766114));
#58189=CARTESIAN_POINT('Ctrl Pts',(17.0783492743462,-16.9976541389962,-1.87714283772241));
#58190=CARTESIAN_POINT('Ctrl Pts',(17.1441452217407,-16.9455200514219,-1.88131840778368));
#58191=CARTESIAN_POINT('Ctrl Pts',(17.2132640597166,-16.8907530377263,-1.88570485652332));
#58192=CARTESIAN_POINT('Ctrl Pts',(17.2851371188669,-16.8396241343394,-1.89009130526296));
#58193=CARTESIAN_POINT('Ctrl Pts',(17.3593324936003,-16.792396043982,-1.89447775400259));
#58194=CARTESIAN_POINT('Ctrl Pts',(17.4335278683337,-16.7451679536245,-1.89886420274223));
#58195=CARTESIAN_POINT('Ctrl Pts',(17.5100450162907,-16.7018408959928,-1.90325065148187));
#58196=CARTESIAN_POINT('Ctrl Pts',(17.5884257348914,-16.662620257991,-1.90763710022151));
#58197=CARTESIAN_POINT('Ctrl Pts',(17.6632002791341,-16.6252041002441,-1.91182173531041));
#58198=CARTESIAN_POINT('Ctrl Pts',(17.7399490034736,-16.5913855369184,-1.91600637039932));
#58199=CARTESIAN_POINT('Ctrl Pts',(17.8182913485561,-16.5613771385535,-1.92019100548822));
#58200=CARTESIAN_POINT('Ctrl Pts',(17.8965221835584,-16.5314114532183,-1.92436968429646));
#58201=CARTESIAN_POINT('Ctrl Pts',(17.9763417078037,-16.5052453236658,-1.92854836310471));
#58202=CARTESIAN_POINT('Ctrl Pts',(18.0573458795832,-16.4830449171111,-1.93272704191295));
#58203=CARTESIAN_POINT('Ctrl Pts',(18.1398019751916,-16.4604465890842,-1.93698061962086));
#58204=CARTESIAN_POINT('Ctrl Pts',(18.2234851739771,-16.4419577675957,-1.94123419732878));
#58205=CARTESIAN_POINT('Ctrl Pts',(18.3079491747708,-16.427701940277,-1.9454877750367));
#58206=CARTESIAN_POINT('Ctrl Pts',(18.3907756952208,-16.4137224867601,-1.94965888980394));
#58207=CARTESIAN_POINT('Ctrl Pts',(18.4743525389444,-16.403813444343,-1.95383000457117));
#58208=CARTESIAN_POINT('Ctrl Pts',(18.5582464958779,-16.3980401910389,-1.95800111933841));
#58209=CARTESIAN_POINT('Ctrl Pts',(18.642112301844,-16.392268874974,-1.96217083447068));
#58210=CARTESIAN_POINT('Ctrl Pts',(18.7262945511254,-16.390630623423,-1.96634054960296));
#58211=CARTESIAN_POINT('Ctrl Pts',(18.8103550385198,-16.3931389431834,-1.97051026473523));
#58212=CARTESIAN_POINT('Ctrl Pts',(18.8944125351178,-16.3956471737001,-1.9746798315128));
#58213=CARTESIAN_POINT('Ctrl Pts',(18.9783478186395,-16.4023016676252,-1.97884939829037));
#58214=CARTESIAN_POINT('Ctrl Pts',(19.0617241844761,-16.4130638332346,-1.98301896506793));
#58215=CARTESIAN_POINT('Ctrl Pts',(19.1480319248427,-16.4242043787102,-1.98733512688752));
#58216=CARTESIAN_POINT('Ctrl Pts',(19.233740190573,-16.4397467505395,-1.9916512887071));
#58217=CARTESIAN_POINT('Ctrl Pts',(19.3183740371494,-16.4595901250585,-1.99596745052669));
#58218=CARTESIAN_POINT('Ctrl Pts',(19.4002509797579,-16.4787871118714,-2.00014301559772));
#58219=CARTESIAN_POINT('Ctrl Pts',(19.4811219861015,-16.5020090222104,-2.00431858066875));
#58220=CARTESIAN_POINT('Ctrl Pts',(19.560572524251,-16.529113733137,-2.00849414573978));
#58221=CARTESIAN_POINT('Ctrl Pts',(19.6440358680249,-16.5575874207752,-2.01288060593364));
#58222=CARTESIAN_POINT('Ctrl Pts',(19.7259309366168,-16.5903462355689,-2.0172670661275));
#58223=CARTESIAN_POINT('Ctrl Pts',(19.8058030522791,-16.6271692067754,-2.02165352632137));
#58224=CARTESIAN_POINT('Ctrl Pts',(19.8856751679414,-16.6639921779819,-2.02603998651523));
#58225=CARTESIAN_POINT('Ctrl Pts',(19.9635238523658,-16.7048789684718,-2.03042644670909));
#58226=CARTESIAN_POINT('Ctrl Pts',(20.0389283878907,-16.7495554711919,-2.03481290690295));
#58227=CARTESIAN_POINT('Ctrl Pts',(20.1108650768449,-16.7921773063025,-2.03899763425893));
#58228=CARTESIAN_POINT('Ctrl Pts',(20.1808452608001,-16.8384065838528,-2.0431823616149));
#58229=CARTESIAN_POINT('Ctrl Pts',(20.2484841862399,-16.8880383604269,-2.04736708897087));
#58230=CARTESIAN_POINT('Ctrl Pts',(20.2636199533809,-16.8991446133446,-2.04830351808172));
#58231=CARTESIAN_POINT('Ctrl Pts',(20.2786385711608,-16.9104210571001,-2.04923994719258));
#58232=CARTESIAN_POINT('Ctrl Pts',(20.293535888361,-16.9218650751948,-2.05017637630343));
#58233=CARTESIAN_POINT('Ctrl Pts',(20.293535888361,-16.9218650751948,-1.25003886335143));
#58234=CARTESIAN_POINT('Ctrl Pts',(20.360183483879,-16.9730633063139,-1.25422273048467));
#58235=CARTESIAN_POINT('Ctrl Pts',(20.4242257550283,-17.027484305077,-1.25840659761791));
#58236=CARTESIAN_POINT('Ctrl Pts',(20.4853525107207,-17.0848191348474,-1.26259046475115));
#58237=CARTESIAN_POINT('Ctrl Pts',(20.5299990664673,-17.1266960943648,-1.26564633210555));
#58238=CARTESIAN_POINT('Ctrl Pts',(20.5730910166659,-17.1701266981197,-1.26870219945995));
#58239=CARTESIAN_POINT('Ctrl Pts',(20.614521157858,-17.2149795122542,-1.27175806681434));
#58240=CARTESIAN_POINT('Ctrl Pts',(20.6712532028065,-17.2763983680518,-1.2759425952547));
#58241=CARTESIAN_POINT('Ctrl Pts',(20.7250787526129,-17.3407138524111,-1.28012712369507));
#58242=CARTESIAN_POINT('Ctrl Pts',(20.7756877943714,-17.4076195577789,-1.28431165213543));
#58243=CARTESIAN_POINT('Ctrl Pts',(20.8262247790097,-17.4744300028477,-1.28849022264697));
#58244=CARTESIAN_POINT('Ctrl Pts',(20.873554077068,-17.5438229797258,-1.29266879315851));
#58245=CARTESIAN_POINT('Ctrl Pts',(20.9174037166617,-17.6154566187108,-1.29684736367005));
#58246=CARTESIAN_POINT('Ctrl Pts',(20.9620407587122,-17.6883765739313,-1.30110096824612));
#58247=CARTESIAN_POINT('Ctrl Pts',(21.0030716111863,-17.7636181037576,-1.30535457282219));
#58248=CARTESIAN_POINT('Ctrl Pts',(21.04025352208,-17.8407868377789,-1.30960817739827));
#58249=CARTESIAN_POINT('Ctrl Pts',(21.0767133920067,-17.9164570208649,-1.3137791806048));
#58250=CARTESIAN_POINT('Ctrl Pts',(21.1094722614084,-17.9939797943655,-1.31795018381133));
#58251=CARTESIAN_POINT('Ctrl Pts',(21.1383468600458,-18.0729572384759,-1.32212118701787));
#58252=CARTESIAN_POINT('Ctrl Pts',(21.1672117626761,-18.151908162188,-1.32629078961353));
#58253=CARTESIAN_POINT('Ctrl Pts',(21.1921948271095,-18.2323123546668,-1.33046039220919));
#58254=CARTESIAN_POINT('Ctrl Pts',(21.2131612187129,-18.3137526720542,-1.33462999480485));
#58255=CARTESIAN_POINT('Ctrl Pts',(21.2341268601602,-18.3951900755902,-1.33879944821639));
#58256=CARTESIAN_POINT('Ctrl Pts',(21.2510760006384,-18.4776630845829,-1.34296890162792));
#58257=CARTESIAN_POINT('Ctrl Pts',(21.263924266104,-18.560741507724,-1.34713835503945));
#58258=CARTESIAN_POINT('Ctrl Pts',(21.2772250217302,-18.6467457864309,-1.35145464824415));
#58259=CARTESIAN_POINT('Ctrl Pts',(21.2861305792208,-18.7333983970715,-1.35577094144884));
#58260=CARTESIAN_POINT('Ctrl Pts',(21.2906057031231,-18.8202150283278,-1.36008723465354));
#58261=CARTESIAN_POINT('Ctrl Pts',(21.2949348018955,-18.9041987972701,-1.36426268543923));
#58262=CARTESIAN_POINT('Ctrl Pts',(21.2951181997827,-18.9883355761622,-1.36843813622492));
#58263=CARTESIAN_POINT('Ctrl Pts',(21.2911771392428,-19.0721876804588,-1.37261358701061));
#58264=CARTESIAN_POINT('Ctrl Pts',(21.2870366744248,-19.1602824164425,-1.37700030142481));
#58265=CARTESIAN_POINT('Ctrl Pts',(21.2783434340466,-19.2480623296263,-1.381387015839));
#58266=CARTESIAN_POINT('Ctrl Pts',(21.2651832590201,-19.3350291232487,-1.3857737302532));
#58267=CARTESIAN_POINT('Ctrl Pts',(21.2520230839935,-19.421995916871,-1.39016044466739));
#58268=CARTESIAN_POINT('Ctrl Pts',(21.2343961652463,-19.5081490374756,-1.39454715908158));
#58269=CARTESIAN_POINT('Ctrl Pts',(21.2124488480671,-19.5930080401328,-1.39893387349578));
#58270=CARTESIAN_POINT('Ctrl Pts',(21.1915123903351,-19.6739585685189,-1.40311854263622));
#58271=CARTESIAN_POINT('Ctrl Pts',(21.166566824132,-19.7540329106642,-1.40730321177665));
#58272=CARTESIAN_POINT('Ctrl Pts',(21.1377020187579,-19.8328045214571,-1.41148788091709));
#58273=CARTESIAN_POINT('Ctrl Pts',(21.1088782963373,-19.9114640175003,-1.41566659406489));
#58274=CARTESIAN_POINT('Ctrl Pts',(21.0761465717546,-19.9888240368999,-1.41984530721269));
#58275=CARTESIAN_POINT('Ctrl Pts',(21.0396471223768,-20.0644708297639,-1.42402402036049));
#58276=CARTESIAN_POINT('Ctrl Pts',(21.0024938345812,-20.1414727329157,-1.42827758951952));
#58277=CARTESIAN_POINT('Ctrl Pts',(20.9614366228418,-20.2166989566014,-1.43253115867855));
#58278=CARTESIAN_POINT('Ctrl Pts',(20.9166756992289,-20.2897319582023,-1.43678472783758));
#58279=CARTESIAN_POINT('Ctrl Pts',(20.8727820889758,-20.361349830425,-1.44095587739797));
#58280=CARTESIAN_POINT('Ctrl Pts',(20.8253272686825,-20.4308583065096,-1.44512702695836));
#58281=CARTESIAN_POINT('Ctrl Pts',(20.7745466530899,-20.4978878861559,-1.44929817651875));
#58282=CARTESIAN_POINT('Ctrl Pts',(20.723783075874,-20.5648949754245,-1.45346792653688));
#58283=CARTESIAN_POINT('Ctrl Pts',(20.6696961971179,-20.6294244537336,-1.45763767655502));
#58284=CARTESIAN_POINT('Ctrl Pts',(20.6125638119978,-20.6911371436009,-1.46180742657315));
#58285=CARTESIAN_POINT('Ctrl Pts',(20.5554334589444,-20.7528476384907,-1.46597702828293));
#58286=CARTESIAN_POINT('Ctrl Pts',(20.4952581280413,-20.8117412071425,-1.47014662999271));
#58287=CARTESIAN_POINT('Ctrl Pts',(20.4323538975484,-20.867514040325,-1.47431623170249));
#58288=CARTESIAN_POINT('Ctrl Pts',(20.3672392245803,-20.9252467200626,-1.47863235240872));
#58289=CARTESIAN_POINT('Ctrl Pts',(20.299200687246,-20.9796349039107,-1.48294847311494));
#58290=CARTESIAN_POINT('Ctrl Pts',(20.2286263802879,-21.0303868704713,-1.48726459382117));
#58291=CARTESIAN_POINT('Ctrl Pts',(20.1603497774659,-21.0794864934453,-1.4914401935811));
#58292=CARTESIAN_POINT('Ctrl Pts',(20.089700407782,-21.1251828200969,-1.49561579334102));
#58293=CARTESIAN_POINT('Ctrl Pts',(20.0170578148023,-21.1672567896013,-1.49979139310095));
#58294=CARTESIAN_POINT('Ctrl Pts',(19.940748273422,-21.2114546243045,-1.50417777428033));
#58295=CARTESIAN_POINT('Ctrl Pts',(19.8622394999333,-21.251654504136,-1.5085641554597));
#58296=CARTESIAN_POINT('Ctrl Pts',(19.7819968158146,-21.287658937868,-1.51295053663908));
#58297=CARTESIAN_POINT('Ctrl Pts',(19.7017541316958,-21.3236633715999,-1.51733691781846));
#58298=CARTESIAN_POINT('Ctrl Pts',(19.6197781052968,-21.3554722202674,-1.52172329899784));
#58299=CARTESIAN_POINT('Ctrl Pts',(19.5365517913642,-21.3829485025763,-1.52610968017722));
#58300=CARTESIAN_POINT('Ctrl Pts',(19.4571532093435,-21.4091610999082,-1.53029432358371));
#58301=CARTESIAN_POINT('Ctrl Pts',(19.376321311697,-21.4315284613918,-1.53447896699021));
#58302=CARTESIAN_POINT('Ctrl Pts',(19.294463394386,-21.4498952707336,-1.53866361039671));
#58303=CARTESIAN_POINT('Ctrl Pts',(19.2127219863795,-21.4682359383869,-1.54284229775267));
#58304=CARTESIAN_POINT('Ctrl Pts',(19.1299579044461,-21.4825872641847,-1.54702098510862));
#58305=CARTESIAN_POINT('Ctrl Pts',(19.0465949711256,-21.4928432427104,-1.55119967246457));
#58306=CARTESIAN_POINT('Ctrl Pts',(18.9617380510235,-21.5032830235057,-1.55545324806433));
#58307=CARTESIAN_POINT('Ctrl Pts',(18.8762610608014,-21.5094790670078,-1.55970682366408));
#58308=CARTESIAN_POINT('Ctrl Pts',(18.7906234643,-21.5113737091896,-1.56396039926383));
#58309=CARTESIAN_POINT('Ctrl Pts',(18.7066458764304,-21.5132316254179,-1.56813152308422));
#58310=CARTESIAN_POINT('Ctrl Pts',(18.6225143342412,-21.5109533994767,-1.5723026469046));
#58311=CARTESIAN_POINT('Ctrl Pts',(18.5386669500421,-21.5045369732081,-1.57647377072499));
#58312=CARTESIAN_POINT('Ctrl Pts',(18.4548476977165,-21.4981226997328,-1.5806434950798));
#58313=CARTESIAN_POINT('Ctrl Pts',(18.3713128723448,-21.4875730184253,-1.58481321943461));
#58314=CARTESIAN_POINT('Ctrl Pts',(18.2884980293892,-21.4729379195414,-1.58898294378941));
#58315=CARTESIAN_POINT('Ctrl Pts',(18.2056861297709,-21.4583033408063,-1.59315251994729));
#58316=CARTESIAN_POINT('Ctrl Pts',(18.1235946145539,-21.4395837140867,-1.59732209610518));
#58317=CARTESIAN_POINT('Ctrl Pts',(18.0426500220353,-21.4168803638246,-1.60149167226306));
#58318=CARTESIAN_POINT('Ctrl Pts',(17.9588599464441,-21.3933789120853,-1.60580782347935));
#58319=CARTESIAN_POINT('Ctrl Pts',(17.8762994409707,-21.3656085753716,-1.61012397469565));
#58320=CARTESIAN_POINT('Ctrl Pts',(17.7954238784078,-21.3337377823717,-1.61444012591195));
#58321=CARTESIAN_POINT('Ctrl Pts',(17.7171824220401,-21.3029050168134,-1.61861570066365));
#58322=CARTESIAN_POINT('Ctrl Pts',(17.6405182464777,-21.2682350343783,-1.62279127541534));
#58323=CARTESIAN_POINT('Ctrl Pts',(17.5658209821028,-21.2299283970627,-1.62696685016703));
#58324=CARTESIAN_POINT('Ctrl Pts',(17.4873515385791,-21.1896872913332,-1.63135328961563));
#58325=CARTESIAN_POINT('Ctrl Pts',(17.4110533971718,-21.1454328556654,-1.63573972906424));
#58326=CARTESIAN_POINT('Ctrl Pts',(17.3373445042313,-21.097449469491,-1.64012616851284));
#58327=CARTESIAN_POINT('Ctrl Pts',(17.2636356112909,-21.0494660833166,-1.64451260796144));
#58328=CARTESIAN_POINT('Ctrl Pts',(17.1925163913427,-20.9977541493591,-1.64889904741004));
#58329=CARTESIAN_POINT('Ctrl Pts',(17.1243635064003,-20.9426457139511,-1.65328548685865));
#58330=CARTESIAN_POINT('Ctrl Pts',(17.0601943718463,-20.8907585398463,-1.6574155251311));
#58331=CARTESIAN_POINT('Ctrl Pts',(16.9984022164044,-20.8356563912925,-1.66154556340355));
#58332=CARTESIAN_POINT('Ctrl Pts',(16.9393333497915,-20.7775880188667,-1.66567560167601));
#58333=CARTESIAN_POINT('Ctrl Pts',(16.8791242536685,-20.7183987298625,-1.66988536369781));
#58334=CARTESIAN_POINT('Ctrl Pts',(16.8217451259872,-20.6561277338344,-1.67409512571962));
#58335=CARTESIAN_POINT('Ctrl Pts',(16.7675298313412,-20.5910836085371,-1.67830488774143));
#58336=CARTESIAN_POINT('Ctrl Pts',(16.7144792342514,-20.5274368146437,-1.6824242121926));
#58337=CARTESIAN_POINT('Ctrl Pts',(16.6644582227548,-20.4611352262018,-1.68654353664378));
#58338=CARTESIAN_POINT('Ctrl Pts',(16.6177431437369,-20.3925057855904,-1.69066286109495));
#58339=CARTESIAN_POINT('Ctrl Pts',(16.5710563620564,-20.3239179167901,-1.69477969029369));
#58340=CARTESIAN_POINT('Ctrl Pts',(16.5276718049372,-20.2530053838409,-1.69889651949243));
#58341=CARTESIAN_POINT('Ctrl Pts',(16.4878244177667,-20.1801267254559,-1.70301334869118));
#58342=CARTESIAN_POINT('Ctrl Pts',(16.4479884749074,-20.1072689980804,-1.70712899552195));
#58343=CARTESIAN_POINT('Ctrl Pts',(16.4116879114515,-20.0324466815215,-1.71124464235271));
#58344=CARTESIAN_POINT('Ctrl Pts',(16.3791125478311,-19.9560443653632,-1.71536028918348));
#58345=CARTESIAN_POINT('Ctrl Pts',(16.3452431871199,-19.8766071061112,-1.71963942260147));
#58346=CARTESIAN_POINT('Ctrl Pts',(16.3154014154543,-19.795462185038,-1.72391855601946));
#58347=CARTESIAN_POINT('Ctrl Pts',(16.28974541526,-19.7130647311349,-1.72819768943746));
#58348=CARTESIAN_POINT('Ctrl Pts',(16.2650470315947,-19.6337427825017,-1.73231710314623));
#58349=CARTESIAN_POINT('Ctrl Pts',(16.2442275676729,-19.5532606331567,-1.736436516855));
#58350=CARTESIAN_POINT('Ctrl Pts',(16.2273766226977,-19.4720377335941,-1.74055593056377));
#58351=CARTESIAN_POINT('Ctrl Pts',(16.2105163820987,-19.3907700283831,-1.74467761669822));
#58352=CARTESIAN_POINT('Ctrl Pts',(16.1976290876222,-19.3087612270287,-1.74879930283266));
#58353=CARTESIAN_POINT('Ctrl Pts',(16.1887526585032,-19.2264375531951,-1.7529209889671));
#58354=CARTESIAN_POINT('Ctrl Pts',(16.1798641546722,-19.1440018934889,-1.75704828188022));
#58355=CARTESIAN_POINT('Ctrl Pts',(16.1749974203025,-19.0612509779236,-1.76117557479333));
#58356=CARTESIAN_POINT('Ctrl Pts',(16.174138321227,-18.9786117558525,-1.76530286770644));
#58357=CARTESIAN_POINT('Ctrl Pts',(16.1740406969692,-18.9692209964452,-1.76577187520409));
#58358=CARTESIAN_POINT('Ctrl Pts',(16.1739947684326,-18.9598316737892,-1.76624088270173));
#58359=CARTESIAN_POINT('Ctrl Pts',(16.1740004726294,-18.9504444093098,-1.76670989019937));
#58360=CARTESIAN_POINT('Origin',(18.734,-18.952,1.76670989022851));
#58361=CARTESIAN_POINT('',(20.2910039261765,-16.9251777670034,-0.450077510764929));
#58362=CARTESIAN_POINT('',(20.2957383198016,-16.919032322281,-0.51674866945634));
#58363=CARTESIAN_POINT('',(20.293535888361,-16.9218650751948,1.76670989022851));
#58364=CARTESIAN_POINT('',(16.1765334791563,-18.9551432954109,-0.166709890228505));
#58365=CARTESIAN_POINT('Ctrl Pts',(16.1765334791563,-18.9551432954109,-0.166709890228505));
#58366=CARTESIAN_POINT('Ctrl Pts',(16.1810511645957,-18.366678437132,-0.195923797939959));
#58367=CARTESIAN_POINT('Ctrl Pts',(16.6739009874383,-16.9152607583549,-0.267529641211892));
#58368=CARTESIAN_POINT('Ctrl Pts',(18.6725570461647,-16.1123849326032,-0.361985514724032));
#58369=CARTESIAN_POINT('Ctrl Pts',(19.9247548372555,-16.6451525276585,-0.42722748052472));
#58370=CARTESIAN_POINT('Ctrl Pts',(20.2910039261765,-16.9251777670034,-0.450077510764929));
#58371=CARTESIAN_POINT('',(18.0722627314315,-21.4249949024184,0.));
#58372=CARTESIAN_POINT('Ctrl Pts',(18.0722627314315,-21.4249949024184,8.32667268468867E-16));
#58373=CARTESIAN_POINT('Ctrl Pts',(17.2488902483963,-21.2046724677036,-0.0423919355604773));
#58374=CARTESIAN_POINT('Ctrl Pts',(16.3345567445347,-20.3367913268265,-0.0979618989699792));
#58375=CARTESIAN_POINT('Ctrl Pts',(16.174495607841,-19.2205924221476,-0.153531862379481));
#58376=CARTESIAN_POINT('Ctrl Pts',(16.1765334791563,-18.9551432954109,-0.166709890228505));
#58377=CARTESIAN_POINT('',(19.3957675194894,-21.4249868075161,-1.730088294849E-11));
#58378=CARTESIAN_POINT('Origin',(18.734,-18.952,0.));
#58379=CARTESIAN_POINT('',(16.1740007446509,-18.9500474088581,-0.233290109771496));
#58380=CARTESIAN_POINT('Ctrl Pts',(19.3957675194894,-21.4249868075161,-1.73008274373387E-11));
#58381=CARTESIAN_POINT('Ctrl Pts',(19.3150528143647,-21.4465859402064,-0.00418159702990585));
#58382=CARTESIAN_POINT('Ctrl Pts',(19.2331283755591,-21.4642697491679,-0.0083631940425111));
#58383=CARTESIAN_POINT('Ctrl Pts',(19.1504091626665,-21.4779064529882,-0.0125447910551162));
#58384=CARTESIAN_POINT('Ctrl Pts',(19.0678077425558,-21.4915237380395,-0.0167204334420983));
#58385=CARTESIAN_POINT('Ctrl Pts',(18.9844142470727,-21.501105290632,-0.0208960758290806));
#58386=CARTESIAN_POINT('Ctrl Pts',(18.9006573352602,-21.506569500445,-0.0250717182160627));
#58387=CARTESIAN_POINT('Ctrl Pts',(18.8165041727153,-21.5120595612247,-0.029267115406781));
#58388=CARTESIAN_POINT('Ctrl Pts',(18.7319846004062,-21.5133930928997,-0.0334625125974991));
#58389=CARTESIAN_POINT('Ctrl Pts',(18.6475423362417,-21.5105396366634,-0.0376579097882175));
#58390=CARTESIAN_POINT('Ctrl Pts',(18.5636493303861,-21.5077047408548,-0.041826017838971));
#58391=CARTESIAN_POINT('Ctrl Pts',(18.4798330960835,-21.5007371781061,-0.0459941258897243));
#58392=CARTESIAN_POINT('Ctrl Pts',(18.3965306502634,-21.4896592438679,-0.0501622339404779));
#58393=CARTESIAN_POINT('Ctrl Pts',(18.3132562868314,-21.4785850441522,-0.0543289368652889));
#58394=CARTESIAN_POINT('Ctrl Pts',(18.2304958242585,-21.4634032856077,-0.0584956397901002));
#58395=CARTESIAN_POINT('Ctrl Pts',(18.1486808249577,-21.4441880874701,-0.0626623427149111));
#58396=CARTESIAN_POINT('Ctrl Pts',(18.0668687681529,-21.4249735804117,-0.0668288957832525));
#58397=CARTESIAN_POINT('Ctrl Pts',(17.9860025553434,-21.4017260285035,-0.0709954488515935));
#58398=CARTESIAN_POINT('Ctrl Pts',(17.9065018743522,-21.3745702986806,-0.0751620019199348));
#58399=CARTESIAN_POINT('Ctrl Pts',(17.8260461859792,-21.3470883587911,-0.0793786059927156));
#58400=CARTESIAN_POINT('Ctrl Pts',(17.7469895187101,-21.3156038569086,-0.0835952100654965));
#58401=CARTESIAN_POINT('Ctrl Pts',(17.6697476372837,-21.2802969974753,-0.0878118141382773));
#58402=CARTESIAN_POINT('Ctrl Pts',(17.5933153937669,-21.24536021929,-0.0919842203944796));
#58403=CARTESIAN_POINT('Ctrl Pts',(17.5186604552654,-21.2066811083584,-0.0961566266506819));
#58404=CARTESIAN_POINT('Ctrl Pts',(17.4461606843492,-21.1644804851262,-0.100329032906884));
#58405=CARTESIAN_POINT('Ctrl Pts',(17.3725089409092,-21.1216093224172,-0.104567735887954));
#58406=CARTESIAN_POINT('Ctrl Pts',(17.3010818658164,-21.0751040329196,-0.108806438869025));
#58407=CARTESIAN_POINT('Ctrl Pts',(17.2322432557832,-21.0252406230824,-0.113045141850095));
#58408=CARTESIAN_POINT('Ctrl Pts',(17.1634046457499,-20.9753772132452,-0.117283844831166));
#58409=CARTESIAN_POINT('Ctrl Pts',(17.0971548434137,-20.922156041386,-0.121522547812235));
#58410=CARTESIAN_POINT('Ctrl Pts',(17.0338195258261,-20.8658929842699,-0.125761250793306));
#58411=CARTESIAN_POINT('Ctrl Pts',(16.9721381141262,-20.8110991516714,-0.129889266466191));
#58412=CARTESIAN_POINT('Ctrl Pts',(16.9129812124539,-20.7532072684117,-0.134017282139077));
#58413=CARTESIAN_POINT('Ctrl Pts',(16.8566825230424,-20.6924824304513,-0.138145297811962));
#58414=CARTESIAN_POINT('Ctrl Pts',(16.8004749041019,-20.6318558228343,-0.142266635881243));
#58415=CARTESIAN_POINT('Ctrl Pts',(16.7471166297386,-20.5684057102785,-0.146387973950524));
#58416=CARTESIAN_POINT('Ctrl Pts',(16.6969071781283,-20.5024363369964,-0.150509312019806));
#58417=CARTESIAN_POINT('Ctrl Pts',(16.6467433529369,-20.4365269115162,-0.154626904939698));
#58418=CARTESIAN_POINT('Ctrl Pts',(16.5997229596986,-20.3681031412178,-0.158744497859592));
#58419=CARTESIAN_POINT('Ctrl Pts',(16.556106820746,-20.2975041061843,-0.162862090779484));
#58420=CARTESIAN_POINT('Ctrl Pts',(16.5125163940206,-20.2269466901128,-0.166977256329893));
#58421=CARTESIAN_POINT('Ctrl Pts',(16.4723264872833,-20.1542169560892,-0.171092421880302));
#58422=CARTESIAN_POINT('Ctrl Pts',(16.4357550860861,-20.0796836061897,-0.175207587430711));
#58423=CARTESIAN_POINT('Ctrl Pts',(16.3991935731796,-20.005170408852,-0.179321640309701));
#58424=CARTESIAN_POINT('Ctrl Pts',(16.3662488306016,-19.9288549893914,-0.18343569318869));
#58425=CARTESIAN_POINT('Ctrl Pts',(16.3370925482441,-19.8511299504059,-0.18754974606768));
#58426=CARTESIAN_POINT('Ctrl Pts',(16.3079200305593,-19.7733616311617,-0.191666089807838));
#58427=CARTESIAN_POINT('Ctrl Pts',(16.2825403576348,-19.694182567114,-0.195782433547997));
#58428=CARTESIAN_POINT('Ctrl Pts',(16.2610764230542,-19.6140037632713,-0.199898777288155));
#58429=CARTESIAN_POINT('Ctrl Pts',(16.239606571648,-19.5338028570508,-0.204016255754456));
#58430=CARTESIAN_POINT('Ctrl Pts',(16.2220547122219,-19.4526021247793,-0.208133734220756));
#58431=CARTESIAN_POINT('Ctrl Pts',(16.2084928022863,-19.3708238225034,-0.212251212687057));
#58432=CARTESIAN_POINT('Ctrl Pts',(16.1949128185011,-19.2889365349339,-0.216374178484198));
#58433=CARTESIAN_POINT('Ctrl Pts',(16.1853334601433,-19.2064706109328,-0.22049714428134));
#58434=CARTESIAN_POINT('Ctrl Pts',(16.1797748249049,-19.1238538766228,-0.224620110078481));
#58435=CARTESIAN_POINT('Ctrl Pts',(16.1758784900672,-19.0659435359969,-0.227510109976153));
#58436=CARTESIAN_POINT('Ctrl Pts',(16.1739565735353,-19.0079591859799,-0.230400109873824));
#58437=CARTESIAN_POINT('Ctrl Pts',(16.1740007446509,-18.9500474088581,-0.233290109771496));
#58438=CARTESIAN_POINT('Ctrl Pts',(16.1719919811635,-18.9500458767116,-0.233290109771496));
#58439=CARTESIAN_POINT('Ctrl Pts',(16.1708576376271,-18.8187090077496,-0.239839092339242));
#58440=CARTESIAN_POINT('Ctrl Pts',(16.2398215302323,-17.838374208454,-0.288780010467466));
#58441=CARTESIAN_POINT('Ctrl Pts',(17.5061738910726,-16.184820909787,-0.380112864156167));
#58442=CARTESIAN_POINT('Ctrl Pts',(19.5043144349347,-16.3488645227434,-0.468050068150036));
#58443=CARTESIAN_POINT('Ctrl Pts',(20.245887371914,-16.8802618854419,-0.513595336583427));
#58444=CARTESIAN_POINT('Ctrl Pts',(20.2957383198016,-16.919032322281,-0.51674866945634));
#58445=CARTESIAN_POINT('Origin',(-18.734,-18.952,1.76670989022851));
#58446=CARTESIAN_POINT('',(-17.1724222329607,-16.9192441176791,-21.2501821957929));
#58447=CARTESIAN_POINT('',(-17.1763092963127,-16.9243021577154,-21.3166133914793));
#58448=CARTESIAN_POINT('',(-17.1744641548914,-16.9218650419685,1.76670989022851));
#58449=CARTESIAN_POINT('',(-21.2914666104891,-18.9488558930302,-21.8332901097715));
#58450=CARTESIAN_POINT('Ctrl Pts',(-17.1763092963129,-16.9243021577153,
-21.3166133914793));
#58451=CARTESIAN_POINT('Ctrl Pts',(-16.9218454642793,-17.1171758532038,
-21.3324492498505));
#58452=CARTESIAN_POINT('Ctrl Pts',(-16.1161224117162,-17.9919927187592,
-21.3906770437821));
#58453=CARTESIAN_POINT('Ctrl Pts',(-16.015951839906,-20.2843427864635,-21.4912967732743));
#58454=CARTESIAN_POINT('Ctrl Pts',(-18.3819425515704,-21.9577205200055,
-21.6184725799557));
#58455=CARTESIAN_POINT('Ctrl Pts',(-20.7940987275605,-20.9887402433146,
-21.7324703587881));
#58456=CARTESIAN_POINT('Ctrl Pts',(-21.2869488458059,-19.5373211115314,
-21.80407620206));
#58457=CARTESIAN_POINT('Ctrl Pts',(-21.2914666104891,-18.9488558930302,
-21.8332901097715));
#58458=CARTESIAN_POINT('',(-19.3957372685685,-16.4790050975816,-22.));
#58459=CARTESIAN_POINT('Ctrl Pts',(-21.2914666104891,-18.9488558930302,
-21.8332901097715));
#58460=CARTESIAN_POINT('Ctrl Pts',(-21.2935045175504,-18.6834066038016,
-21.8464681376205));
#58461=CARTESIAN_POINT('Ctrl Pts',(-21.1334434961762,-17.5672072134799,
-21.90203810103));
#58462=CARTESIAN_POINT('Ctrl Pts',(-20.2191097516036,-16.6993275322964,
-21.9576080644395));
#58463=CARTESIAN_POINT('Ctrl Pts',(-19.3957372685685,-16.4790050975816,
-22.));
#58464=CARTESIAN_POINT('',(-18.072232390111,-16.4790132166747,-21.9999999999826));
#58465=CARTESIAN_POINT('Origin',(-18.734,-18.952,-22.));
#58466=CARTESIAN_POINT('',(-21.2939992553327,-18.9539526125931,-21.7667098902285));
#58467=CARTESIAN_POINT('Ctrl Pts',(-21.2939992553327,-18.9539526125931,
-21.7667098902285));
#58468=CARTESIAN_POINT('Ctrl Pts',(-21.2940622837578,-18.8713183400037,
-21.7708336287807));
#58469=CARTESIAN_POINT('Ctrl Pts',(-21.290120073806,-18.7885361132696,-21.7749573673329));
#58470=CARTESIAN_POINT('Ctrl Pts',(-21.2821561914378,-18.7060324736127,
-21.7790811058851));
#58471=CARTESIAN_POINT('Ctrl Pts',(-21.2742021133718,-18.6236304038401,
-21.7831997677201));
#58472=CARTESIAN_POINT('Ctrl Pts',(-21.2622362429578,-18.5415067083406,
-21.7873184295551));
#58473=CARTESIAN_POINT('Ctrl Pts',(-21.2462941819498,-18.4600874637281,
-21.7914370913901));
#58474=CARTESIAN_POINT('Ctrl Pts',(-21.2303628128015,-18.3787228245485,
-21.7955529909627));
#58475=CARTESIAN_POINT('Ctrl Pts',(-21.2104606337788,-18.2980621623454,
-21.7996688905354));
#58476=CARTESIAN_POINT('Ctrl Pts',(-21.1866748711293,-18.2185247267081,
-21.803784790108));
#58477=CARTESIAN_POINT('Ctrl Pts',(-21.1628974701717,-18.1390152518109,
-21.8078992427696));
#58478=CARTESIAN_POINT('Ctrl Pts',(-21.1352393308965,-18.0606286731435,
-21.8120136954312));
#58479=CARTESIAN_POINT('Ctrl Pts',(-21.1038380346635,-17.9837708486818,
-21.8161281480927));
#58480=CARTESIAN_POINT('Ctrl Pts',(-21.0724377570491,-17.9069155173914,
-21.8202424672866));
#58481=CARTESIAN_POINT('Ctrl Pts',(-21.0372947445442,-17.8315892795539,
-21.8243567864805));
#58482=CARTESIAN_POINT('Ctrl Pts',(-20.9985948099081,-17.758178259983,-21.8284711056744));
#58483=CARTESIAN_POINT('Ctrl Pts',(-20.959859225451,-17.6846996152406,-21.8325892149197));
#58484=CARTESIAN_POINT('Ctrl Pts',(-20.9175603979486,-17.613140131245,-21.836707324165));
#58485=CARTESIAN_POINT('Ctrl Pts',(-20.8719298849008,-17.5438608707773,
-21.8408254334103));
#58486=CARTESIAN_POINT('Ctrl Pts',(-20.8262774812034,-17.4745483744787,
-21.8449455182654));
#58487=CARTESIAN_POINT('Ctrl Pts',(-20.7772904911253,-17.4075186609022,
-21.8490656031205));
#58488=CARTESIAN_POINT('Ctrl Pts',(-20.7252420557879,-17.3431012849587,
-21.8531856879756));
#58489=CARTESIAN_POINT('Ctrl Pts',(-20.6731075913472,-17.2785774357072,
-21.85731258278));
#58490=CARTESIAN_POINT('Ctrl Pts',(-20.6179018945763,-17.2166748979188,
-21.8614394775843));
#58491=CARTESIAN_POINT('Ctrl Pts',(-20.5599360513378,-17.1576874473981,
-21.8655663723887));
#58492=CARTESIAN_POINT('Ctrl Pts',(-20.5193323481527,-17.1163681324571,
-21.8684571646614));
#58493=CARTESIAN_POINT('Ctrl Pts',(-20.4773751065851,-17.076478372295,-21.871347956934));
#58494=CARTESIAN_POINT('Ctrl Pts',(-20.4341804678598,-17.0381070101209,
-21.8742387492067));
#58495=CARTESIAN_POINT('Ctrl Pts',(-20.3717052812394,-16.9826080388726,
-21.8784198881639));
#58496=CARTESIAN_POINT('Ctrl Pts',(-20.3063943198782,-16.9300688092441,
-21.8826010271211));
#58497=CARTESIAN_POINT('Ctrl Pts',(-20.2385599097816,-16.8807927486903,
-21.8867821660783));
#58498=CARTESIAN_POINT('Ctrl Pts',(-20.1708205215985,-16.8315857136584,
-21.8909574481286));
#58499=CARTESIAN_POINT('Ctrl Pts',(-20.1005650755227,-16.7856330369313,
-21.8951327301788));
#58500=CARTESIAN_POINT('Ctrl Pts',(-20.0281405702344,-16.7431993787412,
-21.8993080122291));
#58501=CARTESIAN_POINT('Ctrl Pts',(-19.9553653729372,-16.7005602494225,
-21.9035035117188));
#58502=CARTESIAN_POINT('Ctrl Pts',(-19.880400404287,-16.6614746253178,-21.9076990112086));
#58503=CARTESIAN_POINT('Ctrl Pts',(-19.8036290904368,-16.6261681898961,
-21.9118945106983));
#58504=CARTESIAN_POINT('Ctrl Pts',(-19.7273611982937,-16.5910932735809,
-21.916062498538));
#58505=CARTESIAN_POINT('Ctrl Pts',(-19.6493110036014,-16.5597483260403,
-21.9202304863778));
#58506=CARTESIAN_POINT('Ctrl Pts',(-19.5698794212801,-16.5323087814598,
-21.9243984742175));
#58507=CARTESIAN_POINT('Ctrl Pts',(-19.4904728949047,-16.5048778924257,
-21.9285651473047));
#58508=CARTESIAN_POINT('Ctrl Pts',(-19.4096862815083,-16.4813501100524,
-21.9327318203918));
#58509=CARTESIAN_POINT('Ctrl Pts',(-19.3279387681294,-16.4618520646932,
-21.936898493479));
#58510=CARTESIAN_POINT('Ctrl Pts',(-19.2461924230011,-16.4423542979797,
-21.9410651070204));
#58511=CARTESIAN_POINT('Ctrl Pts',(-19.1634856536714,-16.4268862595724,
-21.9452317205618));
#58512=CARTESIAN_POINT('Ctrl Pts',(-19.0802496942046,-16.415523871734,-21.9493983341032));
#58513=CARTESIAN_POINT('Ctrl Pts',(-18.9960110559548,-16.4040246100579,
-21.9536151395932));
#58514=CARTESIAN_POINT('Ctrl Pts',(-18.9112308686983,-16.39673065975,-21.9578319450831));
#58515=CARTESIAN_POINT('Ctrl Pts',(-18.8263615920593,-16.3936666878,-21.962048750573));
#58516=CARTESIAN_POINT('Ctrl Pts',(-18.742380245673,-16.3906347721311,-21.9662214384587));
#58517=CARTESIAN_POINT('Ctrl Pts',(-18.6583121305892,-16.3917446684187,
-21.9703941263443));
#58518=CARTESIAN_POINT('Ctrl Pts',(-18.5745939384244,-16.3969677678094,
-21.97456681423));
#58519=CARTESIAN_POINT('Ctrl Pts',(-18.4895480243537,-16.402273702523,-21.9788056785221));
#58520=CARTESIAN_POINT('Ctrl Pts',(-18.4048637212048,-16.4118243850528,
-21.9830445428142));
#58521=CARTESIAN_POINT('Ctrl Pts',(-18.3209897195339,-16.4255355715488,
-21.9872834071063));
#58522=CARTESIAN_POINT('Ctrl Pts',(-18.237115717863,-16.4392467580448,-21.9915222713984));
#58523=CARTESIAN_POINT('Ctrl Pts',(-18.1540524839651,-16.4571182804316,
-21.9957611356905));
#58524=CARTESIAN_POINT('Ctrl Pts',(-18.072232390111,-16.4790132166747,-21.9999999999825));
#58525=CARTESIAN_POINT('Ctrl Pts',(-17.1724222329607,-16.9192441176791,
-21.2501821957929));
#58526=CARTESIAN_POINT('Ctrl Pts',(-16.5648621340115,-17.3928060882893,
-21.2886333046889));
#58527=CARTESIAN_POINT('Ctrl Pts',(-15.7493320480079,-19.0034153957527,
-21.3694763491455));
#58528=CARTESIAN_POINT('Ctrl Pts',(-17.0720919824152,-21.4819373889294,
-21.4927113291624));
#58529=CARTESIAN_POINT('Ctrl Pts',(-19.9618261650098,-21.7191790573139,
-21.6198871358439));
#58530=CARTESIAN_POINT('Ctrl Pts',(-21.2281784624135,-20.0656258695291,
-21.7112199895325));
#58531=CARTESIAN_POINT('Ctrl Pts',(-21.297142385429,-19.0852910214283,-21.7601609076607));
#58532=CARTESIAN_POINT('Ctrl Pts',(-21.2960080465361,-18.9539541447775,
-21.7667098902285));
#58533=CARTESIAN_POINT('Origin',(-18.734,-18.952,1.76670989022851));
#58534=CARTESIAN_POINT('',(-17.1739275304994,-16.9211547578705,-20.4499991767297));
#58535=CARTESIAN_POINT('',(-17.1744641548914,-16.9218650419685,-20.5167504990879));
#58536=CARTESIAN_POINT('',(-17.1744641548914,-16.9218650419685,1.76670989022851));
#58537=CARTESIAN_POINT('',(-21.2939288361815,-18.9533417016661,-21.0332900817679));
#58538=CARTESIAN_POINT('Ctrl Pts',(-17.1744641548914,-16.9218650419685,
-20.5167504990879));
#58539=CARTESIAN_POINT('Ctrl Pts',(-17.1078270588004,-16.9730552052415,
-20.5209209383463));
#58540=CARTESIAN_POINT('Ctrl Pts',(-17.0436731835532,-17.0275603476493,
-20.5250913776047));
#58541=CARTESIAN_POINT('Ctrl Pts',(-16.9823431362282,-17.0851046543523,
-20.529261816863));
#58542=CARTESIAN_POINT('Ctrl Pts',(-16.9210263043821,-17.1426365613327,
-20.5334313574697));
#58543=CARTESIAN_POINT('Ctrl Pts',(-16.8625324269728,-17.2032060169337,
-20.5376008980763));
#58544=CARTESIAN_POINT('Ctrl Pts',(-16.8071670928462,-17.2664986063758,
-20.541770438683));
#58545=CARTESIAN_POINT('Ctrl Pts',(-16.7517970815659,-17.3297965426503,
-20.5459403315241));
#58546=CARTESIAN_POINT('Ctrl Pts',(-16.6995564402482,-17.3958177224365,
-20.5501102243653));
#58547=CARTESIAN_POINT('Ctrl Pts',(-16.6507112074467,-17.4642137899477,
-20.5542801172065));
#58548=CARTESIAN_POINT('Ctrl Pts',(-16.6018146060796,-17.5326817868506,
-20.5584543953561));
#58549=CARTESIAN_POINT('Ctrl Pts',(-16.556320811115,-17.6035292833675,-20.5626286735058));
#58550=CARTESIAN_POINT('Ctrl Pts',(-16.5144528430049,-17.6763784190149,
-20.5668029516555));
#58551=CARTESIAN_POINT('Ctrl Pts',(-16.4725619106312,-17.7492675118618,
-20.5709795193651));
#58552=CARTESIAN_POINT('Ctrl Pts',(-16.434300974443,-17.8241600201155,-20.5751560870748));
#58553=CARTESIAN_POINT('Ctrl Pts',(-16.3998462116972,-17.9006551029506,
-20.5793326547844));
#58554=CARTESIAN_POINT('Ctrl Pts',(-16.3653318275832,-17.9772825547571,
-20.5835164497295));
#58555=CARTESIAN_POINT('Ctrl Pts',(-16.3346369396098,-18.0555176912515,
-20.5877002446745));
#58556=CARTESIAN_POINT('Ctrl Pts',(-16.3078887870756,-18.1349416284485,
-20.5918840396196));
#58557=CARTESIAN_POINT('Ctrl Pts',(-16.2883209175697,-18.1930449773331,
-20.5949447352478));
#58558=CARTESIAN_POINT('Ctrl Pts',(-16.2708642209569,-18.2517841874754,
-20.598005430876));
#58559=CARTESIAN_POINT('Ctrl Pts',(-16.2555511525118,-18.3109919576289,
-20.6010661265042));
#58560=CARTESIAN_POINT('Ctrl Pts',(-16.2346154345157,-18.3919396255347,
-20.6052506477694));
#58561=CARTESIAN_POINT('Ctrl Pts',(-16.2176106157921,-18.4740647181832,
-20.6094351690346));
#58562=CARTESIAN_POINT('Ctrl Pts',(-16.2046649096203,-18.5569506352696,
-20.6136196902999));
#58563=CARTESIAN_POINT('Ctrl Pts',(-16.1917376309692,-18.6397185686836,
-20.6177982551227));
#58564=CARTESIAN_POINT('Ctrl Pts',(-16.1828580584881,-18.7232447247143,
-20.6219768199456));
#58565=CARTESIAN_POINT('Ctrl Pts',(-16.1781041153418,-18.8070992519429,
-20.6261553847685));
#58566=CARTESIAN_POINT('Ctrl Pts',(-16.1732647978195,-18.8924596928359,
-20.6304089909525));
#58567=CARTESIAN_POINT('Ctrl Pts',(-16.1727008779273,-18.9781599489881,
-20.6346625971366));
#58568=CARTESIAN_POINT('Ctrl Pts',(-16.1764397017154,-19.0637377314903,
-20.6389162033206));
#58569=CARTESIAN_POINT('Ctrl Pts',(-16.1801059175876,-19.1476535944188,
-20.6430872045204));
#58570=CARTESIAN_POINT('Ctrl Pts',(-16.1879092316882,-19.2314512172152,
-20.6472582057202));
#58571=CARTESIAN_POINT('Ctrl Pts',(-16.1998229036826,-19.3146933201762,
-20.65142920692));
#58572=CARTESIAN_POINT('Ctrl Pts',(-16.2117325790265,-19.3979074981112,
-20.6555988088842));
#58573=CARTESIAN_POINT('Ctrl Pts',(-16.2277498086426,-19.480566071281,-20.6597684108483));
#58574=CARTESIAN_POINT('Ctrl Pts',(-16.2477960843791,-19.5622377323235,
-20.6639380128125));
#58575=CARTESIAN_POINT('Ctrl Pts',(-16.2678416494881,-19.6439064981584,
-20.668107466967));
#58576=CARTESIAN_POINT('Ctrl Pts',(-16.2919158662461,-19.7245879748307,
-20.6722769211214));
#58577=CARTESIAN_POINT('Ctrl Pts',(-16.3198895960846,-19.8038632271131,
-20.6764463752759));
#58578=CARTESIAN_POINT('Ctrl Pts',(-16.3488485215244,-19.8859304427944,
-20.6807626717684));
#58579=CARTESIAN_POINT('Ctrl Pts',(-16.3819865838887,-19.9664900366014,
-20.6850789682609));
#58580=CARTESIAN_POINT('Ctrl Pts',(-16.4191057518191,-20.0450986322098,
-20.6893952647533));
#58581=CARTESIAN_POINT('Ctrl Pts',(-16.4550137144482,-20.1211422148332,
-20.6935707196945));
#58582=CARTESIAN_POINT('Ctrl Pts',(-16.4946467067841,-20.1953597704704,
-20.6977461746357));
#58583=CARTESIAN_POINT('Ctrl Pts',(-16.5377789910434,-20.2673757181192,
-20.7019216295769));
#58584=CARTESIAN_POINT('Ctrl Pts',(-16.5830936067771,-20.3430354020531,
-20.7063083468451));
#58585=CARTESIAN_POINT('Ctrl Pts',(-16.6322706296986,-20.4162643312086,
-20.7106950641132));
#58586=CARTESIAN_POINT('Ctrl Pts',(-16.6849987382266,-20.4866640770054,
-20.7150817813813));
#58587=CARTESIAN_POINT('Ctrl Pts',(-16.7377268467545,-20.5570638228022,
-20.7194684986494));
#58588=CARTESIAN_POINT('Ctrl Pts',(-16.7940056108791,-20.6246339879283,
-20.7238552159176));
#58589=CARTESIAN_POINT('Ctrl Pts',(-16.8534788452301,-20.689020491089,-20.7282419331857));
#58590=CARTESIAN_POINT('Ctrl Pts',(-16.9102137581221,-20.7504424515406,
-20.7324266731751));
#58591=CARTESIAN_POINT('Ctrl Pts',(-16.9700666644563,-20.8091961438448,
-20.7366114131645));
#58592=CARTESIAN_POINT('Ctrl Pts',(-17.0327566307066,-20.8649482477149,
-20.740796153154));
#58593=CARTESIAN_POINT('Ctrl Pts',(-17.0953573578707,-20.9206209885368,
-20.7449749361714));
#58594=CARTESIAN_POINT('Ctrl Pts',(-17.1607867823076,-20.9733003248918,
-20.7491537191888));
#58595=CARTESIAN_POINT('Ctrl Pts',(-17.2287256089521,-21.0226880517488,
-20.7533325022063));
#58596=CARTESIAN_POINT('Ctrl Pts',(-17.297880025795,-21.0729594446868,-20.7575860537755));
#58597=CARTESIAN_POINT('Ctrl Pts',(-17.3696342017319,-21.1198199228446,
-20.7618396053447));
#58598=CARTESIAN_POINT('Ctrl Pts',(-17.443614263699,-21.1629963029256,-20.7660931569139));
#58599=CARTESIAN_POINT('Ctrl Pts',(-17.5161623107921,-21.2053369278474,
-20.7702643734735));
#58600=CARTESIAN_POINT('Ctrl Pts',(-17.5908504241594,-21.244134565952,-20.774435590033));
#58601=CARTESIAN_POINT('Ctrl Pts',(-17.6672964146049,-21.2791749957631,
-20.7786068065926));
#58602=CARTESIAN_POINT('Ctrl Pts',(-17.7437167334923,-21.3142036585421,
-20.7827766224034));
#58603=CARTESIAN_POINT('Ctrl Pts',(-17.8218933392511,-21.3454774273092,
-20.7869464382142));
#58604=CARTESIAN_POINT('Ctrl Pts',(-17.9014210435259,-21.3728288417888,
-20.791116254025));
#58605=CARTESIAN_POINT('Ctrl Pts',(-17.9809458947181,-21.4001792750274,
-20.7952859202423));
#58606=CARTESIAN_POINT('Ctrl Pts',(-18.0618213127757,-21.4236074849553,
-20.7994555864596));
#58607=CARTESIAN_POINT('Ctrl Pts',(-18.1436251063839,-21.4429952800011,
-20.8036252526769));
#58608=CARTESIAN_POINT('Ctrl Pts',(-18.2283005878212,-21.463063675452,-20.807941293276));
#58609=CARTESIAN_POINT('Ctrl Pts',(-18.3139703255072,-21.4788025798654,
-20.8122573338752));
#58610=CARTESIAN_POINT('Ctrl Pts',(-18.4001544397717,-21.490138519056,-20.8165733744744));
#58611=CARTESIAN_POINT('Ctrl Pts',(-18.483535397029,-21.501105754366,-20.8207490349171));
#58612=CARTESIAN_POINT('Ctrl Pts',(-18.5673973100676,-21.5079520575122,
-20.8249246953598));
#58613=CARTESIAN_POINT('Ctrl Pts',(-18.6513021513138,-21.5106639220153,
-20.8291003558025));
#58614=CARTESIAN_POINT('Ctrl Pts',(-18.7394381464964,-21.513512540441,-20.8334865864799));
#58615=CARTESIAN_POINT('Ctrl Pts',(-18.827620929765,-21.5117987866347,-20.8378728171574));
#58616=CARTESIAN_POINT('Ctrl Pts',(-18.9153471676247,-21.5055687194189,
-20.8422590478348));
#58617=CARTESIAN_POINT('Ctrl Pts',(-19.0030734054844,-21.499338652203,-20.8466452785123));
#58618=CARTESIAN_POINT('Ctrl Pts',(-19.0903425315942,-21.4885924178744,
-20.8510315091897));
#58619=CARTESIAN_POINT('Ctrl Pts',(-19.1766642018011,-21.4734377653323,
-20.8554177398671));
#58620=CARTESIAN_POINT('Ctrl Pts',(-19.2590223589629,-21.4589789480642,
-20.8596025740416));
#58621=CARTESIAN_POINT('Ctrl Pts',(-19.3408245084339,-21.4404538839632,
-20.8637874082161));
#58622=CARTESIAN_POINT('Ctrl Pts',(-19.4216382989709,-21.4179184029056,
-20.8679722423906));
#58623=CARTESIAN_POINT('Ctrl Pts',(-19.5023371028523,-21.3954149866674,
-20.8721511221348));
#58624=CARTESIAN_POINT('Ctrl Pts',(-19.5820499018622,-21.3689126104334,
-20.8763300018789));
#58625=CARTESIAN_POINT('Ctrl Pts',(-19.6603531104247,-21.338518366744,-20.8805088816231));
#58626=CARTESIAN_POINT('Ctrl Pts',(-19.7400550610479,-21.3075811860814,
-20.8847624093283));
#58627=CARTESIAN_POINT('Ctrl Pts',(-19.8182960912148,-21.2726118104529,
-20.8890159370335));
#58628=CARTESIAN_POINT('Ctrl Pts',(-19.8946441530214,-21.2337767528961,
-20.8932694647388));
#58629=CARTESIAN_POINT('Ctrl Pts',(-19.9695166174632,-21.195692269843,-20.8974407834904));
#58630=CARTESIAN_POINT('Ctrl Pts',(-20.0425682056166,-21.1538904198174,
-20.901612102242));
#58631=CARTESIAN_POINT('Ctrl Pts',(-20.1134119104384,-21.1085766347016,
-20.9057834209936));
#58632=CARTESIAN_POINT('Ctrl Pts',(-20.1842318561761,-21.0632780466174,
-20.9099533407964));
#58633=CARTESIAN_POINT('Ctrl Pts',(-20.2528450019901,-21.0144701102459,
-20.9141232605992));
#58634=CARTESIAN_POINT('Ctrl Pts',(-20.3188912127324,-20.9624029058384,
-20.9182931804021));
#58635=CARTESIAN_POINT('Ctrl Pts',(-20.3849350802549,-20.9103375486967,
-20.9224629522624));
#58636=CARTESIAN_POINT('Ctrl Pts',(-20.448411833077,-20.8550134388734,-20.9266327241228));
#58637=CARTESIAN_POINT('Ctrl Pts',(-20.5089935615136,-20.7967216203496,
-20.9308024959832));
#58638=CARTESIAN_POINT('Ctrl Pts',(-20.5716986579763,-20.7363866943274,
-20.9351184168636));
#58639=CARTESIAN_POINT('Ctrl Pts',(-20.6313016391124,-20.6728725241964,
-20.9394343377441));
#58640=CARTESIAN_POINT('Ctrl Pts',(-20.687481020985,-20.6065428071378,-20.9437502586245));
#58641=CARTESIAN_POINT('Ctrl Pts',(-20.7418360778663,-20.5423670290593,
-20.9479260276902));
#58642=CARTESIAN_POINT('Ctrl Pts',(-20.79298623453,-20.4755561680757,-20.9521017967558));
#58643=CARTESIAN_POINT('Ctrl Pts',(-20.8406830326348,-20.4064712441326,
-20.9562775658215));
#58644=CARTESIAN_POINT('Ctrl Pts',(-20.8907811103752,-20.333908262383,-20.9606635626093));
#58645=CARTESIAN_POINT('Ctrl Pts',(-20.9370686806316,-20.2588367305564,
-20.9650495593971));
#58646=CARTESIAN_POINT('Ctrl Pts',(-20.9793120741947,-20.1817047163753,
-20.969435556185));
#58647=CARTESIAN_POINT('Ctrl Pts',(-21.0215554677577,-20.1045727021941,
-20.9738215529728));
#58648=CARTESIAN_POINT('Ctrl Pts',(-21.0597545011784,-20.025380760798,-20.9782075497606));
#58649=CARTESIAN_POINT('Ctrl Pts',(-21.0937343889893,-19.9445994224366,
-20.9825935465485));
#58650=CARTESIAN_POINT('Ctrl Pts',(-21.1297844964522,-19.8588964929525,
-20.9872467595436));
#58651=CARTESIAN_POINT('Ctrl Pts',(-21.1612011352353,-19.7711341998165,
-20.9918999725387));
#58652=CARTESIAN_POINT('Ctrl Pts',(-21.187770405969,-19.6818018873577,-20.9965531855338));
#58653=CARTESIAN_POINT('Ctrl Pts',(-21.2142564631891,-19.5927493588517,
-21.0011918249184));
#58654=CARTESIAN_POINT('Ctrl Pts',(-21.2359253189815,-19.5021368713044,
-21.005830464303));
#58655=CARTESIAN_POINT('Ctrl Pts',(-21.2526114126831,-19.410471975046,-21.0104691036876));
#58656=CARTESIAN_POINT('Ctrl Pts',(-21.269207206213,-19.3193031419175,-21.0150826401368));
#58657=CARTESIAN_POINT('Ctrl Pts',(-21.2808739033347,-19.2270935185721,
-21.019696176586));
#58658=CARTESIAN_POINT('Ctrl Pts',(-21.2874964963647,-19.1343612981233,
-21.0243097130352));
#58659=CARTESIAN_POINT('Ctrl Pts',(-21.2917935126354,-19.074192742048,-21.0273031690875));
#58660=CARTESIAN_POINT('Ctrl Pts',(-21.2939679585382,-19.0138045492422,
-21.0302966251399));
#58661=CARTESIAN_POINT('Ctrl Pts',(-21.29399964838,-18.9533417503911,-21.0332900811922));
#58662=CARTESIAN_POINT('Ctrl Pts',(-21.2904839170199,-18.9533393312605,
-21.0332901097715));
#58663=CARTESIAN_POINT('Ctrl Pts',(-21.2880301337774,-18.4391275099938,
-21.0587831909243));
#58664=CARTESIAN_POINT('Ctrl Pts',(-20.8878308621683,-17.0663417376224,
-21.1266682076376));
#58665=CARTESIAN_POINT('Ctrl Pts',(-18.9689508313882,-16.0899930897032,
-21.2211093015402));
#58666=CARTESIAN_POINT('Ctrl Pts',(-17.6030345805997,-16.6008609759918,
-21.29005731429));
#58667=CARTESIAN_POINT('Ctrl Pts',(-17.1763092963129,-16.9243021577153,
-21.3166133914793));
#58668=CARTESIAN_POINT('',(-21.2964370555865,-18.950145562236,-20.9667098902285));
#58669=CARTESIAN_POINT('Ctrl Pts',(-21.2964370555865,-18.950145562236,-20.9667098902285));
#58670=CARTESIAN_POINT('Ctrl Pts',(-21.2973788539875,-18.8345295300019,
-20.9724759609645));
#58671=CARTESIAN_POINT('Ctrl Pts',(-21.2376962631739,-17.8698878407826,
-21.0206339672611));
#58672=CARTESIAN_POINT('Ctrl Pts',(-20.0126665202556,-16.2082458119612,
-21.1111839091181));
#58673=CARTESIAN_POINT('Ctrl Pts',(-17.9939164803171,-16.3361984191612,
-21.1999086069035));
#58674=CARTESIAN_POINT('Ctrl Pts',(-17.2346906331956,-16.8707090898308,
-21.2462413691284));
#58675=CARTESIAN_POINT('Ctrl Pts',(-17.1724222329607,-16.9192441176791,
-21.2501821957929));
#58676=CARTESIAN_POINT('Ctrl Pts',(-17.1739275304995,-16.9211547578705,
-20.4499991767296));
#58677=CARTESIAN_POINT('Ctrl Pts',(-17.0385457733845,-17.0229919684527,
-20.4584344097234));
#58678=CARTESIAN_POINT('Ctrl Pts',(-16.286220291287,-17.716545158234,-20.5092615782776));
#58679=CARTESIAN_POINT('Ctrl Pts',(-15.8255862213472,-19.7912991220784,
-20.6024806823924));
#58680=CARTESIAN_POINT('Ctrl Pts',(-17.8654474230527,-21.8518086612915,
-20.7296564890738));
#58681=CARTESIAN_POINT('Ctrl Pts',(-20.5735369035609,-21.279131873543,-20.8510662250192));
#58682=CARTESIAN_POINT('Ctrl Pts',(-21.2904547875037,-19.6845342581055,
-20.9300840254041));
#58683=CARTESIAN_POINT('Ctrl Pts',(-21.2964370555865,-18.950145562236,-20.9667098902285));
#58684=CARTESIAN_POINT('Origin',(-18.734,-18.952,1.76670989022851));
#58685=CARTESIAN_POINT('',(-17.1744641548914,-16.9218650419685,-19.6501081133027));
#58686=CARTESIAN_POINT('',(-17.1744641548914,-16.9218650419685,-19.7167245499181));
#58687=CARTESIAN_POINT('',(-17.1744641548914,-16.9218650419685,1.76670989022851));
#58688=CARTESIAN_POINT('',(-21.2939995273704,-18.9535555909848,-20.2332901098006));
#58689=CARTESIAN_POINT('Ctrl Pts',(-17.1744641548914,-16.9218650419685,
-19.7167245499181));
#58690=CARTESIAN_POINT('Ctrl Pts',(-17.1080939778308,-16.9728501598607,
-19.7209062184222));
#58691=CARTESIAN_POINT('Ctrl Pts',(-17.0441148850582,-17.027179288429,-19.7250878869263));
#58692=CARTESIAN_POINT('Ctrl Pts',(-16.9828821694244,-17.0845990405271,
-19.7292695554304));
#58693=CARTESIAN_POINT('Ctrl Pts',(-16.9217270963244,-17.141945984895,-19.7334459216164));
#58694=CARTESIAN_POINT('Ctrl Pts',(-16.8633118156132,-17.2023754551086,
-19.7376222878024));
#58695=CARTESIAN_POINT('Ctrl Pts',(-16.807959606527,-17.2655930494953,-19.7417986539884));
#58696=CARTESIAN_POINT('Ctrl Pts',(-16.7526597112601,-17.3287508964237,
-19.745971073057));
#58697=CARTESIAN_POINT('Ctrl Pts',(-16.7004174362064,-17.3946912859582,
-19.7501434921256));
#58698=CARTESIAN_POINT('Ctrl Pts',(-16.6515191818487,-17.4630830640927,
-19.7543159111942));
#58699=CARTESIAN_POINT('Ctrl Pts',(-16.602645405779,-17.5314406055519,-19.7584862415651));
#58700=CARTESIAN_POINT('Ctrl Pts',(-16.5571125936733,-17.6022467254762,
-19.7626565719359));
#58701=CARTESIAN_POINT('Ctrl Pts',(-16.5151660691643,-17.6751382269908,
-19.7668269023067));
#58702=CARTESIAN_POINT('Ctrl Pts',(-16.4732279599042,-17.7480151051215,
-19.7709963960321));
#58703=CARTESIAN_POINT('Ctrl Pts',(-16.4348749381907,-17.8229761350483,
-19.7751658897574));
#58704=CARTESIAN_POINT('Ctrl Pts',(-16.4003075630717,-17.8996314287172,
-19.7793353834828));
#58705=CARTESIAN_POINT('Ctrl Pts',(-16.3657367535408,-17.9762943384071,
-19.7835052914647));
#58706=CARTESIAN_POINT('Ctrl Pts',(-16.3349525253485,-18.054651426181,-19.7876751994465));
#58707=CARTESIAN_POINT('Ctrl Pts',(-16.3081076999676,-18.1342918927617,
-19.7918451074284));
#58708=CARTESIAN_POINT('Ctrl Pts',(-16.2812344036413,-18.2140168240145,
-19.7960194379095));
#58709=CARTESIAN_POINT('Ctrl Pts',(-16.2583089990828,-18.2950274148578,
-19.8001937683907));
#58710=CARTESIAN_POINT('Ctrl Pts',(-16.2394345486869,-18.3768972186511,
-19.8043680988719));
#58711=CARTESIAN_POINT('Ctrl Pts',(-16.2205494936018,-18.4588130213379,
-19.8085447747182));
#58712=CARTESIAN_POINT('Ctrl Pts',(-16.2057200054997,-18.5415885452313,
-19.8127214505646));
#58713=CARTESIAN_POINT('Ctrl Pts',(-16.1949976382843,-18.6247890478577,
-19.8168981264109));
#58714=CARTESIAN_POINT('Ctrl Pts',(-16.1842568801908,-18.708132255007,-19.8210819660424));
#58715=CARTESIAN_POINT('Ctrl Pts',(-16.177637347357,-18.7919014377924,-19.825265805674));
#58716=CARTESIAN_POINT('Ctrl Pts',(-16.1751385264366,-18.8756589290556,
-19.8294496453056));
#58717=CARTESIAN_POINT('Ctrl Pts',(-16.1734340309011,-18.9327915826007,
-19.8323035256756));
#58718=CARTESIAN_POINT('Ctrl Pts',(-16.1736457572909,-18.9899187852792,
-19.8351574060456));
#58719=CARTESIAN_POINT('Ctrl Pts',(-16.1757597065439,-19.0469031134252,
-19.8380112864157));
#58720=CARTESIAN_POINT('Ctrl Pts',(-16.1788593810972,-19.1304589848034,
-19.8421959187327));
#58721=CARTESIAN_POINT('Ctrl Pts',(-16.1860627143182,-19.2140183314082,
-19.8463805510498));
#58722=CARTESIAN_POINT('Ctrl Pts',(-16.1973733531442,-19.2971452657373,
-19.8505651833669));
#58723=CARTESIAN_POINT('Ctrl Pts',(-16.2086678926685,-19.3801538791111,
-19.8547438593752));
#58724=CARTESIAN_POINT('Ctrl Pts',(-16.224058063826,-19.462730850823,-19.8589225353834));
#58725=CARTESIAN_POINT('Ctrl Pts',(-16.2434955344908,-19.5444419864245,
-19.8631012113916));
#58726=CARTESIAN_POINT('Ctrl Pts',(-16.26328142009,-19.6276177868711,-19.867354789796));
#58727=CARTESIAN_POINT('Ctrl Pts',(-16.2872611153603,-19.7098959227523,
-19.8716083682004));
#58728=CARTESIAN_POINT('Ctrl Pts',(-16.3153285555786,-19.7908256338122,
-19.8758619466048));
#58729=CARTESIAN_POINT('Ctrl Pts',(-16.3428518367464,-19.8701863156202,
-19.8800330585225));
#58730=CARTESIAN_POINT('Ctrl Pts',(-16.3743056169175,-19.9482499366746,
-19.8842041704402));
#58731=CARTESIAN_POINT('Ctrl Pts',(-16.4095391526147,-20.0246051318974,
-19.8883752823579));
#58732=CARTESIAN_POINT('Ctrl Pts',(-16.4447608654386,-20.1009347055702,
-19.8925449946281));
#58733=CARTESIAN_POINT('Ctrl Pts',(-16.483759622288,-20.1755565745853,-19.8967147068984));
#58734=CARTESIAN_POINT('Ctrl Pts',(-16.526336784863,-20.2480799082353,-19.9008844191686));
#58735=CARTESIAN_POINT('Ctrl Pts',(-16.5689124324897,-20.3206006614147,
-19.9050539830753));
#58736=CARTESIAN_POINT('Ctrl Pts',(-16.6150659990477,-20.3910226314022,
-19.909223546982));
#58737=CARTESIAN_POINT('Ctrl Pts',(-16.6645538721764,-20.4589813283634,
-19.9133931108887));
#58738=CARTESIAN_POINT('Ctrl Pts',(-16.7157817319262,-20.5293294434996,
-19.9177092760727));
#58739=CARTESIAN_POINT('Ctrl Pts',(-16.7705824262632,-20.5970374134405,
-19.9220254412568));
#58740=CARTESIAN_POINT('Ctrl Pts',(-16.8286393907572,-20.6617370993067,
-19.9263416064408));
#58741=CARTESIAN_POINT('Ctrl Pts',(-16.8848050972204,-20.7243291344967,
-19.9305171686474));
#58742=CARTESIAN_POINT('Ctrl Pts',(-16.9440178143264,-20.7841055699944,
-19.934692730854));
#58743=CARTESIAN_POINT('Ctrl Pts',(-17.0059537742783,-20.8407710930044,
-19.9388682930607));
#58744=CARTESIAN_POINT('Ctrl Pts',(-17.0710180723843,-20.9002987484136,
-19.9432547597334));
#58745=CARTESIAN_POINT('Ctrl Pts',(-17.1390875037942,-20.9563925860382,
-19.9476412264061));
#58746=CARTESIAN_POINT('Ctrl Pts',(-17.2097498583892,-21.0087599533732,
-19.9520276930789));
#58747=CARTESIAN_POINT('Ctrl Pts',(-17.2804122129843,-21.0611273207081,
-19.9564141597516));
#58748=CARTESIAN_POINT('Ctrl Pts',(-17.3536669653183,-21.1097679601685,
-19.9608006264243));
#58749=CARTESIAN_POINT('Ctrl Pts',(-17.4290716122084,-21.1544445288669,
-19.965187093097));
#58750=CARTESIAN_POINT('Ctrl Pts',(-17.5010067187011,-21.1970654263791,
-19.969371728398));
#58751=CARTESIAN_POINT('Ctrl Pts',(-17.5751659818923,-21.2362376725991,
-19.9735563636989));
#58752=CARTESIAN_POINT('Ctrl Pts',(-17.6511848628854,-21.2717222632969,
-19.9777409989998));
#58753=CARTESIAN_POINT('Ctrl Pts',(-17.7270955401342,-21.307156345943,-19.9819196779751));
#58754=CARTESIAN_POINT('Ctrl Pts',(-17.8048601642347,-21.338913006185,-19.9860983569504));
#58755=CARTESIAN_POINT('Ctrl Pts',(-17.8840874846205,-21.3667978623896,
-19.9902770359257));
#58756=CARTESIAN_POINT('Ctrl Pts',(-17.9647348763175,-21.3951825270456,
-19.9945306135862));
#58757=CARTESIAN_POINT('Ctrl Pts',(-18.04689750213,-21.4195549745919,-19.9987841912467));
#58758=CARTESIAN_POINT('Ctrl Pts',(-18.1301389338576,-21.4397604010028,
-20.0030377689073));
#58759=CARTESIAN_POINT('Ctrl Pts',(-18.2117665888522,-21.4595741108567,
-20.0072088837303));
#58760=CARTESIAN_POINT('Ctrl Pts',(-18.2944311264172,-21.4753808138487,
-20.0113799985533));
#58761=CARTESIAN_POINT('Ctrl Pts',(-18.377705058588,-21.4870845971534,-20.0155511133763));
#58762=CARTESIAN_POINT('Ctrl Pts',(-18.460951047014,-21.4987844530881,-20.0197208285227));
#58763=CARTESIAN_POINT('Ctrl Pts',(-18.5448055687472,-21.5063840596946,
-20.0238905436692));
#58764=CARTESIAN_POINT('Ctrl Pts',(-18.6288324774108,-21.5098388909766,
-20.0280602588157));
#58765=CARTESIAN_POINT('Ctrl Pts',(-18.7128563956359,-21.5132935993045,
-20.0322298255659));
#58766=CARTESIAN_POINT('Ctrl Pts',(-18.7970522289138,-21.5126038075458,
-20.0363993923161));
#58767=CARTESIAN_POINT('Ctrl Pts',(-18.8809816357491,-21.507777063586,-20.0405689590664));
#58768=CARTESIAN_POINT('Ctrl Pts',(-18.9678618598034,-21.5027806194017,
-20.0448851207924));
#58769=CARTESIAN_POINT('Ctrl Pts',(-19.0544560474151,-21.4933509339532,
-20.0492012825184));
#58770=CARTESIAN_POINT('Ctrl Pts',(-19.1402833032843,-21.4795549207628,
-20.0535174442444));
#58771=CARTESIAN_POINT('Ctrl Pts',(-19.2233147796995,-21.466208305725,-20.057693009185));
#58772=CARTESIAN_POINT('Ctrl Pts',(-19.3056280710303,-21.4487756011034,
-20.0618685741256));
#58773=CARTESIAN_POINT('Ctrl Pts',(-19.3867996160279,-21.4273691969712,
-20.0660441390663));
#58774=CARTESIAN_POINT('Ctrl Pts',(-19.472070890686,-21.4048816199976,-20.070430599185));
#58775=CARTESIAN_POINT('Ctrl Pts',(-19.5560814940463,-21.3780085540522,
-20.0748170593037));
#58776=CARTESIAN_POINT('Ctrl Pts',(-19.6383622324208,-21.3469381938937,
-20.0792035194224));
#58777=CARTESIAN_POINT('Ctrl Pts',(-19.7206429707954,-21.3158678337352,
-20.0835899795411));
#58778=CARTESIAN_POINT('Ctrl Pts',(-19.8011933431874,-21.2806004817501,
-20.0879764396598));
#58779=CARTESIAN_POINT('Ctrl Pts',(-19.8795742651246,-21.2413797420009,
-20.0923628997785));
#58780=CARTESIAN_POINT('Ctrl Pts',(-19.9543489008138,-21.2039635384947,
-20.0965475399847));
#58781=CARTESIAN_POINT('Ctrl Pts',(-20.0274276531195,-21.162810473499,-20.100732180191));
#58782=CARTESIAN_POINT('Ctrl Pts',(-20.0984122388012,-21.11809769923,-20.1049168203972));
#58783=CARTESIAN_POINT('Ctrl Pts',(-20.1692957874189,-21.0734485676151,
-20.1090955043278));
#58784=CARTESIAN_POINT('Ctrl Pts',(-20.2380907042344,-21.0252500340151,
-20.1132741882584));
#58785=CARTESIAN_POINT('Ctrl Pts',(-20.3044217681325,-20.9737258642496,
-20.117452872189));
#58786=CARTESIAN_POINT('Ctrl Pts',(-20.371941651073,-20.9212782521244,-20.1217064486169));
#58787=CARTESIAN_POINT('Ctrl Pts',(-20.4369080609029,-20.865384834865,-20.1259600250449));
#58788=CARTESIAN_POINT('Ctrl Pts',(-20.4989546028882,-20.8063287868509,
-20.1302136014728));
#58789=CARTESIAN_POINT('Ctrl Pts',(-20.5597983582893,-20.7484175540028,
-20.1343847213367));
#58790=CARTESIAN_POINT('Ctrl Pts',(-20.6178340917841,-20.6874655447192,
-20.1385558412007));
#58791=CARTESIAN_POINT('Ctrl Pts',(-20.6727497644134,-20.6237802938745,
-20.1427269610646));
#58792=CARTESIAN_POINT('Ctrl Pts',(-20.7276470096087,-20.5601164131724,
-20.1468966812728));
#58793=CARTESIAN_POINT('Ctrl Pts',(-20.7794259730566,-20.4937214605129,
-20.151066401481));
#58794=CARTESIAN_POINT('Ctrl Pts',(-20.827813137392,-20.4249380658006,-20.1552361216892));
#58795=CARTESIAN_POINT('Ctrl Pts',(-20.8761985798384,-20.3561571187907,
-20.1594056935151));
#58796=CARTESIAN_POINT('Ctrl Pts',(-20.921192199164,-20.2849882754667,-20.1635752653411));
#58797=CARTESIAN_POINT('Ctrl Pts',(-20.9625630757428,-20.2118041980546,
-20.167744837167));
#58798=CARTESIAN_POINT('Ctrl Pts',(-21.0053883717902,-20.1360472878725,
-20.1720609929414));
#58799=CARTESIAN_POINT('Ctrl Pts',(-21.044331197893,-20.0581312678785,-20.1763771487158));
#58800=CARTESIAN_POINT('Ctrl Pts',(-21.0791875194638,-19.9784967114177,
-20.1806933044902));
#58801=CARTESIAN_POINT('Ctrl Pts',(-21.1129085013345,-19.9014560108021,
-20.184868874489));
#58802=CARTESIAN_POINT('Ctrl Pts',(-21.1428049796707,-19.8228074643854,
-20.1890444444878));
#58803=CARTESIAN_POINT('Ctrl Pts',(-21.1687421906793,-19.7429680555664,
-20.1932200144866));
#58804=CARTESIAN_POINT('Ctrl Pts',(-21.1959893077345,-19.6590965199184,
-20.1976064631488));
#58805=CARTESIAN_POINT('Ctrl Pts',(-21.2188665683597,-19.5739112349382,
-20.201992911811));
#58806=CARTESIAN_POINT('Ctrl Pts',(-21.2372782494394,-19.4879085797817,
-20.2063793604732));
#58807=CARTESIAN_POINT('Ctrl Pts',(-21.2556899305191,-19.4019059246253,
-20.2107658091355));
#58808=CARTESIAN_POINT('Ctrl Pts',(-21.2696360151318,-19.3150864842148,
-20.2151522577977));
#58809=CARTESIAN_POINT('Ctrl Pts',(-21.2790836671994,-19.2279513126528,
-20.2195387064599));
#58810=CARTESIAN_POINT('Ctrl Pts',(-21.2889563823072,-19.136895808223,-20.2241225075637));
#58811=CARTESIAN_POINT('Ctrl Pts',(-21.2939437779019,-19.0453011468624,
-20.2287063086676));
#58812=CARTESIAN_POINT('Ctrl Pts',(-21.2939995273701,-18.9535555915677,
-20.2332901097715));
#58813=CARTESIAN_POINT('Ctrl Pts',(-21.2939995273704,-18.9535555909848,
-20.2332901098006));
#58814=CARTESIAN_POINT('Ctrl Pts',(-21.294049723898,-18.870948345104,-20.2374173417263));
#58815=CARTESIAN_POINT('Ctrl Pts',(-21.2900972917066,-18.7881812203374,
-20.241544573652));
#58816=CARTESIAN_POINT('Ctrl Pts',(-21.2821221997477,-18.7056805830778,
-20.2456718055777));
#58817=CARTESIAN_POINT('Ctrl Pts',(-21.2739869562085,-18.6215232116386,
-20.2498819183928));
#58818=CARTESIAN_POINT('Ctrl Pts',(-21.2616656480612,-18.537643639815,-20.254092031208));
#58819=CARTESIAN_POINT('Ctrl Pts',(-21.2451929664636,-18.4544963465625,
-20.2583021440231));
#58820=CARTESIAN_POINT('Ctrl Pts',(-21.229080068103,-18.3731650904946,-20.2624203028958));
#58821=CARTESIAN_POINT('Ctrl Pts',(-21.2089953895162,-18.2925349412607,
-20.2665384617684));
#58822=CARTESIAN_POINT('Ctrl Pts',(-21.1850236976428,-18.2130258234598,
-20.270656620641));
#58823=CARTESIAN_POINT('Ctrl Pts',(-21.1610629749352,-18.1335530881012,
-20.2747728950923));
#58824=CARTESIAN_POINT('Ctrl Pts',(-21.1332189046361,-18.055200818656,-20.2788891695437));
#58825=CARTESIAN_POINT('Ctrl Pts',(-21.1016267121137,-17.9783759698499,
-20.283005443995));
#58826=CARTESIAN_POINT('Ctrl Pts',(-21.0700389130291,-17.9015618048605,
-20.2871211460075));
#58827=CARTESIAN_POINT('Ctrl Pts',(-21.0347042074052,-17.8262750760015,
-20.2912368480201));
#58828=CARTESIAN_POINT('Ctrl Pts',(-20.9958062193322,-17.752903412485,-20.2953525500326));
#58829=CARTESIAN_POINT('Ctrl Pts',(-20.9553538853537,-17.6765998506772,
-20.299632713625));
#58830=CARTESIAN_POINT('Ctrl Pts',(-20.9110477424172,-17.6023681210458,
-20.3039128772174));
#58831=CARTESIAN_POINT('Ctrl Pts',(-20.8631463424907,-17.5306148121433,
-20.3081930408098));
#58832=CARTESIAN_POINT('Ctrl Pts',(-20.817026382064,-17.4615299884816,-20.3123140263301));
#58833=CARTESIAN_POINT('Ctrl Pts',(-20.767574190865,-17.394742855338,-20.3164350118505));
#58834=CARTESIAN_POINT('Ctrl Pts',(-20.7150628530422,-17.3305839607626,
-20.3205559973708));
#58835=CARTESIAN_POINT('Ctrl Pts',(-20.6625158707606,-17.2663815154195,
-20.3246797801975));
#58836=CARTESIAN_POINT('Ctrl Pts',(-20.6069059305284,-17.204811205117,-20.3288035630242));
#58837=CARTESIAN_POINT('Ctrl Pts',(-20.5485433980296,-17.1461671570527,
-20.3329273458509));
#58838=CARTESIAN_POINT('Ctrl Pts',(-20.4900913111083,-17.0874331225942,
-20.3370574564186));
#58839=CARTESIAN_POINT('Ctrl Pts',(-20.4288785613994,-17.031634616857,-20.3411875669862));
#58840=CARTESIAN_POINT('Ctrl Pts',(-20.3652483132487,-16.9790253573542,
-20.3453176775539));
#58841=CARTESIAN_POINT('Ctrl Pts',(-20.3580748979454,-16.9730944034733,
-20.3457832894164));
#58842=CARTESIAN_POINT('Ctrl Pts',(-20.3508707868094,-16.9672039368768,
-20.3462489012788));
#58843=CARTESIAN_POINT('Ctrl Pts',(-20.3436364930174,-16.961354285578,-20.3467145131413));
#58844=CARTESIAN_POINT('Ctrl Pts',(-20.2786189220457,-16.9087810656599,
-20.3508991582751));
#58845=CARTESIAN_POINT('Ctrl Pts',(-20.2109019646558,-16.8592987216113,
-20.3550838034089));
#58846=CARTESIAN_POINT('Ctrl Pts',(-20.1408117772448,-16.813196450488,-20.3592684485427));
#58847=CARTESIAN_POINT('Ctrl Pts',(-20.0708213560678,-16.7671598012461,
-20.3634471372609));
#58848=CARTESIAN_POINT('Ctrl Pts',(-19.9984647957972,-16.724493919034,-20.3676258259791));
#58849=CARTESIAN_POINT('Ctrl Pts',(-19.9241011351325,-16.6854477089297,
-20.3718045146973));
#58850=CARTESIAN_POINT('Ctrl Pts',(-19.8484047994816,-16.6457017496864,
-20.3760580899108));
#58851=CARTESIAN_POINT('Ctrl Pts',(-19.7706290892635,-16.6097067834814,
-20.3803116651244));
#58852=CARTESIAN_POINT('Ctrl Pts',(-19.6911834645766,-16.5776790833712,
-20.384565240338));
#58853=CARTESIAN_POINT('Ctrl Pts',(-19.6132778070226,-16.5462722054359,
-20.3887363646167));
#58854=CARTESIAN_POINT('Ctrl Pts',(-19.5337668426417,-16.5186803435126,
-20.3929074888954));
#58855=CARTESIAN_POINT('Ctrl Pts',(-19.4530597028474,-16.4950602075466,
-20.3970786131741));
#58856=CARTESIAN_POINT('Ctrl Pts',(-19.3723796478629,-16.47144799835,-20.4012483376496));
#58857=CARTESIAN_POINT('Ctrl Pts',(-19.2905046558528,-16.4518049970839,
-20.4054180621252));
#58858=CARTESIAN_POINT('Ctrl Pts',(-19.2078598549769,-16.4362383185522,
-20.4095877866007));
#58859=CARTESIAN_POINT('Ctrl Pts',(-19.1252179980804,-16.4206721945378,
-20.4137573625421));
#58860=CARTESIAN_POINT('Ctrl Pts',(-19.0418068390792,-16.4091821888638,
-20.4179269384834));
#58861=CARTESIAN_POINT('Ctrl Pts',(-18.9580612068526,-16.4018242069254,
-20.4220965144247));
#58862=CARTESIAN_POINT('Ctrl Pts',(-18.8713716361879,-16.3942075673677,
-20.4264126648745));
#58863=CARTESIAN_POINT('Ctrl Pts',(-18.7843241636749,-16.3910189213341,
-20.4307288153244));
#58864=CARTESIAN_POINT('Ctrl Pts',(-18.6974043010312,-16.3922615846894,
-20.4350449657742));
#58865=CARTESIAN_POINT('Ctrl Pts',(-18.613315412911,-16.3934637745764,-20.4392205394722));
#58866=CARTESIAN_POINT('Ctrl Pts',(-18.5293464168604,-16.3988129730352,
-20.4433961131702));
#58867=CARTESIAN_POINT('Ctrl Pts',(-18.4459326746173,-16.4082592081647,
-20.4475716868682));
#58868=CARTESIAN_POINT('Ctrl Pts',(-18.3583065652387,-16.4181824751278,
-20.4519581256939));
#58869=CARTESIAN_POINT('Ctrl Pts',(-18.2712938422192,-16.432627374356,-20.4563445645197));
#58870=CARTESIAN_POINT('Ctrl Pts',(-18.1853859701636,-16.4514755257613,
-20.4607310033455));
#58871=CARTESIAN_POINT('Ctrl Pts',(-18.099478098108,-16.4703236771666,-20.4651174421712));
#58872=CARTESIAN_POINT('Ctrl Pts',(-18.0146756164478,-16.4935748539843,
-20.469503880997));
#58873=CARTESIAN_POINT('Ctrl Pts',(-17.9314482086937,-16.5210514974045,
-20.4738903198228));
#58874=CARTESIAN_POINT('Ctrl Pts',(-17.852064997737,-16.547259020141,-20.4780741531062));
#58875=CARTESIAN_POINT('Ctrl Pts',(-17.7738191753082,-16.5774078021578,
-20.4822579863897));
#58876=CARTESIAN_POINT('Ctrl Pts',(-17.6971302056129,-16.6113802039871,
-20.4864418196731));
#58877=CARTESIAN_POINT('Ctrl Pts',(-17.6205369308216,-16.6453102139868,
-20.490620432238));
#58878=CARTESIAN_POINT('Ctrl Pts',(-17.545497070241,-16.6830541908193,-20.4947990448029));
#58879=CARTESIAN_POINT('Ctrl Pts',(-17.4724142317339,-16.7244449839996,
-20.4989776573678));
#58880=CARTESIAN_POINT('Ctrl Pts',(-17.3994143757936,-16.7657887796313,
-20.5031515252895));
#58881=CARTESIAN_POINT('Ctrl Pts',(-17.3283675238019,-16.8107709366666,
-20.5073253932112));
#58882=CARTESIAN_POINT('Ctrl Pts',(-17.2596551356225,-16.85917721226,-20.5114992611328));
#58883=CARTESIAN_POINT('Ctrl Pts',(-17.2308389306407,-16.879477556883,-20.5132496737845));
#58884=CARTESIAN_POINT('Ctrl Pts',(-17.2024330111304,-16.9003795571347,
-20.5150000864362));
#58885=CARTESIAN_POINT('Ctrl Pts',(-17.1744641548914,-16.9218650419685,
-20.5167504990879));
#58886=CARTESIAN_POINT('',(-21.2937660523048,-18.9509923322678,-20.1667099325986));
#58887=CARTESIAN_POINT('Ctrl Pts',(-21.2901593135592,-18.9509805599729,
-20.1667105863666));
#58888=CARTESIAN_POINT('Ctrl Pts',(-21.2914430747328,-18.5861666271369,
-20.1847914783605));
#58889=CARTESIAN_POINT('Ctrl Pts',(-21.0477247281039,-17.3676608534593,
-20.2452643059147));
#58890=CARTESIAN_POINT('Ctrl Pts',(-19.3278236160818,-16.0727555198283,
-20.3396938360357));
#58891=CARTESIAN_POINT('Ctrl Pts',(-17.7189175814815,-16.5112009519086,
-20.4160424741629));
#58892=CARTESIAN_POINT('Ctrl Pts',(-17.1739275304995,-16.9211547578705,
-20.4499991767296));
#58893=CARTESIAN_POINT('Ctrl Pts',(-17.1744641548914,-16.9218650419685,
-19.6501081133027));
#58894=CARTESIAN_POINT('Ctrl Pts',(-17.1077737209788,-16.9730961789927,
-19.6542777804462));
#58895=CARTESIAN_POINT('Ctrl Pts',(-17.0436133363582,-17.0276146696201,
-19.6584474475896));
#58896=CARTESIAN_POINT('Ctrl Pts',(-16.9823134737079,-17.0851324863272,
-19.6626171147331));
#58897=CARTESIAN_POINT('Ctrl Pts',(-16.9209516901765,-17.1427084035543,
-19.6667909937859));
#58898=CARTESIAN_POINT('Ctrl Pts',(-16.862456536847,-17.2032893833971,-19.6709648728387));
#58899=CARTESIAN_POINT('Ctrl Pts',(-16.8071223186683,-17.2665497927302,
-19.6751387518915));
#58900=CARTESIAN_POINT('Ctrl Pts',(-16.7517611351814,-17.3298410299397,
-19.6793146649467));
#58901=CARTESIAN_POINT('Ctrl Pts',(-16.6995642411243,-17.3958139365116,
-19.6834905780019));
#58902=CARTESIAN_POINT('Ctrl Pts',(-16.6507846855712,-17.4641109067779,
-19.6876664910572));
#58903=CARTESIAN_POINT('Ctrl Pts',(-16.6019171798243,-17.5325310173988,
-19.6918499333398));
#58904=CARTESIAN_POINT('Ctrl Pts',(-16.5564795739258,-17.6032831769332,
-19.6960333756223));
#58905=CARTESIAN_POINT('Ctrl Pts',(-16.5146806856349,-17.6759820609075,
-19.7002168179049));
#58906=CARTESIAN_POINT('Ctrl Pts',(-16.4746040303209,-17.7456855442744,
-19.7042278904774));
#58907=CARTESIAN_POINT('Ctrl Pts',(-16.4378722519963,-17.817178139003,-19.7082389630498));
#58908=CARTESIAN_POINT('Ctrl Pts',(-16.4046276535563,-17.8901033611394,
-19.7122500356223));
#58909=CARTESIAN_POINT('Ctrl Pts',(-16.3699445411289,-17.9661841019766,
-19.7164346697438));
#58910=CARTESIAN_POINT('Ctrl Pts',(-16.3389281684892,-18.0441074153348,
-19.7206193038652));
#58911=CARTESIAN_POINT('Ctrl Pts',(-16.3117771822314,-18.1234852921757,
-19.7248039379867));
#58912=CARTESIAN_POINT('Ctrl Pts',(-16.2846648420429,-18.2027501844311,
-19.7289826157992));
#58913=CARTESIAN_POINT('Ctrl Pts',(-16.2614071073441,-18.2834650961696,
-19.7331612936118));
#58914=CARTESIAN_POINT('Ctrl Pts',(-16.2421554012958,-18.3652202321922,
-19.7373399714244));
#58915=CARTESIAN_POINT('Ctrl Pts',(-16.2225586206672,-18.4484407770037,
-19.7415935493777));
#58916=CARTESIAN_POINT('Ctrl Pts',(-16.207113098083,-18.5327387664133,-19.745847127331));
#58917=CARTESIAN_POINT('Ctrl Pts',(-16.1959260745188,-18.617663719001,-19.7501007052843));
#58918=CARTESIAN_POINT('Ctrl Pts',(-16.1849559341181,-18.7009422289687,
-19.7542718189934));
#58919=CARTESIAN_POINT('Ctrl Pts',(-16.1780807097886,-18.7848231320472,
-19.7584429327025));
#58920=CARTESIAN_POINT('Ctrl Pts',(-16.1753500450965,-18.8688711345423,
-19.7626140464116));
#58921=CARTESIAN_POINT('Ctrl Pts',(-16.1726202967043,-18.9528909339471,
-19.7667837604647));
#58922=CARTESIAN_POINT('Ctrl Pts',(-16.1740323608325,-19.0370772620014,
-19.7709534745177));
#58923=CARTESIAN_POINT('Ctrl Pts',(-16.1795838629395,-19.1209917120005,
-19.7751231885707));
#58924=CARTESIAN_POINT('Ctrl Pts',(-16.1851351675026,-19.2049031760004,
-19.7792927542493));
#58925=CARTESIAN_POINT('Ctrl Pts',(-16.1948255859618,-19.2885423222071,
-19.7834623199278));
#58926=CARTESIAN_POINT('Ctrl Pts',(-16.2086007337952,-19.3714741306116,
-19.7876318856064));
#58927=CARTESIAN_POINT('Ctrl Pts',(-16.2228602007955,-19.457321730907,-19.7919480486645));
#58928=CARTESIAN_POINT('Ctrl Pts',(-16.2414968944622,-19.5424108074415,
-19.7962642117226));
#58929=CARTESIAN_POINT('Ctrl Pts',(-16.26439285385,-19.6262703787688,-19.8005803747807));
#58930=CARTESIAN_POINT('Ctrl Pts',(-16.2865429767612,-19.7073982223639,
-19.8047559387142));
#58931=CARTESIAN_POINT('Ctrl Pts',(-16.3126789433259,-19.7873750001408,
-19.8089315026477));
#58932=CARTESIAN_POINT('Ctrl Pts',(-16.34264370885,-19.8657916002993,-19.8131070665811));
#58933=CARTESIAN_POINT('Ctrl Pts',(-16.3741219297554,-19.9481688530246,
-19.8174935292016));
#58934=CARTESIAN_POINT('Ctrl Pts',(-16.4098256651424,-20.0288236423437,
-19.821879991822));
#58935=CARTESIAN_POINT('Ctrl Pts',(-16.4495176194985,-20.1073095919183,
-19.8262664544424));
#58936=CARTESIAN_POINT('Ctrl Pts',(-16.4892095738547,-20.1857955414929,
-19.8306529170629));
#58937=CARTESIAN_POINT('Ctrl Pts',(-16.532889392945,-20.2621121855376,-19.8350393796833));
#58938=CARTESIAN_POINT('Ctrl Pts',(-16.5802679097415,-20.3358490103298,
-19.8394258423038));
#58939=CARTESIAN_POINT('Ctrl Pts',(-16.62546646493,-20.4061930854538,-19.8436104767381));
#58940=CARTESIAN_POINT('Ctrl Pts',(-16.6741990691197,-20.4744513619179,
-19.8477951111724));
#58941=CARTESIAN_POINT('Ctrl Pts',(-16.7262469917103,-20.5402467874054,
-19.8519797456066));
#58942=CARTESIAN_POINT('Ctrl Pts',(-16.7782208304952,-20.6059485612105,
-19.8561584237293));
#58943=CARTESIAN_POINT('Ctrl Pts',(-16.8335003313994,-20.6691940894861,
-19.860337101852));
#58944=CARTESIAN_POINT('Ctrl Pts',(-16.8918228839615,-20.7296342349157,
-19.8645157799747));
#58945=CARTESIAN_POINT('Ctrl Pts',(-16.9511908256725,-20.7911577257993,
-19.8687693578502));
#58946=CARTESIAN_POINT('Ctrl Pts',(-17.0137117247795,-20.849773866074,-19.8730229357256));
#58947=CARTESIAN_POINT('Ctrl Pts',(-17.0790648452578,-20.9051486460581,
-19.877276513601));
#58948=CARTESIAN_POINT('Ctrl Pts',(-17.1431509686188,-20.9594498784273,
-19.8814476276115));
#58949=CARTESIAN_POINT('Ctrl Pts',(-17.2099601099664,-21.0106339979947,
-19.8856187416219));
#58950=CARTESIAN_POINT('Ctrl Pts',(-17.2791531272801,-21.0584236461208,
-19.8897898556323));
#58951=CARTESIAN_POINT('Ctrl Pts',(-17.3483229261688,-21.1061972579417,
-19.8939595699827));
#58952=CARTESIAN_POINT('Ctrl Pts',(-17.4198746341319,-21.150578399273,-19.8981292843331));
#58953=CARTESIAN_POINT('Ctrl Pts',(-17.4934383351829,-21.1913317654573,
-19.9022989986835));
#58954=CARTESIAN_POINT('Ctrl Pts',(-17.5669994184791,-21.2320836814384,
-19.9064685646552));
#58955=CARTESIAN_POINT('Ctrl Pts',(-17.6425719496892,-21.2692078567604,
-19.9106381306269));
#58956=CARTESIAN_POINT('Ctrl Pts',(-17.7197607084836,-21.302514552081,-19.9148076965986));
#58957=CARTESIAN_POINT('Ctrl Pts',(-17.7996633275439,-21.3369922691724,
-19.9191238592974));
#58958=CARTESIAN_POINT('Ctrl Pts',(-17.8812974576163,-21.367378857563,-19.9234400219963));
#58959=CARTESIAN_POINT('Ctrl Pts',(-17.9642032279854,-21.3935185704385,
-19.9277561846952));
#58960=CARTESIAN_POINT('Ctrl Pts',(-18.0444083527598,-21.4188067852806,
-19.9319317489083));
#58961=CARTESIAN_POINT('Ctrl Pts',(-18.1258030751317,-21.4401204858059,
-19.9361073131214));
#58962=CARTESIAN_POINT('Ctrl Pts',(-18.2079583914654,-21.4573702772425,
-19.9402828773344));
#58963=CARTESIAN_POINT('Ctrl Pts',(-18.2942631756871,-21.475491314252,-19.9446693392762));
#58964=CARTESIAN_POINT('Ctrl Pts',(-18.38140683144,-21.4891270269169,-19.949055801218));
#58965=CARTESIAN_POINT('Ctrl Pts',(-18.4688855835814,-21.498235328128,-19.9534422631598));
#58966=CARTESIAN_POINT('Ctrl Pts',(-18.5563643357229,-21.5073436293391,
-19.9578287251016));
#58967=CARTESIAN_POINT('Ctrl Pts',(-18.6441776008613,-21.5119245648311,
-19.9622151870434));
#58968=CARTESIAN_POINT('Ctrl Pts',(-18.7318236815561,-21.5119990749291,
-19.9666016489852));
#58969=CARTESIAN_POINT('Ctrl Pts',(-18.8154370559313,-21.5120701567239,
-19.9707862843005));
#58970=CARTESIAN_POINT('Ctrl Pts',(-18.8992095169516,-21.508040657495,-19.9749709196158));
#58971=CARTESIAN_POINT('Ctrl Pts',(-18.9827056283928,-21.4998904039236,
-19.9791555549311));
#58972=CARTESIAN_POINT('Ctrl Pts',(-19.0660828935662,-21.4917517512183,
-19.9833342339415));
#58973=CARTESIAN_POINT('Ctrl Pts',(-19.149184136535,-21.4795040389676,-19.987512912952));
#58974=CARTESIAN_POINT('Ctrl Pts',(-19.2315736418543,-21.4631790997322,
-19.9916915919625));
#58975=CARTESIAN_POINT('Ctrl Pts',(-19.3154398966918,-21.446561552281,-19.9959451696169));
#58976=CARTESIAN_POINT('Ctrl Pts',(-19.3985681653821,-21.4257191734759,
-20.0001987472712));
#58977=CARTESIAN_POINT('Ctrl Pts',(-19.4805039905309,-21.400740858507,-20.0044523249255));
#58978=CARTESIAN_POINT('Ctrl Pts',(-19.560851352111,-21.3762467901208,-20.0086234398338));
#58979=CARTESIAN_POINT('Ctrl Pts',(-19.6400516322992,-21.3477758589918,
-20.0127945547421));
#58980=CARTESIAN_POINT('Ctrl Pts',(-19.7176880451009,-21.315463101029,-20.0169656696504));
#58981=CARTESIAN_POINT('Ctrl Pts',(-19.7952984062491,-21.2831611859264,
-20.0211353849005));
#58982=CARTESIAN_POINT('Ctrl Pts',(-19.8713455178527,-21.247020180909,-20.0253051001507));
#58983=CARTESIAN_POINT('Ctrl Pts',(-19.9454312973038,-21.207223760941,-20.0294748154008));
#58984=CARTESIAN_POINT('Ctrl Pts',(-20.0195144404333,-21.1674287571174,
-20.0336443822728));
#58985=CARTESIAN_POINT('Ctrl Pts',(-20.0916359853166,-21.1239788154148,
-20.0378139491447));
#58986=CARTESIAN_POINT('Ctrl Pts',(-20.1614224658083,-21.0771035513842,
-20.0419835160167));
#58987=CARTESIAN_POINT('Ctrl Pts',(-20.2336625183512,-21.0285802340787,
-20.0462996776542));
#58988=CARTESIAN_POINT('Ctrl Pts',(-20.3033998142158,-20.9763865417844,
-20.0506158392917));
#58989=CARTESIAN_POINT('Ctrl Pts',(-20.3702544760718,-20.9208248498876,
-20.0549320009292));
#58990=CARTESIAN_POINT('Ctrl Pts',(-20.4349313850112,-20.8670730487782,
-20.0591075660348));
#58991=CARTESIAN_POINT('Ctrl Pts',(-20.4969102618753,-20.8101696539258,
-20.0632831311405));
#58992=CARTESIAN_POINT('Ctrl Pts',(-20.555883728143,-20.7504270018902,-20.0674586962461));
#58993=CARTESIAN_POINT('Ctrl Pts',(-20.6178357606472,-20.6876669344389,
-20.0718451561495));
#58994=CARTESIAN_POINT('Ctrl Pts',(-20.6764704135552,-20.6217736908107,
-20.0762316160529));
#58995=CARTESIAN_POINT('Ctrl Pts',(-20.7314796147868,-20.5531480845041,
-20.0806180759564));
#58996=CARTESIAN_POINT('Ctrl Pts',(-20.7864888160183,-20.4845224781975,
-20.0850045358598));
#58997=CARTESIAN_POINT('Ctrl Pts',(-20.8378722882511,-20.4131650245059,
-20.0893909957632));
#58998=CARTESIAN_POINT('Ctrl Pts',(-20.8853760799667,-20.3395089053938,
-20.0937774556666));
#58999=CARTESIAN_POINT('Ctrl Pts',(-20.93172083375,-20.2676499109516,-20.0980568909888));
#59000=CARTESIAN_POINT('Ctrl Pts',(-20.9745398784111,-20.1933453659579,
-20.1023363263109));
#59001=CARTESIAN_POINT('Ctrl Pts',(-21.0135728621542,-20.1169667661055,
-20.1066157616331));
#59002=CARTESIAN_POINT('Ctrl Pts',(-21.0525424988234,-20.0407121219527,
-20.1108882518109));
#59003=CARTESIAN_POINT('Ctrl Pts',(-21.0877380945303,-19.9623904961899,
-20.1151607419887));
#59004=CARTESIAN_POINT('Ctrl Pts',(-21.1189429603293,-19.8824015670536,
-20.1194332321666));
#59005=CARTESIAN_POINT('Ctrl Pts',(-21.1500944336146,-19.8025495015083,
-20.1236984119784));
#59006=CARTESIAN_POINT('Ctrl Pts',(-21.1772686126578,-19.7210362114978,
-20.1279635917902));
#59007=CARTESIAN_POINT('Ctrl Pts',(-21.2002957121622,-19.6382838043918,
-20.132228771602));
#59008=CARTESIAN_POINT('Ctrl Pts',(-21.2232995983466,-19.5556148189128,
-20.1364896517415));
#59009=CARTESIAN_POINT('Ctrl Pts',(-21.242164599727,-19.4717096138904,-20.1407505318809));
#59010=CARTESIAN_POINT('Ctrl Pts',(-21.2567699769455,-19.3870076360505,
-20.1450114120204));
#59011=CARTESIAN_POINT('Ctrl Pts',(-21.2713627640963,-19.3023786726647,
-20.1492686192133));
#59012=CARTESIAN_POINT('Ctrl Pts',(-21.2817031592285,-19.2169547278876,
-20.1535258264062));
#59013=CARTESIAN_POINT('Ctrl Pts',(-21.2877212407691,-19.1311865632376,
-20.1577830335991));
#59014=CARTESIAN_POINT('Ctrl Pts',(-21.2919276409326,-19.0712380199392,
-20.1607586524755));
#59015=CARTESIAN_POINT('Ctrl Pts',(-21.2940234518483,-19.0111215769093,
-20.163734271352));
#59016=CARTESIAN_POINT('Ctrl Pts',(-21.293999801981,-18.9509930952203,-20.1667098902285));
#59017=CARTESIAN_POINT('Origin',(-18.734,-18.952,1.76670989022851));
#59018=CARTESIAN_POINT('',(-17.1744641548914,-16.9218650419685,-18.8501886385061));
#59019=CARTESIAN_POINT('',(-17.1746506085037,-16.9221163620956,-18.9165758982197));
#59020=CARTESIAN_POINT('',(-17.1744641548914,-16.9218650419685,1.76670989022851));
#59021=CARTESIAN_POINT('',(-21.2939990581247,-18.9498040034555,-19.4332901097715));
#59022=CARTESIAN_POINT('Ctrl Pts',(-17.1746506085039,-16.9221163620955,
-18.9165758982197));
#59023=CARTESIAN_POINT('Ctrl Pts',(-17.0075187310044,-17.0478570694681,
-18.926977478695));
#59024=CARTESIAN_POINT('Ctrl Pts',(-16.2393387966466,-17.7870024615573,
-18.9797709947307));
#59025=CARTESIAN_POINT('Ctrl Pts',(-15.867552077141,-19.9250196648857,-19.074956446327));
#59026=CARTESIAN_POINT('Ctrl Pts',(-18.0006016646393,-21.8889061712022,
-19.2021322530084));
#59027=CARTESIAN_POINT('Ctrl Pts',(-20.6359183918341,-21.202775782827,-19.3215765970986));
#59028=CARTESIAN_POINT('Ctrl Pts',(-21.2889868109407,-19.6455867711505,
-19.3986290056282));
#59029=CARTESIAN_POINT('Ctrl Pts',(-21.2953147898194,-18.9498155448408,
-19.4332894785973));
#59030=CARTESIAN_POINT('Ctrl Pts',(-21.2939990581247,-18.9498040034555,
-19.4332901097715));
#59031=CARTESIAN_POINT('Ctrl Pts',(-21.2938905873826,-18.8233534412897,
-19.4395926510315));
#59032=CARTESIAN_POINT('Ctrl Pts',(-21.2844099378408,-18.6972910724131,
-19.4458951922915));
#59033=CARTESIAN_POINT('Ctrl Pts',(-21.2657470116111,-18.5727150554023,
-19.4521977335515));
#59034=CARTESIAN_POINT('Ctrl Pts',(-21.2615163488077,-18.544475158032,-19.4536264444915));
#59035=CARTESIAN_POINT('Ctrl Pts',(-21.25681399964,-18.5163115073431,-19.4550551554314));
#59036=CARTESIAN_POINT('Ctrl Pts',(-21.2516424693647,-18.4882367021301,
-19.4564838663713));
#59037=CARTESIAN_POINT('Ctrl Pts',(-21.2364952751732,-18.4060067810402,
-19.4606685004929));
#59038=CARTESIAN_POINT('Ctrl Pts',(-21.2172870302558,-18.3243667083798,
-19.4648531346144));
#59039=CARTESIAN_POINT('Ctrl Pts',(-21.1940771445919,-18.2437483196936,
-19.469037768736));
#59040=CARTESIAN_POINT('Ctrl Pts',(-21.1709002953281,-18.1632446813081,
-19.4732164465487));
#59041=CARTESIAN_POINT('Ctrl Pts',(-21.1437332452338,-18.0837602766129,
-19.4773951243614));
#59042=CARTESIAN_POINT('Ctrl Pts',(-21.112686592475,-18.0057177509962,-19.4815738021741));
#59043=CARTESIAN_POINT('Ctrl Pts',(-21.0810834482228,-17.9262763627721,
-19.4858273801273));
#59044=CARTESIAN_POINT('Ctrl Pts',(-21.0454603362217,-17.8483295278292,
-19.4900809580806));
#59045=CARTESIAN_POINT('Ctrl Pts',(-21.0059873754064,-17.7723079359452,
-19.4943345360339));
#59046=CARTESIAN_POINT('Ctrl Pts',(-20.967279678073,-17.697760176956,-19.4985056497431));
#59047=CARTESIAN_POINT('Ctrl Pts',(-20.9248702958461,-17.6250641047766,
-19.5026767634523));
#59048=CARTESIAN_POINT('Ctrl Pts',(-20.8789678617061,-17.5546049691487,
-19.5068478771615));
#59049=CARTESIAN_POINT('Ctrl Pts',(-20.8330808305555,-17.4841694767402,
-19.5110175912147));
#59050=CARTESIAN_POINT('Ctrl Pts',(-20.7837033262562,-17.4159698152611,
-19.5151873052678));
#59051=CARTESIAN_POINT('Ctrl Pts',(-20.7310884046656,-17.3503639914293,
-19.519357019321));
#59052=CARTESIAN_POINT('Ctrl Pts',(-20.6784753553166,-17.2847605021054,
-19.5235265849996));
#59053=CARTESIAN_POINT('Ctrl Pts',(-20.6226254062025,-17.2217510252597,
-19.5276961506783));
#59054=CARTESIAN_POINT('Ctrl Pts',(-20.5638323065115,-17.1616610013612,
-19.5318657163569));
#59055=CARTESIAN_POINT('Ctrl Pts',(-20.5029721055919,-17.0994582777943,
-19.5361818794149));
#59056=CARTESIAN_POINT('Ctrl Pts',(-20.4389583090022,-17.0403845006845,
-19.5404980424729));
#59057=CARTESIAN_POINT('Ctrl Pts',(-20.3721573781207,-16.9847581733532,
-19.5448142055309));
#59058=CARTESIAN_POINT('Ctrl Pts',(-20.3075324893086,-16.9309438750886,
-19.5489897694644));
#59059=CARTESIAN_POINT('Ctrl Pts',(-20.2402996649794,-16.8803561190116,
-19.553165333398));
#59060=CARTESIAN_POINT('Ctrl Pts',(-20.1708219663603,-16.8332403069284,
-19.5573408973316));
#59061=CARTESIAN_POINT('Ctrl Pts',(-20.0978350997288,-16.7837447772679,
-19.5617273599518));
#59062=CARTESIAN_POINT('Ctrl Pts',(-20.0223711203466,-16.738081448703,-19.566113822572));
#59063=CARTESIAN_POINT('Ctrl Pts',(-19.9448802162024,-16.6964803033426,
-19.5705002851921));
#59064=CARTESIAN_POINT('Ctrl Pts',(-19.8673893120582,-16.6548791579822,
-19.5748867478123));
#59065=CARTESIAN_POINT('Ctrl Pts',(-19.7878720403135,-16.6173403747379,
-19.5792732104325));
#59066=CARTESIAN_POINT('Ctrl Pts',(-19.706800567316,-16.5840348279103,-19.5836596730527));
#59067=CARTESIAN_POINT('Ctrl Pts',(-19.6294593229195,-16.5522617227512,
-19.587844307487));
#59068=CARTESIAN_POINT('Ctrl Pts',(-19.5504158778324,-16.5242225928466,
-19.5920289419213));
#59069=CARTESIAN_POINT('Ctrl Pts',(-19.4700654949528,-16.500101228203,-19.5962135763556));
#59070=CARTESIAN_POINT('Ctrl Pts',(-19.3898294809444,-16.4760141973502,
-19.6003922544784));
#59071=CARTESIAN_POINT('Ctrl Pts',(-19.3082906610536,-16.4558339863015,
-19.6045709326011));
#59072=CARTESIAN_POINT('Ctrl Pts',(-19.2258642779044,-16.4396963694407,
-19.6087496107238));
#59073=CARTESIAN_POINT('Ctrl Pts',(-19.1419604620519,-16.4232694975866,
-19.6130031885992));
#59074=CARTESIAN_POINT('Ctrl Pts',(-19.0571373968203,-16.4110317555328,
-19.6172567664746));
#59075=CARTESIAN_POINT('Ctrl Pts',(-18.9718493062316,-16.4030732243697,
-19.6215103443501));
#59076=CARTESIAN_POINT('Ctrl Pts',(-18.8882146908572,-16.3952689847839,
-19.6256814583605));
#59077=CARTESIAN_POINT('Ctrl Pts',(-18.8041333991978,-16.391579559832,-19.6298525723709));
#59078=CARTESIAN_POINT('Ctrl Pts',(-18.7200422944405,-16.3920380505844,
-19.6340236863813));
#59079=CARTESIAN_POINT('Ctrl Pts',(-18.6359794073137,-16.3924963874856,
-19.6381934007318));
#59080=CARTESIAN_POINT('Ctrl Pts',(-18.551907173272,-16.397099873298,-19.6423631150822));
#59081=CARTESIAN_POINT('Ctrl Pts',(-18.4682635936936,-16.4058295103502,
-19.6465328294327));
#59082=CARTESIAN_POINT('Ctrl Pts',(-18.3846229905612,-16.4145588367595,
-19.6507023954044));
#59083=CARTESIAN_POINT('Ctrl Pts',(-18.3014114690234,-16.4274139738751,
-19.6548719613761));
#59084=CARTESIAN_POINT('Ctrl Pts',(-18.2190616739277,-16.4443240798816,
-19.6590415273478));
#59085=CARTESIAN_POINT('Ctrl Pts',(-18.1338165629824,-16.4618287240758,
-19.6633576900467));
#59086=CARTESIAN_POINT('Ctrl Pts',(-18.0494954191543,-16.4836786817452,
-19.6676738527455));
#59087=CARTESIAN_POINT('Ctrl Pts',(-17.9665644117748,-16.5097382167496,
-19.6719900154444));
#59088=CARTESIAN_POINT('Ctrl Pts',(-17.8863348720819,-16.5349488655054,
-19.6761655796575));
#59089=CARTESIAN_POINT('Ctrl Pts',(-17.8074067178225,-16.5640988419262,
-19.6803411438706));
#59090=CARTESIAN_POINT('Ctrl Pts',(-17.7301828112974,-16.5970157003357,
-19.6845167080837));
#59091=CARTESIAN_POINT('Ctrl Pts',(-17.6490585105613,-16.6315951102757,
-19.6889031700254));
#59092=CARTESIAN_POINT('Ctrl Pts',(-17.5698156696774,-16.6703316765449,
-19.6932896319672));
#59093=CARTESIAN_POINT('Ctrl Pts',(-17.4928913452169,-16.7129713474315,
-19.6976760939089));
#59094=CARTESIAN_POINT('Ctrl Pts',(-17.4159670207564,-16.7556110183182,
-19.7020625558507));
#59095=CARTESIAN_POINT('Ctrl Pts',(-17.3413616647363,-16.8021534221795,
-19.7064490177924));
#59096=CARTESIAN_POINT('Ctrl Pts',(-17.2694745299275,-16.8522940330825,
-19.7108354797342));
#59097=CARTESIAN_POINT('Ctrl Pts',(-17.2373036985659,-16.8747328900772,
-19.7127985031288));
#59098=CARTESIAN_POINT('Ctrl Pts',(-17.2056206681701,-16.8979308207117,
-19.7147615265234));
#59099=CARTESIAN_POINT('Ctrl Pts',(-17.1744641548914,-16.9218650419685,
-19.7167245499181));
#59100=CARTESIAN_POINT('',(-21.2939989850553,-18.9542795868244,-19.3667098901939));
#59101=CARTESIAN_POINT('Ctrl Pts',(-21.2939989850559,-18.954279586128,-19.3667098902285));
#59102=CARTESIAN_POINT('Ctrl Pts',(-21.294073180434,-18.8709574030256,-19.3708480242597));
#59103=CARTESIAN_POINT('Ctrl Pts',(-21.2900751830219,-18.7875513930813,
-19.3749861582908));
#59104=CARTESIAN_POINT('Ctrl Pts',(-21.2820071809341,-18.7044936245096,
-19.379124292322));
#59105=CARTESIAN_POINT('Ctrl Pts',(-21.2739428344709,-18.6214734895453,
-19.3832605513581));
#59106=CARTESIAN_POINT('Ctrl Pts',(-21.2618121886764,-18.5388017480938,
-19.3873968103941));
#59107=CARTESIAN_POINT('Ctrl Pts',(-21.2456694473266,-18.4569074961523,
-19.3915330694301));
#59108=CARTESIAN_POINT('Ctrl Pts',(-21.2295289836496,-18.3750247991451,
-19.3956687448574));
#59109=CARTESIAN_POINT('Ctrl Pts',(-21.2093776397613,-18.2939198329769,
-19.3998044202847));
#59110=CARTESIAN_POINT('Ctrl Pts',(-21.1853208566141,-18.214012155975,-19.403940095712));
#59111=CARTESIAN_POINT('Ctrl Pts',(-21.1612599617833,-18.1340908214908,
-19.4080764779915));
#59112=CARTESIAN_POINT('Ctrl Pts',(-21.1332924395156,-18.0553676300856,
-19.4122128602709));
#59113=CARTESIAN_POINT('Ctrl Pts',(-21.1015733410968,-17.9782461940883,
-19.4163492425504));
#59114=CARTESIAN_POINT('Ctrl Pts',(-21.0698191717564,-17.901039487072,-19.4204901983123));
#59115=CARTESIAN_POINT('Ctrl Pts',(-21.0343053289603,-17.825438502363,-19.4246311540741));
#59116=CARTESIAN_POINT('Ctrl Pts',(-20.9952344193641,-17.7518254707406,
-19.428772109836));
#59117=CARTESIAN_POINT('Ctrl Pts',(-20.9561382227283,-17.6781647961105,
-19.4329157456612));
#59118=CARTESIAN_POINT('Ctrl Pts',(-20.9134806196083,-17.6064950352479,
-19.4370593814864));
#59119=CARTESIAN_POINT('Ctrl Pts',(-20.8675081508587,-17.5371703387972,
-19.4412030173116));
#59120=CARTESIAN_POINT('Ctrl Pts',(-20.8214607545949,-17.4677326545666,
-19.4453534065774));
#59121=CARTESIAN_POINT('Ctrl Pts',(-20.7720879921757,-17.4006480348511,
-19.4495037958431));
#59122=CARTESIAN_POINT('Ctrl Pts',(-20.7196769297237,-17.3362379102222,
-19.4536541851088));
#59123=CARTESIAN_POINT('Ctrl Pts',(-20.7018115389434,-17.3142823918094,
-19.4550689308257));
#59124=CARTESIAN_POINT('Ctrl Pts',(-20.6835934338648,-17.2926373126042,
-19.4564836765426));
#59125=CARTESIAN_POINT('Ctrl Pts',(-20.6650349200515,-17.2713143846806,
-19.4578984222595));
#59126=CARTESIAN_POINT('Ctrl Pts',(-20.6101412425931,-17.2082439287333,
-19.4620830566462));
#59127=CARTESIAN_POINT('Ctrl Pts',(-20.552052199416,-17.1477482923966,-19.4662676910329));
#59128=CARTESIAN_POINT('Ctrl Pts',(-20.4910387353975,-17.0901689436706,
-19.4704523254196));
#59129=CARTESIAN_POINT('Ctrl Pts',(-20.4301121164985,-17.0326715520257,
-19.4746310034968));
#59130=CARTESIAN_POINT('Ctrl Pts',(-20.3662696766049,-16.9780825158894,
-19.4788096815741));
#59131=CARTESIAN_POINT('Ctrl Pts',(-20.2998217436397,-16.9267093376147,
-19.4829883596513));
#59132=CARTESIAN_POINT('Ctrl Pts',(-20.2321827790971,-16.8744153319368,
-19.4872419375384));
#59133=CARTESIAN_POINT('Ctrl Pts',(-20.1618443123322,-16.8254539702931,
-19.4914955154255));
#59134=CARTESIAN_POINT('Ctrl Pts',(-20.0891719990944,-16.7801093828486,
-19.4957490933125));
#59135=CARTESIAN_POINT('Ctrl Pts',(-20.0179085806131,-16.7356438888117,
-19.4999202072829));
#59136=CARTESIAN_POINT('Ctrl Pts',(-19.9444014087305,-16.6946564386937,
-19.5040913212534));
#59137=CARTESIAN_POINT('Ctrl Pts',(-19.8690261614839,-16.6573724457448,
-19.5082624352238));
#59138=CARTESIAN_POINT('Ctrl Pts',(-19.7936762071349,-16.6201009638025,
-19.5124321495363));
#59139=CARTESIAN_POINT('Ctrl Pts',(-19.7164598343598,-16.5865306747405,
-19.5166018638488));
#59140=CARTESIAN_POINT('Ctrl Pts',(-19.6377770918967,-16.5568409305095,
-19.5207715781614));
#59141=CARTESIAN_POINT('Ctrl Pts',(-19.5590971493085,-16.527152242769,-19.5249411440973));
#59142=CARTESIAN_POINT('Ctrl Pts',(-19.4789513714909,-16.5013439869193,
-19.5291107100332));
#59143=CARTESIAN_POINT('Ctrl Pts',(-19.3977582580731,-16.4795467699389,
-19.5332802759692));
#59144=CARTESIAN_POINT('Ctrl Pts',(-19.3137104946165,-16.4569831896096,
-19.5375964387168));
#59145=CARTESIAN_POINT('Ctrl Pts',(-19.2285408859958,-16.4387180891116,
-19.5419126014644));
#59146=CARTESIAN_POINT('Ctrl Pts',(-19.1427269885612,-16.4248390932072,
-19.5462287642121));
#59147=CARTESIAN_POINT('Ctrl Pts',(-19.0597084701507,-16.4114122041898,
-19.5504043283951));
#59148=CARTESIAN_POINT('Ctrl Pts',(-18.9760874671123,-16.4020900585603,
-19.554579892578));
#59149=CARTESIAN_POINT('Ctrl Pts',(-18.8923014001436,-16.3968990887418,
-19.558755456761));
#59150=CARTESIAN_POINT('Ctrl Pts',(-18.8042834975808,-16.391445935345,-19.5631419187909));
#59151=CARTESIAN_POINT('Ctrl Pts',(-18.7160840019592,-16.3905522627805,
-19.5675283808209));
#59152=CARTESIAN_POINT('Ctrl Pts',(-18.6282074804617,-16.3941868827434,
-19.5719148428509));
#59153=CARTESIAN_POINT('Ctrl Pts',(-18.5403309589642,-16.3978215027064,
-19.5763013048809));
#59154=CARTESIAN_POINT('Ctrl Pts',(-18.4527779822414,-16.4059842855988,
-19.5806877669109));
#59155=CARTESIAN_POINT('Ctrl Pts',(-18.3660419494154,-16.4185819782338,
-19.5850742289409));
#59156=CARTESIAN_POINT('Ctrl Pts',(-18.2832980106531,-16.4305998521666,
-19.5892588006093));
#59157=CARTESIAN_POINT('Ctrl Pts',(-18.2009894838769,-16.4466981015662,
-19.5934433722777));
#59158=CARTESIAN_POINT('Ctrl Pts',(-18.1195501274547,-16.4668337371256,
-19.5976279439461));
#59159=CARTESIAN_POINT('Ctrl Pts',(-18.0344368519108,-16.4878777381211,
-19.6020012913924));
#59160=CARTESIAN_POINT('Ctrl Pts',(-17.9502735214004,-16.5133320171584,
-19.6063746388388));
#59161=CARTESIAN_POINT('Ctrl Pts',(-17.8675488473877,-16.5430868840623,
-19.6107479862852));
#59162=CARTESIAN_POINT('Ctrl Pts',(-17.7886021888952,-16.5714828535114,
-19.6149216040291));
#59163=CARTESIAN_POINT('Ctrl Pts',(-17.7109661623552,-16.6037950541263,
-19.619095221773));
#59164=CARTESIAN_POINT('Ctrl Pts',(-17.6350528481384,-16.6398764830971,
-19.623268839517));
#59165=CARTESIAN_POINT('Ctrl Pts',(-17.559191078058,-16.6759334132549,-19.6274396234296));
#59166=CARTESIAN_POINT('Ctrl Pts',(-17.4850501109929,-16.7157542909664,
-19.6316104073423));
#59167=CARTESIAN_POINT('Ctrl Pts',(-17.4130221293664,-16.7591439934879,
-19.635781191255));
#59168=CARTESIAN_POINT('Ctrl Pts',(-17.3410198802816,-16.8025181947097,
-19.6399504851235));
#59169=CARTESIAN_POINT('Ctrl Pts',(-17.2711295100132,-16.849458449815,-19.644119778992));
#59170=CARTESIAN_POINT('Ctrl Pts',(-17.2037174808643,-16.8997243334222,
-19.6482890728606));
#59171=CARTESIAN_POINT('Ctrl Pts',(-17.1939136458765,-16.9070345781162,
-19.6488954196746));
#59172=CARTESIAN_POINT('Ctrl Pts',(-17.1841621789156,-16.9144150859779,
-19.6495017664887));
#59173=CARTESIAN_POINT('Ctrl Pts',(-17.1744641548914,-16.9218650419685,
-19.6501081133027));
#59174=CARTESIAN_POINT('Ctrl Pts',(-17.1744641548914,-16.9218650419685,
-18.8501886385061));
#59175=CARTESIAN_POINT('Ctrl Pts',(-17.1079119429244,-16.9729899978358,
-18.8543616936919));
#59176=CARTESIAN_POINT('Ctrl Pts',(-17.0438080821223,-17.0274434278499,
-18.8585347488777));
#59177=CARTESIAN_POINT('Ctrl Pts',(-16.9824992587632,-17.0849581811199,
-18.8627078040634));
#59178=CARTESIAN_POINT('Ctrl Pts',(-16.9212252296614,-17.1424402933604,
-18.8668784909383));
#59179=CARTESIAN_POINT('Ctrl Pts',(-16.8627434233976,-17.2029799654239,
-18.8710491778132));
#59180=CARTESIAN_POINT('Ctrl Pts',(-16.8073667378616,-17.2662704032906,
-18.875219864688));
#59181=CARTESIAN_POINT('Ctrl Pts',(-16.7520048680834,-17.3295439081143,
-18.8793894357163));
#59182=CARTESIAN_POINT('Ctrl Pts',(-16.6997467716427,-17.3955663708758,
-18.8835590067445));
#59183=CARTESIAN_POINT('Ctrl Pts',(-16.6508668661375,-17.4639958512813,
-18.8877285777728));
#59184=CARTESIAN_POINT('Ctrl Pts',(-16.601985375499,-17.5324275507959,-18.8918982840166));
#59185=CARTESIAN_POINT('Ctrl Pts',(-16.5564825596719,-17.6032660478446,
-18.8960679902605));
#59186=CARTESIAN_POINT('Ctrl Pts',(-16.5145902773873,-17.6761393167072,
-18.9002376965043));
#59187=CARTESIAN_POINT('Ctrl Pts',(-16.4726552587905,-17.7490869270619,
-18.9044116564641));
#59188=CARTESIAN_POINT('Ctrl Pts',(-16.4343383603789,-17.8240730555622,
-18.9085856164239));
#59189=CARTESIAN_POINT('Ctrl Pts',(-16.3998258519895,-17.9007003059263,
-18.9127595763837));
#59190=CARTESIAN_POINT('Ctrl Pts',(-16.3652960238365,-17.9773660109238,
-18.9169356310043));
#59191=CARTESIAN_POINT('Ctrl Pts',(-16.3345745566648,-18.0556740495226,
-18.9211116856249));
#59192=CARTESIAN_POINT('Ctrl Pts',(-16.3077989187118,-18.1352085252919,
-18.9252877402455));
#59193=CARTESIAN_POINT('Ctrl Pts',(-16.2809754720839,-18.2148850121648,
-18.9294712513322));
#59194=CARTESIAN_POINT('Ctrl Pts',(-16.2581120567994,-18.2957918679272,
-18.9336547624189));
#59195=CARTESIAN_POINT('Ctrl Pts',(-16.2392957334692,-18.3774996757589,
-18.9378382735057));
#59196=CARTESIAN_POINT('Ctrl Pts',(-16.2222689257246,-18.4514367096189,
-18.9416239141817));
#59197=CARTESIAN_POINT('Ctrl Pts',(-16.2085553942316,-18.5260292086691,
-18.9454095548577));
#59198=CARTESIAN_POINT('Ctrl Pts',(-16.1981829862585,-18.6009557395151,
-18.9491951955337));
#59199=CARTESIAN_POINT('Ctrl Pts',(-16.1867173615959,-18.6837792730849,
-18.9533798299225));
#59200=CARTESIAN_POINT('Ctrl Pts',(-16.1792923755172,-18.7673192548711,
-18.9575644643113));
#59201=CARTESIAN_POINT('Ctrl Pts',(-16.1759873564286,-18.8511470608817,
-18.9617490987001));
#59202=CARTESIAN_POINT('Ctrl Pts',(-16.1726870416255,-18.9348555483864,
-18.9659277767798));
#59203=CARTESIAN_POINT('Ctrl Pts',(-16.173495063509,-19.0188505906137,-18.9701064548595));
#59204=CARTESIAN_POINT('Ctrl Pts',(-16.1784392678898,-19.1026961993429,
-18.9742851329392));
#59205=CARTESIAN_POINT('Ctrl Pts',(-16.1834720935872,-19.1880446804577,
-18.9785387108257));
#59206=CARTESIAN_POINT('Ctrl Pts',(-16.1927909085455,-19.2732378406054,
-18.9827922887122));
#59207=CARTESIAN_POINT('Ctrl Pts',(-16.2063695825694,-19.3578133473403,
-18.9870458665987));
#59208=CARTESIAN_POINT('Ctrl Pts',(-16.219685007484,-19.4407491927378,-18.9912169805725));
#59209=CARTESIAN_POINT('Ctrl Pts',(-16.2370965177703,-19.523090644708,-18.9953880945462));
#59210=CARTESIAN_POINT('Ctrl Pts',(-16.2585271389983,-19.6044064028226,
-18.99955920852));
#59211=CARTESIAN_POINT('Ctrl Pts',(-16.2799505689745,-19.6856948746498,
-19.0037289228362));
#59212=CARTESIAN_POINT('Ctrl Pts',(-16.3053903143092,-19.7659578916983,
-19.0078986371525));
#59213=CARTESIAN_POINT('Ctrl Pts',(-16.3347186663492,-19.8447760536634,
-19.0120683514687));
#59214=CARTESIAN_POINT('Ctrl Pts',(-16.3640459747608,-19.9235914109408,
-19.0162379174086));
#59215=CARTESIAN_POINT('Ctrl Pts',(-16.3972614535252,-20.0009615845049,
-19.0204074833486));
#59216=CARTESIAN_POINT('Ctrl Pts',(-16.4341885271964,-20.0764852998421,
-19.0245770492885));
#59217=CARTESIAN_POINT('Ctrl Pts',(-16.4724139113051,-20.154664336009,-19.0288932120324));
#59218=CARTESIAN_POINT('Ctrl Pts',(-16.5146165141599,-20.2308641813284,
-19.0332093747763));
#59219=CARTESIAN_POINT('Ctrl Pts',(-16.5605485527335,-20.3046672933043,
-19.0375255375201));
#59220=CARTESIAN_POINT('Ctrl Pts',(-16.6049843598883,-20.37606627652,-19.0417011017079));
#59221=CARTESIAN_POINT('Ctrl Pts',(-16.6529100541809,-20.4452219153925,
-19.0458766658956));
#59222=CARTESIAN_POINT('Ctrl Pts',(-16.7040581042265,-20.5117871328432,
-19.0500522300833));
#59223=CARTESIAN_POINT('Ctrl Pts',(-16.7577895208536,-20.5817144014007,
-19.0544386921052));
#59224=CARTESIAN_POINT('Ctrl Pts',(-16.8150769912941,-20.6487822429873,
-19.0588251541272));
#59225=CARTESIAN_POINT('Ctrl Pts',(-16.8755654265139,-20.712630834693,-19.0632116161492));
#59226=CARTESIAN_POINT('Ctrl Pts',(-16.9360538617338,-20.7764794263986,
-19.0675980781712));
#59227=CARTESIAN_POINT('Ctrl Pts',(-16.9997427890404,-20.8371084232607,
-19.0719845401931));
#59228=CARTESIAN_POINT('Ctrl Pts',(-17.066237677054,-20.8942072068041,-19.0763710022151));
#59229=CARTESIAN_POINT('Ctrl Pts',(-17.1296730365257,-20.9486787905254,
-19.0805556366056));
#59230=CARTESIAN_POINT('Ctrl Pts',(-17.1958979365974,-21.0001406364728,
-19.0847402709961));
#59231=CARTESIAN_POINT('Ctrl Pts',(-17.2645949112844,-21.0482940359732,
-19.0889249053866));
#59232=CARTESIAN_POINT('Ctrl Pts',(-17.3331941043301,-21.096378895069,-19.0931035834679));
#59233=CARTESIAN_POINT('Ctrl Pts',(-17.4042580092783,-21.1411643998052,
-19.0972822615492));
#59234=CARTESIAN_POINT('Ctrl Pts',(-17.4774351014414,-21.1823911441069,
-19.1014609396306));
#59235=CARTESIAN_POINT('Ctrl Pts',(-17.551923840448,-21.2243568482037,-19.1057145175167));
#59236=CARTESIAN_POINT('Ctrl Pts',(-17.6286019037977,-21.2626346413132,
-19.1099680954027));
#59237=CARTESIAN_POINT('Ctrl Pts',(-17.7070663992904,-21.2969962430106,
-19.1142216732888));
#59238=CARTESIAN_POINT('Ctrl Pts',(-17.7840097073652,-21.3306916779808,
-19.1183927872641));
#59239=CARTESIAN_POINT('Ctrl Pts',(-17.8626703579571,-21.3606212194832,
-19.1225639012393));
#59240=CARTESIAN_POINT('Ctrl Pts',(-17.9426440308619,-21.3866161360899,
-19.1267350152145));
#59241=CARTESIAN_POINT('Ctrl Pts',(-18.0225908678278,-21.4126023298512,
-19.1309047295321));
#59242=CARTESIAN_POINT('Ctrl Pts',(-18.103849414936,-21.4346563787677,-19.1350744438498));
#59243=CARTESIAN_POINT('Ctrl Pts',(-18.1859978966301,-21.4526586521759,
-19.1392441581674));
#59244=CARTESIAN_POINT('Ctrl Pts',(-18.2681434551281,-21.4706602849858,
-19.1434137241086));
#59245=CARTESIAN_POINT('Ctrl Pts',(-18.3511784356968,-21.4846103313097,
-19.1475832900499));
#59246=CARTESIAN_POINT('Ctrl Pts',(-18.4346698530335,-21.4944400608701,
-19.1517528559912));
#59247=CARTESIAN_POINT('Ctrl Pts',(-18.5210967257278,-21.5046153916099,
-19.1560690187333));
#59248=CARTESIAN_POINT('Ctrl Pts',(-18.608012205207,-21.5103752123295,-19.1603851814754));
#59249=CARTESIAN_POINT('Ctrl Pts',(-18.6949310840572,-21.5117018615079,
-19.1647013442175));
#59250=CARTESIAN_POINT('Ctrl Pts',(-18.7790185894518,-21.5129852952271,
-19.1688769084064));
#59251=CARTESIAN_POINT('Ctrl Pts',(-18.8631088069887,-21.5101200064032,
-19.1730524725952));
#59252=CARTESIAN_POINT('Ctrl Pts',(-18.9467650901062,-21.5031430803528,
-19.1772280367841));
#59253=CARTESIAN_POINT('Ctrl Pts',(-19.0346466533943,-21.4958137663384,
-19.1816144988028));
#59254=CARTESIAN_POINT('Ctrl Pts',(-19.1220487155994,-21.483946620245,-19.1860009608216));
#59255=CARTESIAN_POINT('Ctrl Pts',(-19.2084765196392,-21.4676454504383,
-19.1903874228403));
#59256=CARTESIAN_POINT('Ctrl Pts',(-19.2949043236791,-21.4513442806317,
-19.1947738848591));
#59257=CARTESIAN_POINT('Ctrl Pts',(-19.380357323635,-21.43060929785,-19.1991603468779));
#59258=CARTESIAN_POINT('Ctrl Pts',(-19.4643607861739,-21.4056041086572,
-19.2035468088966));
#59259=CARTESIAN_POINT('Ctrl Pts',(-19.5444991251693,-21.3817494451991,
-19.2077314433108));
#59260=CARTESIAN_POINT('Ctrl Pts',(-19.6236166763929,-21.3539201055357,
-19.211916077725));
#59261=CARTESIAN_POINT('Ctrl Pts',(-19.7012904348026,-21.3222213429846,
-19.2161007121391));
#59262=CARTESIAN_POINT('Ctrl Pts',(-19.778853634233,-21.2905676996977,-19.2202793902443));
#59263=CARTESIAN_POINT('Ctrl Pts',(-19.8549767005595,-21.2550557457739,
-19.2244580683494));
#59264=CARTESIAN_POINT('Ctrl Pts',(-19.9292512406756,-21.215840646261,-19.2286367464546));
#59265=CARTESIAN_POINT('Ctrl Pts',(-20.0048570980657,-21.1759226445248,
-19.2328903243347));
#59266=CARTESIAN_POINT('Ctrl Pts',(-20.0785470456786,-21.1321675712325,
-19.2371439022148));
#59267=CARTESIAN_POINT('Ctrl Pts',(-20.1499110579027,-21.0847906311002,
-19.241397480095));
#59268=CARTESIAN_POINT('Ctrl Pts',(-20.2198915399371,-21.038332185107,-19.2455685940941));
#59269=CARTESIAN_POINT('Ctrl Pts',(-20.2876350664325,-20.9883913190918,
-19.2497397080933));
#59270=CARTESIAN_POINT('Ctrl Pts',(-20.3527809100999,-20.935216671243,-19.2539108220924));
#59271=CARTESIAN_POINT('Ctrl Pts',(-20.4179048934498,-20.8820598666613,
-19.2580805364339));
#59272=CARTESIAN_POINT('Ctrl Pts',(-20.480432569049,-20.8256717259784,-19.2622502507755));
#59273=CARTESIAN_POINT('Ctrl Pts',(-20.5400350473299,-20.766342141884,-19.266419965117));
#59274=CARTESIAN_POINT('Ctrl Pts',(-20.5996354046978,-20.7070146689917,
-19.2705895310821));
#59275=CARTESIAN_POINT('Ctrl Pts',(-20.6563104462705,-20.6447462859464,
-19.2747590970472));
#59276=CARTESIAN_POINT('Ctrl Pts',(-20.7097680140269,-20.5798638624738,
-19.2789286630123));
#59277=CARTESIAN_POINT('Ctrl Pts',(-20.7651050833169,-20.5127002537634,
-19.2832448257261));
#59278=CARTESIAN_POINT('Ctrl Pts',(-20.8169938810791,-20.4427357722886,
-19.2875609884399));
#59279=CARTESIAN_POINT('Ctrl Pts',(-20.8651569232062,-20.3703688408415,
-19.2918771511538));
#59280=CARTESIAN_POINT('Ctrl Pts',(-20.9117510598039,-20.3003592538204,
-19.2960527153661));
#59281=CARTESIAN_POINT('Ctrl Pts',(-20.9548582452865,-20.2281017614681,
-19.3002282795785));
#59282=CARTESIAN_POINT('Ctrl Pts',(-20.9942733140313,-20.1539835880236,
-19.3044038437909));
#59283=CARTESIAN_POINT('Ctrl Pts',(-21.0356791435396,-20.0761218830757,
-19.3087903057554));
#59284=CARTESIAN_POINT('Ctrl Pts',(-21.0730098296578,-19.9962071202703,
-19.3131767677199));
#59285=CARTESIAN_POINT('Ctrl Pts',(-21.1060848561741,-19.9147115014943,
-19.3175632296844));
#59286=CARTESIAN_POINT('Ctrl Pts',(-21.1391598826905,-19.8332158827183,
-19.321949691649));
#59287=CARTESIAN_POINT('Ctrl Pts',(-21.1679791313071,-19.7501399810715,
-19.3263361536135));
#59288=CARTESIAN_POINT('Ctrl Pts',(-21.1924232051046,-19.6659715292665,
-19.330722615578));
#59289=CARTESIAN_POINT('Ctrl Pts',(-21.2214742546437,-19.56593984538,-19.3359357942359));
#59290=CARTESIAN_POINT('Ctrl Pts',(-21.2444357643464,-19.4640653478474,
-19.3411489728938));
#59291=CARTESIAN_POINT('Ctrl Pts',(-21.261115150052,-19.3610098023001,-19.3463621515516));
#59292=CARTESIAN_POINT('Ctrl Pts',(-21.277528721009,-19.2595966244285,-19.3514922492257));
#59293=CARTESIAN_POINT('Ctrl Pts',(-21.2878587862943,-19.1570396545895,
-19.3566223468997));
#59294=CARTESIAN_POINT('Ctrl Pts',(-21.2919675308073,-19.0539907414198,
-19.3617524445737));
#59295=CARTESIAN_POINT('Ctrl Pts',(-21.2932910194155,-19.020797131491,-19.3634049264471));
#59296=CARTESIAN_POINT('Ctrl Pts',(-21.2939693565913,-18.9875526505269,
-19.3650574083205));
#59297=CARTESIAN_POINT('Ctrl Pts',(-21.2939989850553,-18.9542795868244,
-19.3667098901939));
#59298=CARTESIAN_POINT('Origin',(-18.734,-18.952,1.76670989022851));
#59299=CARTESIAN_POINT('',(-17.1744641548914,-16.9218650419685,-18.0500683176023));
#59300=CARTESIAN_POINT('',(-17.1744641548915,-16.9218650419685,-18.1167065540548));
#59301=CARTESIAN_POINT('',(-17.1744641548914,-16.9218650419685,1.76670989022851));
#59302=CARTESIAN_POINT('',(-21.2936055493641,-18.9516176052657,-18.6332901348852));
#59303=CARTESIAN_POINT('Ctrl Pts',(-17.1744641548915,-16.9218650419685,
-18.1167065540548));
#59304=CARTESIAN_POINT('Ctrl Pts',(-17.1077794165571,-16.9730918036883,
-18.1208760334781));
#59305=CARTESIAN_POINT('Ctrl Pts',(-17.0436129585211,-17.027614071718,-18.1250455129013));
#59306=CARTESIAN_POINT('Ctrl Pts',(-16.9822980504549,-17.0851469581245,
-18.1292149923245));
#59307=CARTESIAN_POINT('Ctrl Pts',(-16.920972396523,-17.1426899275709,-18.1333852024781));
#59308=CARTESIAN_POINT('Ctrl Pts',(-16.8624996194374,-17.2032442473846,
-18.1375554126317));
#59309=CARTESIAN_POINT('Ctrl Pts',(-16.8071766738075,-17.2664876536672,
-18.1417256227852));
#59310=CARTESIAN_POINT('Ctrl Pts',(-16.7517926209873,-17.3298009157179,
-18.1459004391618));
#59311=CARTESIAN_POINT('Ctrl Pts',(-16.6995656464103,-17.3958088452489,
-18.1500752555384));
#59312=CARTESIAN_POINT('Ctrl Pts',(-16.650752512836,-17.4641559533254,-18.154250071915));
#59313=CARTESIAN_POINT('Ctrl Pts',(-16.6019086309308,-17.532546114559,-18.1584275180887));
#59314=CARTESIAN_POINT('Ctrl Pts',(-16.5564831185187,-17.603278000295,-18.1626049642624));
#59315=CARTESIAN_POINT('Ctrl Pts',(-16.5146881815939,-17.6759690236193,
-18.166782410436));
#59316=CARTESIAN_POINT('Ctrl Pts',(-16.472824736,-17.7487791993012,-18.1709667041204));
#59317=CARTESIAN_POINT('Ctrl Pts',(-16.434603952541,-17.8235545130221,-18.1751509978048));
#59318=CARTESIAN_POINT('Ctrl Pts',(-16.400190878549,-17.8998902221573,-18.1793352914892));
#59319=CARTESIAN_POINT('Ctrl Pts',(-16.3854130795555,-17.9326706057374,
-18.1811321275118));
#59320=CARTESIAN_POINT('Ctrl Pts',(-16.3713368223245,-17.9657385181925,
-18.1829289635344));
#59321=CARTESIAN_POINT('Ctrl Pts',(-16.3579723492966,-17.9990610706384,
-18.184725799557));
#59322=CARTESIAN_POINT('Ctrl Pts',(-16.3268479546497,-18.0766656473996,
-18.1889104339505));
#59323=CARTESIAN_POINT('Ctrl Pts',(-16.2994716572955,-18.1559410996701,
-18.193095068344));
#59324=CARTESIAN_POINT('Ctrl Pts',(-16.2760239311543,-18.236490639487,-18.1972797027375));
#59325=CARTESIAN_POINT('Ctrl Pts',(-16.2526095799489,-18.3169255270041,
-18.2014583808218));
#59326=CARTESIAN_POINT('Ctrl Pts',(-16.2331128202904,-18.398630461953,-18.2056370589062));
#59327=CARTESIAN_POINT('Ctrl Pts',(-16.217665944864,-18.4811890793931,-18.2098157369906));
#59328=CARTESIAN_POINT('Ctrl Pts',(-16.201942195299,-18.565227500706,-18.2140693148759));
#59329=CARTESIAN_POINT('Ctrl Pts',(-16.1904151258529,-18.6501500625611,
-18.2183228927612));
#59330=CARTESIAN_POINT('Ctrl Pts',(-16.1831710111198,-18.7355018025745,
-18.2225764706466));
#59331=CARTESIAN_POINT('Ctrl Pts',(-16.1760673376856,-18.8191988325684,
-18.226747584625));
#59332=CARTESIAN_POINT('Ctrl Pts',(-16.1730820747445,-18.9033080688141,
-18.2309186986033));
#59333=CARTESIAN_POINT('Ctrl Pts',(-16.1742446642318,-18.9873923862777,
-18.2350898125817));
#59334=CARTESIAN_POINT('Ctrl Pts',(-16.1754068636011,-19.0714484884366,
-18.2392595269025));
#59335=CARTESIAN_POINT('Ctrl Pts',(-16.180714144804,-19.1554792288139,-18.2434292412234));
#59336=CARTESIAN_POINT('Ctrl Pts',(-16.1901438433303,-19.2390467804617,
-18.2475989555442));
#59337=CARTESIAN_POINT('Ctrl Pts',(-16.1995732063073,-19.3226113584171,
-18.2517685214886));
#59338=CARTESIAN_POINT('Ctrl Pts',(-16.2131246425146,-19.4057123233778,
-18.2559380874331));
#59339=CARTESIAN_POINT('Ctrl Pts',(-16.2307236899664,-19.4879176388445,
-18.2601076533776));
#59340=CARTESIAN_POINT('Ctrl Pts',(-16.2489414982119,-19.573013191773,-18.264423816116));
#59341=CARTESIAN_POINT('Ctrl Pts',(-16.2714967310845,-19.6571484255569,
-18.2687399788544));
#59342=CARTESIAN_POINT('Ctrl Pts',(-16.2982497538329,-19.7398583237466,
-18.2730561415928));
#59343=CARTESIAN_POINT('Ctrl Pts',(-16.3241312996849,-19.8198739557201,
-18.2772317057849));
#59344=CARTESIAN_POINT('Ctrl Pts',(-16.3539411382348,-19.8985552629114,
-18.281407269977));
#59345=CARTESIAN_POINT('Ctrl Pts',(-16.3875034565753,-19.9755008410821,
-18.2855828341691));
#59346=CARTESIAN_POINT('Ctrl Pts',(-16.4227609278168,-20.0563327574591,
-18.2899692961806));
#59347=CARTESIAN_POINT('Ctrl Pts',(-16.4621596558346,-20.1352484709665,
-18.2943557581922));
#59348=CARTESIAN_POINT('Ctrl Pts',(-16.5054419382129,-20.2118130675793,
-18.2987422202037));
#59349=CARTESIAN_POINT('Ctrl Pts',(-16.5487242205912,-20.2883776641921,
-18.3031286822153));
#59350=CARTESIAN_POINT('Ctrl Pts',(-16.5958896819153,-20.362590695021,-18.3075151442268));
#59351=CARTESIAN_POINT('Ctrl Pts',(-16.6466304638568,-20.4340554711552,
-18.3119016062384));
#59352=CARTESIAN_POINT('Ctrl Pts',(-16.6950365872103,-20.5022320470105,
-18.3160862406309));
#59353=CARTESIAN_POINT('Ctrl Pts',(-16.7468764264203,-20.5681614794156,
-18.3202708750235));
#59354=CARTESIAN_POINT('Ctrl Pts',(-16.8019140327134,-20.6314772445658,
-18.324455509416));
#59355=CARTESIAN_POINT('Ctrl Pts',(-16.8568732997864,-20.6947028875613,
-18.3286341874995));
#59356=CARTESIAN_POINT('Ctrl Pts',(-16.9150209937603,-20.755321908626,-18.3328128655829));
#59357=CARTESIAN_POINT('Ctrl Pts',(-16.976078625133,-20.8129977001022,-18.3369915436664));
#59358=CARTESIAN_POINT('Ctrl Pts',(-17.0382306706759,-20.8717072886985,
-18.3412451215519));
#59359=CARTESIAN_POINT('Ctrl Pts',(-17.1033977218493,-20.9273667019601,
-18.3454986994375));
#59360=CARTESIAN_POINT('Ctrl Pts',(-17.1712439260889,-20.9796571340969,
-18.349752277323));
#59361=CARTESIAN_POINT('Ctrl Pts',(-17.2377747992587,-21.0309338141629,
-18.3539233913005));
#59362=CARTESIAN_POINT('Ctrl Pts',(-17.3068814901404,-21.0789706821841,
-18.358094505278));
#59363=CARTESIAN_POINT('Ctrl Pts',(-17.3782123821184,-21.1235063746623,
-18.3622656192554));
#59364=CARTESIAN_POINT('Ctrl Pts',(-17.4495193383267,-21.1680271227587,
-18.3664353335753));
#59365=CARTESIAN_POINT('Ctrl Pts',(-17.5230486234685,-21.2090487851565,
-18.3706050478952));
#59366=CARTESIAN_POINT('Ctrl Pts',(-17.5984198264987,-21.2463534316994,
-18.3747747622151));
#59367=CARTESIAN_POINT('Ctrl Pts',(-17.6737883474982,-21.2836567507829,
-18.3789443281586));
#59368=CARTESIAN_POINT('Ctrl Pts',(-17.750998243395,-21.3172431136927,-18.3831138941022));
#59369=CARTESIAN_POINT('Ctrl Pts',(-17.8296459350042,-21.346941278012,-18.3872834600458));
#59370=CARTESIAN_POINT('Ctrl Pts',(-17.9110587824485,-21.3776835931598,
-18.3915996227853));
#59371=CARTESIAN_POINT('Ctrl Pts',(-17.994011919152,-21.4042590180671,-18.3959157855248));
#59372=CARTESIAN_POINT('Ctrl Pts',(-18.0780387582278,-21.4265332588779,
-18.4002319482643));
#59373=CARTESIAN_POINT('Ctrl Pts',(-18.1593284318388,-21.4480819186317,
-18.4044075124555));
#59374=CARTESIAN_POINT('Ctrl Pts',(-18.2416224598005,-21.4656052611969,
-18.4085830766467));
#59375=CARTESIAN_POINT('Ctrl Pts',(-18.3244881604797,-21.4790338449045,
-18.4127586408379));
#59376=CARTESIAN_POINT('Ctrl Pts',(-18.4115392107375,-21.4931406744569,
-18.4171451028516));
#59377=CARTESIAN_POINT('Ctrl Pts',(-18.4992206213759,-21.5027281581545,
-18.4215315648652));
#59378=CARTESIAN_POINT('Ctrl Pts',(-18.5870272090958,-21.5077775722339,
-18.4259180268789));
#59379=CARTESIAN_POINT('Ctrl Pts',(-18.6748337968157,-21.5128269863133,
-18.4303044888925));
#59380=CARTESIAN_POINT('Ctrl Pts',(-18.7627649809675,-21.5133384034635,
-18.4346909509062));
#59381=CARTESIAN_POINT('Ctrl Pts',(-18.8503205710794,-21.5093559636358,
-18.4390774129198));
#59382=CARTESIAN_POINT('Ctrl Pts',(-18.9338475986689,-21.5055567617696,
-18.4432620473123));
#59383=CARTESIAN_POINT('Ctrl Pts',(-19.0173437395028,-21.4976540121366,
-18.4474466817047));
#59384=CARTESIAN_POINT('Ctrl Pts',(-19.100373090469,-21.4856477179316,-18.4516313160972));
#59385=CARTESIAN_POINT('Ctrl Pts',(-19.1832842594309,-21.4736585132005,
-18.4558099941805));
#59386=CARTESIAN_POINT('Ctrl Pts',(-19.2657295068645,-21.4575774310127,
-18.4599886722639));
#59387=CARTESIAN_POINT('Ctrl Pts',(-19.3472750579131,-21.437456437627,-18.4641673503472));
#59388=CARTESIAN_POINT('Ctrl Pts',(-19.4302822543734,-21.4169747898919,
-18.4684209282328));
#59389=CARTESIAN_POINT('Ctrl Pts',(-19.5123567014418,-21.3923069974992,
-18.4726745061184));
#59390=CARTESIAN_POINT('Ctrl Pts',(-19.5930485432779,-21.3635628957778,
-18.476928084004));
#59391=CARTESIAN_POINT('Ctrl Pts',(-19.6721760162886,-21.3353760545629,
-18.4810991979813));
#59392=CARTESIAN_POINT('Ctrl Pts',(-19.7499735613546,-21.3032697094725,
-18.4852703119587));
#59393=CARTESIAN_POINT('Ctrl Pts',(-19.8260310897304,-21.2673980433313,
-18.489441425936));
#59394=CARTESIAN_POINT('Ctrl Pts',(-19.9020630962677,-21.2315384142742,
-18.4936111402558));
#59395=CARTESIAN_POINT('Ctrl Pts',(-19.976355829977,-21.1919161695522,-18.4977808545756));
#59396=CARTESIAN_POINT('Ctrl Pts',(-20.0485201368015,-21.1487332131925,
-18.5019505688953));
#59397=CARTESIAN_POINT('Ctrl Pts',(-20.1206818757105,-21.1055517934677,
-18.5061201348388));
#59398=CARTESIAN_POINT('Ctrl Pts',(-20.1907149440062,-21.058810150979,-18.5102897007822));
#59399=CARTESIAN_POINT('Ctrl Pts',(-20.2582569041576,-21.0087549416807,
-18.5144592667256));
#59400=CARTESIAN_POINT('Ctrl Pts',(-20.3281735563277,-20.9569398529571,
-18.5187754294653));
#59401=CARTESIAN_POINT('Ctrl Pts',(-20.3954202425924,-20.9015741660664,
-18.5230915922049));
#59402=CARTESIAN_POINT('Ctrl Pts',(-20.4596314884387,-20.8429775160242,
-18.5274077549446));
#59403=CARTESIAN_POINT('Ctrl Pts',(-20.521751059686,-20.7862896457115,-18.5315833191356));
#59404=CARTESIAN_POINT('Ctrl Pts',(-20.5810296141591,-20.7265784444844,
-18.5357588833267));
#59405=CARTESIAN_POINT('Ctrl Pts',(-20.6371745600423,-20.6641701416646,
-18.5399344475178));
#59406=CARTESIAN_POINT('Ctrl Pts',(-20.6961552536973,-20.5986097438009,
-18.5443209095317));
#59407=CARTESIAN_POINT('Ctrl Pts',(-20.7516770948085,-20.5300730764181,
-18.5487073715456));
#59408=CARTESIAN_POINT('Ctrl Pts',(-20.8034508935154,-20.458974783906,-18.5530938335595));
#59409=CARTESIAN_POINT('Ctrl Pts',(-20.8552246922222,-20.3878764913939,
-18.5574802955735));
#59410=CARTESIAN_POINT('Ctrl Pts',(-20.9032501953501,-20.3142171013321,
-18.5618667575874));
#59411=CARTESIAN_POINT('Ctrl Pts',(-20.9472937739973,-20.238441086869,-18.5662532196013));
#59412=CARTESIAN_POINT('Ctrl Pts',(-20.9909726387703,-20.1632925546555,
-18.5706033584189));
#59413=CARTESIAN_POINT('Ctrl Pts',(-21.0308877830082,-20.0858014915382,
-18.5749534972364));
#59414=CARTESIAN_POINT('Ctrl Pts',(-21.066791372662,-20.0063644586356,-18.579303636054));
#59415=CARTESIAN_POINT('Ctrl Pts',(-21.1039225287105,-19.9242114234328,
-18.5838025088638));
#59416=CARTESIAN_POINT('Ctrl Pts',(-21.1367625751618,-19.839977276334,-18.5883013816736));
#59417=CARTESIAN_POINT('Ctrl Pts',(-21.1650869626509,-19.7541322709059,
-18.5928002544834));
#59418=CARTESIAN_POINT('Ctrl Pts',(-21.1923645588308,-19.6714598603191,
-18.5971328613515));
#59419=CARTESIAN_POINT('Ctrl Pts',(-21.2154541944231,-19.5872939815202,
-18.6014654682196));
#59420=CARTESIAN_POINT('Ctrl Pts',(-21.2342029378176,-19.5020775124729,
-18.6057980750877));
#59421=CARTESIAN_POINT('Ctrl Pts',(-21.252927481766,-19.4169710343355,-18.6101250897577));
#59422=CARTESIAN_POINT('Ctrl Pts',(-21.267322189726,-19.330817060707,-18.6144521044277));
#59423=CARTESIAN_POINT('Ctrl Pts',(-21.2772839154191,-19.2440734934402,
-18.6187791190978));
#59424=CARTESIAN_POINT('Ctrl Pts',(-21.2872318317731,-19.1574501735453,
-18.6231001354886));
#59425=CARTESIAN_POINT('Ctrl Pts',(-21.2927589555484,-19.0702392928319,
-18.6274211518793));
#59426=CARTESIAN_POINT('Ctrl Pts',(-21.2938134141943,-18.9829076772209,
-18.6317421682701));
#59427=CARTESIAN_POINT('Ctrl Pts',(-21.2939393290371,-18.9724792486627,
-18.6322581487706));
#59428=CARTESIAN_POINT('Ctrl Pts',(-21.2940015277989,-18.9620491070299,
-18.632774129271));
#59429=CARTESIAN_POINT('Ctrl Pts',(-21.2939999715072,-18.9516180532908,
-18.6332901097715));
#59430=CARTESIAN_POINT('Ctrl Pts',(-21.2898370902887,-18.9516133246636,
-18.6332903748308));
#59431=CARTESIAN_POINT('Ctrl Pts',(-21.2903731169848,-18.5470182197254,
-18.6533365919814));
#59432=CARTESIAN_POINT('Ctrl Pts',(-21.0089153450218,-17.2875283998103,
-18.7157747446925));
#59433=CARTESIAN_POINT('Ctrl Pts',(-19.2309396615754,-16.0736326248611,
-18.8102032524889));
#59434=CARTESIAN_POINT('Ctrl Pts',(-17.6886694270821,-16.5353972584879,
-18.8845855431345));
#59435=CARTESIAN_POINT('Ctrl Pts',(-17.1746506085039,-16.9221163620955,
-18.9165758982197));
#59436=CARTESIAN_POINT('',(-21.2939999971965,-18.9518801919504,-18.5667098901964));
#59437=CARTESIAN_POINT('Ctrl Pts',(-21.2939999971965,-18.9518801913084,
-18.5667098902285));
#59438=CARTESIAN_POINT('Ctrl Pts',(-21.2939996986147,-18.945500276023,-18.5670291853155));
#59439=CARTESIAN_POINT('Ctrl Pts',(-21.2939755504833,-18.939120426077,-18.5673484804024));
#59440=CARTESIAN_POINT('Ctrl Pts',(-21.2939275539577,-18.9327407557766,
-18.5676677754894));
#59441=CARTESIAN_POINT('Ctrl Pts',(-21.2932985185608,-18.84912973624,-18.5718524098819));
#59442=CARTESIAN_POINT('Ctrl Pts',(-21.2885677156651,-18.7653939703417,
-18.5760370442745));
#59443=CARTESIAN_POINT('Ctrl Pts',(-21.2797186185528,-18.6819690477864,
-18.580221678667));
#59444=CARTESIAN_POINT('Ctrl Pts',(-21.2708821170351,-18.5986628702825,
-18.5844003567505));
#59445=CARTESIAN_POINT('Ctrl Pts',(-21.2579390129528,-18.5156671108363,
-18.5885790348339));
#59446=CARTESIAN_POINT('Ctrl Pts',(-21.2409247859828,-18.4334172029223,
-18.5927577129174));
#59447=CARTESIAN_POINT('Ctrl Pts',(-21.2236055912197,-18.3496930245084,
-18.5970112908029));
#59448=CARTESIAN_POINT('Ctrl Pts',(-21.2020678918843,-18.2667421815314,
-18.6012648686885));
#59449=CARTESIAN_POINT('Ctrl Pts',(-21.1764043852929,-18.1850183713399,
-18.605518446574));
#59450=CARTESIAN_POINT('Ctrl Pts',(-21.1512384158586,-18.1048789366916,
-18.6096895605515));
#59451=CARTESIAN_POINT('Ctrl Pts',(-21.1221053294157,-18.02591984166,-18.613860674529));
#59452=CARTESIAN_POINT('Ctrl Pts',(-21.0891436468891,-17.9485567268061,
-18.6180317885064));
#59453=CARTESIAN_POINT('Ctrl Pts',(-21.0561930249733,-17.8712195718925,
-18.6222015028263));
#59454=CARTESIAN_POINT('Ctrl Pts',(-21.0194165386218,-17.7954777564205,
-18.6263712171462));
#59455=CARTESIAN_POINT('Ctrl Pts',(-20.9790011895035,-17.721727810959,-18.6305409314661));
#59456=CARTESIAN_POINT('Ctrl Pts',(-20.9385872785368,-17.6479804898368,
-18.6347104974097));
#59457=CARTESIAN_POINT('Ctrl Pts',(-20.8945349840831,-17.5762253008168,
-18.6388800633532));
#59458=CARTESIAN_POINT('Ctrl Pts',(-20.8470770406693,-17.5068337741989,
-18.6430496292968));
#59459=CARTESIAN_POINT('Ctrl Pts',(-20.7979505344986,-17.4350025270909,
-18.6473657920363));
#59460=CARTESIAN_POINT('Ctrl Pts',(-20.7451747360216,-17.3657046830186,
-18.6516819547758));
#59461=CARTESIAN_POINT('Ctrl Pts',(-20.6890551911698,-17.2993175745231,
-18.6559981175153));
#59462=CARTESIAN_POINT('Ctrl Pts',(-20.6347637346021,-17.23509301912,-18.6601736817065));
#59463=CARTESIAN_POINT('Ctrl Pts',(-20.5773433873059,-17.173592789127,-18.6643492458977));
#59464=CARTESIAN_POINT('Ctrl Pts',(-20.5171090485652,-17.1151216368728,
-18.668524810089));
#59465=CARTESIAN_POINT('Ctrl Pts',(-20.4538324165453,-17.0536972456979,
-18.6729112721026));
#59466=CARTESIAN_POINT('Ctrl Pts',(-20.3874504923529,-16.9956163559344,
-18.6772977341163));
#59467=CARTESIAN_POINT('Ctrl Pts',(-20.3183666557521,-16.9411836731962,
-18.6816841961299));
#59468=CARTESIAN_POINT('Ctrl Pts',(-20.2492828191514,-16.886750990458,-18.6860706581436));
#59469=CARTESIAN_POINT('Ctrl Pts',(-20.1774975877418,-16.835966787744,-18.6904571201572));
#59470=CARTESIAN_POINT('Ctrl Pts',(-20.1034462555221,-16.7890813808105,
-18.6948435821709));
#59471=CARTESIAN_POINT('Ctrl Pts',(-20.0328021348959,-16.7443532409684,
-18.6990282165633));
#59472=CARTESIAN_POINT('Ctrl Pts',(-19.9598329133702,-16.703006515634,-18.7032128509558));
#59473=CARTESIAN_POINT('Ctrl Pts',(-19.8848959073542,-16.665290877607,-18.7073974853483));
#59474=CARTESIAN_POINT('Ctrl Pts',(-19.810065564891,-16.6276289231225,-18.7115761634316));
#59475=CARTESIAN_POINT('Ctrl Pts',(-19.7332734088094,-16.5935879949175,
-18.715754841515));
#59476=CARTESIAN_POINT('Ctrl Pts',(-19.6549047742286,-16.5633739520798,
-18.7199335195983));
#59477=CARTESIAN_POINT('Ctrl Pts',(-19.5751314381813,-16.5326183442331,
-18.7241870974839));
#59478=CARTESIAN_POINT('Ctrl Pts',(-19.4937249583385,-16.5058284229433,
-18.7284406753695));
#59479=CARTESIAN_POINT('Ctrl Pts',(-19.4111169976704,-16.4831718222068,
-18.7326942532551));
#59480=CARTESIAN_POINT('Ctrl Pts',(-19.3301105535306,-16.4609544638903,
-18.7368653672324));
#59481=CARTESIAN_POINT('Ctrl Pts',(-19.247949263021,-16.4427117186153,-18.7410364812098));
#59482=CARTESIAN_POINT('Ctrl Pts',(-19.1650575928263,-16.4285520905581,
-18.7452075951871));
#59483=CARTESIAN_POINT('Ctrl Pts',(-19.0821937377322,-16.4143972139008,
-18.7493773095069));
#59484=CARTESIAN_POINT('Ctrl Pts',(-18.9986004427846,-16.4043228107593,
-18.7535470238266));
#59485=CARTESIAN_POINT('Ctrl Pts',(-18.9147123478962,-16.3983862767995,
-18.7577167381464));
#59486=CARTESIAN_POINT('Ctrl Pts',(-18.8308272381063,-16.3924499540871,
-18.7618863040898));
#59487=CARTESIAN_POINT('Ctrl Pts',(-18.7466478081782,-16.3906512394234,
-18.7660558700333));
#59488=CARTESIAN_POINT('Ctrl Pts',(-18.6626124310835,-16.3929955422071,
-18.7702254359767));
#59489=CARTESIAN_POINT('Ctrl Pts',(-18.5756224737719,-16.3954222677853,
-18.7745415987163));
#59490=CARTESIAN_POINT('Ctrl Pts',(-18.4887874147824,-16.4022887536938,
-18.778857761456));
#59491=CARTESIAN_POINT('Ctrl Pts',(-18.4025899172854,-16.4135423271059,
-18.7831739241956));
#59492=CARTESIAN_POINT('Ctrl Pts',(-18.319200294229,-16.4244293165443,-18.7873494883867));
#59493=CARTESIAN_POINT('Ctrl Pts',(-18.2364077885012,-16.439421833601,-18.7915250525778));
#59494=CARTESIAN_POINT('Ctrl Pts',(-18.1546390975922,-16.4584200544676,
-18.7957006167688));
#59495=CARTESIAN_POINT('Ctrl Pts',(-18.0687404644525,-16.4783778303154,
-18.8000870787827));
#59496=CARTESIAN_POINT('Ctrl Pts',(-17.9839723511228,-16.5027564393572,
-18.8044735407966));
#59497=CARTESIAN_POINT('Ctrl Pts',(-17.9008093086194,-16.5313816344172,
-18.8088600028106));
#59498=CARTESIAN_POINT('Ctrl Pts',(-17.8176462661159,-16.5600068294773,
-18.8132464648245));
#59499=CARTESIAN_POINT('Ctrl Pts',(-17.7360888041544,-16.5928783231054,
-18.8176329268384));
#59500=CARTESIAN_POINT('Ctrl Pts',(-17.6565830150583,-16.6297655931067,
-18.8220193888523));
#59501=CARTESIAN_POINT('Ctrl Pts',(-17.5807293782487,-16.6649584213697,
-18.8262043557618));
#59502=CARTESIAN_POINT('Ctrl Pts',(-17.5064606949899,-16.7039371893241,
-18.8303893226713));
#59503=CARTESIAN_POINT('Ctrl Pts',(-17.4341804046549,-16.7465365522057,
-18.8345742895809));
#59504=CARTESIAN_POINT('Ctrl Pts',(-17.3620114351116,-16.7890703066789,
-18.8387528111119));
#59505=CARTESIAN_POINT('Ctrl Pts',(-17.2918251656929,-16.8352133429876,
-18.8429313326429));
#59506=CARTESIAN_POINT('Ctrl Pts',(-17.2240032216123,-16.8847531039426,
-18.8471098541739));
#59507=CARTESIAN_POINT('Ctrl Pts',(-17.207345883423,-16.8969202655189,-18.848136115618));
#59508=CARTESIAN_POINT('Ctrl Pts',(-17.1908310530321,-16.9092921023112,
-18.8491623770621));
#59509=CARTESIAN_POINT('Ctrl Pts',(-17.1744641548914,-16.9218650419685,
-18.8501886385061));
#59510=CARTESIAN_POINT('Ctrl Pts',(-17.1744641548914,-16.9218650419685,
-18.0500683176022));
#59511=CARTESIAN_POINT('Ctrl Pts',(-17.1273611601948,-16.9580492416202,
-18.0530337279894));
#59512=CARTESIAN_POINT('Ctrl Pts',(-17.0815714136153,-16.9958326841265,
-18.0559991383765));
#59513=CARTESIAN_POINT('Ctrl Pts',(-17.03720428459,-17.0351055584185,-18.0589645487636));
#59514=CARTESIAN_POINT('Ctrl Pts',(-16.9745956774142,-17.0905254157143,
-18.0631491831567));
#59515=CARTESIAN_POINT('Ctrl Pts',(-16.9145885551718,-17.1491189671382,
-18.0673338175499));
#59516=CARTESIAN_POINT('Ctrl Pts',(-16.8575221052052,-17.2106124181141,
-18.071518451943));
#59517=CARTESIAN_POINT('Ctrl Pts',(-16.8005368822667,-17.2720183407739,
-18.075697130027));
#59518=CARTESIAN_POINT('Ctrl Pts',(-16.7464843277719,-17.3363156298582,
-18.079875808111));
#59519=CARTESIAN_POINT('Ctrl Pts',(-16.6956693348428,-17.4031913935286,
-18.084054486195));
#59520=CARTESIAN_POINT('Ctrl Pts',(-16.6439435196865,-17.4712658571988,
-18.0883080640804));
#59521=CARTESIAN_POINT('Ctrl Pts',(-16.5955728353228,-17.5420118234209,
-18.0925616419658));
#59522=CARTESIAN_POINT('Ctrl Pts',(-16.5508383402301,-17.6150612701733,
-18.0968152198512));
#59523=CARTESIAN_POINT('Ctrl Pts',(-16.5069711106161,-17.6866945108574,
-18.1009863338293));
#59524=CARTESIAN_POINT('Ctrl Pts',(-16.4666005905003,-17.7605423037905,
-18.1051574478073));
#59525=CARTESIAN_POINT('Ctrl Pts',(-16.4299490395872,-17.836227096663,-18.1093285617853));
#59526=CARTESIAN_POINT('Ctrl Pts',(-16.3933097874561,-17.9118864927724,
-18.1134982761057));
#59527=CARTESIAN_POINT('Ctrl Pts',(-16.3603872264447,-17.989381250901,-18.1176679904261));
#59528=CARTESIAN_POINT('Ctrl Pts',(-16.331357352511,-18.0683098345761,-18.1218377047466));
#59529=CARTESIAN_POINT('Ctrl Pts',(-16.3023285115847,-18.1472356096334,
-18.1260072706907));
#59530=CARTESIAN_POINT('Ctrl Pts',(-16.2771922403253,-18.227594676743,-18.1301768366348));
#59531=CARTESIAN_POINT('Ctrl Pts',(-16.2560756369329,-18.3089674573409,
-18.1343464025789));
#59532=CARTESIAN_POINT('Ctrl Pts',(-16.2342165998161,-18.393201204518,-18.1386625653177));
#59533=CARTESIAN_POINT('Ctrl Pts',(-16.2166652853052,-18.478520765314,-18.1429787280566));
#59534=CARTESIAN_POINT('Ctrl Pts',(-16.203505316394,-18.5644478664209,-18.1472948907955));
#59535=CARTESIAN_POINT('Ctrl Pts',(-16.1907740320855,-18.6475759012497,
-18.1514704549872));
#59536=CARTESIAN_POINT('Ctrl Pts',(-16.1821523920334,-18.7312720295791,
-18.1556460191789));
#59537=CARTESIAN_POINT('Ctrl Pts',(-16.177663165104,-18.8150986247193,-18.1598215833707));
#59538=CARTESIAN_POINT('Ctrl Pts',(-16.1729471979947,-18.9031591018972,
-18.1642080453831));
#59539=CARTESIAN_POINT('Ctrl Pts',(-16.172792072363,-18.9913629881318,-18.1685945073955));
#59540=CARTESIAN_POINT('Ctrl Pts',(-16.1771623761344,-19.0792059950832,
-18.1729809694079));
#59541=CARTESIAN_POINT('Ctrl Pts',(-16.1815326799057,-19.1670490020346,
-18.1773674314203));
#59542=CARTESIAN_POINT('Ctrl Pts',(-16.1904282787085,-19.2545305601574,
-18.1817538934327));
#59543=CARTESIAN_POINT('Ctrl Pts',(-16.2037517912765,-19.3411580684653,
-18.1861403554451));
#59544=CARTESIAN_POINT('Ctrl Pts',(-16.2164622692813,-19.4237997167046,
-18.1903249898381));
#59545=CARTESIAN_POINT('Ctrl Pts',(-16.2332494562529,-19.5059717882466,
-18.1945096242311));
#59546=CARTESIAN_POINT('Ctrl Pts',(-16.2540667299572,-19.5872408804027,
-18.1986942586241));
#59547=CARTESIAN_POINT('Ctrl Pts',(-16.274854372849,-19.6683942960652,-18.202872936708));
#59548=CARTESIAN_POINT('Ctrl Pts',(-16.299660595141,-19.748646843478,-18.2070516147919));
#59549=CARTESIAN_POINT('Ctrl Pts',(-16.3283873371777,-19.8275727933582,
-18.2112302928758));
#59550=CARTESIAN_POINT('Ctrl Pts',(-16.3576289854203,-19.9079134341682,
-18.2154838707612));
#59551=CARTESIAN_POINT('Ctrl Pts',(-16.3909330131977,-19.9868789746049,
-18.2197374486466));
#59552=CARTESIAN_POINT('Ctrl Pts',(-16.428142103854,-20.0640338856262,-18.2239910265321));
#59553=CARTESIAN_POINT('Ctrl Pts',(-16.4646298236797,-20.1396929981407,
-18.22816214051));
#59554=CARTESIAN_POINT('Ctrl Pts',(-16.5048723340172,-20.2136106264637,
-18.2323332544879));
#59555=CARTESIAN_POINT('Ctrl Pts',(-16.5486724780857,-20.2853955234528,
-18.2365043684658));
#59556=CARTESIAN_POINT('Ctrl Pts',(-16.5924579245929,-20.3571563323264,
-18.2406740827861));
#59557=CARTESIAN_POINT('Ctrl Pts',(-16.6397983945163,-20.4267854387981,
-18.2448437971064));
#59558=CARTESIAN_POINT('Ctrl Pts',(-16.6904515225008,-20.4939175140423,
-18.2490135114267));
#59559=CARTESIAN_POINT('Ctrl Pts',(-16.7411028480295,-20.5610472004393,
-18.2531830773707));
#59560=CARTESIAN_POINT('Ctrl Pts',(-16.795066319483,-20.6256796655625,-18.2573526433147));
#59561=CARTESIAN_POINT('Ctrl Pts',(-16.8520579335337,-20.6874809300205,
-18.2615222092587));
#59562=CARTESIAN_POINT('Ctrl Pts',(-16.9110533024294,-20.7514550506984,
-18.2658383719977));
#59563=CARTESIAN_POINT('Ctrl Pts',(-16.9732933572893,-20.8123947886944,
-18.2701545347367));
#59564=CARTESIAN_POINT('Ctrl Pts',(-17.0384212094901,-20.8699709500337,
-18.2744706974756));
#59565=CARTESIAN_POINT('Ctrl Pts',(-17.101427528754,-20.9256715739717,-18.2786462616673));
#59566=CARTESIAN_POINT('Ctrl Pts',(-17.1671359972395,-20.9782241356928,
-18.2828218258589));
#59567=CARTESIAN_POINT('Ctrl Pts',(-17.2351909645118,-21.0273726111566,
-18.2869973900505));
#59568=CARTESIAN_POINT('Ctrl Pts',(-17.3066832263984,-21.0790034592786,
-18.2913838520632));
#59569=CARTESIAN_POINT('Ctrl Pts',(-17.3807647695956,-21.1268769860888,
-18.2957703140758));
#59570=CARTESIAN_POINT('Ctrl Pts',(-17.4569923995305,-21.1707500058238,
-18.3001567760885));
#59571=CARTESIAN_POINT('Ctrl Pts',(-17.5332200294655,-21.2146230255589,
-18.3045432381011));
#59572=CARTESIAN_POINT('Ctrl Pts',(-17.6115931945078,-21.25449534292,-18.3089297001138));
#59573=CARTESIAN_POINT('Ctrl Pts',(-17.6916449845513,-21.2901822045702,
-18.3133161621265));
#59574=CARTESIAN_POINT('Ctrl Pts',(-17.7680134730656,-21.3242270608135,
-18.3175007965194));
#59575=CARTESIAN_POINT('Ctrl Pts',(-17.8461937671324,-21.3545898770089,
-18.3216854309123));
#59576=CARTESIAN_POINT('Ctrl Pts',(-17.9257962079471,-21.3810752624222,
-18.3258700653053));
#59577=CARTESIAN_POINT('Ctrl Pts',(-18.00528534454,-21.4075229491675,-18.3300487433891));
#59578=CARTESIAN_POINT('Ctrl Pts',(-18.0861921743113,-21.4301040236941,
-18.3342274214729));
#59579=CARTESIAN_POINT('Ctrl Pts',(-18.1681056484757,-21.4486704994678,
-18.3384060995568));
#59580=CARTESIAN_POINT('Ctrl Pts',(-18.2514873627971,-21.4675697659769,
-18.3426596774422));
#59581=CARTESIAN_POINT('Ctrl Pts',(-18.3359117243118,-21.4823088984315,
-18.3469132553277));
#59582=CARTESIAN_POINT('Ctrl Pts',(-18.4209273694976,-21.4927844316333,
-18.3511668332132));
#59583=CARTESIAN_POINT('Ctrl Pts',(-18.5042948205043,-21.5030568761823,
-18.355337947191));
#59584=CARTESIAN_POINT('Ctrl Pts',(-18.5882303557905,-21.5092295037566,
-18.3595090611688));
#59585=CARTESIAN_POINT('Ctrl Pts',(-18.6722982811997,-21.5112563173502,
-18.3636801751467));
#59586=CARTESIAN_POINT('Ctrl Pts',(-18.7563379968047,-21.513282450827,-18.3678498894669));
#59587=CARTESIAN_POINT('Ctrl Pts',(-18.8405095547877,-21.5111655221263,
-18.3720196037872));
#59588=CARTESIAN_POINT('Ctrl Pts',(-18.9243745836512,-21.5049115765924,
-18.3761893181074));
#59589=CARTESIAN_POINT('Ctrl Pts',(-19.0082366282371,-21.4986578536008,
-18.3803588840514));
#59590=CARTESIAN_POINT('Ctrl Pts',(-19.0917917066947,-21.4882674415331,
-18.3845284499953));
#59591=CARTESIAN_POINT('Ctrl Pts',(-19.1746052695949,-21.4737983655331,
-18.3886980159392));
#59592=CARTESIAN_POINT('Ctrl Pts',(-19.2603304552103,-21.4588205746695,
-18.3930141786783));
#59593=CARTESIAN_POINT('Ctrl Pts',(-19.3452604921636,-21.4394720625983,
-18.3973303414173));
#59594=CARTESIAN_POINT('Ctrl Pts',(-19.4289254033755,-21.4158747297181,
-18.4016465041564));
#59595=CARTESIAN_POINT('Ctrl Pts',(-19.5098649388997,-21.3930460774758,
-18.405822068348));
#59596=CARTESIAN_POINT('Ctrl Pts',(-19.5896200744146,-21.3662413589924,
-18.4099976325395));
#59597=CARTESIAN_POINT('Ctrl Pts',(-19.6677830273837,-21.3356210390434,
-18.4141731967311));
#59598=CARTESIAN_POINT('Ctrl Pts',(-19.7498938052998,-21.3034541595237,
-18.4185596587439));
#59599=CARTESIAN_POINT('Ctrl Pts',(-19.8302467994653,-21.2670763374215,
-18.4229461207567));
#59600=CARTESIAN_POINT('Ctrl Pts',(-19.9083976363218,-21.2267285973939,
-18.4273325827695));
#59601=CARTESIAN_POINT('Ctrl Pts',(-19.9865484731783,-21.1863808573664,
-18.4317190447823));
#59602=CARTESIAN_POINT('Ctrl Pts',(-20.0624966899234,-21.1420635575359,
-18.4361055067951));
#59603=CARTESIAN_POINT('Ctrl Pts',(-20.1358342086536,-21.0940692919344,
-18.4404919688079));
#59604=CARTESIAN_POINT('Ctrl Pts',(-20.2057039471169,-21.0483444454524,
-18.4446710160258));
#59605=CARTESIAN_POINT('Ctrl Pts',(-20.2734659150701,-20.9991112651902,
-18.4488500632436));
#59606=CARTESIAN_POINT('Ctrl Pts',(-20.3387454860835,-20.9465906660001,
-18.4530291104615));
#59607=CARTESIAN_POINT('Ctrl Pts',(-20.4039320790896,-20.8941448721524,
-18.4572022054423));
#59608=CARTESIAN_POINT('Ctrl Pts',(-20.46664294125,-20.8384212459577,-18.461375300423));
#59609=CARTESIAN_POINT('Ctrl Pts',(-20.5265316718116,-20.7796843834624,
-18.4655483954038));
#59610=CARTESIAN_POINT('Ctrl Pts',(-20.5870226816093,-20.7203568256503,
-18.4697634576868));
#59611=CARTESIAN_POINT('Ctrl Pts',(-20.6446340707897,-20.6579553356914,
-18.4739785199699));
#59612=CARTESIAN_POINT('Ctrl Pts',(-20.6990425114804,-20.5927949073771,
-18.4781935822529));
#59613=CARTESIAN_POINT('Ctrl Pts',(-20.7528122887531,-20.528399352699,-18.4823591668069));
#59614=CARTESIAN_POINT('Ctrl Pts',(-20.803453612438,-20.4613096522777,-18.4865247513609));
#59615=CARTESIAN_POINT('Ctrl Pts',(-20.8506921231955,-20.3918661241943,
-18.4906903359149));
#59616=CARTESIAN_POINT('Ctrl Pts',(-20.8979149500345,-20.3224456524396,
-18.4948545374302));
#59617=CARTESIAN_POINT('Ctrl Pts',(-20.9417369482816,-20.2506732862343,
-18.4990187389455));
#59618=CARTESIAN_POINT('Ctrl Pts',(-20.9819260328718,-20.1769198140031,
-18.5031829404608));
#59619=CARTESIAN_POINT('Ctrl Pts',(-21.0221139173366,-20.1031685441961,
-18.5073470176248));
#59620=CARTESIAN_POINT('Ctrl Pts',(-21.0586688839111,-20.0274366916314,
-18.5115110947889));
#59621=CARTESIAN_POINT('Ctrl Pts',(-21.0914046022627,-19.9501200034218,
-18.5156751719529));
#59622=CARTESIAN_POINT('Ctrl Pts',(-21.1248385440614,-19.8711542197507,
-18.5199280651399));
#59623=CARTESIAN_POINT('Ctrl Pts',(-21.1542882228969,-19.7905356687051,
-18.5241809583268));
#59624=CARTESIAN_POINT('Ctrl Pts',(-21.1796074785074,-19.7087060598863,
-18.5284338515138));
#59625=CARTESIAN_POINT('Ctrl Pts',(-21.2044336791703,-19.6284699613236,
-18.5326039259141));
#59626=CARTESIAN_POINT('Ctrl Pts',(-21.2252888283687,-19.5470700198229,
-18.5367740003145));
#59627=CARTESIAN_POINT('Ctrl Pts',(-21.2420864983913,-19.4649348073461,
-18.5409440747148));
#59628=CARTESIAN_POINT('Ctrl Pts',(-21.2593845777048,-19.3803527541243,
-18.5452383772951));
#59629=CARTESIAN_POINT('Ctrl Pts',(-21.2723795196075,-19.294991452669,-18.5495326798753));
#59630=CARTESIAN_POINT('Ctrl Pts',(-21.2810343673868,-19.2093245642189,
-18.5538269824556));
#59631=CARTESIAN_POINT('Ctrl Pts',(-21.2896892151661,-19.1236576757689,
-18.5581212850359));
#59632=CARTESIAN_POINT('Ctrl Pts',(-21.2940040128973,-19.0376857298059,
-18.5624155876161));
#59633=CARTESIAN_POINT('Ctrl Pts',(-21.2939999971965,-18.9518801919504,
-18.5667098901964));
#59634=CARTESIAN_POINT('Origin',(-18.734,-18.952,1.76670989022851));
#59635=CARTESIAN_POINT('',(-17.1762220723152,-16.9241895431829,-17.2500265390144));
#59636=CARTESIAN_POINT('',(-17.1735447326512,-16.9206895600705,-17.3168006994722));
#59637=CARTESIAN_POINT('',(-17.1744641548914,-16.9218650419685,1.76670989022851));
#59638=CARTESIAN_POINT('',(-21.2939989159607,-18.9543559031924,-17.8332901097715));
#59639=CARTESIAN_POINT('Ctrl Pts',(-17.1735447326512,-16.9206895600706,
-17.3168006994722));
#59640=CARTESIAN_POINT('Ctrl Pts',(-16.6213792717057,-17.3535717521052,
-17.3517574528043));
#59641=CARTESIAN_POINT('Ctrl Pts',(-15.7867861609283,-18.831728284438,-17.4291061416968));
#59642=CARTESIAN_POINT('Ctrl Pts',(-16.8703561902843,-21.337397809626,-17.5488467661498));
#59643=CARTESIAN_POINT('Ctrl Pts',(-19.7309870131108,-21.8102001076479,
-17.6760225728312));
#59644=CARTESIAN_POINT('Ctrl Pts',(-21.1817725818657,-20.2077259866878,
-17.7708370079975));
#59645=CARTESIAN_POINT('Ctrl Pts',(-21.2957663888719,-19.1559927477998,
-17.8232595076033));
#59646=CARTESIAN_POINT('Ctrl Pts',(-21.2939116922138,-18.9543565892689,
-17.8332900716486));
#59647=CARTESIAN_POINT('Ctrl Pts',(-21.2939989159607,-18.9543559031924,
-17.8332901097715));
#59648=CARTESIAN_POINT('Ctrl Pts',(-21.2940751741219,-18.8714913735434,
-17.837412174938));
#59649=CARTESIAN_POINT('Ctrl Pts',(-21.290123839502,-18.7885152466555,-17.8415342401044));
#59650=CARTESIAN_POINT('Ctrl Pts',(-21.2821391268744,-18.7058557534859,
-17.8456563052709));
#59651=CARTESIAN_POINT('Ctrl Pts',(-21.2741597741335,-18.6232517470386,
-17.8497756034244));
#59652=CARTESIAN_POINT('Ctrl Pts',(-21.262152459652,-18.5409644216312,-17.8538949015779));
#59653=CARTESIAN_POINT('Ctrl Pts',(-21.2461634417033,-18.4594202174576,
-17.8580141997315));
#59654=CARTESIAN_POINT('Ctrl Pts',(-21.2301800733889,-18.3779048264943,
-17.862132042353));
#59655=CARTESIAN_POINT('Ctrl Pts',(-21.2102178848107,-18.2971324990613,
-17.8662498849744));
#59656=CARTESIAN_POINT('Ctrl Pts',(-21.1863745538874,-18.217521240984,-17.8703677275959));
#59657=CARTESIAN_POINT('Ctrl Pts',(-21.1625320679642,-18.1379128043046,
-17.8744854242823));
#59658=CARTESIAN_POINT('Ctrl Pts',(-21.1348088500427,-18.0594658076282,
-17.8786031209688));
#59659=CARTESIAN_POINT('Ctrl Pts',(-21.103352505349,-17.9825833169393,-17.8827208176552));
#59660=CARTESIAN_POINT('Ctrl Pts',(-21.071866121991,-17.905627408714,-17.8868424464612));
#59661=CARTESIAN_POINT('Ctrl Pts',(-21.0366396717683,-17.8302394286303,
-17.8909640752672));
#59662=CARTESIAN_POINT('Ctrl Pts',(-20.9978687619911,-17.7568020128526,
-17.8950857040732));
#59663=CARTESIAN_POINT('Ctrl Pts',(-20.9590794967265,-17.683329829267,-17.8992092842005));
#59664=CARTESIAN_POINT('Ctrl Pts',(-20.9167426732498,-17.6118104548626,
-17.9033328643279));
#59665=CARTESIAN_POINT('Ctrl Pts',(-20.8710983794442,-17.5425992349311,
-17.9074564444553));
#59666=CARTESIAN_POINT('Ctrl Pts',(-20.8253741239691,-17.4732667677585,
-17.9115872484506));
#59667=CARTESIAN_POINT('Ctrl Pts',(-20.776331105883,-17.4062509123682,-17.9157180524459));
#59668=CARTESIAN_POINT('Ctrl Pts',(-20.724250792007,-17.3418752269108,-17.9198488564413));
#59669=CARTESIAN_POINT('Ctrl Pts',(-20.6800170723894,-17.2871985975131,
-17.9233572996922));
#59670=CARTESIAN_POINT('Ctrl Pts',(-20.6335931281536,-17.2344260450368,
-17.9268657429431));
#59671=CARTESIAN_POINT('Ctrl Pts',(-20.5851713910723,-17.1837340469049,
-17.930374186194));
#59672=CARTESIAN_POINT('Ctrl Pts',(-20.5274172101246,-17.1232720517519,
-17.934558820587));
#59673=CARTESIAN_POINT('Ctrl Pts',(-20.4665902688467,-17.0655300202436,
-17.93874345498));
#59674=CARTESIAN_POINT('Ctrl Pts',(-20.4029770272298,-17.0108365131759,
-17.942928089373));
#59675=CARTESIAN_POINT('Ctrl Pts',(-20.3394543311885,-16.9562208555457,
-17.9471067674569));
#59676=CARTESIAN_POINT('Ctrl Pts',(-20.2731535582845,-16.9046454006956,
-17.9512854455408));
#59677=CARTESIAN_POINT('Ctrl Pts',(-20.2043989371765,-16.8564029572577,
-17.9554641236247));
#59678=CARTESIAN_POINT('Ctrl Pts',(-20.1344119388971,-16.8072958026916,
-17.9597177015102));
#59679=CARTESIAN_POINT('Ctrl Pts',(-20.0618825897098,-16.7616426719214,
-17.9639712793956));
#59680=CARTESIAN_POINT('Ctrl Pts',(-19.9871893049686,-16.7197104654834,
-17.9682248572811));
#59681=CARTESIAN_POINT('Ctrl Pts',(-19.9139440953053,-16.6785911966919,
-17.972395971259));
#59682=CARTESIAN_POINT('Ctrl Pts',(-19.8386185251852,-16.6410501005271,
-17.9765670852369));
#59683=CARTESIAN_POINT('Ctrl Pts',(-19.7615983036834,-16.6072949596448,
-17.9807381992148));
#59684=CARTESIAN_POINT('Ctrl Pts',(-19.6846039270608,-16.5735511456261,
-17.9849079135351));
#59685=CARTESIAN_POINT('Ctrl Pts',(-19.6059164494112,-16.5435909483339,
-17.9890776278554));
#59686=CARTESIAN_POINT('Ctrl Pts',(-19.5259437923519,-16.517575010448,-17.9932473421758));
#59687=CARTESIAN_POINT('Ctrl Pts',(-19.4459739810629,-16.4915599983208,
-17.9974169081197));
#59688=CARTESIAN_POINT('Ctrl Pts',(-19.3647195190222,-16.469489108043,-18.0015864740637));
#59689=CARTESIAN_POINT('Ctrl Pts',(-19.2826045027056,-16.4514734355318,
-18.0057560400077));
#59690=CARTESIAN_POINT('Ctrl Pts',(-19.1976024237126,-16.4328243541993,
-18.0100722027467));
#59691=CARTESIAN_POINT('Ctrl Pts',(-19.1116786655145,-16.4185210722996,
-18.0143883654857));
#59692=CARTESIAN_POINT('Ctrl Pts',(-19.0253143284884,-16.4086290160464,
-18.0187045282247));
#59693=CARTESIAN_POINT('Ctrl Pts',(-18.9417633006593,-16.3990591924854,
-18.0228800924163));
#59694=CARTESIAN_POINT('Ctrl Pts',(-18.8578004300249,-16.3936175999791,
-18.0270556566079));
#59695=CARTESIAN_POINT('Ctrl Pts',(-18.7738638919265,-16.3923103957471,
-18.0312312207996));
#59696=CARTESIAN_POINT('Ctrl Pts',(-18.6856879188254,-16.3909371677368,
-18.0356176828122));
#59697=CARTESIAN_POINT('Ctrl Pts',(-18.5975415917828,-16.3941269389876,
-18.0400041448249));
#59698=CARTESIAN_POINT('Ctrl Pts',(-18.5099274935594,-16.4018251997447,
-18.0443906068376));
#59699=CARTESIAN_POINT('Ctrl Pts',(-18.4223133953359,-16.4095234605017,
-18.0487770688502));
#59700=CARTESIAN_POINT('Ctrl Pts',(-18.3352320899719,-16.4217300548923,
-18.0531635308629));
#59701=CARTESIAN_POINT('Ctrl Pts',(-18.249172131343,-16.4383289917387,-18.0575499928756));
#59702=CARTESIAN_POINT('Ctrl Pts',(-18.1670679985969,-16.4541649430451,
-18.0617348270901));
#59703=CARTESIAN_POINT('Ctrl Pts',(-18.0855877575642,-16.4740572520247,
-18.0659196613047));
#59704=CARTESIAN_POINT('Ctrl Pts',(-18.0051627929096,-16.4979428846173,
-18.0701044955193));
#59705=CARTESIAN_POINT('Ctrl Pts',(-17.9248712290264,-16.5217888981459,
-18.0742823883554));
#59706=CARTESIAN_POINT('Ctrl Pts',(-17.8456318987211,-16.5496149366924,
-18.0784602811916));
#59707=CARTESIAN_POINT('Ctrl Pts',(-17.7678662694262,-16.5813069336906,
-18.0826381740277));
#59708=CARTESIAN_POINT('Ctrl Pts',(-17.6901757083229,-16.6129683379845,
-18.0868120338886));
#59709=CARTESIAN_POINT('Ctrl Pts',(-17.6139564476478,-16.648488119702,-18.0909858937495));
#59710=CARTESIAN_POINT('Ctrl Pts',(-17.5396142320594,-16.6877026172914,
-18.0951597536104));
#59711=CARTESIAN_POINT('Ctrl Pts',(-17.4653211999375,-16.7268911712778,
-18.099330852121));
#59712=CARTESIAN_POINT('Ctrl Pts',(-17.392903152695,-16.7697693732504,-18.1035019506317));
#59713=CARTESIAN_POINT('Ctrl Pts',(-17.3227440412668,-16.8161262633433,
-18.1076730491423));
#59714=CARTESIAN_POINT('Ctrl Pts',(-17.2720952992043,-16.8495918834365,
-18.1106842174465));
#59715=CARTESIAN_POINT('Ctrl Pts',(-17.2226233973444,-16.8848694399857,
-18.1136953857507));
#59716=CARTESIAN_POINT('Ctrl Pts',(-17.1744641548915,-16.9218650419685,
-18.1167065540548));
#59717=CARTESIAN_POINT('',(-21.2939990418858,-18.9497851537328,-17.7667099127498));
#59718=CARTESIAN_POINT('Ctrl Pts',(-21.2939990418858,-18.9497851537328,
-17.7667099127498));
#59719=CARTESIAN_POINT('Ctrl Pts',(-21.2939112972755,-18.8483667746996,
-17.7717442924651));
#59720=CARTESIAN_POINT('Ctrl Pts',(-21.2877929815452,-18.7472123213116,
-17.7767786721804));
#59721=CARTESIAN_POINT('Ctrl Pts',(-21.275760552819,-18.64695362298,-17.7818130518957));
#59722=CARTESIAN_POINT('Ctrl Pts',(-21.2635573150894,-18.54527168012,-17.7869188982619));
#59723=CARTESIAN_POINT('Ctrl Pts',(-21.245270932926,-18.4445110968148,-17.792024744628));
#59724=CARTESIAN_POINT('Ctrl Pts',(-21.2210717431372,-18.345308855769,-17.7971305909941));
#59725=CARTESIAN_POINT('Ctrl Pts',(-21.2092508709201,-18.2968503319384,
-17.7996247057963));
#59726=CARTESIAN_POINT('Ctrl Pts',(-21.1960198419216,-18.2487633198847,
-17.8021188205986));
#59727=CARTESIAN_POINT('Ctrl Pts',(-21.1814026084241,-18.201120201178,-17.8046129354008));
#59728=CARTESIAN_POINT('Ctrl Pts',(-21.1568777637899,-18.121184412756,-17.8087975697939));
#59729=CARTESIAN_POINT('Ctrl Pts',(-21.1283869296254,-18.0423026572185,
-17.8129822041869));
#59730=CARTESIAN_POINT('Ctrl Pts',(-21.0960388974778,-17.9648970434641,
-17.8171668385799));
#59731=CARTESIAN_POINT('Ctrl Pts',(-21.0637369087501,-17.88760160702,-17.8213455166639));
#59732=CARTESIAN_POINT('Ctrl Pts',(-21.0275888032569,-17.8117785597318,
-17.8255241947478));
#59733=CARTESIAN_POINT('Ctrl Pts',(-20.9877531601769,-17.7378349811526,
-17.8297028728318));
#59734=CARTESIAN_POINT('Ctrl Pts',(-20.947203491824,-17.6625660170697,-17.8339564507172));
#59735=CARTESIAN_POINT('Ctrl Pts',(-20.9028329287837,-17.5892450243181,
-17.8382100286026));
#59736=CARTESIAN_POINT('Ctrl Pts',(-20.8548601014715,-17.5182802121801,
-17.8424636064881));
#59737=CARTESIAN_POINT('Ctrl Pts',(-20.8078173210281,-17.448691191402,-17.846634720466));
#59738=CARTESIAN_POINT('Ctrl Pts',(-20.7573109732373,-17.3813682068563,
-17.850805834444));
#59739=CARTESIAN_POINT('Ctrl Pts',(-20.7035927080245,-17.3166698912767,
-17.8549769484219));
#59740=CARTESIAN_POINT('Ctrl Pts',(-20.6498924684943,-17.2519932858418,
-17.8591466627423));
#59741=CARTESIAN_POINT('Ctrl Pts',(-20.5929827456749,-17.1899399538653,
-17.8633163770627));
#59742=CARTESIAN_POINT('Ctrl Pts',(-20.533156175962,-17.1308363460419,-17.867486091383));
#59743=CARTESIAN_POINT('Ctrl Pts',(-20.4733317351351,-17.0717348413785,
-17.8716556573271));
#59744=CARTESIAN_POINT('Ctrl Pts',(-20.4105909816463,-17.015583174876,-17.8758252232711));
#59745=CARTESIAN_POINT('Ctrl Pts',(-20.345263220069,-16.9626707573524,-17.8799947892152));
#59746=CARTESIAN_POINT('Ctrl Pts',(-20.2776386149851,-16.9078980045031,
-17.8843109519541));
#59747=CARTESIAN_POINT('Ctrl Pts',(-20.2072421084912,-16.8565968547186,
-17.888627114693));
#59748=CARTESIAN_POINT('Ctrl Pts',(-20.134474432863,-16.8090414462951,-17.8929432774319));
#59749=CARTESIAN_POINT('Ctrl Pts',(-20.0640771566148,-16.7630351502991,
-17.8971188416236));
#59750=CARTESIAN_POINT('Ctrl Pts',(-19.9914612509379,-16.7205345053977,
-17.9012944058153));
#59751=CARTESIAN_POINT('Ctrl Pts',(-19.9170156443953,-16.6817414276968,
-17.905469970007));
#59752=CARTESIAN_POINT('Ctrl Pts',(-19.8388099672436,-16.640989003863,-17.9098564320195));
#59753=CARTESIAN_POINT('Ctrl Pts',(-19.7585854263165,-16.604328771398,-17.9142428940321));
#59754=CARTESIAN_POINT('Ctrl Pts',(-19.6768157184724,-16.5719372863302,
-17.9186293560446));
#59755=CARTESIAN_POINT('Ctrl Pts',(-19.5950460106283,-16.5395458012623,
-17.9230158180572));
#59756=CARTESIAN_POINT('Ctrl Pts',(-19.5117317099373,-16.5114231770868,
-17.9274022800697));
#59757=CARTESIAN_POINT('Ctrl Pts',(-19.427361531773,-16.4876847226344,-17.9317887420823));
#59758=CARTESIAN_POINT('Ctrl Pts',(-19.3468694922175,-16.4650374240706,
-17.9359735770738));
#59759=CARTESIAN_POINT('Ctrl Pts',(-19.2651168916056,-16.446295797893,-17.9401584120653));
#59760=CARTESIAN_POINT('Ctrl Pts',(-19.1825176034853,-16.431596865705,-17.9443432470568));
#59761=CARTESIAN_POINT('Ctrl Pts',(-19.1000369486853,-16.4169190448749,
-17.9485220715744));
#59762=CARTESIAN_POINT('Ctrl Pts',(-19.0167124711285,-16.4062724641104,
-17.952700896092));
#59763=CARTESIAN_POINT('Ctrl Pts',(-18.9329723420367,-16.3997441336918,
-17.9568797206096));
#59764=CARTESIAN_POINT('Ctrl Pts',(-18.849333389066,-16.3932236909033,-17.9610534962066));
#59765=CARTESIAN_POINT('Ctrl Pts',(-18.7652802392365,-16.3908116415348,
-17.9652272718037));
#59766=CARTESIAN_POINT('Ctrl Pts',(-18.6812489272122,-16.392543549048,-17.9694010474007));
#59767=CARTESIAN_POINT('Ctrl Pts',(-18.5972730476301,-16.3942743140839,
-17.9735720697078));
#59768=CARTESIAN_POINT('Ctrl Pts',(-18.5133194358208,-16.4001435983923,
-17.9777430920148));
#59769=CARTESIAN_POINT('Ctrl Pts',(-18.4298258472946,-16.4101349200192,
-17.9819141143218));
#59770=CARTESIAN_POINT('Ctrl Pts',(-18.3463622898557,-16.4201226479539,
-17.9860836363899));
#59771=CARTESIAN_POINT('Ctrl Pts',(-18.2633588832482,-16.4342294129595,
-17.9902531584579));
#59772=CARTESIAN_POINT('Ctrl Pts',(-18.1812486084936,-16.4523868500931,
-17.994422680526));
#59773=CARTESIAN_POINT('Ctrl Pts',(-18.0991432365368,-16.4705432030475,
-17.9985919536322));
#59774=CARTESIAN_POINT('Ctrl Pts',(-18.0179313390458,-16.4927496461538,
-18.0027612267385));
#59775=CARTESIAN_POINT('Ctrl Pts',(-17.9380347007016,-16.5188869236485,
-18.0069304998447));
#59776=CARTESIAN_POINT('Ctrl Pts',(-17.8580775668942,-16.5450439915467,
-18.011102929806));
#59777=CARTESIAN_POINT('Ctrl Pts',(-17.7794381185581,-16.575137693535,-18.0152753597673));
#59778=CARTESIAN_POINT('Ctrl Pts',(-17.7025213244059,-16.6089994148967,
-18.0194477897286));
#59779=CARTESIAN_POINT('Ctrl Pts',(-17.6255715834959,-16.6428756406841,
-18.0236220069204));
#59780=CARTESIAN_POINT('Ctrl Pts',(-17.5503463787678,-16.6805228962677,
-18.0277962241122));
#59781=CARTESIAN_POINT('Ctrl Pts',(-17.4772271063916,-16.7217260495869,
-18.031970441304));
#59782=CARTESIAN_POINT('Ctrl Pts',(-17.4040091461644,-16.7629848141085,
-18.0361502923664));
#59783=CARTESIAN_POINT('Ctrl Pts',(-17.33290318242,-16.8078088135164,-18.0403301434289));
#59784=CARTESIAN_POINT('Ctrl Pts',(-17.2642621215538,-16.8559392736229,
-18.0445099944913));
#59785=CARTESIAN_POINT('Ctrl Pts',(-17.2338360617677,-16.877273737838,-18.0463627688616));
#59786=CARTESIAN_POINT('Ctrl Pts',(-17.2038938829713,-16.8992573253382,
-18.0482155432319));
#59787=CARTESIAN_POINT('Ctrl Pts',(-17.1744641548914,-16.9218650419685,
-18.0500683176022));
#59788=CARTESIAN_POINT('Ctrl Pts',(-17.1762220723153,-16.9241895431828,
-17.2500265390144));
#59789=CARTESIAN_POINT('Ctrl Pts',(-16.9304195468325,-17.1103102396675,
-17.2653209289013));
#59790=CARTESIAN_POINT('Ctrl Pts',(-16.1279941091616,-17.9709562098429,
-17.3230072543487));
#59791=CARTESIAN_POINT('Ctrl Pts',(-15.9988188303479,-20.2489482632501,
-17.4230855153565));
#59792=CARTESIAN_POINT('Ctrl Pts',(-18.3440265525621,-21.9538680082012,
-17.5502613220379));
#59793=CARTESIAN_POINT('Ctrl Pts',(-20.7784813047341,-21.0089843504267,
-17.6648027803286));
#59794=CARTESIAN_POINT('Ctrl Pts',(-21.2874612586096,-19.5488856065476,
-17.7369523030588));
#59795=CARTESIAN_POINT('Ctrl Pts',(-21.2923872581368,-18.9497870016169,
-17.7667098902285));
#59796=CARTESIAN_POINT('Origin',(-18.734,-18.952,1.76670989022851));
#59797=CARTESIAN_POINT('',(-17.1744641548914,-16.9218650419685,-16.4501666890971));
#59798=CARTESIAN_POINT('',(-17.1744641548915,-16.9218650419685,-16.5166303545479));
#59799=CARTESIAN_POINT('',(-17.1744641548914,-16.9218650419685,1.76670989022851));
#59800=CARTESIAN_POINT('',(-21.2942629985695,-18.9511644346814,-17.0332901097715));
#59801=CARTESIAN_POINT('Ctrl Pts',(-17.1744641548915,-16.9218650419685,
-16.5166303545479));
#59802=CARTESIAN_POINT('Ctrl Pts',(-17.1078974490003,-16.9730011319695,
-16.520815184908));
#59803=CARTESIAN_POINT('Ctrl Pts',(-17.0439434077443,-17.0273416600971,
-16.5250000152682));
#59804=CARTESIAN_POINT('Ctrl Pts',(-16.9829077605317,-17.0845750433086,
-16.5291848456283));
#59805=CARTESIAN_POINT('Ctrl Pts',(-16.9719424500703,-17.0948572610671,
-16.529936667985));
#59806=CARTESIAN_POINT('Ctrl Pts',(-16.9610712293328,-17.1052327594906,
-16.5306884903417));
#59807=CARTESIAN_POINT('Ctrl Pts',(-16.9502957329766,-17.115699619397,-16.5314403126983));
#59808=CARTESIAN_POINT('Ctrl Pts',(-16.8903194470162,-17.1739580385086,
-16.5356249470914));
#59809=CARTESIAN_POINT('Ctrl Pts',(-16.8330887583091,-17.2352663353223,
-16.5398095814844));
#59810=CARTESIAN_POINT('Ctrl Pts',(-16.7789298175348,-17.2993353087708,
-16.5439942158775));
#59811=CARTESIAN_POINT('Ctrl Pts',(-16.7248479653093,-17.3633130879657,
-16.5481728939614));
#59812=CARTESIAN_POINT('Ctrl Pts',(-16.6738294707906,-17.4300433902868,
-16.5523515720454));
#59813=CARTESIAN_POINT('Ctrl Pts',(-16.6261644175018,-17.4991995466843,
-16.5565302501293));
#59814=CARTESIAN_POINT('Ctrl Pts',(-16.577645002389,-17.5695952774836,-16.5607838280147));
#59815=CARTESIAN_POINT('Ctrl Pts',(-16.5326007777018,-17.6425043486949,
-16.5650374059002));
#59816=CARTESIAN_POINT('Ctrl Pts',(-16.4912954660574,-17.7175461234078,
-16.5692909837856));
#59817=CARTESIAN_POINT('Ctrl Pts',(-16.45079093848,-17.791133066886,-16.5734620977636));
#59818=CARTESIAN_POINT('Ctrl Pts',(-16.4138818774499,-17.8667703369927,
-16.5776332117415));
#59819=CARTESIAN_POINT('Ctrl Pts',(-16.3807728287042,-17.9440704983605,
-16.5818043257195));
#59820=CARTESIAN_POINT('Ctrl Pts',(-16.3476748900196,-18.0213447209125,
-16.5859740400399));
#59821=CARTESIAN_POINT('Ctrl Pts',(-16.318374612164,-18.1002803040064,-16.5901437543602));
#59822=CARTESIAN_POINT('Ctrl Pts',(-16.2930292165598,-18.1804679952255,
-16.5943134686806));
#59823=CARTESIAN_POINT('Ctrl Pts',(-16.2676847228536,-18.2606528330224,
-16.5984830346246));
#59824=CARTESIAN_POINT('Ctrl Pts',(-16.2462949694201,-18.3420892514569,
-16.6026526005687));
#59825=CARTESIAN_POINT('Ctrl Pts',(-16.2289674972205,-18.4243522386873,
-16.6068221665127));
#59826=CARTESIAN_POINT('Ctrl Pts',(-16.2110308124741,-18.5095074910663,
-16.6111383292517));
#59827=CARTESIAN_POINT('Ctrl Pts',(-16.1974474922546,-18.5955480019176,
-16.6154544919906));
#59828=CARTESIAN_POINT('Ctrl Pts',(-16.1882789321129,-18.6819921399002,
-16.6197706547295));
#59829=CARTESIAN_POINT('Ctrl Pts',(-16.1794090368535,-18.7656203691804,
-16.6239462189212));
#59830=CARTESIAN_POINT('Ctrl Pts',(-16.1746706763875,-18.8496258601583,
-16.6281217831129));
#59831=CARTESIAN_POINT('Ctrl Pts',(-16.1740663387713,-18.9335704012975,
-16.6322973473045));
#59832=CARTESIAN_POINT('Ctrl Pts',(-16.1734314774988,-19.0217547816503,
-16.6366838093171));
#59833=CARTESIAN_POINT('Ctrl Pts',(-16.1773592072922,-19.1098713098955,
-16.6410702713296));
#59834=CARTESIAN_POINT('Ctrl Pts',(-16.1857908120614,-19.1974178773141,
-16.6454567333422));
#59835=CARTESIAN_POINT('Ctrl Pts',(-16.1942224168306,-19.2849644447327,
-16.6498431953547));
#59836=CARTESIAN_POINT('Ctrl Pts',(-16.2071577359856,-19.3719404886095,
-16.6542296573672));
#59837=CARTESIAN_POINT('Ctrl Pts',(-16.2244766916358,-19.4578584434176,
-16.6586161193798));
#59838=CARTESIAN_POINT('Ctrl Pts',(-16.2409987764638,-19.5398231857641,
-16.6628007537728));
#59839=CARTESIAN_POINT('Ctrl Pts',(-16.2615714655045,-19.6211301562753,
-16.6669853881659));
#59840=CARTESIAN_POINT('Ctrl Pts',(-16.2861281256043,-19.7013485747917,
-16.6711700225589));
#59841=CARTESIAN_POINT('Ctrl Pts',(-16.3106498323379,-19.7814528123184,
-16.6753487006429));
#59842=CARTESIAN_POINT('Ctrl Pts',(-16.3391441128499,-19.8604711393629,
-16.6795273787268));
#59843=CARTESIAN_POINT('Ctrl Pts',(-16.3714933068752,-19.9379828218282,
-16.6837060568108));
#59844=CARTESIAN_POINT('Ctrl Pts',(-16.4044223369544,-20.0168838454952,
-16.6879596346962));
#59845=CARTESIAN_POINT('Ctrl Pts',(-16.4413457432406,-20.0942232074709,
-16.6922132125816));
#59846=CARTESIAN_POINT('Ctrl Pts',(-16.48208621838,-20.1695731272288,-16.6964667904671));
#59847=CARTESIAN_POINT('Ctrl Pts',(-16.5220368599103,-20.2434622417589,
-16.700637904445));
#59848=CARTESIAN_POINT('Ctrl Pts',(-16.5656576595127,-20.3154379408342,
-16.704809018423));
#59849=CARTESIAN_POINT('Ctrl Pts',(-16.6127335620839,-20.3851185224435,
-16.7089801324009));
#59850=CARTESIAN_POINT('Ctrl Pts',(-16.6597936678814,-20.4547757220608,
-16.7131498467213));
#59851=CARTESIAN_POINT('Ctrl Pts',(-16.7103063167569,-20.5221389528648,
-16.7173195610417));
#59852=CARTESIAN_POINT('Ctrl Pts',(-16.7640124931678,-20.5868544959491,
-16.721489275362));
#59853=CARTESIAN_POINT('Ctrl Pts',(-16.8177167584824,-20.6515677361767,
-16.7256588413061));
#59854=CARTESIAN_POINT('Ctrl Pts',(-16.8746140309484,-20.713633122547,-16.7298284072501));
#59855=CARTESIAN_POINT('Ctrl Pts',(-16.934405152749,-20.7727301792818,-16.7339979731942));
#59856=CARTESIAN_POINT('Ctrl Pts',(-16.9962984566318,-20.8339050156273,
-16.7383141359331));
#59857=CARTESIAN_POINT('Ctrl Pts',(-17.061292516445,-20.8918985349615,-16.742630298672));
#59858=CARTESIAN_POINT('Ctrl Pts',(-17.1290155886979,-20.9463984154319,
-16.7469464614109));
#59859=CARTESIAN_POINT('Ctrl Pts',(-17.1945325889952,-20.9991229680282,
-16.7511220256026));
#59860=CARTESIAN_POINT('Ctrl Pts',(-17.2626031281003,-21.0485777582944,
-16.7552975897943));
#59861=CARTESIAN_POINT('Ctrl Pts',(-17.3328600861971,-21.0945234985756,
-16.759473153986));
#59862=CARTESIAN_POINT('Ctrl Pts',(-17.4066655562275,-21.1427898489728,
-16.7638596159985));
#59863=CARTESIAN_POINT('Ctrl Pts',(-17.4828836173808,-21.1871830552703,
-16.7682460780111));
#59864=CARTESIAN_POINT('Ctrl Pts',(-17.5610602937788,-21.2274807064816,
-16.7726325400236));
#59865=CARTESIAN_POINT('Ctrl Pts',(-17.6392369701769,-21.2677783576928,
-16.7770190020362));
#59866=CARTESIAN_POINT('Ctrl Pts',(-17.719371701741,-21.3039802842616,-16.7814054640487));
#59867=CARTESIAN_POINT('Ctrl Pts',(-17.8009895271371,-21.3359235427186,
-16.7857919260613));
#59868=CARTESIAN_POINT('Ctrl Pts',(-17.8788519954,-21.3663970445028,-16.7899765604543));
#59869=CARTESIAN_POINT('Ctrl Pts',(-17.9583538968788,-21.3931085897472,
-16.7941611948473));
#59870=CARTESIAN_POINT('Ctrl Pts',(-18.0390969463692,-21.4158810332592,
-16.7983458292404));
#59871=CARTESIAN_POINT('Ctrl Pts',(-18.1197250681227,-21.4386210630166,
-16.8025245073243));
#59872=CARTESIAN_POINT('Ctrl Pts',(-18.2015903898501,-21.4574330041517,
-16.8067031854083));
#59873=CARTESIAN_POINT('Ctrl Pts',(-18.2842754534887,-21.4721880549406,
-16.8108818634922));
#59874=CARTESIAN_POINT('Ctrl Pts',(-18.3684425874682,-21.4872075794106,
-16.8151354413777));
#59875=CARTESIAN_POINT('Ctrl Pts',(-18.4534586911853,-21.49802316776,-16.8193890192631));
#59876=CARTESIAN_POINT('Ctrl Pts',(-18.538868095807,-21.5045523579284,-16.8236425971485));
#59877=CARTESIAN_POINT('Ctrl Pts',(-18.6226216724574,-21.5109549670048,
-16.8278137111265));
#59878=CARTESIAN_POINT('Ctrl Pts',(-18.7067529564692,-21.5132358584627,
-16.8319848251044));
#59879=CARTESIAN_POINT('Ctrl Pts',(-18.7908245916082,-21.5113692515517,
-16.8361559390824));
#59880=CARTESIAN_POINT('Ctrl Pts',(-18.8748680156982,-21.5095032709988,
-16.8403256534027));
#59881=CARTESIAN_POINT('Ctrl Pts',(-18.9588513711302,-21.503492566284,-16.8444953677231));
#59882=CARTESIAN_POINT('Ctrl Pts',(-19.0423370360803,-21.4933634671533,
-16.8486650820435));
#59883=CARTESIAN_POINT('Ctrl Pts',(-19.1258197302523,-21.4832347284594,
-16.8528346479875));
#59884=CARTESIAN_POINT('Ctrl Pts',(-19.2088043125731,-21.4689879429832,
-16.8570042139316));
#59885=CARTESIAN_POINT('Ctrl Pts',(-19.2908593851774,-21.4507011876453,
-16.8611737798756));
#59886=CARTESIAN_POINT('Ctrl Pts',(-19.3757994129086,-21.4317714925488,
-16.8654899426145));
#59887=CARTESIAN_POINT('Ctrl Pts',(-19.4597428368621,-21.4085125658604,
-16.8698061053535));
#59888=CARTESIAN_POINT('Ctrl Pts',(-19.5422258260852,-21.381067931131,-16.8741222680924));
#59889=CARTESIAN_POINT('Ctrl Pts',(-19.6220219406102,-21.3545173024912,
-16.8782978322841));
#59890=CARTESIAN_POINT('Ctrl Pts',(-19.7004508845915,-21.3240496914869,
-16.8824733964757));
#59891=CARTESIAN_POINT('Ctrl Pts',(-19.7771127399862,-21.2898442659165,
-16.8866489606674));
#59892=CARTESIAN_POINT('Ctrl Pts',(-19.8576466034505,-21.2539112056161,
-16.8910354226799));
#59893=CARTESIAN_POINT('Ctrl Pts',(-19.9362296554817,-21.2138530785412,
-16.8954218846925));
#59894=CARTESIAN_POINT('Ctrl Pts',(-20.0124291551049,-21.169931219713,-16.899808346705));
#59895=CARTESIAN_POINT('Ctrl Pts',(-20.0886286547281,-21.1260093608849,
-16.9041948087175));
#59896=CARTESIAN_POINT('Ctrl Pts',(-20.1624441562134,-21.0782241494638,
-16.9085812707301));
#59897=CARTESIAN_POINT('Ctrl Pts',(-20.2334815623277,-21.0268867545577,
-16.9129677327426));
#59898=CARTESIAN_POINT('Ctrl Pts',(-20.3007008312569,-20.9783086554537,
-16.9171184300413));
#59899=CARTESIAN_POINT('Ctrl Pts',(-20.3656920487852,-20.9263629083339,
-16.9212691273401));
#59900=CARTESIAN_POINT('Ctrl Pts',(-20.4280939407346,-20.8712826055499,
-16.9254198246388));
#59901=CARTESIAN_POINT('Ctrl Pts',(-20.4904067758306,-20.816280910614,-16.9295645982704));
#59902=CARTESIAN_POINT('Ctrl Pts',(-20.5501372744547,-20.758153849065,-16.9337093719019));
#59903=CARTESIAN_POINT('Ctrl Pts',(-20.6069541187602,-20.6971770308536,
-16.9378541455334));
#59904=CARTESIAN_POINT('Ctrl Pts',(-20.6637057912846,-20.636270156123,-16.9419941649009));
#59905=CARTESIAN_POINT('Ctrl Pts',(-20.7175501324576,-20.5725203603438,
-16.9461341842684));
#59906=CARTESIAN_POINT('Ctrl Pts',(-20.7681909845743,-20.5062416280221,
-16.9502742036359));
#59907=CARTESIAN_POINT('Ctrl Pts',(-20.8188004163148,-20.4400040186795,
-16.9544116543072));
#59908=CARTESIAN_POINT('Ctrl Pts',(-20.8662100198436,-20.3712409577298,
-16.9585491049784));
#59909=CARTESIAN_POINT('Ctrl Pts',(-20.9101632231194,-20.3003002730633,
-16.9626865556497));
#59910=CARTESIAN_POINT('Ctrl Pts',(-20.9541028768145,-20.2293814574863,
-16.9668227308571));
#59911=CARTESIAN_POINT('Ctrl Pts',(-20.9945879994369,-20.1562867489274,
-16.9709589060645));
#59912=CARTESIAN_POINT('Ctrl Pts',(-21.0314055962389,-20.0813925475095,
-16.9750950812719));
#59913=CARTESIAN_POINT('Ctrl Pts',(-21.0682233367814,-20.0064980536955,
-16.9792312726275));
#59914=CARTESIAN_POINT('Ctrl Pts',(-21.101373318238,-19.9298044742117,-16.983367463983));
#59915=CARTESIAN_POINT('Ctrl Pts',(-21.1306893947114,-19.8517110343203,
-16.9875036553386));
#59916=CARTESIAN_POINT('Ctrl Pts',(-21.1600333335746,-19.773543373383,-16.9916437777855));
#59917=CARTESIAN_POINT('Ctrl Pts',(-21.1855359272153,-19.6939736349119,
-16.9957839002324));
#59918=CARTESIAN_POINT('Ctrl Pts',(-21.2070801670876,-19.6134185415892,
-16.9999240226793));
#59919=CARTESIAN_POINT('Ctrl Pts',(-21.2286351815299,-19.5328231615589,
-17.0040662156583));
#59920=CARTESIAN_POINT('Ctrl Pts',(-21.2462278030767,-19.4512419037244,
-17.0082084086373));
#59921=CARTESIAN_POINT('Ctrl Pts',(-21.2597921942375,-19.3691016561091,
-17.0123506016163));
#59922=CARTESIAN_POINT('Ctrl Pts',(-21.2733789861849,-19.286825758752,-17.016499635181));
#59923=CARTESIAN_POINT('Ctrl Pts',(-21.2829242114339,-19.2039894937101,
-17.0206486687457));
#59924=CARTESIAN_POINT('Ctrl Pts',(-21.2884139728529,-19.1210244221818,
-17.0247977023105));
#59925=CARTESIAN_POINT('Ctrl Pts',(-21.2921595270972,-19.0644190158498,
-17.0276285047975));
#59926=CARTESIAN_POINT('Ctrl Pts',(-21.2940183320645,-19.0077536994293,
-17.0304593072845));
#59927=CARTESIAN_POINT('Ctrl Pts',(-21.2939998636668,-18.9511645205579,
-17.0332901097715));
#59928=CARTESIAN_POINT('Ctrl Pts',(-21.2979001731334,-18.9511632476561,
-17.0332901097715));
#59929=CARTESIAN_POINT('Ctrl Pts',(-21.2980948808476,-18.9054257555603,
-17.0355745863224));
#59930=CARTESIAN_POINT('Ctrl Pts',(-21.2762380388006,-18.0111494605167,
-17.0802509984337));
#59931=CARTESIAN_POINT('Ctrl Pts',(-20.2331955662249,-16.3222274596702,
-17.1673193461055));
#59932=CARTESIAN_POINT('Ctrl Pts',(-18.131091639517,-16.2828821145566,-17.2595383994549));
#59933=CARTESIAN_POINT('Ctrl Pts',(-17.2909884432664,-16.8286169939874,
-17.3093655172438));
#59934=CARTESIAN_POINT('Ctrl Pts',(-17.1735447326512,-16.9206895600706,
-17.3168006994722));
#59935=CARTESIAN_POINT('',(-21.2938494935628,-18.9531967451209,-16.9667098397524));
#59936=CARTESIAN_POINT('Ctrl Pts',(-21.290325207156,-18.9531940791588,-16.9667098902285));
#59937=CARTESIAN_POINT('Ctrl Pts',(-21.2882101978943,-18.4498774972589,
-16.9916592919231));
#59938=CARTESIAN_POINT('Ctrl Pts',(-20.9008594754591,-17.088363994255,-17.0590006291781));
#59939=CARTESIAN_POINT('Ctrl Pts',(-18.9946005776491,-16.0873964875648,
-17.1534395121067));
#59940=CARTESIAN_POINT('Ctrl Pts',(-17.611718042421,-16.5944337234933,-17.2229289933409));
#59941=CARTESIAN_POINT('Ctrl Pts',(-17.1762220723153,-16.9241895431828,
-17.2500265390144));
#59942=CARTESIAN_POINT('Ctrl Pts',(-17.1744641548914,-16.9218650419685,
-16.4501666890971));
#59943=CARTESIAN_POINT('Ctrl Pts',(-17.1078206357512,-16.9730601393841,
-16.4543369048848));
#59944=CARTESIAN_POINT('Ctrl Pts',(-17.0436639638458,-17.0275684362512,
-16.4585071206726));
#59945=CARTESIAN_POINT('Ctrl Pts',(-16.9823340376993,-17.0851131912949,
-16.4626773364604));
#59946=CARTESIAN_POINT('Ctrl Pts',(-16.9210149346286,-17.1426477912433,
-16.4668468163177));
#59947=CARTESIAN_POINT('Ctrl Pts',(-16.86252192151,-17.2032174699326,-16.471016296175));
#59948=CARTESIAN_POINT('Ctrl Pts',(-16.8071597460482,-17.2665070051314,
-16.4751857760323));
#59949=CARTESIAN_POINT('Ctrl Pts',(-16.7517907333809,-17.3298043565614,
-16.4793557708186));
#59950=CARTESIAN_POINT('Ctrl Pts',(-16.6995536280125,-17.395821884368,-16.483525765605));
#59951=CARTESIAN_POINT('Ctrl Pts',(-16.6507135127919,-17.4642105618684,
-16.4876957603913));
#59952=CARTESIAN_POINT('Ctrl Pts',(-16.601820905061,-17.5326727423353,-16.4918702370158));
#59953=CARTESIAN_POINT('Ctrl Pts',(-16.5563328438427,-17.6035107849438,
-16.4960447136403));
#59954=CARTESIAN_POINT('Ctrl Pts',(-16.5144712872111,-17.6763463271305,
-16.5002191902648));
#59955=CARTESIAN_POINT('Ctrl Pts',(-16.4725853040748,-17.7492243693543,
-16.504396102725));
#59956=CARTESIAN_POINT('Ctrl Pts',(-16.4343302474926,-17.8241018219044,
-16.5085730151852));
#59957=CARTESIAN_POINT('Ctrl Pts',(-16.3998811614755,-17.9005775122982,
-16.5127499276454));
#59958=CARTESIAN_POINT('Ctrl Pts',(-16.3653738366734,-17.9771824906297,
-16.516933901492));
#59959=CARTESIAN_POINT('Ctrl Pts',(-16.334685497607,-18.0553906735663,-16.5211178753385));
#59960=CARTESIAN_POINT('Ctrl Pts',(-16.3079421752585,-18.1347831187435,
-16.5253018491851));
#59961=CARTESIAN_POINT('Ctrl Pts',(-16.2918495927868,-18.182556894006,-16.5278195223189));
#59962=CARTESIAN_POINT('Ctrl Pts',(-16.2771845020012,-18.2307592098647,
-16.5303371954527));
#59963=CARTESIAN_POINT('Ctrl Pts',(-16.2639654295305,-18.2792970784325,
-16.5328548685865));
#59964=CARTESIAN_POINT('Ctrl Pts',(-16.2419939573157,-18.3599720602031,
-16.5370395029795));
#59965=CARTESIAN_POINT('Ctrl Pts',(-16.223938199736,-18.4418747378536,-16.5412241373726));
#59966=CARTESIAN_POINT('Ctrl Pts',(-16.2099316900943,-18.5245901651461,
-16.5454087717656));
#59967=CARTESIAN_POINT('Ctrl Pts',(-16.1959451169854,-18.6071878572661,
-16.5495874498496));
#59968=CARTESIAN_POINT('Ctrl Pts',(-16.1859964196337,-18.6905955514665,
-16.5537661279335));
#59969=CARTESIAN_POINT('Ctrl Pts',(-16.18016901464,-18.7743844088627,-16.5579448060175));
#59970=CARTESIAN_POINT('Ctrl Pts',(-16.1742371575999,-18.8596751213096,
-16.5621983839029));
#59971=CARTESIAN_POINT('Ctrl Pts',(-16.1725759211884,-18.9453603308628,
-16.5664519617884));
#59972=CARTESIAN_POINT('Ctrl Pts',(-16.1752185615464,-19.0309781629659,
-16.5707055396738));
#59973=CARTESIAN_POINT('Ctrl Pts',(-16.1778099691644,-19.1149361263243,
-16.5748766536517));
#59974=CARTESIAN_POINT('Ctrl Pts',(-16.1845398497979,-19.1988288204161,
-16.5790477676297));
#59975=CARTESIAN_POINT('Ctrl Pts',(-16.1953870618678,-19.2822186402182,
-16.5832188816076));
#59976=CARTESIAN_POINT('Ctrl Pts',(-16.2062306340508,-19.3655804777609,
-16.587388595928));
#59977=CARTESIAN_POINT('Ctrl Pts',(-16.2211887344791,-19.4484393203328,
-16.5915583102484));
#59978=CARTESIAN_POINT('Ctrl Pts',(-16.2401883815476,-19.5303628719688,
-16.5957280245688));
#59979=CARTESIAN_POINT('Ctrl Pts',(-16.2591873525272,-19.6122835084131,
-16.5998975905128));
#59980=CARTESIAN_POINT('Ctrl Pts',(-16.2822274794425,-19.6932684721477,
-16.6040671564568));
#59981=CARTESIAN_POINT('Ctrl Pts',(-16.3091849959465,-19.7728971897364,
-16.6082367224009));
#59982=CARTESIAN_POINT('Ctrl Pts',(-16.3370903054751,-19.8553255548029,
-16.6125528851398));
#59983=CARTESIAN_POINT('Ctrl Pts',(-16.3691934316989,-19.9363000284499,
-16.6168690478787));
#59984=CARTESIAN_POINT('Ctrl Pts',(-16.4053020683427,-20.015374789571,-16.6211852106176));
#59985=CARTESIAN_POINT('Ctrl Pts',(-16.4402344699458,-20.0918736986657,
-16.6253607748093));
#59986=CARTESIAN_POINT('Ctrl Pts',(-16.4789151719815,-20.1665943642433,
-16.629536339001));
#59987=CARTESIAN_POINT('Ctrl Pts',(-16.5211232637328,-20.2391583236289,
-16.6337119031927));
#59988=CARTESIAN_POINT('Ctrl Pts',(-16.5654631858582,-20.3153873160987,
-16.6380983652052));
#59989=CARTESIAN_POINT('Ctrl Pts',(-16.6136958800291,-20.3892355173248,
-16.6424848272177));
#59990=CARTESIAN_POINT('Ctrl Pts',(-16.6655152292138,-20.460300617591,-16.6468712892303));
#59991=CARTESIAN_POINT('Ctrl Pts',(-16.7173345783985,-20.5313657178572,
-16.6512577512428));
#59992=CARTESIAN_POINT('Ctrl Pts',(-16.7727401579416,-20.5996473145404,
-16.6556442132554));
#59993=CARTESIAN_POINT('Ctrl Pts',(-16.8313804354228,-20.664786849695,-16.6600306752679));
#59994=CARTESIAN_POINT('Ctrl Pts',(-16.8873225868114,-20.7269292182772,
-16.664215309661));
#59995=CARTESIAN_POINT('Ctrl Pts',(-16.9464165382123,-20.7864436190212,
-16.668399944054));
#59996=CARTESIAN_POINT('Ctrl Pts',(-17.0083856645506,-20.842993169023,-16.6725845784471));
#59997=CARTESIAN_POINT('Ctrl Pts',(-17.0702665855077,-20.8994622277397,
-16.676763256531));
#59998=CARTESIAN_POINT('Ctrl Pts',(-17.1350142155918,-20.9529745107155,
-16.6809419346149));
#59999=CARTESIAN_POINT('Ctrl Pts',(-17.2023131209901,-21.0032277554355,
-16.6851206126989));
#60000=CARTESIAN_POINT('Ctrl Pts',(-17.2708183109008,-21.0543817534507,
-16.6893741905843));
#60001=CARTESIAN_POINT('Ctrl Pts',(-17.3419668163949,-21.102158369159,-16.6936277684697));
#60002=CARTESIAN_POINT('Ctrl Pts',(-17.4153882749822,-21.1462796354716,
-16.6978813463552));
#60003=CARTESIAN_POINT('Ctrl Pts',(-17.4873863153245,-21.1895455249412,
-16.7020524603331));
#60004=CARTESIAN_POINT('Ctrl Pts',(-17.5615695514937,-21.2292962845163,
-16.7062235743111));
#60005=CARTESIAN_POINT('Ctrl Pts',(-17.637558583382,-21.26531282362,-16.710394688289));
#60006=CARTESIAN_POINT('Ctrl Pts',(-17.7135221164167,-21.3013172770261,
-16.7145644026094));
#60007=CARTESIAN_POINT('Ctrl Pts',(-17.7912898263826,-21.3335898016786,
-16.7187341169298));
#60008=CARTESIAN_POINT('Ctrl Pts',(-17.8704587172267,-21.3619577699508,
-16.7229038312502));
#60009=CARTESIAN_POINT('Ctrl Pts',(-17.9496247909019,-21.3903247287689,
-16.7270733971942));
#60010=CARTESIAN_POINT('Ctrl Pts',(-18.030191512963,-21.4147872530805,-16.7312429631382));
#60011=CARTESIAN_POINT('Ctrl Pts',(-18.1117382553313,-21.4352217623728,
-16.7354125290823));
#60012=CARTESIAN_POINT('Ctrl Pts',(-18.1961520805624,-21.4563747238031,
-16.7397286918212));
#60013=CARTESIAN_POINT('Ctrl Pts',(-18.2816156117522,-21.4732110218616,
-16.7440448545601));
#60014=CARTESIAN_POINT('Ctrl Pts',(-18.3676498921637,-21.4856510411831,
-16.748361017299));
#60015=CARTESIAN_POINT('Ctrl Pts',(-18.4508816149399,-21.4976858281837,
-16.7525365814907));
#60016=CARTESIAN_POINT('Ctrl Pts',(-18.5346470002632,-21.5056063582132,
-16.7567121456824));
#60017=CARTESIAN_POINT('Ctrl Pts',(-18.6185082461362,-21.5093935275568,
-16.7608877098741));
#60018=CARTESIAN_POINT('Ctrl Pts',(-18.7066051241771,-21.5133719778208,
-16.7652741718866));
#60019=CARTESIAN_POINT('Ctrl Pts',(-18.7948072172264,-21.5127885456943,
-16.7696606338992));
#60020=CARTESIAN_POINT('Ctrl Pts',(-18.8826105511363,-21.5076828645376,
-16.7740470959117));
#60021=CARTESIAN_POINT('Ctrl Pts',(-18.9704138850463,-21.5025771833809,
-16.7784335579242));
#60022=CARTESIAN_POINT('Ctrl Pts',(-19.0578178914167,-21.4929493923299,
-16.7828200199368));
#60023=CARTESIAN_POINT('Ctrl Pts',(-19.1443308019265,-21.4789009939035,
-16.7872064819493));
#60024=CARTESIAN_POINT('Ctrl Pts',(-19.226863125181,-21.4654989831134,-16.7913911163424));
#60025=CARTESIAN_POINT('Ctrl Pts',(-19.3088917529366,-21.4480243381486,
-16.7955757507354));
#60026=CARTESIAN_POINT('Ctrl Pts',(-19.3899836880773,-21.4265273085938,
-16.7997603851285));
#60027=CARTESIAN_POINT('Ctrl Pts',(-19.4709601988853,-21.4050608773999,
-16.8039390632124));
#60028=CARTESIAN_POINT('Ctrl Pts',(-19.5510022244941,-21.3795835508679,
-16.8081177412964));
#60029=CARTESIAN_POINT('Ctrl Pts',(-19.6296848716226,-21.3501969499494,
-16.8122964193803));
#60030=CARTESIAN_POINT('Ctrl Pts',(-19.7097778486527,-21.3202836153291,
-16.8165499972657));
#60031=CARTESIAN_POINT('Ctrl Pts',(-19.7884617582359,-21.2863195576314,
-16.8208035751512));
#60032=CARTESIAN_POINT('Ctrl Pts',(-19.8653024038482,-21.2484657347862,
-16.8250571530366));
#60033=CARTESIAN_POINT('Ctrl Pts',(-19.9406533436032,-21.2113457821626,
-16.8292282670146));
#60034=CARTESIAN_POINT('Ctrl Pts',(-20.0142314204538,-21.1704857525211,
-16.8333993809925));
#60035=CARTESIAN_POINT('Ctrl Pts',(-20.0856470518143,-21.1260860717372,
-16.8375704949705));
#60036=CARTESIAN_POINT('Ctrl Pts',(-20.15703871897,-21.081701289695,-16.8417402092909));
#60037=CARTESIAN_POINT('Ctrl Pts',(-20.2262689913883,-21.0337794581181,
-16.8459099236112));
#60038=CARTESIAN_POINT('Ctrl Pts',(-20.2929745824341,-20.9825659928514,
-16.8500796379316));
#60039=CARTESIAN_POINT('Ctrl Pts',(-20.3596777998085,-20.9313543499797,
-16.8542492038756));
#60040=CARTESIAN_POINT('Ctrl Pts',(-20.4238561500589,-20.8768515871279,
-16.8584187698197));
#60041=CARTESIAN_POINT('Ctrl Pts',(-20.4851780435301,-20.8193444941569,
-16.8625883357637));
#60042=CARTESIAN_POINT('Ctrl Pts',(-20.5486559391271,-20.7598155227396,
-16.8669044985026));
#60043=CARTESIAN_POINT('Ctrl Pts',(-20.6090723898813,-20.6970673867193,
-16.8712206612416));
#60044=CARTESIAN_POINT('Ctrl Pts',(-20.6661012016726,-20.6314597186284,
-16.8755368239805));
#60045=CARTESIAN_POINT('Ctrl Pts',(-20.7212723059182,-20.5679892134248,
-16.8797123881722));
#60046=CARTESIAN_POINT('Ctrl Pts',(-20.7732728325614,-20.5018430132075,
-16.8838879523639));
#60047=CARTESIAN_POINT('Ctrl Pts',(-20.8218497444836,-20.4333788996943,
-16.8880635165556));
#60048=CARTESIAN_POINT('Ctrl Pts',(-20.8728801607463,-20.3614568265658,
-16.8924499785681));
#60049=CARTESIAN_POINT('Ctrl Pts',(-20.9201317067406,-20.2869770238507,
-16.8968364405806));
#60050=CARTESIAN_POINT('Ctrl Pts',(-20.9633649162028,-20.2103847068381,
-16.9012229025932));
#60051=CARTESIAN_POINT('Ctrl Pts',(-21.0065981256651,-20.1337923898255,
-16.9056093646057));
#60052=CARTESIAN_POINT('Ctrl Pts',(-21.0458128079223,-20.0550881117615,
-16.9099958266183));
#60053=CARTESIAN_POINT('Ctrl Pts',(-21.0808281256648,-19.9747403133684,
-16.9143822886308));
#60054=CARTESIAN_POINT('Ctrl Pts',(-21.1176528956138,-19.890240460661,-16.9189954255354));
#60055=CARTESIAN_POINT('Ctrl Pts',(-21.1499518315865,-19.8036540013275,
-16.9236085624399));
#60056=CARTESIAN_POINT('Ctrl Pts',(-21.1775079602931,-19.7154584782318,
-16.9282216993445));
#60057=CARTESIAN_POINT('Ctrl Pts',(-21.2049852187145,-19.6275153855896,
-16.9328216326736));
#60058=CARTESIAN_POINT('Ctrl Pts',(-21.2277466226989,-19.5379726851093,
-16.9374215660027));
#60059=CARTESIAN_POINT('Ctrl Pts',(-21.2456232056933,-19.4473270360306,
-16.9420214993319));
#60060=CARTESIAN_POINT('Ctrl Pts',(-21.2634117418665,-19.3571278403517,
-16.9465987767929));
#60061=CARTESIAN_POINT('Ctrl Pts',(-21.2763633328304,-19.2658368103367,
-16.9511760542538));
#60062=CARTESIAN_POINT('Ctrl Pts',(-21.2843593339855,-19.1739623111095,
-16.9557533317148));
#60063=CARTESIAN_POINT('Ctrl Pts',(-21.2907392715843,-19.1006564722762,
-16.9594055003435));
#60064=CARTESIAN_POINT('Ctrl Pts',(-21.2939652250916,-19.0269796001108,
-16.9630576689721));
#60065=CARTESIAN_POINT('Ctrl Pts',(-21.2939997202205,-18.9531968587605,
-16.9667098376008));
#60066=CARTESIAN_POINT('Origin',(-18.734,-18.952,1.76670989022851));
#60067=CARTESIAN_POINT('',(-17.1721129765924,-16.9188350422745,-15.6501589808892));
#60068=CARTESIAN_POINT('',(-17.1744641548914,-16.9218650419685,-15.7166572062078));
#60069=CARTESIAN_POINT('',(-17.1744641548914,-16.9218650419685,1.76670989022851));
#60070=CARTESIAN_POINT('',(-21.2939992944986,-18.9500994299065,-16.2332901098004));
#60071=CARTESIAN_POINT('Ctrl Pts',(-17.1744641548914,-16.9218650419685,
-15.7166572062078));
#60072=CARTESIAN_POINT('Ctrl Pts',(-17.1055401828173,-16.9748119677931,
-15.7209678950746));
#60073=CARTESIAN_POINT('Ctrl Pts',(-17.0393402583663,-17.0312538502349,
-15.7252785839415));
#60074=CARTESIAN_POINT('Ctrl Pts',(-16.9762229031562,-17.0908660236803,
-15.7295892728083));
#60075=CARTESIAN_POINT('Ctrl Pts',(-16.9150839105399,-17.1486097016275,
-15.7337648466093));
#60076=CARTESIAN_POINT('Ctrl Pts',(-16.8568373862815,-17.2093274875522,
-15.7379404204102));
#60077=CARTESIAN_POINT('Ctrl Pts',(-16.8017702605312,-17.2726881665657,
-15.7421159942111));
#60078=CARTESIAN_POINT('Ctrl Pts',(-16.7440303051251,-17.339124224938,-15.7464942406109));
#60079=CARTESIAN_POINT('Ctrl Pts',(-16.6897865650317,-17.4084657801725,
-15.7508724870107));
#60080=CARTESIAN_POINT('Ctrl Pts',(-16.6393195124585,-17.4802956631466,
-15.7552507334104));
#60081=CARTESIAN_POINT('Ctrl Pts',(-16.5888524598854,-17.5521255461208,
-15.7596289798102));
#60082=CARTESIAN_POINT('Ctrl Pts',(-16.5421623367065,-17.6264432299862,
-15.76400722621));
#60083=CARTESIAN_POINT('Ctrl Pts',(-16.4994739740979,-17.7028028820213,
-15.7683854726097));
#60084=CARTESIAN_POINT('Ctrl Pts',(-16.458673348906,-17.7757858064552,-15.7725701070028));
#60085=CARTESIAN_POINT('Ctrl Pts',(-16.4213761508428,-17.8509055642072,
-15.7767547413958));
#60086=CARTESIAN_POINT('Ctrl Pts',(-16.3878121523981,-17.9277917283261,
-15.7809393757889));
#60087=CARTESIAN_POINT('Ctrl Pts',(-16.3542959281507,-18.0045684545072,
-15.7851180538728));
#60088=CARTESIAN_POINT('Ctrl Pts',(-16.3245025312235,-18.0831061749373,
-15.7892967319568));
#60089=CARTESIAN_POINT('Ctrl Pts',(-16.2986164546583,-18.163008880228,-15.7934754100407));
#60090=CARTESIAN_POINT('Ctrl Pts',(-16.2722663887748,-18.2443437840859,
-15.7977289879262));
#60091=CARTESIAN_POINT('Ctrl Pts',(-16.2499653337518,-18.3270926679903,
-15.8019825658116));
#60092=CARTESIAN_POINT('Ctrl Pts',(-16.2318570828657,-18.4108153529206,
-15.806236143697));
#60093=CARTESIAN_POINT('Ctrl Pts',(-16.2140998957582,-18.4929149102322,
-15.810407257675));
#60094=CARTESIAN_POINT('Ctrl Pts',(-16.2003744938965,-18.5759503771067,
-15.8145783716529));
#60095=CARTESIAN_POINT('Ctrl Pts',(-16.1907660223745,-18.6594919914754,
-15.8187494856309));
#60096=CARTESIAN_POINT('Ctrl Pts',(-16.1811607750679,-18.7430055726484,
-15.8229191999512));
#60097=CARTESIAN_POINT('Ctrl Pts',(-16.1756697669882,-18.8270245073658,
-15.8270889142716));
#60098=CARTESIAN_POINT('Ctrl Pts',(-16.1743265551335,-18.9111116685931,
-15.831258628592));
#60099=CARTESIAN_POINT('Ctrl Pts',(-16.172983391076,-18.9951958376385,-15.835428194536));
#60100=CARTESIAN_POINT('Ctrl Pts',(-16.1757877362795,-19.079347768379,-15.8395977604801));
#60101=CARTESIAN_POINT('Ctrl Pts',(-16.182721035153,-19.1631294473286,-15.8437673264241));
#60102=CARTESIAN_POINT('Ctrl Pts',(-16.1898981002617,-19.2498567867541,
-15.848083489163));
#60103=CARTESIAN_POINT('Ctrl Pts',(-16.2014998257647,-19.3361868282292,
-15.8523996519019));
#60104=CARTESIAN_POINT('Ctrl Pts',(-16.2174472402025,-19.4216405084271,
-15.8567158146408));
#60105=CARTESIAN_POINT('Ctrl Pts',(-16.2328751692924,-19.5043105439808,
-15.8608913788325));
#60106=CARTESIAN_POINT('Ctrl Pts',(-16.2523698584565,-19.5861599891147,
-15.8650669430242));
#60107=CARTESIAN_POINT('Ctrl Pts',(-16.2758083142181,-19.6667682393286,
-15.8692425072159));
#60108=CARTESIAN_POINT('Ctrl Pts',(-16.3004305906605,-19.7514478206325,
-15.8736289692284));
#60109=CARTESIAN_POINT('Ctrl Pts',(-16.3294053113242,-19.8347569748338,
-15.8780154312409));
#60110=CARTESIAN_POINT('Ctrl Pts',(-16.3625325554082,-19.9162313826263,
-15.8824018932535));
#60111=CARTESIAN_POINT('Ctrl Pts',(-16.3956597994923,-19.9977057904188,
-15.886788355266));
#60112=CARTESIAN_POINT('Ctrl Pts',(-16.4329392521204,-20.0773449585575,
-15.8911748172785));
#60113=CARTESIAN_POINT('Ctrl Pts',(-16.4741163568262,-20.1547160593073,
-15.8955612792911));
#60114=CARTESIAN_POINT('Ctrl Pts',(-16.5133988419055,-20.2285272010201,
-15.8997459136841));
#60115=CARTESIAN_POINT('Ctrl Pts',(-16.5563744043011,-20.3005491422939,
-15.9039305480772));
#60116=CARTESIAN_POINT('Ctrl Pts',(-16.6028559450592,-20.370388175744,-15.9081151824702));
#60117=CARTESIAN_POINT('Ctrl Pts',(-16.6492713250974,-20.4401278019745,
-15.9122938605541));
#60118=CARTESIAN_POINT('Ctrl Pts',(-16.699182518435,-20.5076903123662,-15.9164725386381));
#60119=CARTESIAN_POINT('Ctrl Pts',(-16.7523564064307,-20.5727062250963,
-15.920651216722));
#60120=CARTESIAN_POINT('Ctrl Pts',(-16.8064833981534,-20.6388875013359,
-15.9249047946075));
#60121=CARTESIAN_POINT('Ctrl Pts',(-16.8639909761113,-20.7024295607927,
-15.9291583724929));
#60122=CARTESIAN_POINT('Ctrl Pts',(-16.924586851981,-20.7629732355217,-15.9334119503784));
#60123=CARTESIAN_POINT('Ctrl Pts',(-16.9840079585538,-20.8223431529748,
-15.9375830643563));
#60124=CARTESIAN_POINT('Ctrl Pts',(-17.0463983458427,-20.8788295671755,
-15.9417541783343));
#60125=CARTESIAN_POINT('Ctrl Pts',(-17.1114427393838,-20.9321282625178,
-15.9459252923122));
#60126=CARTESIAN_POINT('Ctrl Pts',(-17.1764653066504,-20.985409072968,-15.9500950066326));
#60127=CARTESIAN_POINT('Ctrl Pts',(-17.2441397559347,-21.0355039976096,
-15.954264720953));
#60128=CARTESIAN_POINT('Ctrl Pts',(-17.3141166963442,-21.0821482117448,
-15.9584344352733));
#60129=CARTESIAN_POINT('Ctrl Pts',(-17.384091146674,-21.1287907660788,-15.9626040012174));
#60130=CARTESIAN_POINT('Ctrl Pts',(-17.456367541965,-21.1719825996022,-15.9667735671614));
#60131=CARTESIAN_POINT('Ctrl Pts',(-17.5305675384034,-21.2115022262382,
-15.9709431331055));
#60132=CARTESIAN_POINT('Ctrl Pts',(-17.6073763151809,-21.2524113141941,
-15.9752592958444));
#60133=CARTESIAN_POINT('Ctrl Pts',(-17.686246012007,-21.2893849131308,-15.9795754585833));
#60134=CARTESIAN_POINT('Ctrl Pts',(-17.766731066684,-21.3222301176556,-15.9838916213223));
#60135=CARTESIAN_POINT('Ctrl Pts',(-17.8445943291705,-21.3540053930978,
-15.9880671855139));
#60136=CARTESIAN_POINT('Ctrl Pts',(-17.9239688650711,-21.3819169968657,
-15.9922427497056));
#60137=CARTESIAN_POINT('Ctrl Pts',(-18.004434438527,-21.4058406817706,-15.9964183138973));
#60138=CARTESIAN_POINT('Ctrl Pts',(-18.0889641368095,-21.430972695127,-16.0008047759098));
#60139=CARTESIAN_POINT('Ctrl Pts',(-18.1746974182798,-21.451703205484,-16.0051912379224));
#60140=CARTESIAN_POINT('Ctrl Pts',(-18.2611356505439,-21.4679489873631,
-16.0095776999349));
#60141=CARTESIAN_POINT('Ctrl Pts',(-18.3475738828079,-21.4841947692422,
-16.0139641619475));
#60142=CARTESIAN_POINT('Ctrl Pts',(-18.4347164806881,-21.4959558204205,
-16.01835062396));
#60143=CARTESIAN_POINT('Ctrl Pts',(-18.5220617179685,-21.5032119011579,
-16.0227370859726));
#60144=CARTESIAN_POINT('Ctrl Pts',(-18.605388071405,-21.5101341188644,-16.0269217203656));
#60145=CARTESIAN_POINT('Ctrl Pts',(-18.6892089831259,-21.5129825827272,
-16.0311063547587));
#60146=CARTESIAN_POINT('Ctrl Pts',(-18.7730921344112,-21.5117015070174,
-16.0352909891517));
#60147=CARTESIAN_POINT('Ctrl Pts',(-18.8568558884131,-21.5104222547604,
-16.0394696672357));
#60148=CARTESIAN_POINT('Ctrl Pts',(-18.9406812499662,-21.5050251452316,
-16.0436483453196));
#60149=CARTESIAN_POINT('Ctrl Pts',(-19.0241313606303,-21.4955062008139,
-16.0478270234035));
#60150=CARTESIAN_POINT('Ctrl Pts',(-19.1090772545536,-21.4858166361586,
-16.052080601289));
#60151=CARTESIAN_POINT('Ctrl Pts',(-19.1936338320389,-21.471855975481,-16.0563341791744));
#60152=CARTESIAN_POINT('Ctrl Pts',(-19.2773408795583,-21.453675576209,-16.0605877570599));
#60153=CARTESIAN_POINT('Ctrl Pts',(-19.3594251026208,-21.4358476394531,
-16.0647588710378));
#60154=CARTESIAN_POINT('Ctrl Pts',(-19.440691971107,-21.4139622218932,-16.0689299850158));
#60155=CARTESIAN_POINT('Ctrl Pts',(-19.5207150357478,-21.3881197533226,
-16.0731010989937));
#60156=CARTESIAN_POINT('Ctrl Pts',(-19.6007112478764,-21.3622859564419,
-16.0772708133141));
#60157=CARTESIAN_POINT('Ctrl Pts',(-19.6794640476564,-21.3324978868906,
-16.0814405276345));
#60158=CARTESIAN_POINT('Ctrl Pts',(-19.7565616407632,-21.298905982531,-16.0856102419548));
#60159=CARTESIAN_POINT('Ctrl Pts',(-19.8336564904068,-21.2653152735155,
-16.0897798078989));
#60160=CARTESIAN_POINT('Ctrl Pts',(-19.9090958290848,-21.2279211833516,
-16.0939493738429));
#60161=CARTESIAN_POINT('Ctrl Pts',(-19.9824886317269,-21.1869219531001,
-16.098118939787));
#60162=CARTESIAN_POINT('Ctrl Pts',(-20.0584618347702,-21.1444812404909,
-16.1024351025259));
#60163=CARTESIAN_POINT('Ctrl Pts',(-20.1322414512869,-21.098177414705,-16.1067512652648));
#60164=CARTESIAN_POINT('Ctrl Pts',(-20.2034241040028,-21.0482807070084,
-16.1110674280037));
#60165=CARTESIAN_POINT('Ctrl Pts',(-20.2722879892936,-21.0000093793168,
-16.1152429921954));
#60166=CARTESIAN_POINT('Ctrl Pts',(-20.3387211617813,-20.9483759776511,
-16.1194185563871));
#60167=CARTESIAN_POINT('Ctrl Pts',(-20.4023916835426,-20.8936666012181,
-16.1235941205788));
#60168=CARTESIAN_POINT('Ctrl Pts',(-20.4692780519956,-20.8361939842408,
-16.1279805825913));
#60169=CARTESIAN_POINT('Ctrl Pts',(-20.533114929731,-20.7753268941813,-16.1323670446039));
#60170=CARTESIAN_POINT('Ctrl Pts',(-20.5935624370343,-20.7114395535997,
-16.1367535066164));
#60171=CARTESIAN_POINT('Ctrl Pts',(-20.6540099443376,-20.6475522130181,
-16.141139968629));
#60172=CARTESIAN_POINT('Ctrl Pts',(-20.7110677625942,-20.5806451127529,
-16.1455264306415));
#60173=CARTESIAN_POINT('Ctrl Pts',(-20.764447298501,-20.5111291697643,-16.149912892654));
#60174=CARTESIAN_POINT('Ctrl Pts',(-20.8154455601759,-20.4447143500982,
-16.1541036735168));
#60175=CARTESIAN_POINT('Ctrl Pts',(-20.8632791399794,-20.3756679864259,
-16.1582944543796));
#60176=CARTESIAN_POINT('Ctrl Pts',(-20.9076654294935,-20.3043234082959,
-16.1624852352424));
#60177=CARTESIAN_POINT('Ctrl Pts',(-20.9519891627481,-20.233079380358,-16.1666701097864));
#60178=CARTESIAN_POINT('Ctrl Pts',(-20.9928750133147,-20.1595439541276,
-16.1708549843304));
#60179=CARTESIAN_POINT('Ctrl Pts',(-21.0300812471761,-20.0840825528053,
-16.1750398588744));
#60180=CARTESIAN_POINT('Ctrl Pts',(-21.0672460755937,-20.0087051296902,
-16.1792200762261));
#60181=CARTESIAN_POINT('Ctrl Pts',(-21.1007392197538,-19.9314063968234,
-16.1834002935778));
#60182=CARTESIAN_POINT('Ctrl Pts',(-21.1303635397436,-19.8525785836825,
-16.1875805109294));
#60183=CARTESIAN_POINT('Ctrl Pts',(-21.159964013956,-19.7738142221411,-16.1917573634601));
#60184=CARTESIAN_POINT('Ctrl Pts',(-21.1857016914125,-19.6935236530682,
-16.1959342159908));
#60185=CARTESIAN_POINT('Ctrl Pts',(-21.2074270380285,-19.6121202068937,
-16.2001110685216));
#60186=CARTESIAN_POINT('Ctrl Pts',(-21.2291418983467,-19.5307560521882,
-16.2042859049869));
#60187=CARTESIAN_POINT('Ctrl Pts',(-21.2468481598046,-19.4482805298198,
-16.2084607414522));
#60188=CARTESIAN_POINT('Ctrl Pts',(-21.2604461548152,-19.3651220483335,
-16.2126355779175));
#60189=CARTESIAN_POINT('Ctrl Pts',(-21.2740449836494,-19.2819584676034,
-16.216810670382));
#60190=CARTESIAN_POINT('Ctrl Pts',(-21.2835349604933,-19.1981122945302,
-16.2209857628466));
#60191=CARTESIAN_POINT('Ctrl Pts',(-21.2888677421722,-19.1140210480402,
-16.2251608553111));
#60192=CARTESIAN_POINT('Ctrl Pts',(-21.2923288662564,-19.0594434830793,
-16.2278706067979));
#60193=CARTESIAN_POINT('Ctrl Pts',(-21.2940398771788,-19.0047628516758,
-16.2305803582847));
#60194=CARTESIAN_POINT('Ctrl Pts',(-21.293999294499,-18.9500994304893,-16.2332901097715));
#60195=CARTESIAN_POINT('Ctrl Pts',(-21.2939992944986,-18.9500994299065,
-16.2332901098004));
#60196=CARTESIAN_POINT('Ctrl Pts',(-21.2939272486892,-18.8530563258845,
-16.2381006886061));
#60197=CARTESIAN_POINT('Ctrl Pts',(-21.2883332378637,-18.7562381388316,
-16.2429112674119));
#60198=CARTESIAN_POINT('Ctrl Pts',(-21.277317503626,-18.6602191305971,-16.2477218462176));
#60199=CARTESIAN_POINT('Ctrl Pts',(-21.2661096544806,-18.5625255464771,
-16.2526163217373));
#60200=CARTESIAN_POINT('Ctrl Pts',(-21.2492893600035,-18.4656594493969,
-16.2575107972569));
#60201=CARTESIAN_POINT('Ctrl Pts',(-21.2270132516535,-18.3702054253606,
-16.2624052727766));
#60202=CARTESIAN_POINT('Ctrl Pts',(-21.2047371433035,-18.2747514013242,
-16.2672997482962));
#60203=CARTESIAN_POINT('Ctrl Pts',(-21.1770053785921,-18.1807095711097,
-16.2721942238158));
#60204=CARTESIAN_POINT('Ctrl Pts',(-21.1440235064311,-18.088642195582,-16.2770886993355));
#60205=CARTESIAN_POINT('Ctrl Pts',(-21.1158249638011,-18.0099272639074,
-16.2812733337285));
#60206=CARTESIAN_POINT('Ctrl Pts',(-21.0837134704203,-17.9324488089605,
-16.2854579681216));
#60207=CARTESIAN_POINT('Ctrl Pts',(-21.0478172393664,-17.856623451588,-16.2896426025146));
#60208=CARTESIAN_POINT('Ctrl Pts',(-21.0119721021543,-17.7809060222264,
-16.2938212805986));
#60209=CARTESIAN_POINT('Ctrl Pts',(-20.9723531229121,-17.7068374289185,
-16.2979999586825));
#60210=CARTESIAN_POINT('Ctrl Pts',(-20.9291375533229,-17.6348169747558,
-16.3021786367665));
#60211=CARTESIAN_POINT('Ctrl Pts',(-20.8851473757074,-17.5615056057125,
-16.3064322146519));
#60212=CARTESIAN_POINT('Ctrl Pts',(-20.8374305643562,-17.4903169777088,
-16.3106857925373));
#60213=CARTESIAN_POINT('Ctrl Pts',(-20.7862244101174,-17.4216487427658,
-16.3149393704228));
#60214=CARTESIAN_POINT('Ctrl Pts',(-20.7360109870992,-17.3543117755523,
-16.3191104844007));
#60215=CARTESIAN_POINT('Ctrl Pts',(-20.6824425969515,-17.2893987337786,
-16.3232815983787));
#60216=CARTESIAN_POINT('Ctrl Pts',(-20.6257872198942,-17.2272562176819,
-16.3274527123566));
#60217=CARTESIAN_POINT('Ctrl Pts',(-20.5691508540959,-17.1651345541068,
-16.331622426677));
#60218=CARTESIAN_POINT('Ctrl Pts',(-20.5094298683179,-17.105781909528,-16.3357921409974));
#60219=CARTESIAN_POINT('Ctrl Pts',(-20.4469316957118,-17.0495108394984,
-16.3399618553177));
#60220=CARTESIAN_POINT('Ctrl Pts',(-20.3844357470588,-16.993241771835,-16.3441314212618));
#60221=CARTESIAN_POINT('Ctrl Pts',(-20.3191631505139,-16.9400543678782,
-16.3483009872058));
#60222=CARTESIAN_POINT('Ctrl Pts',(-20.2514562536418,-16.890222485746,-16.3524705531499));
#60223=CARTESIAN_POINT('Ctrl Pts',(-20.1813688658012,-16.8386385761122,
-16.3567867158888));
#60224=CARTESIAN_POINT('Ctrl Pts',(-20.108673237446,-16.7906508514966,-16.3611028786277));
#60225=CARTESIAN_POINT('Ctrl Pts',(-20.0337823603675,-16.7465146076935,
-16.3654190413666));
#60226=CARTESIAN_POINT('Ctrl Pts',(-19.9613310457328,-16.7038160973899,
-16.3695946055583));
#60227=CARTESIAN_POINT('Ctrl Pts',(-19.8868257455389,-16.6647221743667,
-16.37377016975));
#60228=CARTESIAN_POINT('Ctrl Pts',(-19.8106643175706,-16.6294165359948,
-16.3779457339417));
#60229=CARTESIAN_POINT('Ctrl Pts',(-19.7306561569322,-16.59232769376,-16.3823321959542));
#60230=CARTESIAN_POINT('Ctrl Pts',(-19.6488207114385,-16.5594201038734,
-16.3867186579667));
#60231=CARTESIAN_POINT('Ctrl Pts',(-19.5656393424726,-16.5308482071436,
-16.3911051199793));
#60232=CARTESIAN_POINT('Ctrl Pts',(-19.4824579735068,-16.5022763104138,
-16.3954915819918));
#60233=CARTESIAN_POINT('Ctrl Pts',(-19.3979312597771,-16.4780401936422,
-16.3998780440044));
#60234=CARTESIAN_POINT('Ctrl Pts',(-19.3125527301389,-16.4582324209244,
-16.4042645060169));
#60235=CARTESIAN_POINT('Ctrl Pts',(-19.2310959760785,-16.4393344980203,
-16.408449480376));
#60236=CARTESIAN_POINT('Ctrl Pts',(-19.1485607218034,-16.424396672901,-16.412634454735));
#60237=CARTESIAN_POINT('Ctrl Pts',(-19.0653667817925,-16.4135366742999,
-16.4168194290941));
#60238=CARTESIAN_POINT('Ctrl Pts',(-18.9823149545929,-16.4026952268689,
-16.4209972546335));
#60239=CARTESIAN_POINT('Ctrl Pts',(-18.8986071312438,-16.3959178140196,
-16.425175080173));
#60240=CARTESIAN_POINT('Ctrl Pts',(-18.8146747411091,-16.39327149034,-16.4293529057124));
#60241=CARTESIAN_POINT('Ctrl Pts',(-18.7308239310132,-16.3906277388162,
-16.4335266705171));
#60242=CARTESIAN_POINT('Ctrl Pts',(-18.6467494445236,-16.3921071193267,
-16.4377004353219));
#60243=CARTESIAN_POINT('Ctrl Pts',(-18.5628884909385,-16.397724985154,-16.4418742001266));
#60244=CARTESIAN_POINT('Ctrl Pts',(-18.4790838891877,-16.403339075958,-16.4460451602971));
#60245=CARTESIAN_POINT('Ctrl Pts',(-18.3954929930032,-16.4130860985613,
-16.4502161204676));
#60246=CARTESIAN_POINT('Ctrl Pts',(-18.3125523070062,-16.4269293391926,
-16.4543870806381));
#60247=CARTESIAN_POINT('Ctrl Pts',(-18.22964247348,-16.4407674303829,-16.458556489285));
#60248=CARTESIAN_POINT('Ctrl Pts',(-18.1473828227084,-16.4586986359206,
-16.462725897932));
#60249=CARTESIAN_POINT('Ctrl Pts',(-18.0662026746028,-16.4806346421073,
-16.4668953065789));
#60250=CARTESIAN_POINT('Ctrl Pts',(-17.9849897282849,-16.5025795108275,
-16.4710663997405));
#60251=CARTESIAN_POINT('Ctrl Pts',(-17.9048576030274,-16.5285323016448,
-16.4752374929021));
#60252=CARTESIAN_POINT('Ctrl Pts',(-17.8262226566495,-16.5583541834892,
-16.4794085860637));
#60253=CARTESIAN_POINT('Ctrl Pts',(-17.7475755658492,-16.5881806710407,
-16.4835803234112));
#60254=CARTESIAN_POINT('Ctrl Pts',(-17.6704265406045,-16.6218772648513,
-16.4877520607586));
#60255=CARTESIAN_POINT('Ctrl Pts',(-17.5951721110539,-16.6592568745368,
-16.491923798106));
#60256=CARTESIAN_POINT('Ctrl Pts',(-17.5198228508105,-16.6966835875531,
-16.496100792403));
#60257=CARTESIAN_POINT('Ctrl Pts',(-17.4463733639788,-16.7378023734028,
-16.5002777867));
#60258=CARTESIAN_POINT('Ctrl Pts',(-17.3751954107008,-16.7823801973388,
-16.504454780997));
#60259=CARTESIAN_POINT('Ctrl Pts',(-17.3060362383624,-16.8256936850985,
-16.508513305514));
#60260=CARTESIAN_POINT('Ctrl Pts',(-17.2390217557067,-16.8722723328004,
-16.5125718300309));
#60261=CARTESIAN_POINT('Ctrl Pts',(-17.1744641548915,-16.9218650419685,
-16.5166303545479));
#60262=CARTESIAN_POINT('',(-21.2939994369002,-18.9536979607663,-16.1667098902285));
#60263=CARTESIAN_POINT('Ctrl Pts',(-21.2939994369002,-18.9536979607663,
-16.1667098902285));
#60264=CARTESIAN_POINT('Ctrl Pts',(-21.2940542005915,-18.8711312597184,
-16.1708335669039));
#60265=CARTESIAN_POINT('Ctrl Pts',(-21.2901102644712,-18.7884072256502,
-16.1749572435793));
#60266=CARTESIAN_POINT('Ctrl Pts',(-21.282148407848,-18.7059518510906,-16.1790809202548));
#60267=CARTESIAN_POINT('Ctrl Pts',(-21.274150019936,-18.6231181475505,-16.1832235175451));
#60268=CARTESIAN_POINT('Ctrl Pts',(-21.2620966823449,-18.5405560554535,
-16.1873661148355));
#60269=CARTESIAN_POINT('Ctrl Pts',(-21.2460219433306,-18.45869912201,-16.1915087121259));
#60270=CARTESIAN_POINT('Ctrl Pts',(-21.2300543085101,-18.3773875921873,
-16.1956237077524));
#60271=CARTESIAN_POINT('Ctrl Pts',(-21.2101187777555,-18.2967723256484,
-16.1997387033789));
#60272=CARTESIAN_POINT('Ctrl Pts',(-21.1863001253011,-18.2172727748014,
-16.2038536990054));
#60273=CARTESIAN_POINT('Ctrl Pts',(-21.1624916905598,-18.1378073276301,
-16.2079669293832));
#60274=CARTESIAN_POINT('Ctrl Pts',(-21.1348035753301,-18.0594570997617,
-16.2120801597611));
#60275=CARTESIAN_POINT('Ctrl Pts',(-21.1033710027997,-17.9826285278121,
-16.2161933901389));
#60276=CARTESIAN_POINT('Ctrl Pts',(-21.0719418753926,-17.9058083765509,
-16.2203061696918));
#60277=CARTESIAN_POINT('Ctrl Pts',(-21.0367692860286,-17.830509988201,-16.2244189492448));
#60278=CARTESIAN_POINT('Ctrl Pts',(-20.998036835518,-17.757120421374,-16.2285317287978));
#60279=CARTESIAN_POINT('Ctrl Pts',(-20.9588192445656,-17.68281161896,-16.2326960226666));
#60280=CARTESIAN_POINT('Ctrl Pts',(-20.9159522062818,-17.610460238745,-16.2368603165354));
#60281=CARTESIAN_POINT('Ctrl Pts',(-20.8696736494984,-17.5404412648287,
-16.2410246104042));
#60282=CARTESIAN_POINT('Ctrl Pts',(-20.8239074514183,-17.4711974842889,
-16.2451428005836));
#60283=CARTESIAN_POINT('Ctrl Pts',(-20.7748052350545,-17.4042350697679,
-16.2492609907631));
#60284=CARTESIAN_POINT('Ctrl Pts',(-20.7226388747277,-17.3398847975651,
-16.2533791809425));
#60285=CARTESIAN_POINT('Ctrl Pts',(-20.6695965003384,-17.2744539105173,
-16.257566526656));
#60286=CARTESIAN_POINT('Ctrl Pts',(-20.6133864683218,-17.2117240820488,
-16.2617538723695));
#60287=CARTESIAN_POINT('Ctrl Pts',(-20.5543334369044,-17.152003839313,-16.265941218083));
#60288=CARTESIAN_POINT('Ctrl Pts',(-20.495280405487,-17.0922835965773,-16.2701285637965));
#60289=CARTESIAN_POINT('Ctrl Pts',(-20.4333847973435,-17.0355732283015,
-16.27431590951));
#60290=CARTESIAN_POINT('Ctrl Pts',(-20.369004471075,-16.9821369642625,-16.2785032552236));
#60291=CARTESIAN_POINT('Ctrl Pts',(-20.3046658312848,-16.9287353003847,
-16.2826878896166));
#60292=CARTESIAN_POINT('Ctrl Pts',(-20.2375884427954,-16.8783896656033,
-16.2868725240096));
#60293=CARTESIAN_POINT('Ctrl Pts',(-20.1680947292198,-16.8313934104545,
-16.2910571584027));
#60294=CARTESIAN_POINT('Ctrl Pts',(-20.0986999313439,-16.7844640486578,
-16.2952358364866));
#60295=CARTESIAN_POINT('Ctrl Pts',(-20.0268960178071,-16.740874852386,-16.2994145145706));
#60296=CARTESIAN_POINT('Ctrl Pts',(-19.9530388079927,-16.7008793047445,
-16.3035931926545));
#60297=CARTESIAN_POINT('Ctrl Pts',(-19.8778577607726,-16.6601668656558,
-16.30784677054));
#60298=CARTESIAN_POINT('Ctrl Pts',(-19.8005494535676,-16.623178482619,-16.3121003484254));
#60299=CARTESIAN_POINT('Ctrl Pts',(-19.7215205448425,-16.5901356572584,
-16.3163539263108));
#60300=CARTESIAN_POINT('Ctrl Pts',(-19.6440237657252,-16.5577334315453,
-16.3205250402888));
#60301=CARTESIAN_POINT('Ctrl Pts',(-19.5648729481498,-16.5291253296777,
-16.3246961542667));
#60302=CARTESIAN_POINT('Ctrl Pts',(-19.4844751811847,-16.5044732887207,
-16.3288672682447));
#60303=CARTESIAN_POINT('Ctrl Pts',(-19.4041043924668,-16.479829519994,-16.3330369825651));
#60304=CARTESIAN_POINT('Ctrl Pts',(-19.3224879248152,-16.4591393105013,
-16.3372066968854));
#60305=CARTESIAN_POINT('Ctrl Pts',(-19.2400494979669,-16.4425152111225,
-16.3413764112058));
#60306=CARTESIAN_POINT('Ctrl Pts',(-19.1576140046316,-16.4258917033006,
-16.3455459771499));
#60307=CARTESIAN_POINT('Ctrl Pts',(-19.0743570613776,-16.4133341080144,
-16.3497155430939));
#60308=CARTESIAN_POINT('Ctrl Pts',(-18.9907127437438,-16.404903895178,-16.3538851090379));
#60309=CARTESIAN_POINT('Ctrl Pts',(-18.9041275950884,-16.3961772864581,
-16.3582012717769));
#60310=CARTESIAN_POINT('Ctrl Pts',(-18.8171278498232,-16.3918737507556,
-16.3625174345158));
#60311=CARTESIAN_POINT('Ctrl Pts',(-18.7301989430816,-16.3920028218831,
-16.3668335972547));
#60312=CARTESIAN_POINT('Ctrl Pts',(-18.6461017363339,-16.3921276885323,
-16.3710091614464));
#60313=CARTESIAN_POINT('Ctrl Pts',(-18.5620712918896,-16.3964007414036,
-16.3751847256381));
#60314=CARTESIAN_POINT('Ctrl Pts',(-18.4785435740568,-16.4047775883437,
-16.3793602898298));
#60315=CARTESIAN_POINT('Ctrl Pts',(-18.3907970697645,-16.4135775299086,
-16.3837467518423));
#60316=CARTESIAN_POINT('Ctrl Pts',(-18.303605989369,-16.42690663756,-16.3881332138548));
#60317=CARTESIAN_POINT('Ctrl Pts',(-18.2174632822104,-16.4446528323395,
-16.3925196758674));
#60318=CARTESIAN_POINT('Ctrl Pts',(-18.1313205750518,-16.462399027119,-16.3969061378799));
#60319=CARTESIAN_POINT('Ctrl Pts',(-18.046226783443,-16.4845620891763,-16.4012925998925));
#60320=CARTESIAN_POINT('Ctrl Pts',(-17.9626538344087,-16.510970485056,-16.405679061905));
#60321=CARTESIAN_POINT('Ctrl Pts',(-17.8829440437002,-16.5361581532291,
-16.4098627597763));
#60322=CARTESIAN_POINT('Ctrl Pts',(-17.8043209701197,-16.5653010733625,
-16.4140464576476));
#60323=CARTESIAN_POINT('Ctrl Pts',(-17.7272055153423,-16.5982870043986,
-16.4182301555188));
#60324=CARTESIAN_POINT('Ctrl Pts',(-17.6501861873222,-16.6312318174695,
-16.4224086382836));
#60325=CARTESIAN_POINT('Ctrl Pts',(-17.5746711677127,-16.6680099558202,
-16.4265871210483));
#60326=CARTESIAN_POINT('Ctrl Pts',(-17.5010661413011,-16.708459472157,-16.4307656038131));
#60327=CARTESIAN_POINT('Ctrl Pts',(-17.4275438125226,-16.7488635421511,
-16.434939391917));
#60328=CARTESIAN_POINT('Ctrl Pts',(-17.3559276133303,-16.79293057247,-16.439113180021));
#60329=CARTESIAN_POINT('Ctrl Pts',(-17.2866017020174,-16.8404512397302,
-16.4432869681249));
#60330=CARTESIAN_POINT('Ctrl Pts',(-17.2485113698382,-16.8665609289797,
-16.4455802084489));
#60331=CARTESIAN_POINT('Ctrl Pts',(-17.2111120439232,-16.8937123832665,
-16.447873448773));
#60332=CARTESIAN_POINT('Ctrl Pts',(-17.1744641548914,-16.9218650419685,
-16.4501666890971));
#60333=CARTESIAN_POINT('Ctrl Pts',(-17.1721129765924,-16.9188350422745,
-15.6501589808892));
#60334=CARTESIAN_POINT('Ctrl Pts',(-16.5413044634767,-17.4084201550706,
-15.6900393300921));
#60335=CARTESIAN_POINT('Ctrl Pts',(-15.7364335242104,-19.0750467767261,
-15.7723116148555));
#60336=CARTESIAN_POINT('Ctrl Pts',(-17.1577428497044,-21.5363189092118,
-15.8969758351793));
#60337=CARTESIAN_POINT('Ctrl Pts',(-20.0538051259393,-21.6762256253679,
-16.0241516418607));
#60338=CARTESIAN_POINT('Ctrl Pts',(-21.2452320241039,-20.0081650284355,
-16.1140629935438));
#60339=CARTESIAN_POINT('Ctrl Pts',(-21.2975539525536,-19.0564768252052,
-16.1615824096664));
#60340=CARTESIAN_POINT('Ctrl Pts',(-21.2967673506771,-18.9536997966296,
-16.1667098902285));
#60341=CARTESIAN_POINT('Origin',(-18.734,-18.952,1.76670989022851));
#60342=CARTESIAN_POINT('',(-17.1744641548915,-16.9218650419685,-14.8500370269081));
#60343=CARTESIAN_POINT('',(-17.1744641548914,-16.9218650419685,-14.9167585796912));
#60344=CARTESIAN_POINT('',(-17.1744641548914,-16.9218650419685,1.76670989022851));
#60345=CARTESIAN_POINT('',(-21.293999428374,-18.9537107672548,-15.4332901097416));
#60346=CARTESIAN_POINT('Ctrl Pts',(-17.1744641548914,-16.9218650419685,
-14.9167585796912));
#60347=CARTESIAN_POINT('Ctrl Pts',(-17.1078480248072,-16.9730390992979,
-14.9209295740523));
#60348=CARTESIAN_POINT('Ctrl Pts',(-17.0437052951214,-17.0275323959551,
-14.9251005684134));
#60349=CARTESIAN_POINT('Ctrl Pts',(-16.9823783827407,-17.0850715841388,
-14.9292715627744));
#60350=CARTESIAN_POINT('Ctrl Pts',(-16.9210709423153,-17.1425925030105,
-14.9334412327999));
#60351=CARTESIAN_POINT('Ctrl Pts',(-16.8625778787664,-17.2031570781273,
-14.9376109028253));
#60352=CARTESIAN_POINT('Ctrl Pts',(-16.8072069412376,-17.2664530535447,
-14.9417805728507));
#60353=CARTESIAN_POINT('Ctrl Pts',(-16.7518369746777,-17.3297479190219,
-14.945950169758));
#60354=CARTESIAN_POINT('Ctrl Pts',(-16.6995893273772,-17.3957737426153,
-14.9501197666653));
#60355=CARTESIAN_POINT('Ctrl Pts',(-16.6507325015835,-17.4641839730526,
-14.9542893635725));
#60356=CARTESIAN_POINT('Ctrl Pts',(-16.6008932637074,-17.5339697950445,
-14.9585428026516));
#60357=CARTESIAN_POINT('Ctrl Pts',(-16.5545830040309,-17.6062365666551,
-14.9627962417306));
#60358=CARTESIAN_POINT('Ctrl Pts',(-16.512040211465,-17.6805855521767,-14.9670496808097));
#60359=CARTESIAN_POINT('Ctrl Pts',(-16.4702752098586,-17.7535752482561,
-14.9712253561534));
#60360=CARTESIAN_POINT('Ctrl Pts',(-16.4321412272479,-17.8285712145274,
-14.9754010314971));
#60361=CARTESIAN_POINT('Ctrl Pts',(-16.397816458658,-17.905173146522,-14.9795767068408));
#60362=CARTESIAN_POINT('Ctrl Pts',(-16.3625328431747,-17.9839149188573,
-14.9838690277875));
#60363=CARTESIAN_POINT('Ctrl Pts',(-16.3312746199873,-18.0643532285809,
-14.9881613487342));
#60364=CARTESIAN_POINT('Ctrl Pts',(-16.3041808697538,-18.1460353641197,
-14.9924536696809));
#60365=CARTESIAN_POINT('Ctrl Pts',(-16.2770871195203,-18.2277174996585,
-14.9967459906277));
#60366=CARTESIAN_POINT('Ctrl Pts',(-16.2541579140775,-18.3106429409755,
-15.0010383115744));
#60367=CARTESIAN_POINT('Ctrl Pts',(-16.2354754819719,-18.3943484665023,
-15.0053306325211));
#60368=CARTESIAN_POINT('Ctrl Pts',(-16.21726175823,-18.4759539720913,-15.0095152669141));
#60369=CARTESIAN_POINT('Ctrl Pts',(-16.2030163785017,-18.5586046111965,
-15.0136999013072));
#60370=CARTESIAN_POINT('Ctrl Pts',(-16.1928535263697,-18.6418797014761,
-15.0178845357002));
#60371=CARTESIAN_POINT('Ctrl Pts',(-16.1827051397999,-18.7250362599721,
-15.0220632137842));
#60372=CARTESIAN_POINT('Ctrl Pts',(-16.1766277936582,-18.8088150514093,
-15.0262418918681));
#60373=CARTESIAN_POINT('Ctrl Pts',(-16.1746849654928,-18.8927838354389,
-15.0304205699521));
#60374=CARTESIAN_POINT('Ctrl Pts',(-16.1727073135288,-18.978257699575,-15.0346741478375));
#60375=CARTESIAN_POINT('Ctrl Pts',(-16.1750139649456,-19.0639279639718,
-15.0389277257229));
#60376=CARTESIAN_POINT('Ctrl Pts',(-16.1816167614736,-19.149331709792,-15.0431813036084));
#60377=CARTESIAN_POINT('Ctrl Pts',(-16.1880915499065,-19.2330797373478,
-15.0473524175863));
#60378=CARTESIAN_POINT('Ctrl Pts',(-16.1986973545604,-19.3165710082866,
-15.0515235315643));
#60379=CARTESIAN_POINT('Ctrl Pts',(-16.2133928011124,-19.3993693651964,
-15.0556946455422));
#60380=CARTESIAN_POINT('Ctrl Pts',(-16.2280833164655,-19.4821399383179,
-15.0598643598626));
#60381=CARTESIAN_POINT('Ctrl Pts',(-16.2468606679443,-19.5642176066097,
-15.064034074183));
#60382=CARTESIAN_POINT('Ctrl Pts',(-16.2696319425036,-19.6451739155444,
-15.0682037885034));
#60383=CARTESIAN_POINT('Ctrl Pts',(-16.2924024067631,-19.7261273437063,
-15.0723733544474));
#60384=CARTESIAN_POINT('Ctrl Pts',(-16.3191663861463,-19.8059590492309,
-15.0765429203915));
#60385=CARTESIAN_POINT('Ctrl Pts',(-16.3497807798976,-19.8842546382263,
-15.0807124863355));
#60386=CARTESIAN_POINT('Ctrl Pts',(-16.3814715379663,-19.9653030035427,
-15.0850286490744));
#60387=CARTESIAN_POINT('Ctrl Pts',(-16.4172883172413,-20.0447047315976,
-15.0893448118133));
#60388=CARTESIAN_POINT('Ctrl Pts',(-16.4570183818636,-20.1220233803942,
-15.0936609745523));
#60389=CARTESIAN_POINT('Ctrl Pts',(-16.4954542438098,-20.1968233823387,
-15.0978365387439));
#60390=CARTESIAN_POINT('Ctrl Pts',(-16.5375520792277,-20.2696735493081,
-15.1020121029356));
#60391=CARTESIAN_POINT('Ctrl Pts',(-16.583073696292,-20.3402060495535,-15.1061876671273));
#60392=CARTESIAN_POINT('Ctrl Pts',(-16.6308945020167,-20.4143009787112,
-15.1105741291398));
#60393=CARTESIAN_POINT('Ctrl Pts',(-16.6824937078808,-20.4858374838362,
-15.1149605911524));
#60394=CARTESIAN_POINT('Ctrl Pts',(-16.7375469032625,-20.5544278556388,
-15.1193470531649));
#60395=CARTESIAN_POINT('Ctrl Pts',(-16.7926000986442,-20.6230182274414,
-15.1237335151774));
#60396=CARTESIAN_POINT('Ctrl Pts',(-16.851106840707,-20.6886620833861,-15.12811997719));
#60397=CARTESIAN_POINT('Ctrl Pts',(-16.9126993772538,-20.7510175211999,
-15.1325064392025));
#60398=CARTESIAN_POINT('Ctrl Pts',(-16.9714579498921,-20.810503892887,-15.1366910735956));
#60399=CARTESIAN_POINT('Ctrl Pts',(-17.0332433037704,-20.8672192262126,
-15.1408757079886));
#60400=CARTESIAN_POINT('Ctrl Pts',(-17.0977635170215,-20.9208398034807,
-15.1450603423817));
#60401=CARTESIAN_POINT('Ctrl Pts',(-17.162191893735,-20.9743840584939,-15.1492390204656));
#60402=CARTESIAN_POINT('Ctrl Pts',(-17.2293470468519,-21.0248420156528,
-15.1534176985496));
#60403=CARTESIAN_POINT('Ctrl Pts',(-17.2988998898354,-21.0719263368819,
-15.1575963766335));
#60404=CARTESIAN_POINT('Ctrl Pts',(-17.3696994175427,-21.1198546107302,
-15.1618499545189));
#60405=CARTESIAN_POINT('Ctrl Pts',(-17.4429830989499,-21.1642867711771,
-15.1661035324044));
#60406=CARTESIAN_POINT('Ctrl Pts',(-17.5183681022775,-21.2049622920146,
-15.1703571102898));
#60407=CARTESIAN_POINT('Ctrl Pts',(-17.5922916202138,-21.2448492385089,
-15.1745282242678));
#60408=CARTESIAN_POINT('Ctrl Pts',(-17.6682352871973,-21.281123676622,-15.1786993382457));
#60409=CARTESIAN_POINT('Ctrl Pts',(-17.7458099687318,-21.3135843118767,
-15.1828704522237));
#60410=CARTESIAN_POINT('Ctrl Pts',(-17.8233586193327,-21.3460340546518,
-15.187040166544));
#60411=CARTESIAN_POINT('Ctrl Pts',(-17.9025367735084,-21.3746723587587,
-15.1912098808644));
#60412=CARTESIAN_POINT('Ctrl Pts',(-17.9829338767364,-21.3993454350553,
-15.1953795951848));
#60413=CARTESIAN_POINT('Ctrl Pts',(-18.0633281190904,-21.4240176333778,
-15.1995491611289));
#60414=CARTESIAN_POINT('Ctrl Pts',(-18.1449407842163,-21.4447247502805,
-15.2037187270729));
#60415=CARTESIAN_POINT('Ctrl Pts',(-18.2273459747055,-21.4613628072985,
-15.2078882930169));
#60416=CARTESIAN_POINT('Ctrl Pts',(-18.3126484300345,-21.4785858378759,
-15.2122044557559));
#60417=CARTESIAN_POINT('Ctrl Pts',(-18.3987996610354,-21.4914482440571,
-15.2165206184948));
#60418=CARTESIAN_POINT('Ctrl Pts',(-18.4853175391717,-21.4998926652582,
-15.2208367812337));
#60419=CARTESIAN_POINT('Ctrl Pts',(-18.5690171065278,-21.5080620103268,
-15.2250123454254));
#60420=CARTESIAN_POINT('Ctrl Pts',(-18.6530593280231,-21.512096806535,-15.2291879096171));
#60421=CARTESIAN_POINT('Ctrl Pts',(-18.7370059866504,-21.5119982351643,
-15.2333634738087));
#60422=CARTESIAN_POINT('Ctrl Pts',(-18.8251925914409,-21.5118946851879,
-15.2377499358213));
#60423=CARTESIAN_POINT('Ctrl Pts',(-18.9132731428316,-21.5072292722347,
-15.2421363978338));
#60424=CARTESIAN_POINT('Ctrl Pts',(-19.0007460413497,-21.4980649146132,
-15.2465228598464));
#60425=CARTESIAN_POINT('Ctrl Pts',(-19.0882189398678,-21.4889005569917,
-15.2509093218589));
#60426=CARTESIAN_POINT('Ctrl Pts',(-19.1750836241625,-21.4752374199982,
-15.2552957838715));
#60427=CARTESIAN_POINT('Ctrl Pts',(-19.2608535512399,-21.4571996598167,
-15.259682245884));
#60428=CARTESIAN_POINT('Ctrl Pts',(-19.3426770768309,-21.4399918437197,
-15.263866880277));
#60429=CARTESIAN_POINT('Ctrl Pts',(-19.4238089369639,-21.4187390730901,
-15.2680515146701));
#60430=CARTESIAN_POINT('Ctrl Pts',(-19.5038189245161,-21.3935115857716,
-15.2722361490631));
#60431=CARTESIAN_POINT('Ctrl Pts',(-19.5837150277544,-21.3683200066587,
-15.2764148271471));
#60432=CARTESIAN_POINT('Ctrl Pts',(-19.6624919952641,-21.33916508562,-15.280593505231));
#60433=CARTESIAN_POINT('Ctrl Pts',(-19.7397300928954,-21.3061680017035,
-15.284772183315));
#60434=CARTESIAN_POINT('Ctrl Pts',(-19.8183526279167,-21.2725794687723,
-15.2890257612004));
#60435=CARTESIAN_POINT('Ctrl Pts',(-19.8953801101215,-21.2350097758302,
-15.2932793390858));
#60436=CARTESIAN_POINT('Ctrl Pts',(-19.9703862586167,-21.1936398059242,
-15.2975329169713));
#60437=CARTESIAN_POINT('Ctrl Pts',(-20.0439382665608,-21.1530718736117,
-15.3017040309492));
#60438=CARTESIAN_POINT('Ctrl Pts',(-20.1155461950122,-21.1088499333759,
-15.3058751449272));
#60439=CARTESIAN_POINT('Ctrl Pts',(-20.1848301560489,-21.0611922288637,
-15.3100462589051));
#60440=CARTESIAN_POINT('Ctrl Pts',(-20.2540908681833,-21.0135505163546,
-15.3142159732255));
#60441=CARTESIAN_POINT('Ctrl Pts',(-20.3210287829501,-20.9624755897522,
-15.3183856875459));
#60442=CARTESIAN_POINT('Ctrl Pts',(-20.385292362642,-20.9082294172924,-15.3225554018662));
#60443=CARTESIAN_POINT('Ctrl Pts',(-20.4495536555601,-20.8539851751441,
-15.3267249678103));
#60444=CARTESIAN_POINT('Ctrl Pts',(-20.5111404516291,-20.7965702088954,
-15.3308945337543));
#60445=CARTESIAN_POINT('Ctrl Pts',(-20.5697347912254,-20.7362863492962,
-15.3350640996984));
#60446=CARTESIAN_POINT('Ctrl Pts',(-20.630389235518,-20.6738829835616,-15.3393802624373));
#60447=CARTESIAN_POINT('Ctrl Pts',(-20.68783651095,-20.6084056085287,-15.3436964251762));
#60448=CARTESIAN_POINT('Ctrl Pts',(-20.7417674193154,-20.540228569802,-15.3480125879152));
#60449=CARTESIAN_POINT('Ctrl Pts',(-20.7939415340134,-20.474272390941,-15.3521881521068));
#60450=CARTESIAN_POINT('Ctrl Pts',(-20.8428246196129,-20.4057901412947,
-15.3563637162985));
#60451=CARTESIAN_POINT('Ctrl Pts',(-20.8881804708301,-20.3351509314223,
-15.3605392804902));
#60452=CARTESIAN_POINT('Ctrl Pts',(-20.9358271382689,-20.2609439029881,
-15.3649257425027));
#60453=CARTESIAN_POINT('Ctrl Pts',(-20.9795805961809,-20.1843567987729,
-15.3693122045153));
#60454=CARTESIAN_POINT('Ctrl Pts',(-21.0192222426254,-20.1058454410407,
-15.3736986665278));
#60455=CARTESIAN_POINT('Ctrl Pts',(-21.0588638890698,-20.0273340833085,
-15.3780851285404));
#60456=CARTESIAN_POINT('Ctrl Pts',(-21.0943935591863,-19.9468990335382,
-15.3824715905529));
#60457=CARTESIAN_POINT('Ctrl Pts',(-21.1256522921828,-19.8650166007783,
-15.3868580525655));
#60458=CARTESIAN_POINT('Ctrl Pts',(-21.1596866697226,-19.7758633510054,
-15.3916340140293));
#60459=CARTESIAN_POINT('Ctrl Pts',(-21.1887650239783,-19.6847190703918,
-15.3964099754931));
#60460=CARTESIAN_POINT('Ctrl Pts',(-21.2126811308614,-19.5921092496689,
-15.4011859369569));
#60461=CARTESIAN_POINT('Ctrl Pts',(-21.2364993763692,-19.4998783754223,
-15.4059423558521));
#60462=CARTESIAN_POINT('Ctrl Pts',(-21.2551974088384,-19.4061941121839,
-15.4106987747474));
#60463=CARTESIAN_POINT('Ctrl Pts',(-21.2686182636666,-19.3115973546727,
-15.4154551936427));
#60464=CARTESIAN_POINT('Ctrl Pts',(-21.2819450244391,-19.2176638181475,
-15.4201782651282));
#60465=CARTESIAN_POINT('Ctrl Pts',(-21.2900682365862,-19.1228307363249,
-15.4249013366138));
#60466=CARTESIAN_POINT('Ctrl Pts',(-21.2928821031965,-19.0276464271503,
-15.4296244080994));
#60467=CARTESIAN_POINT('Ctrl Pts',(-21.2936100754836,-19.0030214008636,
-15.4308463086468));
#60468=CARTESIAN_POINT('Ctrl Pts',(-21.2939829474075,-18.9783729560409,
-15.4320682091942));
#60469=CARTESIAN_POINT('Ctrl Pts',(-21.293999428374,-18.9537107672549,-15.4332901097416));
#60470=CARTESIAN_POINT('Ctrl Pts',(-21.2939994283744,-18.9537107666516,
-15.4332901097715));
#60471=CARTESIAN_POINT('Ctrl Pts',(-21.2940559692553,-18.8691027211111,
-15.437482057942));
#60472=CARTESIAN_POINT('Ctrl Pts',(-21.2899137324165,-18.7844696898645,
-15.4416740061124));
#60473=CARTESIAN_POINT('Ctrl Pts',(-21.2815918669692,-18.7002547332074,
-15.4458659542829));
#60474=CARTESIAN_POINT('Ctrl Pts',(-21.2732695913204,-18.6160356254257,
-15.4500581090829));
#60475=CARTESIAN_POINT('Ctrl Pts',(-21.2607673227297,-18.5322350838833,
-15.4542502638829));
#60476=CARTESIAN_POINT('Ctrl Pts',(-21.2441560631151,-18.449290800953,-15.4584424186829));
#60477=CARTESIAN_POINT('Ctrl Pts',(-21.2275392030056,-18.3663185533138,
-15.4626359868701));
#60478=CARTESIAN_POINT('Ctrl Pts',(-21.2068106889621,-18.2842035816671,
-15.4668295550574));
#60479=CARTESIAN_POINT('Ctrl Pts',(-21.1820923104735,-18.2033718951306,
-15.4710231232446));
#60480=CARTESIAN_POINT('Ctrl Pts',(-21.1573415752886,-18.1224343988081,
-15.4752221808701));
#60481=CARTESIAN_POINT('Ctrl Pts',(-21.1285906849035,-18.0427839738201,
-15.4794212384956));
#60482=CARTESIAN_POINT('Ctrl Pts',(-21.0960107310926,-17.9648296468171,
-15.483620296121));
#60483=CARTESIAN_POINT('Ctrl Pts',(-21.0634063961442,-17.8868169828631,
-15.4878224961022));
#60484=CARTESIAN_POINT('Ctrl Pts',(-21.0269674888688,-17.8105033515339,
-15.4920246960833));
#60485=CARTESIAN_POINT('Ctrl Pts',(-20.9869114421218,-17.7362738655615,
-15.4962268960644));
#60486=CARTESIAN_POINT('Ctrl Pts',(-20.9467843119657,-17.6619126520388,
-15.5004365532642));
#60487=CARTESIAN_POINT('Ctrl Pts',(-20.9030274638811,-17.5896433529156,
-15.5046462104641));
#60488=CARTESIAN_POINT('Ctrl Pts',(-20.8559018807132,-17.5198224940232,
-15.5088558676639));
#60489=CARTESIAN_POINT('Ctrl Pts',(-20.8365799691019,-17.4911953158865,
-15.5105818648582));
#60490=CARTESIAN_POINT('Ctrl Pts',(-20.8166922183615,-17.4629793510679,
-15.5123078620525));
#60491=CARTESIAN_POINT('Ctrl Pts',(-20.7962584977301,-17.435197478727,-15.5140338592469));
#60492=CARTESIAN_POINT('Ctrl Pts',(-20.7467174843303,-17.3678410665132,
-15.5182184936399));
#60493=CARTESIAN_POINT('Ctrl Pts',(-20.6937808669812,-17.3027889832896,
-15.522403128033));
#60494=CARTESIAN_POINT('Ctrl Pts',(-20.6376906991394,-17.2404037502932,
-15.526587762426));
#60495=CARTESIAN_POINT('Ctrl Pts',(-20.581680368709,-17.1781073149544,-15.53076644051));
#60496=CARTESIAN_POINT('Ctrl Pts',(-20.522525708678,-17.1184705290968,-15.5349451185939));
#60497=CARTESIAN_POINT('Ctrl Pts',(-20.4605108062944,-17.061825289623,-15.5391237966778));
#60498=CARTESIAN_POINT('Ctrl Pts',(-20.3973843313549,-17.0041647249419,
-15.5433773745633));
#60499=CARTESIAN_POINT('Ctrl Pts',(-20.3312943514667,-16.9496043968549,
-15.5476309524487));
#60500=CARTESIAN_POINT('Ctrl Pts',(-20.2625820107878,-16.8984574422973,
-15.5518845303342));
#60501=CARTESIAN_POINT('Ctrl Pts',(-20.195201792914,-16.8483020712589,-15.5560556443121));
#60502=CARTESIAN_POINT('Ctrl Pts',(-20.1253003720614,-16.8014291923403,
-15.5602267582901));
#60503=CARTESIAN_POINT('Ctrl Pts',(-20.0532336923064,-16.7580942442567,
-15.564397872268));
#60504=CARTESIAN_POINT('Ctrl Pts',(-19.9811911952218,-16.7147738376335,
-15.5685675865884));
#60505=CARTESIAN_POINT('Ctrl Pts',(-19.9069852761389,-16.6749892409427,
-15.5727373009088));
#60506=CARTESIAN_POINT('Ctrl Pts',(-19.8309999421957,-16.6389519834594,
-15.5769070152291));
#60507=CARTESIAN_POINT('Ctrl Pts',(-19.7550173121369,-16.6029160083363,
-15.5810765811732));
#60508=CARTESIAN_POINT('Ctrl Pts',(-19.6772558091333,-16.5706273036551,
-15.5852461471172));
#60509=CARTESIAN_POINT('Ctrl Pts',(-19.5981218233864,-16.5422503295265,
-15.5894157130613));
#60510=CARTESIAN_POINT('Ctrl Pts',(-19.516205584323,-16.5128756559943,-15.5937318758002));
#60511=CARTESIAN_POINT('Ctrl Pts',(-19.4328190502828,-16.4876930819298,
-15.5980480385391));
#60512=CARTESIAN_POINT('Ctrl Pts',(-19.3484309915969,-16.4668290689441,
-15.602364201278));
#60513=CARTESIAN_POINT('Ctrl Pts',(-19.2667918650467,-16.4466446989869,
-15.6065397654697));
#60514=CARTESIAN_POINT('Ctrl Pts',(-19.1842159325102,-16.4305019005906,
-15.6107153296614));
#60515=CARTESIAN_POINT('Ctrl Pts',(-19.1011369778116,-16.4184628600466,
-15.6148908938531));
#60516=CARTESIAN_POINT('Ctrl Pts',(-19.0138619026128,-16.4058157561848,
-15.6192773558656));
#60517=CARTESIAN_POINT('Ctrl Pts',(-18.926032235907,-16.3976979204099,-15.6236638178781));
#60518=CARTESIAN_POINT('Ctrl Pts',(-18.8381534037014,-16.3941196141146,
-15.6280502798907));
#60519=CARTESIAN_POINT('Ctrl Pts',(-18.7502745714958,-16.3905413078192,
-15.6324367419032));
#60520=CARTESIAN_POINT('Ctrl Pts',(-18.6623471531412,-16.391502448601,-15.6368232039158));
#60521=CARTESIAN_POINT('Ctrl Pts',(-18.5748705298081,-16.3969505265619,
-15.6412096659283));
#60522=CARTESIAN_POINT('Ctrl Pts',(-18.4914284406973,-16.4021473321697,
-15.6453938186789));
#60523=CARTESIAN_POINT('Ctrl Pts',(-18.4080859286891,-16.4114456475977,
-15.6495779714295));
#60524=CARTESIAN_POINT('Ctrl Pts',(-18.3252786851494,-16.4248381755838,
-15.6537621241801));
#60525=CARTESIAN_POINT('Ctrl Pts',(-18.2425831161189,-16.4382126422997,
-15.6579406341489));
#60526=CARTESIAN_POINT('Ctrl Pts',(-18.1604218322578,-16.4556702853485,
-15.6621191441177));
#60527=CARTESIAN_POINT('Ctrl Pts',(-18.0792276257711,-16.477151895985,-15.6662976540865));
#60528=CARTESIAN_POINT('Ctrl Pts',(-17.997681334868,-16.4987266578532,-15.67049428343));
#60529=CARTESIAN_POINT('Ctrl Pts',(-17.9171109977116,-16.5243603430073,
-15.6746909127734));
#60530=CARTESIAN_POINT('Ctrl Pts',(-17.8379469013808,-16.5539406086473,
-15.6788875421169));
#60531=CARTESIAN_POINT('Ctrl Pts',(-17.7592670966102,-16.5833399150688,
-15.6830584983046));
#60532=CARTESIAN_POINT('Ctrl Pts',(-17.6819768120108,-16.6166374905021,
-15.6872294544923));
#60533=CARTESIAN_POINT('Ctrl Pts',(-17.6064837009691,-16.6536730007634,
-15.69140041068));
#60534=CARTESIAN_POINT('Ctrl Pts',(-17.5302935747919,-16.6910504536318,
-15.6956098766013));
#60535=CARTESIAN_POINT('Ctrl Pts',(-17.4559344312179,-16.7322350696159,
-15.6998193425226));
#60536=CARTESIAN_POINT('Ctrl Pts',(-17.383803351038,-16.777012871502,-15.7040288084439));
#60537=CARTESIAN_POINT('Ctrl Pts',(-17.3116722708582,-16.8217906733882,
-15.7082382743652));
#60538=CARTESIAN_POINT('Ctrl Pts',(-17.2417696646533,-16.8701614078669,
-15.7124477402865));
#60539=CARTESIAN_POINT('Ctrl Pts',(-17.1744641548914,-16.9218650419685,
-15.7166572062078));
#60540=CARTESIAN_POINT('',(-21.2939991231355,-18.9498811452879,-15.3667098902285));
#60541=CARTESIAN_POINT('Ctrl Pts',(-21.2956373739999,-18.9498797893439,
-15.3667098902285));
#60542=CARTESIAN_POINT('Ctrl Pts',(-21.296922788715,-18.8056440679786,-15.3738974629702));
#60543=CARTESIAN_POINT('Ctrl Pts',(-21.2201491749354,-17.8120820090192,
-15.4234769712724));
#60544=CARTESIAN_POINT('Ctrl Pts',(-19.9200692397814,-16.166945137558,-15.515448415135));
#60545=CARTESIAN_POINT('Ctrl Pts',(-17.9391679634644,-16.3593206301496,
-15.6027438726135));
#60546=CARTESIAN_POINT('Ctrl Pts',(-17.2118400624246,-16.888001929858,-15.6476473945316));
#60547=CARTESIAN_POINT('Ctrl Pts',(-17.1721129765924,-16.9188350422745,
-15.6501589808892));
#60548=CARTESIAN_POINT('Ctrl Pts',(-17.1744641548915,-16.9218650419685,
-14.8500370269081));
#60549=CARTESIAN_POINT('Ctrl Pts',(-17.1078234648678,-16.9730579660761,
-14.8542147166677));
#60550=CARTESIAN_POINT('Ctrl Pts',(-17.0437722116886,-17.0274847849136,
-14.8583924064273));
#60551=CARTESIAN_POINT('Ctrl Pts',(-16.98262429975,-17.0848408861123,-14.8625700961868));
#60552=CARTESIAN_POINT('Ctrl Pts',(-16.9213774940062,-17.142289748665,-14.8667545424754));
#60553=CARTESIAN_POINT('Ctrl Pts',(-16.8630437183746,-17.2026770171266,
-14.8709389887639));
#60554=CARTESIAN_POINT('Ctrl Pts',(-16.8078981185104,-17.2656632773606,
-14.8751234350524));
#60555=CARTESIAN_POINT('Ctrl Pts',(-16.7883675060572,-17.2879707731814,
-14.8766054172776));
#60556=CARTESIAN_POINT('Ctrl Pts',(-16.7692364062925,-17.3106039888822,
-14.8780873995027));
#60557=CARTESIAN_POINT('Ctrl Pts',(-16.7505157350919,-17.3335469821889,
-14.8795693817278));
#60558=CARTESIAN_POINT('Ctrl Pts',(-16.6976546661539,-17.398330511467,-14.8837540161209));
#60559=CARTESIAN_POINT('Ctrl Pts',(-16.6478724513803,-17.4658271045687,
-14.8879386505139));
#60560=CARTESIAN_POINT('Ctrl Pts',(-16.6014597312929,-17.5357118928894,
-14.892123284907));
#60561=CARTESIAN_POINT('Ctrl Pts',(-16.5551130739679,-17.605497208864,-14.8963019629909));
#60562=CARTESIAN_POINT('Ctrl Pts',(-16.5121266371781,-17.6776635880369,
-14.9004806410749));
#60563=CARTESIAN_POINT('Ctrl Pts',(-16.4727509157818,-17.7518531010238,
-14.9046593191588));
#60564=CARTESIAN_POINT('Ctrl Pts',(-16.4326694128783,-17.8273724077119,
-14.9089128970443));
#60565=CARTESIAN_POINT('Ctrl Pts',(-16.3963296475342,-17.9049877173956,
-14.9131664749297));
#60566=CARTESIAN_POINT('Ctrl Pts',(-16.3639497085597,-17.98429053118,-14.9174200528151));
#60567=CARTESIAN_POINT('Ctrl Pts',(-16.3321975178866,-18.0620559051724,
-14.9215911667931));
#60568=CARTESIAN_POINT('Ctrl Pts',(-16.3042531677127,-18.1414434905287,
-14.925762280771));
#60569=CARTESIAN_POINT('Ctrl Pts',(-16.2802751807717,-18.2220448565132,
-14.929933394749));
#60570=CARTESIAN_POINT('Ctrl Pts',(-16.2563052398757,-18.302619175931,-14.9341031090694));
#60571=CARTESIAN_POINT('Ctrl Pts',(-16.2362991499856,-18.3844060265128,
-14.9382728233897));
#60572=CARTESIAN_POINT('Ctrl Pts',(-16.2203659101291,-18.4669807609602,
-14.9424425377101));
#60573=CARTESIAN_POINT('Ctrl Pts',(-16.2044332372455,-18.5495525570442,
-14.9466121036542));
#60574=CARTESIAN_POINT('Ctrl Pts',(-16.1925732125598,-18.6329117293879,
-14.9507816695982));
#60575=CARTESIAN_POINT('Ctrl Pts',(-16.1848436692123,-18.7166237029672,
-14.9549512355423));
#60576=CARTESIAN_POINT('Ctrl Pts',(-16.1768423646561,-18.8032788862675,
-14.9592673982812));
#60577=CARTESIAN_POINT('Ctrl Pts',(-16.1732674495782,-18.890311616191,-14.9635835610201));
#60578=CARTESIAN_POINT('Ctrl Pts',(-16.1741243927921,-18.9772363947927,
-14.967899723759));
#60579=CARTESIAN_POINT('Ctrl Pts',(-16.174953421171,-19.0613296078744,-14.9720752879507));
#60580=CARTESIAN_POINT('Ctrl Pts',(-16.1799299313356,-19.1453213272336,
-14.9762508521424));
#60581=CARTESIAN_POINT('Ctrl Pts',(-16.1890058822549,-19.228775975552,-14.9804264163341));
#60582=CARTESIAN_POINT('Ctrl Pts',(-16.1985402378791,-19.3164457197621,
-14.9848128783466));
#60583=CARTESIAN_POINT('Ctrl Pts',(-16.2125989501167,-19.4035221357512,
-14.9891993403591));
#60584=CARTESIAN_POINT('Ctrl Pts',(-16.2310658163555,-19.4895132299243,
-14.9935858023717));
#60585=CARTESIAN_POINT('Ctrl Pts',(-16.2495326825942,-19.5755043240973,
-14.9979722643842));
#60586=CARTESIAN_POINT('Ctrl Pts',(-16.2724074784503,-19.660409556001,-15.0023587263968));
#60587=CARTESIAN_POINT('Ctrl Pts',(-16.2995147249235,-19.7437584514457,
-15.0067451884093));
#60588=CARTESIAN_POINT('Ctrl Pts',(-16.325374726804,-19.8232723406583,-15.0109298228023));
#60589=CARTESIAN_POINT('Ctrl Pts',(-16.3551825113724,-19.9016659307484,
-15.0151144571954));
#60590=CARTESIAN_POINT('Ctrl Pts',(-16.3888222337461,-19.9785189938177,
-15.0192990915884));
#60591=CARTESIAN_POINT('Ctrl Pts',(-16.4224140741388,-20.0552626660643,
-15.0234777696724));
#60592=CARTESIAN_POINT('Ctrl Pts',(-16.459826835514,-20.130469748956,-15.0276564477563));
#60593=CARTESIAN_POINT('Ctrl Pts',(-16.5008951440188,-20.2037358755717,
-15.0318351258403));
#60594=CARTESIAN_POINT('Ctrl Pts',(-16.5426995724383,-20.2783152448515,
-15.0360887037257));
#60595=CARTESIAN_POINT('Ctrl Pts',(-16.5882917392507,-20.3508829316544,
-15.0403422816111));
#60596=CARTESIAN_POINT('Ctrl Pts',(-16.6374462088682,-20.4210344451002,
-15.0445958594966));
#60597=CARTESIAN_POINT('Ctrl Pts',(-16.6856477231751,-20.4898259345683,
-15.0487669734745));
#60598=CARTESIAN_POINT('Ctrl Pts',(-16.7372743723593,-20.5562937050238,
-15.0529380874525));
#60599=CARTESIAN_POINT('Ctrl Pts',(-16.7920685361568,-20.6200833881242,
-15.0571092014304));
#60600=CARTESIAN_POINT('Ctrl Pts',(-16.8468443132435,-20.6838516659803,
-15.0612789157508));
#60601=CARTESIAN_POINT('Ctrl Pts',(-16.9047851945211,-20.744943292555,-15.0654486300712));
#60602=CARTESIAN_POINT('Ctrl Pts',(-16.9655931179196,-20.8030367633872,
-15.0696183443915));
#60603=CARTESIAN_POINT('Ctrl Pts',(-17.0263988775113,-20.8611281670043,
-15.0737879103356));
#60604=CARTESIAN_POINT('Ctrl Pts',(-17.090071143158,-20.9162213098333,-15.0779574762796));
#60605=CARTESIAN_POINT('Ctrl Pts',(-17.1562758100195,-20.9680323361371,
-15.0821270422237));
#60606=CARTESIAN_POINT('Ctrl Pts',(-17.2248081512956,-21.02166497421,-15.0864432049626));
#60607=CARTESIAN_POINT('Ctrl Pts',(-17.2960538702051,-21.0717800780493,
-15.0907593677015));
#60608=CARTESIAN_POINT('Ctrl Pts',(-17.3696076999733,-21.118110258419,-15.0950755304404));
#60609=CARTESIAN_POINT('Ctrl Pts',(-17.4407655214732,-21.1629312380361,
-15.0992510946321));
#60610=CARTESIAN_POINT('Ctrl Pts',(-17.5140829560416,-21.2042099051977,
-15.1034266588238));
#60611=CARTESIAN_POINT('Ctrl Pts',(-17.5891677483864,-21.241750885067,-15.1076022230155));
#60612=CARTESIAN_POINT('Ctrl Pts',(-17.6680448950955,-21.2811879705844,
-15.111988685028));
#60613=CARTESIAN_POINT('Ctrl Pts',(-17.7488720950907,-21.3164996308722,
-15.1163751470406));
#60614=CARTESIAN_POINT('Ctrl Pts',(-17.831172761348,-21.3475172671363,-15.1207616090531));
#60615=CARTESIAN_POINT('Ctrl Pts',(-17.9134734276052,-21.3785349034003,
-15.1251480710657));
#60616=CARTESIAN_POINT('Ctrl Pts',(-17.9972469842344,-21.4052584117747,
-15.1295345330782));
#60617=CARTESIAN_POINT('Ctrl Pts',(-18.0820028534413,-21.4275806835729,
-15.1339209950908));
#60618=CARTESIAN_POINT('Ctrl Pts',(-18.1628589794675,-21.4488758745561,
-15.1381056294838));
#60619=CARTESIAN_POINT('Ctrl Pts',(-18.2449099711163,-21.4662452083818,
-15.1422902638769));
#60620=CARTESIAN_POINT('Ctrl Pts',(-18.3277397785898,-21.4795586308728,
-15.1464748982699));
#60621=CARTESIAN_POINT('Ctrl Pts',(-18.4104516880846,-21.4928531033548,
-15.1506535763538));
#60622=CARTESIAN_POINT('Ctrl Pts',(-18.4939397611609,-21.5021030592902,
-15.1548322544378));
#60623=CARTESIAN_POINT('Ctrl Pts',(-18.5777744755002,-21.5072286757734,
-15.1590109325217));
#60624=CARTESIAN_POINT('Ctrl Pts',(-18.6631118668432,-21.5124461652484,
-15.1632645104072));
#60625=CARTESIAN_POINT('Ctrl Pts',(-18.7488079825307,-21.5133898805874,
-15.1675180882926));
#60626=CARTESIAN_POINT('Ctrl Pts',(-18.8344006857365,-21.510030434202,-15.171771666178));
#60627=CARTESIAN_POINT('Ctrl Pts',(-18.9183340073703,-21.5067361172402,
-15.175942780156));
#60628=CARTESIAN_POINT('Ctrl Pts',(-19.0021674095972,-21.4993040188572,
-15.1801138941339));
#60629=CARTESIAN_POINT('Ctrl Pts',(-19.0854634797585,-21.4877589440631,
-15.1842850081119));
#60630=CARTESIAN_POINT('Ctrl Pts',(-19.1687315991189,-21.4762177433303,
-15.1884547224322));
#60631=CARTESIAN_POINT('Ctrl Pts',(-19.2514622892086,-21.4605663702897,
-15.1926244367526));
#60632=CARTESIAN_POINT('Ctrl Pts',(-19.3332238803095,-21.4408814237056,
-15.196794151073));
#60633=CARTESIAN_POINT('Ctrl Pts',(-19.4149825619821,-21.4211971775964,
-15.200963717017));
#60634=CARTESIAN_POINT('Ctrl Pts',(-19.495771766177,-21.3974797518312,-15.2051332829611));
#60635=CARTESIAN_POINT('Ctrl Pts',(-19.5751719705271,-21.3698564299808,
-15.2093028489051));
#60636=CARTESIAN_POINT('Ctrl Pts',(-19.6573637881113,-21.3412619062112,
-15.213619011644));
#60637=CARTESIAN_POINT('Ctrl Pts',(-19.7380666159167,-21.3084818866879,
-15.217935174383));
#60638=CARTESIAN_POINT('Ctrl Pts',(-19.8168362586923,-21.2717124039116,
-15.2222513371219));
#60639=CARTESIAN_POINT('Ctrl Pts',(-19.8930399886395,-21.2361406831693,
-15.2264269013136));
#60640=CARTESIAN_POINT('Ctrl Pts',(-19.9674341519885,-21.1968356830556,
-15.2306024655052));
#60641=CARTESIAN_POINT('Ctrl Pts',(-20.0396421490702,-21.1540214755018,
-15.2347780296969));
#60642=CARTESIAN_POINT('Ctrl Pts',(-20.1154972004263,-21.1090448241057,
-15.2391644917094));
#60643=CARTESIAN_POINT('Ctrl Pts',(-20.188938948885,-21.0601954720668,-15.243550953722));
#60644=CARTESIAN_POINT('Ctrl Pts',(-20.259567662025,-21.0077828943212,-15.2479374157345));
#60645=CARTESIAN_POINT('Ctrl Pts',(-20.330196375165,-20.9553703165755,-15.252323877747));
#60646=CARTESIAN_POINT('Ctrl Pts',(-20.398011653933,-20.899394941135,-15.2567103397596));
#60647=CARTESIAN_POINT('Ctrl Pts',(-20.4626578964185,-20.8402112903883,
-15.2610968017721));
#60648=CARTESIAN_POINT('Ctrl Pts',(-20.5234100187943,-20.7845927075509,
-15.2652190348167));
#60649=CARTESIAN_POINT('Ctrl Pts',(-20.5816044022752,-20.7259204795934,
-15.2693412678613));
#60650=CARTESIAN_POINT('Ctrl Pts',(-20.6369112461382,-20.6644627847987,
-15.2734635009059));
#60651=CARTESIAN_POINT('Ctrl Pts',(-20.6921256485478,-20.6031078121671,
-15.2775788439313));
#60652=CARTESIAN_POINT('Ctrl Pts',(-20.7444617859852,-20.538976972769,-15.2816941869567));
#60653=CARTESIAN_POINT('Ctrl Pts',(-20.7936245240703,-20.4723771965695,
-15.2858095299821));
#60654=CARTESIAN_POINT('Ctrl Pts',(-20.8427410076358,-20.4058400804406,
-15.2899210011074));
#60655=CARTESIAN_POINT('Ctrl Pts',(-20.888689733586,-20.3368390147958,-15.2940324722326));
#60656=CARTESIAN_POINT('Ctrl Pts',(-20.9312146121388,-20.26571532236,-15.2981439433578));
#60657=CARTESIAN_POINT('Ctrl Pts',(-20.9737131282065,-20.1946357216972,
-15.3022528656552));
#60658=CARTESIAN_POINT('Ctrl Pts',(-21.0127917657816,-20.1214365120737,
-15.3063617879525));
#60659=CARTESIAN_POINT('Ctrl Pts',(-21.0482376124058,-20.0464881330222,
-15.3104707102499));
#60660=CARTESIAN_POINT('Ctrl Pts',(-21.0836728562216,-19.9715621730513,
-15.3145784034578));
#60661=CARTESIAN_POINT('Ctrl Pts',(-21.1154772648505,-19.8948885121031,
-15.3186860966657));
#60662=CARTESIAN_POINT('Ctrl Pts',(-21.1434845038947,-19.8168609284106,
-15.3227937898736));
#60663=CARTESIAN_POINT('Ctrl Pts',(-21.1715053065238,-19.7387955568538,
-15.3269034723903));
#60664=CARTESIAN_POINT('Ctrl Pts',(-21.1957251016683,-19.6593753990475,
-15.3310131549069));
#60665=CARTESIAN_POINT('Ctrl Pts',(-21.2160265895469,-19.5790119686115,
-15.3351228374236));
#60666=CARTESIAN_POINT('Ctrl Pts',(-21.2363332616042,-19.4986280166064,
-15.3392335693869));
#60667=CARTESIAN_POINT('Ctrl Pts',(-21.2527195357624,-19.4173007774455,
-15.3433443013502));
#60668=CARTESIAN_POINT('Ctrl Pts',(-21.265119175788,-19.3354523672614,-15.3474550333135));
#60669=CARTESIAN_POINT('Ctrl Pts',(-21.277533866187,-19.2535046115213,-15.3515707547806));
#60670=CARTESIAN_POINT('Ctrl Pts',(-21.2859522113271,-19.1710348943524,
-15.3556864762477));
#60671=CARTESIAN_POINT('Ctrl Pts',(-21.2903598951029,-19.0884700945603,
-15.3598021977147));
#60672=CARTESIAN_POINT('Ctrl Pts',(-21.2928257992759,-19.0422787399392,
-15.362104761886));
#60673=CARTESIAN_POINT('Ctrl Pts',(-21.294037342402,-18.9960576424384,-15.3644073260573));
#60674=CARTESIAN_POINT('Ctrl Pts',(-21.2939991231355,-18.9498811452879,
-15.3667098902285));
#60675=CARTESIAN_POINT('Origin',(-18.734,-18.952,1.76670989022851));
#60676=CARTESIAN_POINT('',(-17.1770150863476,-16.9251769922837,-14.0501277838374));
#60677=CARTESIAN_POINT('',(-17.17189441536,-16.9185281387053,-14.1167030432336));
#60678=CARTESIAN_POINT('',(-17.1744641548914,-16.9218650419685,1.76670989022851));
#60679=CARTESIAN_POINT('',(-21.2941233742573,-18.953130183291,-14.6332901097715));
#60680=CARTESIAN_POINT('Ctrl Pts',(-17.17189441536,-16.9185281387053,-14.1167030432336));
#60681=CARTESIAN_POINT('Ctrl Pts',(-16.5081486518363,-17.4296845150534,
-14.1585606262999));
#60682=CARTESIAN_POINT('Ctrl Pts',(-15.7210164188585,-19.1757114375145,
-14.2428101449267));
#60683=CARTESIAN_POINT('Ctrl Pts',(-17.2790525445471,-21.6065091564228,
-14.369451599114));
#60684=CARTESIAN_POINT('Ctrl Pts',(-20.1784866529944,-21.6122160192327,
-14.4966274057954));
#60685=CARTESIAN_POINT('Ctrl Pts',(-21.2671017221445,-19.9284206152422,
-14.5845735760146));
#60686=CARTESIAN_POINT('Ctrl Pts',(-21.2979708163172,-19.0164624131716,
-14.6301278106733));
#60687=CARTESIAN_POINT('Ctrl Pts',(-21.2976210374783,-18.9531317273574,
-14.6332901097715));
#60688=CARTESIAN_POINT('Ctrl Pts',(-21.2939997505486,-18.9531301287165,
-14.6332901097715));
#60689=CARTESIAN_POINT('Ctrl Pts',(-21.2940362985033,-18.8703406609988,
-14.6374299052976));
#60690=CARTESIAN_POINT('Ctrl Pts',(-21.2900525381051,-18.7873874928942,
-14.6415697008237));
#60691=CARTESIAN_POINT('Ctrl Pts',(-21.2820270867845,-18.7046986352398,
-14.6457094963498));
#60692=CARTESIAN_POINT('Ctrl Pts',(-21.2740124509524,-18.6221212131097,
-14.6498437128863));
#60693=CARTESIAN_POINT('Ctrl Pts',(-21.2619669829652,-18.5398078587026,
-14.6539779294227));
#60694=CARTESIAN_POINT('Ctrl Pts',(-21.2459213201025,-18.4581869973214,
-14.6581121459591));
#60695=CARTESIAN_POINT('Ctrl Pts',(-21.2298921267196,-18.3766499126674,
-14.6622421190812));
#60696=CARTESIAN_POINT('Ctrl Pts',(-21.2098709847548,-18.2958043686398,
-14.6663720922033));
#60697=CARTESIAN_POINT('Ctrl Pts',(-21.1859402178852,-18.2160725797221,
-14.6705020653254));
#60698=CARTESIAN_POINT('Ctrl Pts',(-21.1620224032905,-18.1363839447932,
-14.6746298031432));
#60699=CARTESIAN_POINT('Ctrl Pts',(-21.1341992976673,-18.0578083185522,
-14.6787575409609));
#60700=CARTESIAN_POINT('Ctrl Pts',(-21.1026037847562,-17.9807553805356,
-14.6828852787787));
#60701=CARTESIAN_POINT('Ctrl Pts',(-21.0710154147149,-17.9037198620526,
-14.6870120834293));
#60702=CARTESIAN_POINT('Ctrl Pts',(-21.0356565094079,-17.8282067834225,
-14.69113888808));
#60703=CARTESIAN_POINT('Ctrl Pts',(-20.9967085276618,-17.7546069488901,
-14.6952656927306));
#60704=CARTESIAN_POINT('Ctrl Pts',(-20.9577570758465,-17.6810005569824,
-14.6993928650588));
#60705=CARTESIAN_POINT('Ctrl Pts',(-20.9152161348637,-17.6093081624228,
-14.703520037387));
#60706=CARTESIAN_POINT('Ctrl Pts',(-20.8693129406038,-17.5398956675621,
-14.7076472097152));
#60707=CARTESIAN_POINT('Ctrl Pts',(-20.8233622278895,-17.4704113176916,
-14.7117786544444));
#60708=CARTESIAN_POINT('Ctrl Pts',(-20.7740425759674,-17.4032119705945,
-14.7159100991735));
#60709=CARTESIAN_POINT('Ctrl Pts',(-20.7216239583869,-17.3386336435743,
-14.7200415439027));
#60710=CARTESIAN_POINT('Ctrl Pts',(-20.6691749218115,-17.2740178411706,
-14.7241753861463));
#60711=CARTESIAN_POINT('Ctrl Pts',(-20.6136236562292,-17.2120264344647,
-14.7283092283899));
#60712=CARTESIAN_POINT('Ctrl Pts',(-20.5552780488236,-17.1529596255578,
-14.7324430706336));
#60713=CARTESIAN_POINT('Ctrl Pts',(-20.4968364594113,-17.0937956482246,
-14.7365837132944));
#60714=CARTESIAN_POINT('Ctrl Pts',(-20.4355917013472,-17.0375661867587,
-14.7407243559553));
#60715=CARTESIAN_POINT('Ctrl Pts',(-20.3718854170603,-16.9845317383548,
-14.7448649986162));
#60716=CARTESIAN_POINT('Ctrl Pts',(-20.3405294527256,-16.9584284066148,
-14.7469030054636));
#60717=CARTESIAN_POINT('Ctrl Pts',(-20.3085776248464,-16.9330984310457,
-14.7489410123109));
#60718=CARTESIAN_POINT('Ctrl Pts',(-20.2760730898183,-16.9085689182999,
-14.7509790191583));
#60719=CARTESIAN_POINT('Ctrl Pts',(-20.2093316088542,-16.8582025307612,
-14.7551636535514));
#60720=CARTESIAN_POINT('Ctrl Pts',(-20.1399957688999,-16.811015665153,-14.7593482879444));
#60721=CARTESIAN_POINT('Ctrl Pts',(-20.0684012262925,-16.767286433587,-14.7635329223375));
#60722=CARTESIAN_POINT('Ctrl Pts',(-19.9969085896549,-16.7236194451695,
-14.7677116004214));
#60723=CARTESIAN_POINT('Ctrl Pts',(-19.9231640255692,-16.6834005528598,
-14.7718902785053));
#60724=CARTESIAN_POINT('Ctrl Pts',(-19.8475347050067,-16.6468664982814,
-14.7760689565893));
#60725=CARTESIAN_POINT('Ctrl Pts',(-19.7705497832269,-16.6096775970311,
-14.7803225344747));
#60726=CARTESIAN_POINT('Ctrl Pts',(-19.6916122567006,-16.5763072247155,
-14.7845761123601));
#60727=CARTESIAN_POINT('Ctrl Pts',(-19.6111386006651,-16.5469578225688,
-14.7888296902456));
#60728=CARTESIAN_POINT('Ctrl Pts',(-19.5322250834833,-16.5181774158532,
-14.7930008042235));
#60729=CARTESIAN_POINT('Ctrl Pts',(-19.4518349191003,-16.4932636267838,
-14.7971719182015));
#60730=CARTESIAN_POINT('Ctrl Pts',(-19.3703822558338,-16.4723593759458,
-14.8013430321794));
#60731=CARTESIAN_POINT('Ctrl Pts',(-19.288956924795,-16.4514621397311,-14.8055127464998));
#60732=CARTESIAN_POINT('Ctrl Pts',(-19.2064702481718,-16.4345718839471,
-14.8096824608202));
#60733=CARTESIAN_POINT('Ctrl Pts',(-19.1233507011893,-16.4217814261445,
-14.8138521751405));
#60734=CARTESIAN_POINT('Ctrl Pts',(-19.0402341119571,-16.4089914234813,
-14.8180217410846));
#60735=CARTESIAN_POINT('Ctrl Pts',(-18.9564851519522,-16.4003009978601,
-14.8221913070286));
#60736=CARTESIAN_POINT('Ctrl Pts',(-18.87254027672,-16.3957514612764,-14.8263608729727));
#60737=CARTESIAN_POINT('Ctrl Pts',(-18.7856440032318,-16.3910419685989,
-14.8306770357116));
#60738=CARTESIAN_POINT('Ctrl Pts',(-18.6985383080789,-16.3907699986349,
-14.8349931984505));
#60739=CARTESIAN_POINT('Ctrl Pts',(-18.611708547389,-16.3949226056652,-14.8393093611894));
#60740=CARTESIAN_POINT('Ctrl Pts',(-18.5277072570206,-16.3989399419582,
-14.8434849253811));
#60741=CARTESIAN_POINT('Ctrl Pts',(-18.4439646643006,-16.4070979281598,
-14.8476604895728));
#60742=CARTESIAN_POINT('Ctrl Pts',(-18.3609142114861,-16.4193320402372,
-14.8518360537644));
#60743=CARTESIAN_POINT('Ctrl Pts',(-18.2736690777338,-16.4321840682319,
-14.856222515777));
#60744=CARTESIAN_POINT('Ctrl Pts',(-18.1871884138653,-16.4495346990029,
-14.8606089777895));
#60745=CARTESIAN_POINT('Ctrl Pts',(-18.1019594530764,-16.471249156597,-14.864995439802));
#60746=CARTESIAN_POINT('Ctrl Pts',(-18.0167304922876,-16.4929636141912,
-14.8693819018146));
#60747=CARTESIAN_POINT('Ctrl Pts',(-17.932753766134,-16.5190416538915,-14.8737683638271));
#60748=CARTESIAN_POINT('Ctrl Pts',(-17.8504927560606,-16.549290082031,-14.8781548258397));
#60749=CARTESIAN_POINT('Ctrl Pts',(-17.7720269461594,-16.5781429664058,
-14.8823389137096));
#60750=CARTESIAN_POINT('Ctrl Pts',(-17.6948300019267,-16.6108972906705,
-14.8865230015795));
#60751=CARTESIAN_POINT('Ctrl Pts',(-17.6193172941295,-16.6474214126584,
-14.8907070894494));
#60752=CARTESIAN_POINT('Ctrl Pts',(-17.5409561860664,-16.6853232539975,
-14.8950490044897));
#60753=CARTESIAN_POINT('Ctrl Pts',(-17.4644093908721,-16.7272848596456,
-14.89939091953));
#60754=CARTESIAN_POINT('Ctrl Pts',(-17.3901227433324,-16.7731025909852,
-14.9037328345703));
#60755=CARTESIAN_POINT('Ctrl Pts',(-17.3158360957927,-16.8189203223247,
-14.9080747496106));
#60756=CARTESIAN_POINT('Ctrl Pts',(-17.2438101074633,-16.8685939536001,
-14.9124166646509));
#60757=CARTESIAN_POINT('Ctrl Pts',(-17.1744641548914,-16.9218650419685,
-14.9167585796912));
#60758=CARTESIAN_POINT('',(-21.2936354977614,-18.9514398261094,-14.566709915054));
#60759=CARTESIAN_POINT('Ctrl Pts',(-21.2939999386838,-18.9514396975034,
-14.566709917474));
#60760=CARTESIAN_POINT('Ctrl Pts',(-21.2939802627005,-18.8615409084184,
-14.571157199273));
#60761=CARTESIAN_POINT('Ctrl Pts',(-21.2892209204008,-18.7717655181781,
-14.575604481072));
#60762=CARTESIAN_POINT('Ctrl Pts',(-21.2797861099468,-18.6826060832129,
-14.5800517628709));
#60763=CARTESIAN_POINT('Ctrl Pts',(-21.2703167670437,-18.5931203148612,
-14.5845153222128));
#60764=CARTESIAN_POINT('Ctrl Pts',(-21.2561377674616,-18.5042553694628,
-14.5889788815547));
#60765=CARTESIAN_POINT('Ctrl Pts',(-21.2373647797459,-18.4164957707656,
-14.5934424408966));
#60766=CARTESIAN_POINT('Ctrl Pts',(-21.2185553401018,-18.3285657673013,
-14.5979146672311));
#60767=CARTESIAN_POINT('Ctrl Pts',(-21.1951342035189,-18.2417457397356,
-14.6023868935656));
#60768=CARTESIAN_POINT('Ctrl Pts',(-21.1672666877164,-18.1565044145631,
-14.6068591199));
#60769=CARTESIAN_POINT('Ctrl Pts',(-21.139316159677,-18.0710091710603,-14.6113446681795));
#60770=CARTESIAN_POINT('Ctrl Pts',(-21.1068928974786,-17.9871023685111,
-14.6158302164589));
#60771=CARTESIAN_POINT('Ctrl Pts',(-21.0702104967804,-17.9052333045357,
-14.6203157647383));
#60772=CARTESIAN_POINT('Ctrl Pts',(-21.0568477853901,-17.875409938211,-14.6219497659472));
#60773=CARTESIAN_POINT('Ctrl Pts',(-21.0429203172351,-17.8458567318452,
-14.6235837671561));
#60774=CARTESIAN_POINT('Ctrl Pts',(-21.0284398795323,-17.8165945044999,
-14.625217768365));
#60775=CARTESIAN_POINT('Ctrl Pts',(-20.9913558570061,-17.7416547050056,
-14.629402402758));
#60776=CARTESIAN_POINT('Ctrl Pts',(-20.9505274948144,-17.6683941847451,
-14.6335870371511));
#60777=CARTESIAN_POINT('Ctrl Pts',(-20.9061301751471,-17.5972120083883,
-14.6377716715441));
#60778=CARTESIAN_POINT('Ctrl Pts',(-20.8617960495691,-17.526131151049,-14.641950349628));
#60779=CARTESIAN_POINT('Ctrl Pts',(-20.8139032983065,-17.4571231485616,
-14.646129027712));
#60780=CARTESIAN_POINT('Ctrl Pts',(-20.7626740190629,-17.3905642106128,
-14.6503077057959));
#60781=CARTESIAN_POINT('Ctrl Pts',(-20.7105264918066,-17.3228122515362,
-14.6545612836814));
#60782=CARTESIAN_POINT('Ctrl Pts',(-20.6549218593555,-17.2575984516732,
-14.6588148615668));
#60783=CARTESIAN_POINT('Ctrl Pts',(-20.5961416680529,-17.1952904599504,
-14.6630684394522));
#60784=CARTESIAN_POINT('Ctrl Pts',(-20.5385010454588,-17.1341904302312,
-14.6672395534302));
#60785=CARTESIAN_POINT('Ctrl Pts',(-20.4778072242624,-17.0758848946115,
-14.6714106674081));
#60786=CARTESIAN_POINT('Ctrl Pts',(-20.4143663508876,-17.0206872529793,
-14.6755817813861));
#60787=CARTESIAN_POINT('Ctrl Pts',(-20.3509467657106,-16.9655081334487,
-14.6797514957065));
#60788=CARTESIAN_POINT('Ctrl Pts',(-20.2847823058332,-16.9134351384329,
-14.6839212100268));
#60789=CARTESIAN_POINT('Ctrl Pts',(-20.2162143833073,-16.8647433023423,
-14.6880909243472));
#60790=CARTESIAN_POINT('Ctrl Pts',(-20.1476489007224,-16.8160531989162,
-14.6922604902913));
#60791=CARTESIAN_POINT('Ctrl Pts',(-20.0766805011099,-16.7707442808556,
-14.6964300562353));
#60792=CARTESIAN_POINT('Ctrl Pts',(-20.003680817563,-16.729049118511,-14.7005996221794));
#60793=CARTESIAN_POINT('Ctrl Pts',(-19.9281145551974,-16.685888005695,-14.7049157849183));
#60794=CARTESIAN_POINT('Ctrl Pts',(-19.850371969323,-16.6465997576133,-14.7092319476572));
#60795=CARTESIAN_POINT('Ctrl Pts',(-19.7708927266887,-16.6113903628883,
-14.7135481103961));
#60796=CARTESIAN_POINT('Ctrl Pts',(-19.6940025120234,-16.5773279104931,
-14.7177236745878));
#60797=CARTESIAN_POINT('Ctrl Pts',(-19.6154875027973,-16.5470827802972,
-14.7218992387795));
#60798=CARTESIAN_POINT('Ctrl Pts',(-19.5357640795052,-16.5207915842497,
-14.7260748029712));
#60799=CARTESIAN_POINT('Ctrl Pts',(-19.4520140156271,-16.4931724823912,
-14.7304612649837));
#60800=CARTESIAN_POINT('Ctrl Pts',(-19.3669308187544,-16.4699173921691,
-14.7348477269962));
#60801=CARTESIAN_POINT('Ctrl Pts',(-19.2810104439706,-16.4511242385542,
-14.7392341890088));
#60802=CARTESIAN_POINT('Ctrl Pts',(-19.1950900691869,-16.4323310849393,
-14.7436206510213));
#60803=CARTESIAN_POINT('Ctrl Pts',(-19.1083331013483,-16.4179998874471,
-14.7480071130339));
#60804=CARTESIAN_POINT('Ctrl Pts',(-19.021240449396,-16.4081657042506,-14.7523935750464));
#60805=CARTESIAN_POINT('Ctrl Pts',(-18.9381783893877,-16.3987866407305,
-14.7565770344169));
#60806=CARTESIAN_POINT('Ctrl Pts',(-18.854501943096,-16.3934626556781,-14.7607604937874));
#60807=CARTESIAN_POINT('Ctrl Pts',(-18.7706412277849,-16.3922622360042,
-14.7649439531578));
#60808=CARTESIAN_POINT('Ctrl Pts',(-18.6868897531745,-16.3910633800504,
-14.7691219629679));
#60809=CARTESIAN_POINT('Ctrl Pts',(-18.6029549415358,-16.3939774328896,
-14.773299972778));
#60810=CARTESIAN_POINT('Ctrl Pts',(-18.5192731319703,-16.4010212913185,
-14.7774779825881));
#60811=CARTESIAN_POINT('Ctrl Pts',(-18.4356752189539,-16.4080580878134,
-14.781651803667));
#60812=CARTESIAN_POINT('Ctrl Pts',(-18.3523302600701,-16.4192164297761,
-14.7858256247459));
#60813=CARTESIAN_POINT('Ctrl Pts',(-18.2696743384303,-16.4344611859977,
-14.7899994458248));
#60814=CARTESIAN_POINT('Ctrl Pts',(-18.1870764857767,-16.4496952321877,
-14.7941703346327));
#60815=CARTESIAN_POINT('Ctrl Pts',(-18.1051671597325,-16.4690099061388,
-14.7983412234407));
#60816=CARTESIAN_POINT('Ctrl Pts',(-18.0243757041687,-16.4923184436261,
-14.8025121122486));
#60817=CARTESIAN_POINT('Ctrl Pts',(-17.9435959999426,-16.5156235908231,
-14.8066823943894));
#60818=CARTESIAN_POINT('Ctrl Pts',(-17.8639342884434,-16.5429213326383,
-14.8108526765302));
#60819=CARTESIAN_POINT('Ctrl Pts',(-17.7858071130399,-16.5740743810795,
-14.8150229586709));
#60820=CARTESIAN_POINT('Ctrl Pts',(-17.7076898405936,-16.6052234807372,
-14.8191927122104));
#60821=CARTESIAN_POINT('Ctrl Pts',(-17.631107142899,-16.6402267397327,-14.82336246575));
#60822=CARTESIAN_POINT('Ctrl Pts',(-17.5564562226973,-16.6788984508967,
-14.8275322192895));
#60823=CARTESIAN_POINT('Ctrl Pts',(-17.4817531859644,-16.7175971601933,
-14.831704883886));
#60824=CARTESIAN_POINT('Ctrl Pts',(-17.4089850280066,-16.7599692220366,
-14.8358775484826));
#60825=CARTESIAN_POINT('Ctrl Pts',(-17.3385243273809,-16.8057829450104,
-14.8400502130792));
#60826=CARTESIAN_POINT('Ctrl Pts',(-17.2823110146712,-16.8423329808893,
-14.8433791510222));
#60827=CARTESIAN_POINT('Ctrl Pts',(-17.2275659250877,-16.8810726238427,
-14.8467080889651));
#60828=CARTESIAN_POINT('Ctrl Pts',(-17.1744641548915,-16.9218650419685,
-14.8500370269081));
#60829=CARTESIAN_POINT('Ctrl Pts',(-17.1770150863476,-16.9251769922837,
-14.0501277838374));
#60830=CARTESIAN_POINT('Ctrl Pts',(-16.8231471804876,-17.1976900874761,
-14.0722567031047));
#60831=CARTESIAN_POINT('Ctrl Pts',(-15.9876142224497,-18.2487089372057,
-14.1367775579324));
#60832=CARTESIAN_POINT('Ctrl Pts',(-16.2435266831926,-20.6727072634931,
-14.2436903483206));
#60833=CARTESIAN_POINT('Ctrl Pts',(-18.8327965299441,-21.9774801394222,
-14.3708661550021));
#60834=CARTESIAN_POINT('Ctrl Pts',(-20.9482575115022,-20.7321304478324,
-14.478539335638));
#60835=CARTESIAN_POINT('Ctrl Pts',(-21.2889974874197,-19.4133916920799,
-14.5438205807135));
#60836=CARTESIAN_POINT('Ctrl Pts',(-21.2898969963344,-18.9514411453738,
-14.5667098902285));
#60837=CARTESIAN_POINT('Origin',(-18.734,-18.952,1.76670989022851));
#60838=CARTESIAN_POINT('',(-17.1744641548914,-16.9218650419685,-13.250188010165));
#60839=CARTESIAN_POINT('',(-17.1744641548914,-16.9218650419685,-13.3166223748392));
#60840=CARTESIAN_POINT('',(-17.1744641548914,-16.9218650419685,1.76670989022851));
#60841=CARTESIAN_POINT('',(-21.2939989424941,-18.949673107456,-13.8332901097715));
#60842=CARTESIAN_POINT('Ctrl Pts',(-17.1744641548914,-16.9218650419685,
-13.3166223748392));
#60843=CARTESIAN_POINT('Ctrl Pts',(-17.1077897102854,-16.9730838961163,
-13.3207986479985));
#60844=CARTESIAN_POINT('Ctrl Pts',(-17.0436958183771,-17.027548772347,-13.3249749211578));
#60845=CARTESIAN_POINT('Ctrl Pts',(-16.9824997154987,-17.0849577526495,
-13.329151194317));
#60846=CARTESIAN_POINT('Ctrl Pts',(-16.9211959283922,-17.1424677531384,
-13.3333348162899));
#60847=CARTESIAN_POINT('Ctrl Pts',(-16.8628004366934,-17.202931875454,-13.3375184382627));
#60848=CARTESIAN_POINT('Ctrl Pts',(-16.807592344652,-17.2660125903742,-13.3417020602355));
#60849=CARTESIAN_POINT('Ctrl Pts',(-16.762095721873,-17.3179969894946,-13.3451497553778));
#60850=CARTESIAN_POINT('Ctrl Pts',(-16.7187630874481,-17.3717576702114,
-13.3485974505202));
#60851=CARTESIAN_POINT('Ctrl Pts',(-16.677728404917,-17.4270911085396,-13.3520451456625));
#60852=CARTESIAN_POINT('Ctrl Pts',(-16.6279226254792,-17.4942519796595,
-13.3562297800555));
#60853=CARTESIAN_POINT('Ctrl Pts',(-16.5813179797007,-17.5639804959206,
-13.3604144144486));
#60854=CARTESIAN_POINT('Ctrl Pts',(-16.5381897594127,-17.6359386840531,
-13.3645990488416));
#60855=CARTESIAN_POINT('Ctrl Pts',(-16.495122926808,-17.7077944486115,-13.3687777269256));
#60856=CARTESIAN_POINT('Ctrl Pts',(-16.4555229253634,-17.7818731899371,
-13.3729564050095));
#60857=CARTESIAN_POINT('Ctrl Pts',(-16.4196234139921,-17.8578057676361,
-13.3771350830935));
#60858=CARTESIAN_POINT('Ctrl Pts',(-16.3830804296801,-17.9350993822185,
-13.3813886609789));
#60859=CARTESIAN_POINT('Ctrl Pts',(-16.350372190068,-18.0143135596368,-13.3856422388643));
#60860=CARTESIAN_POINT('Ctrl Pts',(-16.3216976420462,-18.0950301441646,
-13.3898958167498));
#60861=CARTESIAN_POINT('Ctrl Pts',(-16.2935790060915,-18.1741818801959,
-13.3940669307277));
#60862=CARTESIAN_POINT('Ctrl Pts',(-16.2693392165557,-18.2547778355446,
-13.3982380447057));
#60863=CARTESIAN_POINT('Ctrl Pts',(-16.2491177212505,-18.3364026797033,
-13.4024091586836));
#60864=CARTESIAN_POINT('Ctrl Pts',(-16.2289030114633,-18.4180001338573,
-13.406578873004));
#60865=CARTESIAN_POINT('Ctrl Pts',(-16.2127040285388,-18.5006253449796,
-13.4107485873244));
#60866=CARTESIAN_POINT('Ctrl Pts',(-16.2006099990479,-18.5838490756822,
-13.4149183016447));
#60867=CARTESIAN_POINT('Ctrl Pts',(-16.1885163999146,-18.6670698449272,
-13.4190878675888));
#60868=CARTESIAN_POINT('Ctrl Pts',(-16.1805275291,-18.7508886360331,-13.4232574335328));
#60869=CARTESIAN_POINT('Ctrl Pts',(-16.1766810426044,-18.8348686628402,
-13.4274269994769));
#60870=CARTESIAN_POINT('Ctrl Pts',(-16.1726993183887,-18.9218013237893,
-13.4317431622158));
#60871=CARTESIAN_POINT('Ctrl Pts',(-16.1731567148617,-19.0089062426184,
-13.4360593249547));
#60872=CARTESIAN_POINT('Ctrl Pts',(-16.1780362227548,-19.095698188612,-13.4403754876936));
#60873=CARTESIAN_POINT('Ctrl Pts',(-16.1827567811915,-19.1796628960938,
-13.4445510518853));
#60874=CARTESIAN_POINT('Ctrl Pts',(-16.1916156782437,-19.2633342443402,
-13.448726616077));
#60875=CARTESIAN_POINT('Ctrl Pts',(-16.2045447628248,-19.346279346564,-13.4529021802687));
#60876=CARTESIAN_POINT('Ctrl Pts',(-16.2181268647321,-19.4334138087178,
-13.4572886422812));
#60877=CARTESIAN_POINT('Ctrl Pts',(-16.236201010622,-19.5197461599059,-13.4616751042937));
#60878=CARTESIAN_POINT('Ctrl Pts',(-16.2586283495454,-19.6047903125243,
-13.4660615663063));
#60879=CARTESIAN_POINT('Ctrl Pts',(-16.2810556884688,-19.6898344651427,
-13.4704480283188));
#60880=CARTESIAN_POINT('Ctrl Pts',(-16.3078359712666,-19.7735898897036,
-13.4748344903314));
#60881=CARTESIAN_POINT('Ctrl Pts',(-16.3387721302028,-19.8555947386669,
-13.4792209523439));
#60882=CARTESIAN_POINT('Ctrl Pts',(-16.3682848706079,-19.9338264229691,
-13.4834055867369));
#60883=CARTESIAN_POINT('Ctrl Pts',(-16.4016893071736,-20.0107562780699,
-13.48759022113));
#60884=CARTESIAN_POINT('Ctrl Pts',(-16.4388502681124,-20.0859698885844,
-13.491774855523));
#60885=CARTESIAN_POINT('Ctrl Pts',(-16.4759583350229,-20.1610764418341,
-13.495953533607));
#60886=CARTESIAN_POINT('Ctrl Pts',(-16.5168121035543,-20.2344711938782,
-13.5001322116909));
#60887=CARTESIAN_POINT('Ctrl Pts',(-16.5612276601911,-20.3057578658539,
-13.5043108897749));
#60888=CARTESIAN_POINT('Ctrl Pts',(-16.6064393337596,-20.3783223001918,
-13.5085644676603));
#60889=CARTESIAN_POINT('Ctrl Pts',(-16.6553415713119,-20.4487018853352,
-13.5128180455458));
#60890=CARTESIAN_POINT('Ctrl Pts',(-16.707690456235,-20.5165029986698,-13.5170716234312));
#60891=CARTESIAN_POINT('Ctrl Pts',(-16.7590244558735,-20.5829896551195,
-13.5212427374092));
#60892=CARTESIAN_POINT('Ctrl Pts',(-16.8136723614036,-20.6469965440965,
-13.5254138513871));
#60893=CARTESIAN_POINT('Ctrl Pts',(-16.8713604260518,-20.7081816015327,
-13.5295849653651));
#60894=CARTESIAN_POINT('Ctrl Pts',(-16.9290291329127,-20.769346127732,-13.5337546796854));
#60895=CARTESIAN_POINT('Ctrl Pts',(-16.9897356575244,-20.8276903684962,
-13.5379243940058));
#60896=CARTESIAN_POINT('Ctrl Pts',(-17.0531673758224,-20.8829069603428,
-13.5420941083262));
#60897=CARTESIAN_POINT('Ctrl Pts',(-17.1165968369475,-20.9381215873459,
-13.5462636742702));
#60898=CARTESIAN_POINT('Ctrl Pts',(-17.1827509514054,-20.9902084853113,
-13.5504332402143));
#60899=CARTESIAN_POINT('Ctrl Pts',(-17.251282833637,-21.0388995674379,-13.5546028061583));
#60900=CARTESIAN_POINT('Ctrl Pts',(-17.3222242123048,-21.0893025679452,
-13.5589189688972));
#60901=CARTESIAN_POINT('Ctrl Pts',(-17.3957132444234,-21.1360662103826,
-13.5632351316361));
#60902=CARTESIAN_POINT('Ctrl Pts',(-17.4713327209561,-21.1789421506703,
-13.5675512943751));
#60903=CARTESIAN_POINT('Ctrl Pts',(-17.5444889009946,-21.2204214117129,
-13.5717268585667));
#60904=CARTESIAN_POINT('Ctrl Pts',(-17.619638416544,-21.2582621950959,-13.5759024227584));
#60905=CARTESIAN_POINT('Ctrl Pts',(-17.6963803894315,-21.2922874916906,
-13.5800779869501));
#60906=CARTESIAN_POINT('Ctrl Pts',(-17.7769984169327,-21.3280313251289,
-13.5844644489626));
#60907=CARTESIAN_POINT('Ctrl Pts',(-17.8593734542579,-21.3595638930066,
-13.5888509109752));
#60908=CARTESIAN_POINT('Ctrl Pts',(-17.9430216212721,-21.3867388369977,
-13.5932373729877));
#60909=CARTESIAN_POINT('Ctrl Pts',(-18.0266697882863,-21.4139137809888,
-13.5976238350002));
#60910=CARTESIAN_POINT('Ctrl Pts',(-18.1115905049088,-21.4367310239951,
-13.6020102970128));
#60911=CARTESIAN_POINT('Ctrl Pts',(-18.1972887614197,-21.4551062794819,
-13.6063967590253));
#60912=CARTESIAN_POINT('Ctrl Pts',(-18.2790439141132,-21.4726360622251,
-13.6105813934184));
#60913=CARTESIAN_POINT('Ctrl Pts',(-18.3618109357871,-21.4861888889159,
-13.6147660278114));
#60914=CARTESIAN_POINT('Ctrl Pts',(-18.4451682027606,-21.4956541024486,
-13.6189506622044));
#60915=CARTESIAN_POINT('Ctrl Pts',(-18.5284068209818,-21.5051058434213,
-13.6231293402884));
#60916=CARTESIAN_POINT('Ctrl Pts',(-18.6122335625321,-21.5104814765753,
-13.6273080183723));
#60917=CARTESIAN_POINT('Ctrl Pts',(-18.6962156707026,-21.5117211458398,
-13.6314866964562));
#60918=CARTESIAN_POINT('Ctrl Pts',(-18.7817030978056,-21.512983035285,-13.6357402743417));
#60919=CARTESIAN_POINT('Ctrl Pts',(-18.8673510447832,-21.5099591270342,
-13.6399938522271));
#60920=CARTESIAN_POINT('Ctrl Pts',(-18.9526965098726,-21.5026414559027,
-13.6442474301125));
#60921=CARTESIAN_POINT('Ctrl Pts',(-19.0363873865832,-21.4954656521054,
-13.6484185440905));
#60922=CARTESIAN_POINT('Ctrl Pts',(-19.1197869256869,-21.4841611267898,
-13.6525896580684));
#60923=CARTESIAN_POINT('Ctrl Pts',(-19.2024593314988,-21.4687729048787,
-13.6567607720464));
#60924=CARTESIAN_POINT('Ctrl Pts',(-19.2851039957867,-21.4533898466341,
-13.6609304863668));
#60925=CARTESIAN_POINT('Ctrl Pts',(-19.3670215594753,-21.4339258973911,
-13.6651002006872));
#60926=CARTESIAN_POINT('Ctrl Pts',(-19.4477843610403,-21.4104775544906,
-13.6692699150075));
#60927=CARTESIAN_POINT('Ctrl Pts',(-19.5285442887181,-21.3870300459828,
-13.6734394809516));
#60928=CARTESIAN_POINT('Ctrl Pts',(-19.6081490944209,-21.3595985548019,
-13.6776090468956));
#60929=CARTESIAN_POINT('Ctrl Pts',(-19.6861855970008,-21.3283296465062,
-13.6817786128397));
#60930=CARTESIAN_POINT('Ctrl Pts',(-19.766965766743,-21.2959613619692,-13.6860947755786));
#60931=CARTESIAN_POINT('Ctrl Pts',(-19.8460648087822,-21.2594809885576,
-13.6904109383175));
#60932=CARTESIAN_POINT('Ctrl Pts',(-19.9230480777099,-21.2191049091064,
-13.6947271010565));
#60933=CARTESIAN_POINT('Ctrl Pts',(-19.9975236247494,-21.1800440761966,
-13.6989026652482));
#60934=CARTESIAN_POINT('Ctrl Pts',(-20.0700187425842,-21.1373377246263,
-13.7030782294398));
#60935=CARTESIAN_POINT('Ctrl Pts',(-20.1401676067978,-21.0912271178144,
-13.7072537936315));
#60936=CARTESIAN_POINT('Ctrl Pts',(-20.2138595233798,-21.04278757387,-13.7116402556441));
#60937=CARTESIAN_POINT('Ctrl Pts',(-20.2849614681661,-20.9905911845414,
-13.7160267176566));
#60938=CARTESIAN_POINT('Ctrl Pts',(-20.3530884618265,-20.9349655954605,
-13.7204131796692));
#60939=CARTESIAN_POINT('Ctrl Pts',(-20.4212154554869,-20.8793400063797,
-13.7247996416817));
#60940=CARTESIAN_POINT('Ctrl Pts',(-20.4863671192074,-20.8202856635708,
-13.7291861036942));
#60941=CARTESIAN_POINT('Ctrl Pts',(-20.548204641978,-20.7581731691688,-13.7335725657068));
#60942=CARTESIAN_POINT('Ctrl Pts',(-20.6067777194386,-20.6993396360183,
-13.7377274633762));
#60943=CARTESIAN_POINT('Ctrl Pts',(-20.6626103382647,-20.6375286216454,
-13.7418823610455));
#60944=CARTESIAN_POINT('Ctrl Pts',(-20.7153787245626,-20.5730300274365,
-13.7460372587149));
#60945=CARTESIAN_POINT('Ctrl Pts',(-20.7677053791601,-20.5090713601742,
-13.7501573751423));
#60946=CARTESIAN_POINT('Ctrl Pts',(-20.8170185699061,-20.4424702805591,
-13.7542774915697));
#60947=CARTESIAN_POINT('Ctrl Pts',(-20.8630375889924,-20.3735480803185,
-13.7583976079971));
#60948=CARTESIAN_POINT('Ctrl Pts',(-20.909012526032,-20.3046919012951,-13.7625137777266));
#60949=CARTESIAN_POINT('Ctrl Pts',(-20.9516992900879,-20.233519404422,-13.7666299474561));
#60950=CARTESIAN_POINT('Ctrl Pts',(-20.9908578231796,-20.1603843618457,
-13.7707461171856));
#60951=CARTESIAN_POINT('Ctrl Pts',(-21.0299913601116,-20.0872960037352,
-13.7748596594307));
#60952=CARTESIAN_POINT('Ctrl Pts',(-21.0656009133713,-20.0122480031423,
-13.7789732016758));
#60953=CARTESIAN_POINT('Ctrl Pts',(-21.0974909394085,-19.9356211564083,
-13.7830867439209));
#60954=CARTESIAN_POINT('Ctrl Pts',(-21.1299241917561,-19.8576890200775,
-13.7872703577418));
#60955=CARTESIAN_POINT('Ctrl Pts',(-21.158509766141,-19.7781241832438,-13.7914539715627));
#60956=CARTESIAN_POINT('Ctrl Pts',(-21.1830923574769,-19.6973500013741,
-13.7956375853835));
#60957=CARTESIAN_POINT('Ctrl Pts',(-21.2072638620763,-19.6179265800633,
-13.7997512379815));
#60958=CARTESIAN_POINT('Ctrl Pts',(-21.227565151866,-19.5373344318,-13.8038648905795));
#60959=CARTESIAN_POINT('Ctrl Pts',(-21.2438990336339,-19.4559909135726,
-13.8079785431775));
#60960=CARTESIAN_POINT('Ctrl Pts',(-21.260649602877,-19.372572271641,-13.8121971376098));
#60961=CARTESIAN_POINT('Ctrl Pts',(-21.2732274574716,-19.2883639128976,
-13.8164157320421));
#60962=CARTESIAN_POINT('Ctrl Pts',(-21.2815840465261,-19.2038243949373,
-13.8206343264745));
#60963=CARTESIAN_POINT('Ctrl Pts',(-21.2899406355806,-19.119284876977,-13.8248529209068));
#60964=CARTESIAN_POINT('Ctrl Pts',(-21.2940759677847,-19.0344147354448,
-13.8290715153392));
#60965=CARTESIAN_POINT('Ctrl Pts',(-21.2939989424941,-18.949673107456,-13.8332901097715));
#60966=CARTESIAN_POINT('Ctrl Pts',(-21.294449633852,-18.9496726978033,-13.8332901097715));
#60967=CARTESIAN_POINT('Ctrl Pts',(-21.2961551522482,-18.7657813487039,
-13.8424428639771));
#60968=CARTESIAN_POINT('Ctrl Pts',(-21.1940976782198,-17.7320561538789,
-13.8939875537431));
#60969=CARTESIAN_POINT('Ctrl Pts',(-19.7898862958127,-16.1150306505046,
-13.9879241790696));
#60970=CARTESIAN_POINT('Ctrl Pts',(-17.8646300934828,-16.3924604551013,
-14.0732424026848));
#60971=CARTESIAN_POINT('Ctrl Pts',(-17.1803677713987,-16.9120027336387,
-14.1161686907394));
#60972=CARTESIAN_POINT('Ctrl Pts',(-17.17189441536,-16.9185281387053,-14.1167030432336));
#60973=CARTESIAN_POINT('',(-21.2939989173812,-18.9543543592142,-13.7667098774877));
#60974=CARTESIAN_POINT('Ctrl Pts',(-21.2935815865034,-18.9543537192076,
-13.7667098902285));
#60975=CARTESIAN_POINT('Ctrl Pts',(-21.2877697346816,-18.3145386563719,
-13.7985275695778));
#60976=CARTESIAN_POINT('Ctrl Pts',(-20.7208249375185,-16.8130884735802,
-13.8727371844876));
#60977=CARTESIAN_POINT('Ctrl Pts',(-18.6774626831344,-16.1321013561092,
-13.9672098156905));
#60978=CARTESIAN_POINT('Ctrl Pts',(-17.5010449702959,-16.675642108935,-14.0298647675442));
#60979=CARTESIAN_POINT('Ctrl Pts',(-17.1770150863476,-16.9251769922837,
-14.0501277838374));
#60980=CARTESIAN_POINT('Ctrl Pts',(-17.1744641548914,-16.9218650419685,
-13.250188010165));
#60981=CARTESIAN_POINT('Ctrl Pts',(-17.1058905228881,-16.9745428389373,
-13.2544909973061));
#60982=CARTESIAN_POINT('Ctrl Pts',(-17.0399075290738,-17.0307614250666,
-13.2587939844472));
#60983=CARTESIAN_POINT('Ctrl Pts',(-16.9768962778943,-17.0902302747756,
-13.2630969715882));
#60984=CARTESIAN_POINT('Ctrl Pts',(-16.915813603391,-17.1478789696017,-13.2672682577952));
#60985=CARTESIAN_POINT('Ctrl Pts',(-16.8575237492257,-17.2085815017709,
-13.2714395440022));
#60986=CARTESIAN_POINT('Ctrl Pts',(-16.8023405437521,-17.2720322190328,
-13.2756108302092));
#60987=CARTESIAN_POINT('Ctrl Pts',(-16.7471772277534,-17.3354600669916,
-13.2797806129752));
#60988=CARTESIAN_POINT('Ctrl Pts',(-16.695118638371,-17.4016337861567,-13.2839503957412));
#60989=CARTESIAN_POINT('Ctrl Pts',(-16.6464403094113,-17.4702123842368,
-13.2881201785072));
#60990=CARTESIAN_POINT('Ctrl Pts',(-16.5977649230779,-17.5387868367106,
-13.292289709208));
#60991=CARTESIAN_POINT('Ctrl Pts',(-16.5524696567119,-17.6097655036099,
-13.2964592399087));
#60992=CARTESIAN_POINT('Ctrl Pts',(-16.5107876396202,-17.6827770878784,
-13.3006287706095));
#60993=CARTESIAN_POINT('Ctrl Pts',(-16.4690956388469,-17.75580615989,-13.3047992999968));
#60994=CARTESIAN_POINT('Ctrl Pts',(-16.431018832745,-17.8308687160974,-13.3089698293841));
#60995=CARTESIAN_POINT('Ctrl Pts',(-16.3967445142583,-17.9075686741723,
-13.3131403587714));
#60996=CARTESIAN_POINT('Ctrl Pts',(-16.3624311151704,-17.9843560878291,
-13.3173156435208));
#60997=CARTESIAN_POINT('Ctrl Pts',(-16.3319290415391,-18.0627842076895,
-13.3214909282701));
#60998=CARTESIAN_POINT('Ctrl Pts',(-16.3053772882528,-18.1424373254742,
-13.3256662130195));
#60999=CARTESIAN_POINT('Ctrl Pts',(-16.2788072794351,-18.2221452083798,
-13.329844368466));
#61000=CARTESIAN_POINT('Ctrl Pts',(-16.2561931190383,-18.3030793228292,
-13.3340225239125));
#61001=CARTESIAN_POINT('Ctrl Pts',(-16.2376231931974,-18.3848114612778,
-13.338200679359));
#61002=CARTESIAN_POINT('Ctrl Pts',(-16.2190239659388,-18.4666725645667,
-13.3423854275016));
#61003=CARTESIAN_POINT('Ctrl Pts',(-16.2044817823337,-18.549333752171,-13.3465701756442));
#61004=CARTESIAN_POINT('Ctrl Pts',(-16.1940334157616,-18.6323599665996,
-13.3507549237868));
#61005=CARTESIAN_POINT('Ctrl Pts',(-16.1917823436453,-18.6502477383323,
-13.3516565163747));
#61006=CARTESIAN_POINT('Ctrl Pts',(-16.1897211040228,-18.6681524506455,
-13.3525581089627));
#61007=CARTESIAN_POINT('Ctrl Pts',(-16.1878497481281,-18.6860697555883,
-13.3534597015506));
#61008=CARTESIAN_POINT('Ctrl Pts',(-16.1791640730867,-18.7692307880738,
-13.3576443359436));
#61009=CARTESIAN_POINT('Ctrl Pts',(-16.1745407622114,-18.852972557727,-13.3618289703367));
#61010=CARTESIAN_POINT('Ctrl Pts',(-16.1740447460464,-18.9368640244713,
-13.3660136047297));
#61011=CARTESIAN_POINT('Ctrl Pts',(-16.173549435899,-19.0206360820962,-13.3701922828137));
#61012=CARTESIAN_POINT('Ctrl Pts',(-16.1771697541693,-19.1045569574875,
-13.3743709608976));
#61013=CARTESIAN_POINT('Ctrl Pts',(-16.1849189310736,-19.1881899744724,
-13.3785496389816));
#61014=CARTESIAN_POINT('Ctrl Pts',(-16.1928070064048,-19.2733220531809,
-13.382803216867));
#61015=CARTESIAN_POINT('Ctrl Pts',(-16.2049734659499,-19.3581553727241,
-13.3870567947524));
#61016=CARTESIAN_POINT('Ctrl Pts',(-16.2213767120001,-19.4422287349806,
-13.3913103726379));
#61017=CARTESIAN_POINT('Ctrl Pts',(-16.2374619491174,-19.5246721710542,
-13.3954814866158));
#61018=CARTESIAN_POINT('Ctrl Pts',(-16.2576210698179,-19.6063843810837,
-13.3996526005938));
#61019=CARTESIAN_POINT('Ctrl Pts',(-16.2817626998464,-19.686936884185,-13.4038237145717));
#61020=CARTESIAN_POINT('Ctrl Pts',(-16.3058962289179,-19.7674623571159,
-13.4079934288921));
#61021=CARTESIAN_POINT('Ctrl Pts',(-16.334009481308,-19.8468284556772,-13.4121631432125));
#61022=CARTESIAN_POINT('Ctrl Pts',(-16.3659607754928,-19.9246202913754,
-13.4163328575329));
#61023=CARTESIAN_POINT('Ctrl Pts',(-16.3979109327134,-20.0024093589062,
-13.4205024234769));
#61024=CARTESIAN_POINT('Ctrl Pts',(-16.4336986846161,-20.0786238497405,
-13.4246719894209));
#61025=CARTESIAN_POINT('Ctrl Pts',(-16.4731341172713,-20.1528686274167,
-13.428841555365));
#61026=CARTESIAN_POINT('Ctrl Pts',(-16.5139560510899,-20.2297237598851,
-13.4331577181039));
#61027=CARTESIAN_POINT('Ctrl Pts',(-16.5586866956795,-20.3044676260571,
-13.4374738808428));
#61028=CARTESIAN_POINT('Ctrl Pts',(-16.6070644247003,-20.3766912151497,
-13.4417900435817));
#61029=CARTESIAN_POINT('Ctrl Pts',(-16.6538662542869,-20.4465621284242,
-13.4459656077734));
#61030=CARTESIAN_POINT('Ctrl Pts',(-16.7040808906406,-20.514074089366,-13.4501411719651));
#61031=CARTESIAN_POINT('Ctrl Pts',(-16.75742932982,-20.5788891744013,-13.4543167361568));
#61032=CARTESIAN_POINT('Ctrl Pts',(-16.8134722718384,-20.6469779152985,
-13.4587031981693));
#61033=CARTESIAN_POINT('Ctrl Pts',(-16.8729735193545,-20.7120897510531,
-13.4630896601819));
#61034=CARTESIAN_POINT('Ctrl Pts',(-16.9355661330672,-20.7738769514621,
-13.4674761221944));
#61035=CARTESIAN_POINT('Ctrl Pts',(-16.9981587467798,-20.8356641518712,
-13.4718625842069));
#61036=CARTESIAN_POINT('Ctrl Pts',(-17.0638422427094,-20.8941263879947,
-13.4762490462195));
#61037=CARTESIAN_POINT('Ctrl Pts',(-17.1322119090441,-20.9489664272771,
-13.480635508232));
#61038=CARTESIAN_POINT('Ctrl Pts',(-17.1974357856827,-21.0012831950598,
-13.4848201426251));
#61039=CARTESIAN_POINT('Ctrl Pts',(-17.2653468510499,-21.0504984994761,
-13.4890047770181));
#61040=CARTESIAN_POINT('Ctrl Pts',(-17.3356178143268,-21.0963244303957,
-13.4931894114112));
#61041=CARTESIAN_POINT('Ctrl Pts',(-17.4057887555854,-21.1420851337748,
-13.4973680894951));
#61042=CARTESIAN_POINT('Ctrl Pts',(-17.4783125406379,-21.1844657972013,
-13.5015467675791));
#61043=CARTESIAN_POINT('Ctrl Pts',(-17.552829155194,-21.2232189316269,-13.505725445663));
#61044=CARTESIAN_POINT('Ctrl Pts',(-17.6286814265118,-21.2626666881356,
-13.5099790235484));
#61045=CARTESIAN_POINT('Ctrl Pts',(-17.7065982968803,-21.2983552879197,
-13.5142326014339));
#61046=CARTESIAN_POINT('Ctrl Pts',(-17.7861694556149,-21.3300700702735,
-13.5184861793193));
#61047=CARTESIAN_POINT('Ctrl Pts',(-17.864197972167,-21.361169999685,-13.5226572932973));
#61048=CARTESIAN_POINT('Ctrl Pts',(-17.9438167592515,-21.3884486389203,
-13.5268284072752));
#61049=CARTESIAN_POINT('Ctrl Pts',(-18.0246160731019,-21.4117508906917,
-13.5309995212532));
#61050=CARTESIAN_POINT('Ctrl Pts',(-18.1053882739622,-21.4350453231675,
-13.5351692355736));
#61051=CARTESIAN_POINT('Ctrl Pts',(-18.1873397732036,-21.4543658907802,
-13.5393389498939));
#61052=CARTESIAN_POINT('Ctrl Pts',(-18.2700450257389,-21.4696071539973,
-13.5435086642143));
#61053=CARTESIAN_POINT('Ctrl Pts',(-18.3527473352663,-21.4848478748648,
-13.5476782301583));
#61054=CARTESIAN_POINT('Ctrl Pts',(-18.4362028921898,-21.4960094974156,
-13.5518477961024));
#61055=CARTESIAN_POINT('Ctrl Pts',(-18.5199766524688,-21.5030378293376,
-13.5560173620464));
#61056=CARTESIAN_POINT('Ctrl Pts',(-18.6066957948131,-21.5103132687396,
-13.5603335247854));
#61057=CARTESIAN_POINT('Ctrl Pts',(-18.6937554073231,-21.5131593125471,
-13.5646496875243));
#61058=CARTESIAN_POINT('Ctrl Pts',(-18.780669963282,-21.5115745573293,-13.5689658502632));
#61059=CARTESIAN_POINT('Ctrl Pts',(-18.8647532867224,-21.5100414253459,
-13.5731414144549));
#61060=CARTESIAN_POINT('Ctrl Pts',(-18.9487003921373,-21.5043618068031,
-13.5773169786466));
#61061=CARTESIAN_POINT('Ctrl Pts',(-19.032076119737,-21.4945873882411,-13.5814925428382));
#61062=CARTESIAN_POINT('Ctrl Pts',(-19.1196629571309,-21.484319287034,-13.5858790048508));
#61063=CARTESIAN_POINT('Ctrl Pts',(-19.2066186035792,-21.4695319558998,
-13.5902654668633));
#61064=CARTESIAN_POINT('Ctrl Pts',(-19.2924520557266,-21.4503457129578,
-13.5946519288759));
#61065=CARTESIAN_POINT('Ctrl Pts',(-19.378285507874,-21.4311594700159,-13.5990383908884));
#61066=CARTESIAN_POINT('Ctrl Pts',(-19.4629962271651,-21.4075745441673,
-13.6034248529009));
#61067=CARTESIAN_POINT('Ctrl Pts',(-19.546115225231,-21.379770347654,-13.6078113149135));
#61068=CARTESIAN_POINT('Ctrl Pts',(-19.6254097949839,-21.353245463438,-13.6119959493065));
#61069=CARTESIAN_POINT('Ctrl Pts',(-19.7035510491552,-21.3227823154618,
-13.6161805836996));
#61070=CARTESIAN_POINT('Ctrl Pts',(-19.7801197445754,-21.2885002632162,
-13.6203652180926));
#61071=CARTESIAN_POINT('Ctrl Pts',(-19.856579453935,-21.2542670072287,-13.6245438961766));
#61072=CARTESIAN_POINT('Ctrl Pts',(-19.9314706343177,-21.2162258304373,
-13.6287225742605));
#61073=CARTESIAN_POINT('Ctrl Pts',(-20.0043903176929,-21.1745454867588,
-13.6329012523444));
#61074=CARTESIAN_POINT('Ctrl Pts',(-20.0786170339862,-21.1321180528751,
-13.6371548302299));
#61075=CARTESIAN_POINT('Ctrl Pts',(-20.1508004226815,-21.0859198576825,
-13.6414084081153));
#61076=CARTESIAN_POINT('Ctrl Pts',(-20.2205378947045,-21.0361797157653,
-13.6456619860007));
#61077=CARTESIAN_POINT('Ctrl Pts',(-20.2889233697509,-20.9874038835591,
-13.6498330999787));
#61078=CARTESIAN_POINT('Ctrl Pts',(-20.3549565277685,-20.935222493605,-13.6540042139566));
#61079=CARTESIAN_POINT('Ctrl Pts',(-20.418285169954,-20.8798961243472,-13.6581753279346));
#61080=CARTESIAN_POINT('Ctrl Pts',(-20.4815925616021,-20.8245883203869,
-13.662345042255));
#61081=CARTESIAN_POINT('Ctrl Pts',(-20.5421968936245,-20.7661379354361,
-13.6665147565753));
#61082=CARTESIAN_POINT('Ctrl Pts',(-20.599779168576,-20.7048457131499,-13.6706844708957));
#61083=CARTESIAN_POINT('Ctrl Pts',(-20.657359394503,-20.643555671904,-13.6748540368397));
#61084=CARTESIAN_POINT('Ctrl Pts',(-20.711917462806,-20.5794243302495,-13.6790236027838));
#61085=CARTESIAN_POINT('Ctrl Pts',(-20.7631723252387,-20.5127881581065,
-13.6831931687278));
#61086=CARTESIAN_POINT('Ctrl Pts',(-20.816229245405,-20.4438091403553,-13.6875093314667));
#61087=CARTESIAN_POINT('Ctrl Pts',(-20.8657460348865,-20.3721462932503,
-13.6918254942057));
#61088=CARTESIAN_POINT('Ctrl Pts',(-20.9114587072169,-20.2982071082733,
-13.6961416569446));
#61089=CARTESIAN_POINT('Ctrl Pts',(-20.9556822940541,-20.22667648447,-13.7003172211363));
#61090=CARTESIAN_POINT('Ctrl Pts',(-20.9963456096571,-20.1530159839388,
-13.7044927853279));
#61091=CARTESIAN_POINT('Ctrl Pts',(-21.0332565704857,-20.0776194841413,
-13.7086683495196));
#61092=CARTESIAN_POINT('Ctrl Pts',(-21.0720318161984,-19.998414886377,-13.7130548115322));
#61093=CARTESIAN_POINT('Ctrl Pts',(-21.1066654530387,-19.9172948468642,
-13.7174412735447));
#61094=CARTESIAN_POINT('Ctrl Pts',(-21.1369928787005,-19.8347373476378,
-13.7218277355573));
#61095=CARTESIAN_POINT('Ctrl Pts',(-21.1673203043624,-19.7521798484114,
-13.7262141975698));
#61096=CARTESIAN_POINT('Ctrl Pts',(-21.1933414198056,-19.6681854662111,
-13.7306006595824));
#61097=CARTESIAN_POINT('Ctrl Pts',(-21.214953227824,-19.5832456584798,-13.7349871215949));
#61098=CARTESIAN_POINT('Ctrl Pts',(-21.2416966549182,-19.4781373050501,
-13.740415127754));
#61099=CARTESIAN_POINT('Ctrl Pts',(-21.261771847948,-19.3712684537292,-13.7458431339132));
#61100=CARTESIAN_POINT('Ctrl Pts',(-21.2749934581328,-19.2633715557439,
-13.7512711400723));
#61101=CARTESIAN_POINT('Ctrl Pts',(-21.2875287526693,-19.1610754377283,
-13.7564173858775));
#61102=CARTESIAN_POINT('Ctrl Pts',(-21.2939037306885,-19.05785506064,-13.7615636316826));
#61103=CARTESIAN_POINT('Ctrl Pts',(-21.2939989173812,-18.9543543592142,
-13.7667098774877));
#61104=CARTESIAN_POINT('Origin',(-18.734,-18.952,1.76670989022851));
#61105=CARTESIAN_POINT('',(-17.1725834092545,-16.9193794902115,-12.4500366838548));
#61106=CARTESIAN_POINT('',(-17.1744641548914,-16.9218650419685,-12.516719348784));
#61107=CARTESIAN_POINT('',(-17.1744641548914,-16.9218650419685,1.76670989022851));
#61108=CARTESIAN_POINT('',(-21.293999998394,-18.9520906788001,-13.0332901097364));
#61109=CARTESIAN_POINT('Ctrl Pts',(-17.1744641548914,-16.9218650419685,
-12.516719348784));
#61110=CARTESIAN_POINT('Ctrl Pts',(-17.1077873931624,-16.9730856761145,
-12.5208888646352));
#61111=CARTESIAN_POINT('Ctrl Pts',(-17.0436201053814,-17.0276073338008,
-12.5250583804865));
#61112=CARTESIAN_POINT('Ctrl Pts',(-16.9822975341889,-17.0851474425463,
-12.5292278963377));
#61113=CARTESIAN_POINT('Ctrl Pts',(-16.9209704681146,-17.1426917689231,
-12.5333977178102));
#61114=CARTESIAN_POINT('Ctrl Pts',(-16.8624888672419,-17.2032546699353,
-12.5375675392827));
#61115=CARTESIAN_POINT('Ctrl Pts',(-16.8071519907267,-17.2665158709856,
-12.5417373607552));
#61116=CARTESIAN_POINT('Ctrl Pts',(-16.7517572859962,-17.3298431813393,
-12.5459115397801));
#61117=CARTESIAN_POINT('Ctrl Pts',(-16.6995141714666,-17.3958740754972,
-12.5500857188049));
#61118=CARTESIAN_POINT('Ctrl Pts',(-16.6506820340232,-17.4642546411976,
-12.5542598978297));
#61119=CARTESIAN_POINT('Ctrl Pts',(-16.6018236009596,-17.5326720291522,
-12.5584363246084));
#61120=CARTESIAN_POINT('Ctrl Pts',(-16.5563800512887,-17.60344122091,-12.5626127513871));
#61121=CARTESIAN_POINT('Ctrl Pts',(-16.5145664411709,-17.6761807816375,
-12.5667891781657));
#61122=CARTESIAN_POINT('Ctrl Pts',(-16.4726799830268,-17.7490470698447,
-12.5709728811506));
#61123=CARTESIAN_POINT('Ctrl Pts',(-16.4344363059152,-17.8238901736935,
-12.5751565841354));
#61124=CARTESIAN_POINT('Ctrl Pts',(-16.4000035693677,-17.9003058135581,
-12.5793402871203));
#61125=CARTESIAN_POINT('Ctrl Pts',(-16.3735296901039,-17.9590585769595,
-12.5825569599381));
#61126=CARTESIAN_POINT('Ctrl Pts',(-16.3493076566629,-18.0187404532435,
-12.585773632756));
#61127=CARTESIAN_POINT('Ctrl Pts',(-16.3273937923111,-18.0791617783844,
-12.5889903055738));
#61128=CARTESIAN_POINT('Ctrl Pts',(-16.2988856052357,-18.1577650960284,
-12.5931749399669));
#61129=CARTESIAN_POINT('Ctrl Pts',(-16.2741793660911,-18.2379128391993,
-12.5973595743599));
#61130=CARTESIAN_POINT('Ctrl Pts',(-16.2534421603043,-18.3192023989267,
-12.601544208753));
#61131=CARTESIAN_POINT('Ctrl Pts',(-16.2327344713632,-18.4003762530275,
-12.6057228868369));
#61132=CARTESIAN_POINT('Ctrl Pts',(-16.2159847069801,-18.482688253513,-12.6099015649209));
#61133=CARTESIAN_POINT('Ctrl Pts',(-16.2033111427937,-18.5657178388638,
-12.6140802430048));
#61134=CARTESIAN_POINT('Ctrl Pts',(-16.1904104140776,-18.6502356698597,
-12.6183338208902));
#61135=CARTESIAN_POINT('Ctrl Pts',(-16.1817336190671,-18.7354966109226,
-12.6225873987757));
#61136=CARTESIAN_POINT('Ctrl Pts',(-16.177351748603,-18.8210430657489,-12.6268409766611));
#61137=CARTESIAN_POINT('Ctrl Pts',(-16.1730548292482,-18.9049310356181,
-12.6310120906391));
#61138=CARTESIAN_POINT('Ctrl Pts',(-16.1728878141637,-18.9890930669701,
-12.635183204617));
#61139=CARTESIAN_POINT('Ctrl Pts',(-16.1768654907269,-19.0730912940078,
-12.639354318595));
#61140=CARTESIAN_POINT('Ctrl Pts',(-16.1808418325422,-19.1570613346291,
-12.6435240329153));
#61141=CARTESIAN_POINT('Ctrl Pts',(-16.1889600821296,-19.2408672209642,
-12.6476937472357));
#61142=CARTESIAN_POINT('Ctrl Pts',(-16.2011829261396,-19.3240721305891,
-12.6518634615561));
#61143=CARTESIAN_POINT('Ctrl Pts',(-16.2134053352083,-19.4072740794261,
-12.6560330275001));
#61144=CARTESIAN_POINT('Ctrl Pts',(-16.229731980592,-19.4898746390482,-12.6602025934442));
#61145=CARTESIAN_POINT('Ctrl Pts',(-16.250073974422,-19.5714445087789,-12.6643721593882));
#61146=CARTESIAN_POINT('Ctrl Pts',(-16.2711311676606,-19.6558822745023,
-12.6686883221271));
#61147=CARTESIAN_POINT('Ctrl Pts',(-16.2964911945897,-19.7392150119464,
-12.6730044848661));
#61148=CARTESIAN_POINT('Ctrl Pts',(-16.3259989267241,-19.8209826414273,
-12.677320647605));
#61149=CARTESIAN_POINT('Ctrl Pts',(-16.3545454475878,-19.9000866989782,
-12.6814962117967));
#61150=CARTESIAN_POINT('Ctrl Pts',(-16.3869733753121,-19.9777256330116,
-12.6856717759884));
#61151=CARTESIAN_POINT('Ctrl Pts',(-16.4230935537342,-20.0535041518792,
-12.68984734018));
#61152=CARTESIAN_POINT('Ctrl Pts',(-16.4610380765009,-20.1331100635887,
-12.6942338021926));
#61153=CARTESIAN_POINT('Ctrl Pts',(-16.5030573653642,-20.2106621684909,
-12.6986202642051));
#61154=CARTESIAN_POINT('Ctrl Pts',(-16.5488792984353,-20.2857344261859,
-12.7030067262177));
#61155=CARTESIAN_POINT('Ctrl Pts',(-16.5947012315064,-20.3608066838809,
-12.7073931882302));
#61156=CARTESIAN_POINT('Ctrl Pts',(-16.6443254185492,-20.4333986583029,
-12.7117796502428));
#61157=CARTESIAN_POINT('Ctrl Pts',(-16.6974308899397,-20.5031241923032,
-12.7161661122553));
#61158=CARTESIAN_POINT('Ctrl Pts',(-16.7480928998703,-20.5696415511261,
-12.7203507466484));
#61159=CARTESIAN_POINT('Ctrl Pts',(-16.8021114495637,-20.6337980416559,
-12.7245353810414));
#61160=CARTESIAN_POINT('Ctrl Pts',(-16.8592384487626,-20.6952352468906,
-12.7287200154345));
#61161=CARTESIAN_POINT('Ctrl Pts',(-16.916284134749,-20.7565850038681,-12.7328986935184));
#61162=CARTESIAN_POINT('Ctrl Pts',(-16.9764291712246,-20.8152228296987,
-12.7370773716024));
#61163=CARTESIAN_POINT('Ctrl Pts',(-17.0393839528669,-20.8708216313141,
-12.7412560496863));
#61164=CARTESIAN_POINT('Ctrl Pts',(-17.1034671537253,-20.9274170014903,
-12.7455096275717));
#61165=CARTESIAN_POINT('Ctrl Pts',(-17.1704615277519,-20.9808629432572,
-12.7497632054572));
#61166=CARTESIAN_POINT('Ctrl Pts',(-17.2400207348673,-21.0308520763521,
-12.7540167833426));
#61167=CARTESIAN_POINT('Ctrl Pts',(-17.308231401019,-21.0798720725562,-12.7581878973205));
#61168=CARTESIAN_POINT('Ctrl Pts',(-17.3789079483581,-21.1255678171231,
-12.7623590112985));
#61169=CARTESIAN_POINT('Ctrl Pts',(-17.4516902051702,-21.1676898677575,
-12.7665301252764));
#61170=CARTESIAN_POINT('Ctrl Pts',(-17.524448039193,-21.2097977839311,-12.7706998395968));
#61171=CARTESIAN_POINT('Ctrl Pts',(-17.5993097815587,-21.2483341575378,
-12.7748695539172));
#61172=CARTESIAN_POINT('Ctrl Pts',(-17.6758879367288,-21.2830939195064,
-12.7790392682375));
#61173=CARTESIAN_POINT('Ctrl Pts',(-17.7524633669194,-21.3178524445735,
-12.7832088341816));
#61174=CARTESIAN_POINT('Ctrl Pts',(-17.8307546692264,-21.3488344358334,
-12.7873784001256));
#61175=CARTESIAN_POINT('Ctrl Pts',(-17.910352756402,-21.375882261603,-12.7915479660697));
#61176=CARTESIAN_POINT('Ctrl Pts',(-17.9927494141279,-21.4038810555595,
-12.7958641288086));
#61177=CARTESIAN_POINT('Ctrl Pts',(-18.0765459602124,-21.4276637164715,
-12.8001802915475));
#61178=CARTESIAN_POINT('Ctrl Pts',(-18.1612715723437,-21.4471116504386,
-12.8044964542864));
#61179=CARTESIAN_POINT('Ctrl Pts',(-18.2432372565715,-21.4659260700023,
-12.8086720184781));
#61180=CARTESIAN_POINT('Ctrl Pts',(-18.3260719356987,-21.4806837970704,
-12.8128475826698));
#61181=CARTESIAN_POINT('Ctrl Pts',(-18.4093408453622,-21.4913299181693,
-12.8170231468614));
#61182=CARTESIAN_POINT('Ctrl Pts',(-18.4968154696998,-21.5025137495362,
-12.821409608874));
#61183=CARTESIAN_POINT('Ctrl Pts',(-18.5847687611385,-21.5091596607904,
-12.8257960708865));
#61184=CARTESIAN_POINT('Ctrl Pts',(-18.6726951927072,-21.5112658557881,
-12.8301825328991));
#61185=CARTESIAN_POINT('Ctrl Pts',(-18.7606216242758,-21.5133720507858,
-12.8345689949116));
#61186=CARTESIAN_POINT('Ctrl Pts',(-18.8485206180845,-21.5109386216197,
-12.8389554569241));
#61187=CARTESIAN_POINT('Ctrl Pts',(-18.9358937423124,-21.5040264334084,
-12.8433419189367));
#61188=CARTESIAN_POINT('Ctrl Pts',(-19.0192466995766,-21.497432285223,-12.8475265533297));
#61189=CARTESIAN_POINT('Ctrl Pts',(-19.1024313715337,-21.4867379250515,
-12.8517111877228));
#61190=CARTESIAN_POINT('Ctrl Pts',(-19.1850120996547,-21.4719579532137,
-12.8558958221158));
#61191=CARTESIAN_POINT('Ctrl Pts',(-19.2674752843307,-21.4571990188365,
-12.8600745001998));
#61192=CARTESIAN_POINT('Ctrl Pts',(-19.3493357837206,-21.4383661042867,
-12.8642531782837));
#61193=CARTESIAN_POINT('Ctrl Pts',(-19.4301618064492,-21.4155256725355,
-12.8684318563676));
#61194=CARTESIAN_POINT('Ctrl Pts',(-19.5124365775465,-21.3922758424603,
-12.8726854342531));
#61195=CARTESIAN_POINT('Ctrl Pts',(-19.5936389405807,-21.3648734505894,
-12.8769390121385));
#61196=CARTESIAN_POINT('Ctrl Pts',(-19.6733229700786,-21.333443335014,-12.881192590024));
#61197=CARTESIAN_POINT('Ctrl Pts',(-19.7514621691741,-21.3026225535599,
-12.8853637040019));
#61198=CARTESIAN_POINT('Ctrl Pts',(-19.8281409334346,-21.2679290018995,
-12.8895348179799));
#61199=CARTESIAN_POINT('Ctrl Pts',(-19.9029545672469,-21.229530509063,-12.8937059319578));
#61200=CARTESIAN_POINT('Ctrl Pts',(-19.9777430966217,-21.1911449012116,
-12.8978756462782));
#61201=CARTESIAN_POINT('Ctrl Pts',(-20.0506673295889,-21.1490570311429,
-12.9020453605985));
#61202=CARTESIAN_POINT('Ctrl Pts',(-20.1213450915269,-21.1034817212833,
-12.9062150749189));
#61203=CARTESIAN_POINT('Ctrl Pts',(-20.1920203384467,-21.0579080331889,
-12.9103846408629));
#61204=CARTESIAN_POINT('Ctrl Pts',(-20.2604488871165,-21.008847402065,-12.914554206807));
#61205=CARTESIAN_POINT('Ctrl Pts',(-20.3262767630685,-20.9565584825073,
-12.918723772751));
#61206=CARTESIAN_POINT('Ctrl Pts',(-20.3944190659317,-20.9024311490432,
-12.9230399354899));
#61207=CARTESIAN_POINT('Ctrl Pts',(-20.4597740011395,-20.8448446181548,
-12.9273560982289));
#61208=CARTESIAN_POINT('Ctrl Pts',(-20.521987002802,-20.7841305842682,-12.9316722609678));
#61209=CARTESIAN_POINT('Ctrl Pts',(-20.582173422479,-20.7253943036496,-12.9358478251595));
#61210=CARTESIAN_POINT('Ctrl Pts',(-20.63941917621,-20.6637315251353,-12.9400233893512));
#61211=CARTESIAN_POINT('Ctrl Pts',(-20.6934427607502,-20.5994780931301,
-12.9441989535428));
#61212=CARTESIAN_POINT('Ctrl Pts',(-20.7501949481167,-20.5319793730223,
-12.9485854155554));
#61213=CARTESIAN_POINT('Ctrl Pts',(-20.803390556233,-20.4616218795445,-12.9529718775679));
#61214=CARTESIAN_POINT('Ctrl Pts',(-20.852754442665,-20.3888297086597,-12.9573583395805));
#61215=CARTESIAN_POINT('Ctrl Pts',(-20.9021183290971,-20.316037537775,-12.961744801593));
#61216=CARTESIAN_POINT('Ctrl Pts',(-20.9476502584794,-20.240811225245,-12.9661312636056));
#61217=CARTESIAN_POINT('Ctrl Pts',(-20.9891316170535,-20.1636028184871,
-12.9705177256181));
#61218=CARTESIAN_POINT('Ctrl Pts',(-21.0308618762442,-20.0859311380874,
-12.9749305077209));
#61219=CARTESIAN_POINT('Ctrl Pts',(-21.0686351706121,-20.0059905501583,
-12.9793432898236));
#61220=CARTESIAN_POINT('Ctrl Pts',(-21.1022126120118,-19.9241980375974,
-12.9837560719264));
#61221=CARTESIAN_POINT('Ctrl Pts',(-21.1356929152447,-19.8426421474353,
-12.9881560880307));
#61222=CARTESIAN_POINT('Ctrl Pts',(-21.1650014030469,-19.759245362016,-12.9925561041351));
#61223=CARTESIAN_POINT('Ctrl Pts',(-21.1899457627449,-19.6744475139796,
-12.9969561202394));
#61224=CARTESIAN_POINT('Ctrl Pts',(-21.2148467487816,-19.5897971138308,
-13.0013484855236));
#61225=CARTESIAN_POINT('Ctrl Pts',(-21.235398596884,-19.5037508664335,-13.0057408508078));
#61226=CARTESIAN_POINT('Ctrl Pts',(-21.2514572537729,-19.4167676574658,
-13.0101332160921));
#61227=CARTESIAN_POINT('Ctrl Pts',(-21.2674789983323,-19.3299843875645,
-13.0145154851126));
#61228=CARTESIAN_POINT('Ctrl Pts',(-21.2790280568698,-19.2422688247272,
-13.0188977541331));
#61229=CARTESIAN_POINT('Ctrl Pts',(-21.2860106924303,-19.1540926166924,
-13.0232800231537));
#61230=CARTESIAN_POINT('Ctrl Pts',(-21.2913273283411,-19.0869545296399,
-13.0266167186812));
#61231=CARTESIAN_POINT('Ctrl Pts',(-21.2939976088987,-19.0195497546626,
-13.0299534142088));
#61232=CARTESIAN_POINT('Ctrl Pts',(-21.293999998394,-18.9520906788001,-13.0332901097364));
#61233=CARTESIAN_POINT('Ctrl Pts',(-21.293999998394,-18.9520906780896,-13.0332901097715));
#61234=CARTESIAN_POINT('Ctrl Pts',(-21.2940031178915,-18.8640218456489,
-13.0376462156856));
#61235=CARTESIAN_POINT('Ctrl Pts',(-21.2894573285641,-18.7760356076548,
-13.0420023215996));
#61236=CARTESIAN_POINT('Ctrl Pts',(-21.2804139262416,-18.6886065372051,
-13.0463584275137));
#61237=CARTESIAN_POINT('Ctrl Pts',(-21.2713470661108,-18.600950683262,-13.0507258327921));
#61238=CARTESIAN_POINT('Ctrl Pts',(-21.2577593163574,-18.5138552818864,
-13.0550932380704));
#61239=CARTESIAN_POINT('Ctrl Pts',(-21.2397536148681,-18.4277874271106,
-13.0594606433487));
#61240=CARTESIAN_POINT('Ctrl Pts',(-21.2217244341812,-18.3416073409855,
-13.0638337436661));
#61241=CARTESIAN_POINT('Ctrl Pts',(-21.1992659159007,-18.25645785704,-13.0682068439834));
#61242=CARTESIAN_POINT('Ctrl Pts',(-21.172530963322,-18.1727909517209,-13.0725799443007));
#61243=CARTESIAN_POINT('Ctrl Pts',(-21.1457232584229,-18.0888963683656,
-13.0769649448896));
#61244=CARTESIAN_POINT('Ctrl Pts',(-21.114615990053,-18.0064928038113,-13.0813499454785));
#61245=CARTESIAN_POINT('Ctrl Pts',(-21.0794107185113,-17.9260133716796,
-13.0857349460673));
#61246=CARTESIAN_POINT('Ctrl Pts',(-21.0474072811094,-17.8528533488881,
-13.0897211414781));
#61247=CARTESIAN_POINT('Ctrl Pts',(-21.0120180507083,-17.7812832866316,
-13.0937073368888));
#61248=CARTESIAN_POINT('Ctrl Pts',(-20.9734262024016,-17.7116088181557,
-13.0976935322996));
#61249=CARTESIAN_POINT('Ctrl Pts',(-20.9329131921061,-17.6384658467109,
-13.1018781666926));
#61250=CARTESIAN_POINT('Ctrl Pts',(-20.8887375841054,-17.5671736686977,
-13.1060628010857));
#61251=CARTESIAN_POINT('Ctrl Pts',(-20.8410930440999,-17.4981228031551,
-13.1102474354787));
#61252=CARTESIAN_POINT('Ctrl Pts',(-20.7935163201999,-17.4291702229727,
-13.1144261135626));
#61253=CARTESIAN_POINT('Ctrl Pts',(-20.7424807309408,-17.3624529938651,
-13.1186047916466));
#61254=CARTESIAN_POINT('Ctrl Pts',(-20.6882255495785,-17.2983366420657,
-13.1227834697305));
#61255=CARTESIAN_POINT('Ctrl Pts',(-20.6329978830829,-17.23307105074,-13.127037047616));
#61256=CARTESIAN_POINT('Ctrl Pts',(-20.5744343004281,-17.1705009170561,
-13.1312906255014));
#61257=CARTESIAN_POINT('Ctrl Pts',(-20.5128330635401,-17.1109804639666,
-13.1355442033868));
#61258=CARTESIAN_POINT('Ctrl Pts',(-20.4524260868341,-17.0526139310049,
-13.1397153173648));
#61259=CARTESIAN_POINT('Ctrl Pts',(-20.3890985326089,-16.9971802202218,
-13.1438864313427));
#61260=CARTESIAN_POINT('Ctrl Pts',(-20.323170725482,-16.9449782250132,-13.1480575453207));
#61261=CARTESIAN_POINT('Ctrl Pts',(-20.2572650410674,-16.8927937466883,
-13.1522272596411));
#61262=CARTESIAN_POINT('Ctrl Pts',(-20.1887611969918,-16.8438391155729,
-13.1563969739614));
#61263=CARTESIAN_POINT('Ctrl Pts',(-20.1180129698811,-16.7983732683678,
-13.1605666882818));
#61264=CARTESIAN_POINT('Ctrl Pts',(-20.0472672602961,-16.7529090390327,
-13.1647362542259));
#61265=CARTESIAN_POINT('Ctrl Pts',(-19.9742777139359,-16.7109335947646,
-13.1689058201699));
#61266=CARTESIAN_POINT('Ctrl Pts',(-19.8994263305447,-16.672662054878,-13.1730753861139));
#61267=CARTESIAN_POINT('Ctrl Pts',(-19.8219432648525,-16.6330449348619,
-13.1773915488529));
#61268=CARTESIAN_POINT('Ctrl Pts',(-19.7424654713775,-16.5973972639687,
-13.1817077115918));
#61269=CARTESIAN_POINT('Ctrl Pts',(-19.6614416802126,-16.5659044592045,
-13.1860238743307));
#61270=CARTESIAN_POINT('Ctrl Pts',(-19.5830572305228,-16.535437529243,-13.1901994385224));
#61271=CARTESIAN_POINT('Ctrl Pts',(-19.5032264199663,-16.5088590368059,
-13.1943750027141));
#61272=CARTESIAN_POINT('Ctrl Pts',(-19.4223715061057,-16.4862861744351,
-13.1985505669057));
#61273=CARTESIAN_POINT('Ctrl Pts',(-19.3374328027602,-16.4625732104478,
-13.2029370289183));
#61274=CARTESIAN_POINT('Ctrl Pts',(-19.2513643920954,-16.4432812873466,
-13.2073234909308));
#61275=CARTESIAN_POINT('Ctrl Pts',(-19.1646662302708,-16.4284852688949,
-13.2117099529434));
#61276=CARTESIAN_POINT('Ctrl Pts',(-19.0779680684462,-16.4136892504433,
-13.2160964149559));
#61277=CARTESIAN_POINT('Ctrl Pts',(-18.9906407405946,-16.4033891290646,
-13.2204828769685));
#61278=CARTESIAN_POINT('Ctrl Pts',(-18.9031862415112,-16.3975967398073,
-13.224869338981));
#61279=CARTESIAN_POINT('Ctrl Pts',(-18.8197759389863,-16.3920722105337,
-13.2290529559168));
#61280=CARTESIAN_POINT('Ctrl Pts',(-18.7359395737696,-16.3906271591048,
-13.2332365728527));
#61281=CARTESIAN_POINT('Ctrl Pts',(-18.6521100212328,-16.3933100947208,
-13.2374201897885));
#61282=CARTESIAN_POINT('Ctrl Pts',(-18.5683906915468,-16.395989502693,-13.2415983059174));
#61283=CARTESIAN_POINT('Ctrl Pts',(-18.4846786121397,-16.4027861079029,
-13.2457764220463));
#61284=CARTESIAN_POINT('Ctrl Pts',(-18.401410469972,-16.4136965893503,-13.2499545381752));
#61285=CARTESIAN_POINT('Ctrl Pts',(-18.3182268241528,-16.4245959993866,
-13.2541284145607));
#61286=CARTESIAN_POINT('Ctrl Pts',(-18.2354866744767,-16.4396009359398,
-13.2583022909461));
#61287=CARTESIAN_POINT('Ctrl Pts',(-18.1536240274504,-16.4586561146751,
-13.2624761673316));
#61288=CARTESIAN_POINT('Ctrl Pts',(-18.0718198886652,-16.4776976744397,
-13.2666470605963));
#61289=CARTESIAN_POINT('Ctrl Pts',(-17.9908924531682,-16.5007836209311,
-13.2708179538609));
#61290=CARTESIAN_POINT('Ctrl Pts',(-17.9112665890683,-16.5278074056427,
-13.2749888471256));
#61291=CARTESIAN_POINT('Ctrl Pts',(-17.8316596834658,-16.554824756134,-13.2791587473226));
#61292=CARTESIAN_POINT('Ctrl Pts',(-17.7533541711449,-16.5857779414179,
-13.2833286475196));
#61293=CARTESIAN_POINT('Ctrl Pts',(-17.6767596812526,-16.6205105815349,
-13.2874985477166));
#61294=CARTESIAN_POINT('Ctrl Pts',(-17.6001752728535,-16.6552386500844,
-13.2916678990645));
#61295=CARTESIAN_POINT('Ctrl Pts',(-17.525301855604,-16.6937449890596,-13.2958372504123));
#61296=CARTESIAN_POINT('Ctrl Pts',(-17.4525274999375,-16.7358257668713,
-13.3000066017602));
#61297=CARTESIAN_POINT('Ctrl Pts',(-17.3797189214012,-16.7779263335904,
-13.3041779137873));
#61298=CARTESIAN_POINT('Ctrl Pts',(-17.3090117698551,-16.82360445842,-13.3083492258144));
#61299=CARTESIAN_POINT('Ctrl Pts',(-17.240767157218,-16.8726117059969,-13.3125205378415));
#61300=CARTESIAN_POINT('Ctrl Pts',(-17.2183978343134,-16.8886753761292,
-13.3138878168408));
#61301=CARTESIAN_POINT('Ctrl Pts',(-17.1962928438732,-16.9050963917938,
-13.31525509584));
#61302=CARTESIAN_POINT('Ctrl Pts',(-17.1744641548914,-16.9218650419685,
-13.3166223748392));
#61303=CARTESIAN_POINT('',(-21.2943301210028,-18.9513574887884,-12.9667098341108));
#61304=CARTESIAN_POINT('Ctrl Pts',(-21.2939999191096,-18.9513564484225,
-12.9667098902285));
#61305=CARTESIAN_POINT('Ctrl Pts',(-21.2939911726516,-18.9165636940744,
-12.9684506873211));
#61306=CARTESIAN_POINT('Ctrl Pts',(-21.2932731600888,-18.881780730387,-12.9701914844137));
#61307=CARTESIAN_POINT('Ctrl Pts',(-21.2918468828523,-18.8470270326106,
-12.9719322815063));
#61308=CARTESIAN_POINT('Ctrl Pts',(-21.2884183105029,-18.7634839708603,
-12.9761169158993));
#61309=CARTESIAN_POINT('Ctrl Pts',(-21.2808860937369,-18.6799535889704,
-12.9803015502924));
#61310=CARTESIAN_POINT('Ctrl Pts',(-21.2692483017375,-18.5968717857769,
-12.9844861846854));
#61311=CARTESIAN_POINT('Ctrl Pts',(-21.2576270746945,-18.5139082392468,
-12.9886648627694));
#61312=CARTESIAN_POINT('Ctrl Pts',(-21.2419119432712,-18.4313924548469,
-12.9928435408533));
#61313=CARTESIAN_POINT('Ctrl Pts',(-21.2221529486457,-18.3497584337279,
-12.9970222189372));
#61314=CARTESIAN_POINT('Ctrl Pts',(-21.2020397882419,-18.2666611814494,
-13.0012757968227));
#61315=CARTESIAN_POINT('Ctrl Pts',(-21.1777363859676,-18.1844780963255,
-13.0055293747081));
#61316=CARTESIAN_POINT('Ctrl Pts',(-21.1493505801536,-18.1036595170853,
-13.0097829525935));
#61317=CARTESIAN_POINT('Ctrl Pts',(-21.1215150885756,-18.0244077637083,
-13.0139540665715));
#61318=CARTESIAN_POINT('Ctrl Pts',(-21.0897542310845,-17.9464685351597,
-13.0181251805494));
#61319=CARTESIAN_POINT('Ctrl Pts',(-21.0542203695086,-17.8702526002261,
-13.0222962945274));
#61320=CARTESIAN_POINT('Ctrl Pts',(-21.0186984316631,-17.7940622402855,
-13.0264660088478));
#61321=CARTESIAN_POINT('Ctrl Pts',(-20.9794061983924,-17.7195944421082,
-13.0306357231681));
#61322=CARTESIAN_POINT('Ctrl Pts',(-20.9365438451406,-17.6472392517272,
-13.0348054374885));
#61323=CARTESIAN_POINT('Ctrl Pts',(-20.8936830171152,-17.5748866360543,
-13.0389750034325));
#61324=CARTESIAN_POINT('Ctrl Pts',(-20.8472525568965,-17.5046468740728,
-13.0431445693766));
#61325=CARTESIAN_POINT('Ctrl Pts',(-20.7974975099507,-17.4368834941077,
-13.0473141353206));
#61326=CARTESIAN_POINT('Ctrl Pts',(-20.7459931369336,-17.366737637298,-13.0516302980595));
#61327=CARTESIAN_POINT('Ctrl Pts',(-20.6909263546122,-17.2992459668448,
-13.0559464607985));
#61328=CARTESIAN_POINT('Ctrl Pts',(-20.6326151733211,-17.234775371818,-13.0602626235374));
#61329=CARTESIAN_POINT('Ctrl Pts',(-20.5762034726275,-17.1724048996433,
-13.0644381877291));
#61330=CARTESIAN_POINT('Ctrl Pts',(-20.5167558657732,-17.1128620023875,
-13.0686137519208));
#61331=CARTESIAN_POINT('Ctrl Pts',(-20.4545972806997,-17.0564407163983,
-13.0727893161124));
#61332=CARTESIAN_POINT('Ctrl Pts',(-20.3892992132619,-16.9971697253824,
-13.077175778125));
#61333=CARTESIAN_POINT('Ctrl Pts',(-20.3210095593889,-16.9413443477726,
-13.0815622401375));
#61334=CARTESIAN_POINT('Ctrl Pts',(-20.2501416763133,-16.889255610274,-13.0859487021501));
#61335=CARTESIAN_POINT('Ctrl Pts',(-20.1792737932376,-16.8371668727754,
-13.0903351641627));
#61336=CARTESIAN_POINT('Ctrl Pts',(-20.1058282074104,-16.7888150309008,
-13.0947216261752));
#61337=CARTESIAN_POINT('Ctrl Pts',(-20.0302483510417,-16.7444356832877,
-13.0991080881878));
#61338=CARTESIAN_POINT('Ctrl Pts',(-19.958146035901,-16.7020982952443,-13.1032927225808));
#61339=CARTESIAN_POINT('Ctrl Pts',(-19.8838331576254,-16.6632182861073,
-13.1074773569739));
#61340=CARTESIAN_POINT('Ctrl Pts',(-19.8076751930389,-16.6280332231607,
-13.1116619913669));
#61341=CARTESIAN_POINT('Ctrl Pts',(-19.7316256298885,-16.5928982417961,
-13.1158406694508));
#61342=CARTESIAN_POINT('Ctrl Pts',(-19.6537366110356,-16.5614479512896,
-13.1200193475348));
#61343=CARTESIAN_POINT('Ctrl Pts',(-19.5744001491065,-16.533875191521,-13.1241980256187));
#61344=CARTESIAN_POINT('Ctrl Pts',(-19.4936416381154,-16.5058082098496,
-13.1284516035042));
#61345=CARTESIAN_POINT('Ctrl Pts',(-19.4113836985809,-16.4817593798136,
-13.1327051813896));
#61346=CARTESIAN_POINT('Ctrl Pts',(-19.3280633649497,-16.461881786255,-13.136958759275));
#61347=CARTESIAN_POINT('Ctrl Pts',(-19.2463583585721,-16.4423895586354,
-13.141129873253));
#61348=CARTESIAN_POINT('Ctrl Pts',(-19.1636322517454,-16.4269083873419,
-13.1453009872309));
#61349=CARTESIAN_POINT('Ctrl Pts',(-19.0803129065813,-16.4155325015417,
-13.1494721012089));
#61350=CARTESIAN_POINT('Ctrl Pts',(-18.9970215200281,-16.4041604330299,
-13.1536418155293));
#61351=CARTESIAN_POINT('Ctrl Pts',(-18.9131377459122,-16.39689097632,-13.1578115298496));
#61352=CARTESIAN_POINT('Ctrl Pts',(-18.8290979023925,-16.3937669400618,
-13.16198124417));
#61353=CARTESIAN_POINT('Ctrl Pts',(-18.745061049371,-16.3906430149703,-13.1661508101141));
#61354=CARTESIAN_POINT('Ctrl Pts',(-18.6608685977346,-16.3916642332765,
-13.1703203760581));
#61355=CARTESIAN_POINT('Ctrl Pts',(-18.5769588557386,-16.3968213215102,
-13.1744899420021));
#61356=CARTESIAN_POINT('Ctrl Pts',(-18.4900989507279,-16.4021597266042,
-13.1788061047411));
#61357=CARTESIAN_POINT('Ctrl Pts',(-18.4035425318191,-16.4119302148937,
-13.18312226748));
#61358=CARTESIAN_POINT('Ctrl Pts',(-18.3177702276209,-16.4260639801085,
-13.1874384302189));
#61359=CARTESIAN_POINT('Ctrl Pts',(-18.2347919472102,-16.4397373394081,
-13.1916139944106));
#61360=CARTESIAN_POINT('Ctrl Pts',(-18.1525479314086,-16.4574939280207,
-13.1957895586023));
#61361=CARTESIAN_POINT('Ctrl Pts',(-18.0714612955843,-16.4792196892665,
-13.1999651227939));
#61362=CARTESIAN_POINT('Ctrl Pts',(-17.9862791665498,-16.5020427670648,
-13.2043515848065));
#61363=CARTESIAN_POINT('Ctrl Pts',(-17.9023749641123,-16.5292463408117,
-13.208738046819));
#61364=CARTESIAN_POINT('Ctrl Pts',(-17.8202171381046,-16.5606403697256,
-13.2131245088315));
#61365=CARTESIAN_POINT('Ctrl Pts',(-17.738059312097,-16.5920343986395,-13.2175109708441));
#61366=CARTESIAN_POINT('Ctrl Pts',(-17.6576483623232,-16.6276185783625,
-13.2218974328566));
#61367=CARTESIAN_POINT('Ctrl Pts',(-17.579422411398,-16.6671475776545,-13.2262838948691));
#61368=CARTESIAN_POINT('Ctrl Pts',(-17.5048157787117,-16.7048476694496,
-13.2304674063035));
#61369=CARTESIAN_POINT('Ctrl Pts',(-17.4319187998419,-16.746275904748,-13.2346509177379));
#61370=CARTESIAN_POINT('Ctrl Pts',(-17.3611287395177,-16.7912537163883,
-13.2388344291723));
#61371=CARTESIAN_POINT('Ctrl Pts',(-17.2970899771861,-16.8319419624025,
-13.2426189561699));
#61372=CARTESIAN_POINT('Ctrl Pts',(-17.2347754579772,-16.8755343097897,
-13.2464034831674));
#61373=CARTESIAN_POINT('Ctrl Pts',(-17.1744641548914,-16.9218650419685,
-13.250188010165));
#61374=CARTESIAN_POINT('Ctrl Pts',(-17.1725834092545,-16.9193794902115,
-12.4500366838548));
#61375=CARTESIAN_POINT('Ctrl Pts',(-17.1023021766235,-16.9725280716596,
-12.4544341408301));
#61376=CARTESIAN_POINT('Ctrl Pts',(-16.385846986399,-17.5778645097674,-12.5012235333658));
#61377=CARTESIAN_POINT('Ctrl Pts',(-15.7591749835997,-19.5120954830799,
-12.590404861462));
#61378=CARTESIAN_POINT('Ctrl Pts',(-17.5947353048798,-21.7565261244674,
-12.7175806681434));
#61379=CARTESIAN_POINT('Ctrl Pts',(-20.4360628533385,-21.4324759086211,
-12.8430154491812));
#61380=CARTESIAN_POINT('Ctrl Pts',(-21.2952859035193,-19.7651270969621,
-12.9260582946585));
#61381=CARTESIAN_POINT('Ctrl Pts',(-21.2980343668152,-18.9513691597422,
-12.9667092045753));
#61382=CARTESIAN_POINT('Origin',(-18.734,-18.952,1.76670989022851));
#61383=CARTESIAN_POINT('',(-17.1744641548914,-16.9218650419685,-11.6500725286462));
#61384=CARTESIAN_POINT('',(-17.1744641548914,-16.9218650419685,-11.716761786294));
#61385=CARTESIAN_POINT('',(-17.1744641548914,-16.9218650419685,1.76670989022851));
#61386=CARTESIAN_POINT('',(-21.2939989766127,-18.9542890482673,-12.2332901098107));
#61387=CARTESIAN_POINT('Ctrl Pts',(-17.1744641548914,-16.9218650419685,
-11.716761786294));
#61388=CARTESIAN_POINT('Ctrl Pts',(-17.1079832457044,-16.9729352235259,
-11.7209383110854));
#61389=CARTESIAN_POINT('Ctrl Pts',(-17.0439255031023,-17.0273420721353,
-11.7251148358768));
#61390=CARTESIAN_POINT('Ctrl Pts',(-16.9826416876458,-17.0848245766003,
-11.7292913606681));
#61391=CARTESIAN_POINT('Ctrl Pts',(-16.9214167468941,-17.1422518582393,
-11.7334638731168));
#61392=CARTESIAN_POINT('Ctrl Pts',(-16.8629607713186,-17.2027486100786,
-11.7376363855656));
#61393=CARTESIAN_POINT('Ctrl Pts',(-16.8075914573689,-17.2660136041837,
-11.7418088980143));
#61394=CARTESIAN_POINT('Ctrl Pts',(-16.7522504334316,-17.3292462741122,
-11.7459792785886));
#61395=CARTESIAN_POINT('Ctrl Pts',(-16.6999932422071,-17.3952440324702,
-11.7501496591628));
#61396=CARTESIAN_POINT('Ctrl Pts',(-16.6510998775129,-17.4636697007239,
-11.754320039737));
#61397=CARTESIAN_POINT('Ctrl Pts',(-16.6022168271016,-17.5320809342644,
-11.75848954055));
#61398=CARTESIAN_POINT('Ctrl Pts',(-16.5566964608029,-17.6029186859973,
-11.762659041363));
#61399=CARTESIAN_POINT('Ctrl Pts',(-16.5147768698912,-17.6758147866433,
-11.7668285421761));
#61400=CARTESIAN_POINT('Ctrl Pts',(-16.4728535473591,-17.7487173763933,
-11.7709984141519));
#61401=CARTESIAN_POINT('Ctrl Pts',(-16.4345318648703,-17.8236782794338,
-11.7751682861278));
#61402=CARTESIAN_POINT('Ctrl Pts',(-16.4000044799957,-17.9003037926285,
-11.7793381581037));
#61403=CARTESIAN_POINT('Ctrl Pts',(-16.3654406882584,-17.977010102401,-11.783512426936));
#61404=CARTESIAN_POINT('Ctrl Pts',(-16.3346793719312,-18.0553841066984,
-11.7876866957684));
#61405=CARTESIAN_POINT('Ctrl Pts',(-16.3078652231149,-18.1350116008238,
-11.7918609646007));
#61406=CARTESIAN_POINT('Ctrl Pts',(-16.2810362571641,-18.2146830960208,
-11.7960375400774));
#61407=CARTESIAN_POINT('Ctrl Pts',(-16.2581589268918,-18.2956090173988,
-11.800214115554));
#61408=CARTESIAN_POINT('Ctrl Pts',(-16.2393274875384,-18.3773618046384,
-11.8043906910306));
#61409=CARTESIAN_POINT('Ctrl Pts',(-16.220463547881,-18.459255685205,-11.8085744746643));
#61410=CARTESIAN_POINT('Ctrl Pts',(-16.2056595258686,-18.5419788285982,
-11.8127582582979));
#61411=CARTESIAN_POINT('Ctrl Pts',(-16.1949581528301,-18.6250955822875,
-11.8169420419316));
#61412=CARTESIAN_POINT('Ctrl Pts',(-16.1872902945174,-18.6846512569105,
-11.8199398497828));
#61413=CARTESIAN_POINT('Ctrl Pts',(-16.181727707034,-18.7444088772759,-11.8229376576341));
#61414=CARTESIAN_POINT('Ctrl Pts',(-16.1782696504242,-18.8042083214207,
-11.8259354654853));
#61415=CARTESIAN_POINT('Ctrl Pts',(-16.1734425556468,-18.8876822540642,
-11.8301200998784));
#61416=CARTESIAN_POINT('Ctrl Pts',(-16.172700351485,-18.9715482669721,-11.8343047342714));
#61417=CARTESIAN_POINT('Ctrl Pts',(-16.1760879473577,-19.0553727766261,
-11.8384893686645));
#61418=CARTESIAN_POINT('Ctrl Pts',(-16.179470721407,-19.1390779724659,-11.8426680467484));
#61419=CARTESIAN_POINT('Ctrl Pts',(-16.186971601001,-19.2227413266666,-11.8468467248323));
#61420=CARTESIAN_POINT('Ctrl Pts',(-16.1985835897661,-19.3059260187055,
-11.8510254029163));
#61421=CARTESIAN_POINT('Ctrl Pts',(-16.2104037150845,-19.3906017365655,
-11.8552789808017));
#61422=CARTESIAN_POINT('Ctrl Pts',(-16.2264838103271,-19.4747809821047,
-11.8595325586872));
#61423=CARTESIAN_POINT('Ctrl Pts',(-16.2467609749144,-19.5580049769523,
-11.8637861365726));
#61424=CARTESIAN_POINT('Ctrl Pts',(-16.2666450270985,-19.6396155122616,
-11.8679572505505));
#61425=CARTESIAN_POINT('Ctrl Pts',(-16.2905647501889,-19.7203070376072,
-11.8721283645285));
#61426=CARTESIAN_POINT('Ctrl Pts',(-16.3184090347921,-19.7996557607931,
-11.8762994785064));
#61427=CARTESIAN_POINT('Ctrl Pts',(-16.3462439759767,-19.8789778577487,
-11.8804691928268));
#61428=CARTESIAN_POINT('Ctrl Pts',(-16.3780007110438,-19.9569576137028,
-11.8846389071472));
#61429=CARTESIAN_POINT('Ctrl Pts',(-16.4135185064017,-20.0331871428518,
-11.8888086214675));
#61430=CARTESIAN_POINT('Ctrl Pts',(-16.4490350378841,-20.109413959427,-11.8929781874116));
#61431=CARTESIAN_POINT('Ctrl Pts',(-16.4883121684974,-20.1838902563955,
-11.8971477533556));
#61432=CARTESIAN_POINT('Ctrl Pts',(-16.531141898202,-20.2562301113465,-11.9013173192997));
#61433=CARTESIAN_POINT('Ctrl Pts',(-16.5754774683667,-20.3311133463566,
-11.9056334820386));
#61434=CARTESIAN_POINT('Ctrl Pts',(-16.6236198358017,-20.4037066556453,
-11.9099496447775));
#61435=CARTESIAN_POINT('Ctrl Pts',(-16.6752887227193,-20.4736135766998,
-11.9142658075164));
#61436=CARTESIAN_POINT('Ctrl Pts',(-16.7252745010802,-20.5412432871539,
-11.9184413717081));
#61437=CARTESIAN_POINT('Ctrl Pts',(-16.778560239593,-20.6063586052094,-11.9226169358998));
#61438=CARTESIAN_POINT('Ctrl Pts',(-16.8348515919043,-20.6686348837268,
-11.9267925000914));
#61439=CARTESIAN_POINT('Ctrl Pts',(-16.8939860866009,-20.7340565890242,
-11.931178962104));
#61440=CARTESIAN_POINT('Ctrl Pts',(-16.9564373882607,-20.7963445054469,
-11.9355654241165));
#61441=CARTESIAN_POINT('Ctrl Pts',(-17.0218228555023,-20.8551682599969,
-11.9399518861291));
#61442=CARTESIAN_POINT('Ctrl Pts',(-17.0872083227439,-20.9139920145469,
-11.9443383481416));
#61443=CARTESIAN_POINT('Ctrl Pts',(-17.1555274568808,-20.9693513010386,
-11.9487248101541));
#61444=CARTESIAN_POINT('Ctrl Pts',(-17.2263622218881,-21.0209679383717,
-11.9531112721667));
#61445=CARTESIAN_POINT('Ctrl Pts',(-17.2939377743552,-21.0702096177069,
-11.9572959065597));
#61446=CARTESIAN_POINT('Ctrl Pts',(-17.3640540780907,-21.1162287760929,
-11.9614805409527));
#61447=CARTESIAN_POINT('Ctrl Pts',(-17.4363708665884,-21.1587529612808,
-11.9656651753458));
#61448=CARTESIAN_POINT('Ctrl Pts',(-17.5085847210887,-21.2012166185545,
-11.9698438534297));
#61449=CARTESIAN_POINT('Ctrl Pts',(-17.5829924458174,-21.2401949526837,
-11.9740225315137));
#61450=CARTESIAN_POINT('Ctrl Pts',(-17.659222956839,-21.2754574038476,-11.9782012095976));
#61451=CARTESIAN_POINT('Ctrl Pts',(-17.7368198449848,-21.3113519091059,
-11.9824547874831));
#61452=CARTESIAN_POINT('Ctrl Pts',(-17.8163051194007,-21.3433957227619,
-11.9867083653685));
#61453=CARTESIAN_POINT('Ctrl Pts',(-17.8972589731891,-21.3713934062181,
-11.9909619432539));
#61454=CARTESIAN_POINT('Ctrl Pts',(-17.9766433785533,-21.3988482999474,
-11.9951330572319));
#61455=CARTESIAN_POINT('Ctrl Pts',(-18.0574394740936,-21.4224123904404,
-11.9993041712098));
#61456=CARTESIAN_POINT('Ctrl Pts',(-18.1392307762325,-21.4419497124358,
-12.0034752851878));
#61457=CARTESIAN_POINT('Ctrl Pts',(-18.2209946325099,-21.461480478494,-12.0076449995081));
#61458=CARTESIAN_POINT('Ctrl Pts',(-18.303752585081,-21.4769870528098,-12.0118147138285));
#61459=CARTESIAN_POINT('Ctrl Pts',(-18.3870746644898,-21.4883838060477,
-12.0159844281489));
#61460=CARTESIAN_POINT('Ctrl Pts',(-18.4703937789414,-21.4997801537403,
-12.0201539940929));
#61461=CARTESIAN_POINT('Ctrl Pts',(-18.5542765244138,-21.5070669096296,
-12.024323560037));
#61462=CARTESIAN_POINT('Ctrl Pts',(-18.6382858147563,-21.5102100763509,
-12.028493125981));
#61463=CARTESIAN_POINT('Ctrl Pts',(-18.7252487681107,-21.5134637529366,
-12.0328092887199));
#61464=CARTESIAN_POINT('Ctrl Pts',(-18.8123468034828,-21.5122770220956,
-12.0371254514589));
#61465=CARTESIAN_POINT('Ctrl Pts',(-18.8990948495902,-21.5066709554537,
-12.0414416141978));
#61466=CARTESIAN_POINT('Ctrl Pts',(-18.9830170872199,-21.501247505843,-12.0456171783895));
#61467=CARTESIAN_POINT('Ctrl Pts',(-19.0666113245951,-21.4916883190585,
-12.0497927425811));
#61468=CARTESIAN_POINT('Ctrl Pts',(-19.1494452607497,-21.4780651684627,
-12.0539683067728));
#61469=CARTESIAN_POINT('Ctrl Pts',(-19.2364629421006,-21.4637539449163,
-12.0583547687854));
#61470=CARTESIAN_POINT('Ctrl Pts',(-19.3226409276417,-21.444957551129,-12.0627412307979));
#61471=CARTESIAN_POINT('Ctrl Pts',(-19.4074943094419,-21.4218189033104,
-12.0671276928105));
#61472=CARTESIAN_POINT('Ctrl Pts',(-19.4923476912421,-21.3986802554918,
-12.071514154823));
#61473=CARTESIAN_POINT('Ctrl Pts',(-19.5758759419182,-21.371199607226,-12.0759006168356));
#61474=CARTESIAN_POINT('Ctrl Pts',(-19.6576188802164,-21.3395778865008,
-12.0802870788481));
#61475=CARTESIAN_POINT('Ctrl Pts',(-19.7356007047513,-21.3094111280209,
-12.0844717132412));
#61476=CARTESIAN_POINT('Ctrl Pts',(-19.8122481596154,-21.2753637103369,
-12.0886563476342));
#61477=CARTESIAN_POINT('Ctrl Pts',(-19.8871479757777,-21.2375742704974,
-12.0928409820272));
#61478=CARTESIAN_POINT('Ctrl Pts',(-19.9619411813225,-21.1998386192481,
-12.0970196601112));
#61479=CARTESIAN_POINT('Ctrl Pts',(-20.0349912820117,-21.1583717310105,
-12.1011983381951));
#61480=CARTESIAN_POINT('Ctrl Pts',(-20.1059035528267,-21.1133608309908,
-12.1053770162791));
#61481=CARTESIAN_POINT('Ctrl Pts',(-20.1780868751323,-21.0675431429372,
-12.1096305941645));
#61482=CARTESIAN_POINT('Ctrl Pts',(-20.2480545228573,-21.0180533145438,
-12.11388417205));
#61483=CARTESIAN_POINT('Ctrl Pts',(-20.3154149295588,-20.9651385497696,
-12.1181377499354));
#61484=CARTESIAN_POINT('Ctrl Pts',(-20.3814694233334,-20.9132496409652,
-12.1223088639134));
#61485=CARTESIAN_POINT('Ctrl Pts',(-20.4450164884367,-20.8580677061306,
-12.1264799778913));
#61486=CARTESIAN_POINT('Ctrl Pts',(-20.5057163649395,-20.7998693466275,
-12.1306510918693));
#61487=CARTESIAN_POINT('Ctrl Pts',(-20.5663958730126,-20.7416905161459,
-12.1348208061896));
#61488=CARTESIAN_POINT('Ctrl Pts',(-20.6242297581416,-20.6804975893352,
-12.13899052051));
#61489=CARTESIAN_POINT('Ctrl Pts',(-20.6789132852951,-20.6166057529285,
-12.1431602348304));
#61490=CARTESIAN_POINT('Ctrl Pts',(-20.7335948665741,-20.5527161900675,
-12.1473298007744));
#61491=CARTESIAN_POINT('Ctrl Pts',(-20.785126014285,-20.486128258616,-12.1514993667185));
#61492=CARTESIAN_POINT('Ctrl Pts',(-20.8332415555809,-20.4171910767277,
-12.1556689326625));
#61493=CARTESIAN_POINT('Ctrl Pts',(-20.8830487799517,-20.3458301485675,
-12.1599850954014));
#61494=CARTESIAN_POINT('Ctrl Pts',(-20.9291954417206,-20.2719521294864,
-12.1643012581404));
#61495=CARTESIAN_POINT('Ctrl Pts',(-20.9714366989051,-20.1959762933403,
-12.1686174208793));
#61496=CARTESIAN_POINT('Ctrl Pts',(-21.0123019515798,-20.1224753620654,
-12.172792985071));
#61497=CARTESIAN_POINT('Ctrl Pts',(-21.0495121634692,-20.0470116310055,
-12.1769685492626));
#61498=CARTESIAN_POINT('Ctrl Pts',(-21.0828936882991,-19.96998744642,-12.1811441134543));
#61499=CARTESIAN_POINT('Ctrl Pts',(-21.117961234591,-19.8890729533789,-12.1855305754669));
#61500=CARTESIAN_POINT('Ctrl Pts',(-21.1488029510882,-19.8064367740456,
-12.1899170374794));
#61501=CARTESIAN_POINT('Ctrl Pts',(-21.1752765362399,-19.7225639970856,
-12.1943034994919));
#61502=CARTESIAN_POINT('Ctrl Pts',(-21.2017501213916,-19.6386912201256,
-12.1986899615045));
#61503=CARTESIAN_POINT('Ctrl Pts',(-21.2238555029593,-19.5535824262448,
-12.203076423517));
#61504=CARTESIAN_POINT('Ctrl Pts',(-21.2415125421985,-19.4677333135615,
-12.2074628855296));
#61505=CARTESIAN_POINT('Ctrl Pts',(-21.2654843862316,-19.3511814097151,
-12.2134181072288));
#61506=CARTESIAN_POINT('Ctrl Pts',(-21.2813366135095,-19.2329068373031,
-12.219373328928));
#61507=CARTESIAN_POINT('Ctrl Pts',(-21.2888788650992,-19.1138455580776,
-12.2253285506272));
#61508=CARTESIAN_POINT('Ctrl Pts',(-21.2922399536332,-19.060787728371,-12.2279824036753));
#61509=CARTESIAN_POINT('Ctrl Pts',(-21.2939513313562,-19.0075739736056,
-12.2306362567234));
#61510=CARTESIAN_POINT('Ctrl Pts',(-21.293998976612,-18.9542890490546,-12.2332901097715));
#61511=CARTESIAN_POINT('Ctrl Pts',(-21.2939989766127,-18.9542890482673,
-12.2332901098107));
#61512=CARTESIAN_POINT('Ctrl Pts',(-21.2940747905549,-18.869501140071,-12.2375129674107));
#61513=CARTESIAN_POINT('Ctrl Pts',(-21.2899336304853,-18.7845778436852,
-12.2417358250107));
#61514=CARTESIAN_POINT('Ctrl Pts',(-21.2815646644669,-18.699979603286,-12.2459586826108));
#61515=CARTESIAN_POINT('Ctrl Pts',(-21.2734134565488,-18.6175825848873,
-12.2500716626647));
#61516=CARTESIAN_POINT('Ctrl Pts',(-21.2612518149667,-18.5354944186517,
-12.2541846427187));
#61517=CARTESIAN_POINT('Ctrl Pts',(-21.2451224198776,-18.4541403888767,
-12.2582976227727));
#61518=CARTESIAN_POINT('Ctrl Pts',(-21.2290007459443,-18.3728253033476,
-12.2624086339395));
#61519=CARTESIAN_POINT('Ctrl Pts',(-21.2089151790601,-18.2922441216167,
-12.2665196451063));
#61520=CARTESIAN_POINT('Ctrl Pts',(-21.1849598944702,-18.2128142346483,
-12.2706306562731));
#61521=CARTESIAN_POINT('Ctrl Pts',(-21.1610084101084,-18.1333969483105,
-12.2747410152756));
#61522=CARTESIAN_POINT('Ctrl Pts',(-21.133188564531,-18.0551310480641,-12.2788513742782));
#61523=CARTESIAN_POINT('Ctrl Pts',(-21.1016446063283,-17.9784194855459,
-12.2829617332807));
#61524=CARTESIAN_POINT('Ctrl Pts',(-21.0685960771622,-17.8980489659376,
-12.2872681465249));
#61525=CARTESIAN_POINT('Ctrl Pts',(-21.031459503672,-17.8193852938559,-12.2915745597691));
#61526=CARTESIAN_POINT('Ctrl Pts',(-20.9904568914618,-17.7428671301405,
-12.2958809730133));
#61527=CARTESIAN_POINT('Ctrl Pts',(-20.9512718262792,-17.669740832297,-12.2999964933321));
#61528=CARTESIAN_POINT('Ctrl Pts',(-20.9085564982552,-17.5985742591841,
-12.304112013651));
#61529=CARTESIAN_POINT('Ctrl Pts',(-20.8625501361326,-17.5297221375659,
-12.3082275339698));
#61530=CARTESIAN_POINT('Ctrl Pts',(-20.8165130556118,-17.4608240434608,
-12.3123458022171));
#61531=CARTESIAN_POINT('Ctrl Pts',(-20.7671808550883,-17.3942438526559,
-12.3164640704644));
#61532=CARTESIAN_POINT('Ctrl Pts',(-20.7148334041519,-17.3303036582036,
-12.3205823387118));
#61533=CARTESIAN_POINT('Ctrl Pts',(-20.6624054653519,-17.2662651512345,
-12.3247069390843));
#61534=CARTESIAN_POINT('Ctrl Pts',(-20.6069533520103,-17.204875081262,-12.3288315394568));
#61535=CARTESIAN_POINT('Ctrl Pts',(-20.5487934990227,-17.146418499235,-12.3329561398293));
#61536=CARTESIAN_POINT('Ctrl Pts',(-20.5408850965653,-17.1384697484523,
-12.3335169906232));
#61537=CARTESIAN_POINT('Ctrl Pts',(-20.5329266770602,-17.1305751748486,
-12.3340778414171));
#61538=CARTESIAN_POINT('Ctrl Pts',(-20.524919080494,-17.1227354354489,-12.334638692211));
#61539=CARTESIAN_POINT('Ctrl Pts',(-20.4651725946905,-17.0642413698601,
-12.338823326604));
#61540=CARTESIAN_POINT('Ctrl Pts',(-20.4024461555816,-17.0085686402269,
-12.3430079609971));
#61541=CARTESIAN_POINT('Ctrl Pts',(-20.3370370650427,-16.9560360303604,
-12.3471925953901));
#61542=CARTESIAN_POINT('Ctrl Pts',(-20.2717210762481,-16.9035781941619,
-12.3513712734741));
#61543=CARTESIAN_POINT('Ctrl Pts',(-20.2037303762193,-16.8542518853563,
-12.355549951558));
#61544=CARTESIAN_POINT('Ctrl Pts',(-20.1333988170805,-16.8083388908799,
-12.3597286296419));
#61545=CARTESIAN_POINT('Ctrl Pts',(-20.0618066152904,-16.7616029389746,
-12.3639822075274));
#61546=CARTESIAN_POINT('Ctrl Pts',(-19.9877891536757,-16.7184042096101,
-12.3682357854128));
#61547=CARTESIAN_POINT('Ctrl Pts',(-19.9117335730786,-16.6789967816029,
-12.3724893632982));
#61548=CARTESIAN_POINT('Ctrl Pts',(-19.8371524783216,-16.6403533434849,
-12.3766604772762));
#61549=CARTESIAN_POINT('Ctrl Pts',(-19.760612012467,-16.605355736394,-12.3808315912541));
#61550=CARTESIAN_POINT('Ctrl Pts',(-19.6825046263015,-16.5741987101768,
-12.3850027052321));
#61551=CARTESIAN_POINT('Ctrl Pts',(-19.6044234498237,-16.5430521390007,
-12.3891724195525));
#61552=CARTESIAN_POINT('Ctrl Pts',(-19.5247768242089,-16.5157437595369,
-12.3933421338728));
#61553=CARTESIAN_POINT('Ctrl Pts',(-19.443977821747,-16.4924204642607,-12.3975118481932));
#61554=CARTESIAN_POINT('Ctrl Pts',(-19.3631816944604,-16.4690979989275,
-12.4016814141372));
#61555=CARTESIAN_POINT('Ctrl Pts',(-19.2812337140819,-16.449760462599,-12.4058509800813));
#61556=CARTESIAN_POINT('Ctrl Pts',(-19.1985614595122,-16.4345046871273,
-12.4100205460253));
#61557=CARTESIAN_POINT('Ctrl Pts',(-19.1129825504589,-16.4187125374101,
-12.4143367087642));
#61558=CARTESIAN_POINT('Ctrl Pts',(-19.0266280073014,-16.4072946141391,
-12.4186528715032));
#61559=CARTESIAN_POINT('Ctrl Pts',(-18.9399808515253,-16.400300196182,-12.4229690342421));
#61560=CARTESIAN_POINT('Ctrl Pts',(-18.856156217735,-16.3935336206541,-12.4271445984338));
#61561=CARTESIAN_POINT('Ctrl Pts',(-18.7720582145667,-16.3909067522804,
-12.4313201626255));
#61562=CARTESIAN_POINT('Ctrl Pts',(-18.6881249777986,-16.3924110716097,
-12.4354957268171));
#61563=CARTESIAN_POINT('Ctrl Pts',(-18.5999524727736,-16.3939913705322,
-12.4398821888297));
#61564=CARTESIAN_POINT('Ctrl Pts',(-18.5119623987475,-16.4001311167978,
-12.4442686508422));
#61565=CARTESIAN_POINT('Ctrl Pts',(-18.4246552312345,-16.4107590011891,
-12.4486551128548));
#61566=CARTESIAN_POINT('Ctrl Pts',(-18.3373480637214,-16.4213868855804,
-12.4530415748673));
#61567=CARTESIAN_POINT('Ctrl Pts',(-18.2507243612256,-16.4365027334242,
-12.4574280368799));
#61568=CARTESIAN_POINT('Ctrl Pts',(-18.1652685194104,-16.4559742583486,
-12.4618144988924));
#61569=CARTESIAN_POINT('Ctrl Pts',(-18.0837368018554,-16.4745516526704,
-12.4659995349798));
#61570=CARTESIAN_POINT('Ctrl Pts',(-18.0029645350392,-16.49716262688,-12.4701845710671));
#61571=CARTESIAN_POINT('Ctrl Pts',(-17.9233808127844,-16.5237297239974,
-12.4743696071545));
#61572=CARTESIAN_POINT('Ctrl Pts',(-17.843930616112,-16.5502522468348,-12.4785476215876));
#61573=CARTESIAN_POINT('Ctrl Pts',(-17.7656654318456,-16.5807175510247,
-12.4827256360207));
#61574=CARTESIAN_POINT('Ctrl Pts',(-17.6890027069078,-16.6149975058999,
-12.4869036504538));
#61575=CARTESIAN_POINT('Ctrl Pts',(-17.6124142567096,-16.6492442486147,
-12.4910776170145));
#61576=CARTESIAN_POINT('Ctrl Pts',(-17.5374256012172,-16.6872981182065,
-12.4952515835751));
#61577=CARTESIAN_POINT('Ctrl Pts',(-17.4644368058942,-16.7289819397558,
-12.4994255501358));
#61578=CARTESIAN_POINT('Ctrl Pts',(-17.3915013099807,-16.7706353220704,
-12.503596468695));
#61579=CARTESIAN_POINT('Ctrl Pts',(-17.320563170554,-16.81591316144,-12.5077673872542));
#61580=CARTESIAN_POINT('Ctrl Pts',(-17.2519990079484,-16.8645917841596,
-12.5119383058134));
#61581=CARTESIAN_POINT('Ctrl Pts',(-17.2258010851161,-16.8831915708868,
-12.5135319868036));
#61582=CARTESIAN_POINT('Ctrl Pts',(-17.1999494849507,-16.9022873850278,
-12.5151256677938));
#61583=CARTESIAN_POINT('Ctrl Pts',(-17.1744641548914,-16.9218650419685,
-12.516719348784));
#61584=CARTESIAN_POINT('',(-21.2939992159918,-18.9499964727371,-12.1667098902285));
#61585=CARTESIAN_POINT('Ctrl Pts',(-21.2916488572292,-18.9499800095201,
-12.1667107986763));
#61586=CARTESIAN_POINT('Ctrl Pts',(-21.2937096036451,-18.6667985676303,
-12.1807663462568));
#61587=CARTESIAN_POINT('Ctrl Pts',(-21.1196059381089,-17.531999452779,-12.2372138293977));
#61588=CARTESIAN_POINT('Ctrl Pts',(-19.5298543213825,-16.0798455362524,
-12.3316557911239));
#61589=CARTESIAN_POINT('Ctrl Pts',(-17.7798204562966,-16.4601703038494,
-12.4120422052696));
#61590=CARTESIAN_POINT('Ctrl Pts',(-17.1725834092545,-16.9193794902115,
-12.4500366838548));
#61591=CARTESIAN_POINT('Ctrl Pts',(-17.1744641548914,-16.9218650419685,
-11.6500725286462));
#61592=CARTESIAN_POINT('Ctrl Pts',(-17.1077138142499,-16.9731421989338,
-11.65424766915));
#61593=CARTESIAN_POINT('Ctrl Pts',(-17.0435213657551,-17.0276947206701,
-11.6584228096539));
#61594=CARTESIAN_POINT('Ctrl Pts',(-16.9822122674274,-17.0852274535959,
-11.6625979501577));
#61595=CARTESIAN_POINT('Ctrl Pts',(-16.920893230811,-17.1427695126565,-11.6667737674575));
#61596=CARTESIAN_POINT('Ctrl Pts',(-16.8624587859411,-17.2032924040061,
-11.6709495847573));
#61597=CARTESIAN_POINT('Ctrl Pts',(-16.8071962002176,-17.2664653319661,
-11.6751254020571));
#61598=CARTESIAN_POINT('Ctrl Pts',(-16.7518333044684,-17.3297529284301,
-11.6793087991025));
#61599=CARTESIAN_POINT('Ctrl Pts',(-16.6996540596349,-17.3956998124642,
-11.6834921961479));
#61600=CARTESIAN_POINT('Ctrl Pts',(-16.6509044868842,-17.4639431854808,
-11.6876755931933));
#61601=CARTESIAN_POINT('Ctrl Pts',(-16.6023552296323,-17.5319061415721,
-11.6918418003595));
#61602=CARTESIAN_POINT('Ctrl Pts',(-16.5572076777017,-17.6021463237409,
-11.6960080075258));
#61603=CARTESIAN_POINT('Ctrl Pts',(-16.5156592733601,-17.6742815566288,
-11.700174214692));
#61604=CARTESIAN_POINT('Ctrl Pts',(-16.4739270995034,-17.7467358452539,
-11.704358849085));
#61605=CARTESIAN_POINT('Ctrl Pts',(-16.4356706929265,-17.8213716700561,
-11.7085434834781));
#61606=CARTESIAN_POINT('Ctrl Pts',(-16.4011245523601,-17.8978215778158,
-11.7127281178711));
#61607=CARTESIAN_POINT('Ctrl Pts',(-16.3666275839487,-17.9741626685944,
-11.7169067959551));
#61608=CARTESIAN_POINT('Ctrl Pts',(-16.3358305794285,-18.0523122977898,
-11.721085474039));
#61609=CARTESIAN_POINT('Ctrl Pts',(-16.3089230895031,-18.1318768518236,
-11.7252641521229));
#61610=CARTESIAN_POINT('Ctrl Pts',(-16.2815333021588,-18.2128675433065,
-11.7295177300084));
#61611=CARTESIAN_POINT('Ctrl Pts',(-16.258174080664,-18.2953239658201,-11.7337713078938));
#61612=CARTESIAN_POINT('Ctrl Pts',(-16.2389948450999,-18.3788078184222,
-11.7380248857792));
#61613=CARTESIAN_POINT('Ctrl Pts',(-16.2201874364424,-18.4606731736362,
-11.7421959997572));
#61614=CARTESIAN_POINT('Ctrl Pts',(-16.2053994934178,-18.5435260079657,
-11.7463671137351));
#61615=CARTESIAN_POINT('Ctrl Pts',(-16.194721659298,-18.6269376852946,-11.7505382277131));
#61616=CARTESIAN_POINT('Ctrl Pts',(-16.1840474082285,-18.7103213730297,
-11.7547079420335));
#61617=CARTESIAN_POINT('Ctrl Pts',(-16.1774805853424,-18.7942630754069,
-11.7588776563538));
#61618=CARTESIAN_POINT('Ctrl Pts',(-16.1750603443919,-18.8783261311159,
-11.7630473706742));
#61619=CARTESIAN_POINT('Ctrl Pts',(-16.172640189564,-18.9623861955006,-11.7672169366183));
#61620=CARTESIAN_POINT('Ctrl Pts',(-16.1743663356855,-19.0465671447644,
-11.7713865025623));
#61621=CARTESIAN_POINT('Ctrl Pts',(-16.1802258395509,-19.1304307636666,
-11.7755560685064));
#61622=CARTESIAN_POINT('Ctrl Pts',(-16.1862913563438,-19.2172429239522,
-11.7798722312453));
#61623=CARTESIAN_POINT('Ctrl Pts',(-16.1967862597982,-19.3037144978782,
-11.7841883939842));
#61624=CARTESIAN_POINT('Ctrl Pts',(-16.2116377216373,-19.3893654498161,
-11.7885045567231));
#61625=CARTESIAN_POINT('Ctrl Pts',(-16.2260053986691,-19.4722263310035,
-11.7926801209148));
#61626=CARTESIAN_POINT('Ctrl Pts',(-16.2444500136975,-19.5543187834628,
-11.7968556851065));
#61627=CARTESIAN_POINT('Ctrl Pts',(-16.2668539711946,-19.6352206616825,
-11.8010312492982));
#61628=CARTESIAN_POINT('Ctrl Pts',(-16.2903894993246,-19.7202087014451,
-11.8054177113107));
#61629=CARTESIAN_POINT('Ctrl Pts',(-16.3182946694535,-19.8038821804656,
-11.8098041733232));
#61630=CARTESIAN_POINT('Ctrl Pts',(-16.3503755250188,-19.8857742565901,
-11.8141906353358));
#61631=CARTESIAN_POINT('Ctrl Pts',(-16.382456380584,-19.9676663327146,-11.8185770973483));
#61632=CARTESIAN_POINT('Ctrl Pts',(-16.4187126130535,-20.0477765087051,
-11.8229635593609));
#61633=CARTESIAN_POINT('Ctrl Pts',(-16.4588952312817,-20.1256687315232,
-11.8273500213734));
#61634=CARTESIAN_POINT('Ctrl Pts',(-16.4972289876803,-20.1999770177056,
-11.8315346557664));
#61635=CARTESIAN_POINT('Ctrl Pts',(-16.5392784376738,-20.2725435578143,
-11.8357192901595));
#61636=CARTESIAN_POINT('Ctrl Pts',(-16.5848615409703,-20.3429722800687,
-11.8399039245525));
#61637=CARTESIAN_POINT('Ctrl Pts',(-16.6303797623612,-20.4133007557541,
-11.8440826026365));
#61638=CARTESIAN_POINT('Ctrl Pts',(-16.6794213986321,-20.4814970748824,
-11.8482612807204));
#61639=CARTESIAN_POINT('Ctrl Pts',(-16.7317580832551,-20.5471887997443,
-11.8524399588043));
#61640=CARTESIAN_POINT('Ctrl Pts',(-16.7850328653364,-20.6140580015628,
-11.8566935366898));
#61641=CARTESIAN_POINT('Ctrl Pts',(-16.8417217641061,-20.6783315077599,
-11.8609471145752));
#61642=CARTESIAN_POINT('Ctrl Pts',(-16.9015371160905,-20.7396464357065,
-11.8652006924607));
#61643=CARTESIAN_POINT('Ctrl Pts',(-16.9601928307565,-20.7997726541285,
-11.8693718064386));
#61644=CARTESIAN_POINT('Ctrl Pts',(-17.0218545195986,-20.8570536417638,
-11.8735429204166));
#61645=CARTESIAN_POINT('Ctrl Pts',(-17.0862108309602,-20.9111811693652,
-11.8777140343945));
#61646=CARTESIAN_POINT('Ctrl Pts',(-17.15054554694,-20.965290533952,-11.8818837487149));
#61647=CARTESIAN_POINT('Ctrl Pts',(-17.2175727378981,-21.0162482441934,
-11.8860534630352));
#61648=CARTESIAN_POINT('Ctrl Pts',(-17.2869464339592,-21.0637850214945,
-11.8902231773556));
#61649=CARTESIAN_POINT('Ctrl Pts',(-17.3563176614066,-21.1113201072332,
-11.8943927432997));
#61650=CARTESIAN_POINT('Ctrl Pts',(-17.42803484797,-21.155434242732,-11.8985623092437));
#61651=CARTESIAN_POINT('Ctrl Pts',(-17.5017225180692,-21.1959011135802,
-11.9027318751877));
#61652=CARTESIAN_POINT('Ctrl Pts',(-17.5780009557456,-21.237790749686,-11.9070480379267));
#61653=CARTESIAN_POINT('Ctrl Pts',(-17.6563905571824,-21.2757716196384,
-11.9113642006656));
#61654=CARTESIAN_POINT('Ctrl Pts',(-17.7364482678185,-21.3096451263118,
-11.9156803634045));
#61655=CARTESIAN_POINT('Ctrl Pts',(-17.8138981069511,-21.3424152070681,
-11.9198559275962));
#61656=CARTESIAN_POINT('Ctrl Pts',(-17.8929085883422,-21.3713412922625,
-11.9240314917879));
#61657=CARTESIAN_POINT('Ctrl Pts',(-17.9730611021937,-21.3962937617654,
-11.9282070559795));
#61658=CARTESIAN_POINT('Ctrl Pts',(-18.0572619289755,-21.4225065211841,
-11.9325935179921));
#61659=CARTESIAN_POINT('Ctrl Pts',(-18.142722622544,-21.4443335563954,-11.9369799800046));
#61660=CARTESIAN_POINT('Ctrl Pts',(-18.2289456575187,-21.4616852613706,
-11.9413664420172));
#61661=CARTESIAN_POINT('Ctrl Pts',(-18.3151686924933,-21.4790369663458,
-11.9457529040297));
#61662=CARTESIAN_POINT('Ctrl Pts',(-18.4021534837731,-21.4919133313661,
-11.9501393660423));
#61663=CARTESIAN_POINT('Ctrl Pts',(-18.489398605575,-21.500287691342,-11.9545258280548));
#61664=CARTESIAN_POINT('Ctrl Pts',(-18.5726294499945,-21.5082767346017,
-11.9587104624479));
#61665=CARTESIAN_POINT('Ctrl Pts',(-18.6564069960724,-21.5121986934545,
-11.9628950968409));
#61666=CARTESIAN_POINT('Ctrl Pts',(-18.7402996751639,-21.5119922488345,
-11.967079731234));
#61667=CARTESIAN_POINT('Ctrl Pts',(-18.8240729434106,-21.5117860980629,
-11.9712584093179));
#61668=CARTESIAN_POINT('Ctrl Pts',(-18.9079605630615,-21.507463217065,-11.9754370874019));
#61669=CARTESIAN_POINT('Ctrl Pts',(-18.9915257624726,-21.4990140324825,
-11.9796157654858));
#61670=CARTESIAN_POINT('Ctrl Pts',(-19.0765888080257,-21.4904134023388,
-11.9838693433712));
#61671=CARTESIAN_POINT('Ctrl Pts',(-19.1613172809486,-21.4775370395472,
-11.9881229212567));
#61672=CARTESIAN_POINT('Ctrl Pts',(-19.2452503475952,-21.4604304020809,
-11.9923764991421));
#61673=CARTESIAN_POINT('Ctrl Pts',(-19.3275562079629,-21.4436554101628,
-11.9965476131201));
#61674=CARTESIAN_POINT('Ctrl Pts',(-19.409096756315,-21.4228128002075,-12.000718727098));
#61675=CARTESIAN_POINT('Ctrl Pts',(-19.4894442918869,-21.3979975310404,
-12.004889841076));
#61676=CARTESIAN_POINT('Ctrl Pts',(-19.5697648660672,-21.3731905888764,
-12.0090595553963));
#61677=CARTESIAN_POINT('Ctrl Pts',(-19.6488927833422,-21.3444137706278,
-12.0132292697167));
#61678=CARTESIAN_POINT('Ctrl Pts',(-19.7264143560961,-21.3118122268126,
-12.0173989840371));
#61679=CARTESIAN_POINT('Ctrl Pts',(-19.8039331702998,-21.2792118431002,
-12.0215685499811));
#61680=CARTESIAN_POINT('Ctrl Pts',(-19.8798453299038,-21.242787183546,-12.0257381159252));
#61681=CARTESIAN_POINT('Ctrl Pts',(-19.9537573024934,-21.2027314639943,
-12.0299076818692));
#61682=CARTESIAN_POINT('Ctrl Pts',(-20.030267928859,-21.1612674347573,-12.0342238446082));
#61683=CARTESIAN_POINT('Ctrl Pts',(-20.1046346343673,-21.1159125099133,
-12.0385400073471));
#61684=CARTESIAN_POINT('Ctrl Pts',(-20.1764506132337,-21.0669317313762,
-12.042856170086));
#61685=CARTESIAN_POINT('Ctrl Pts',(-20.2459271941422,-21.019546496548,-12.0470317342777));
#61686=CARTESIAN_POINT('Ctrl Pts',(-20.3130163291632,-20.968768326667,-12.0512072984694));
#61687=CARTESIAN_POINT('Ctrl Pts',(-20.3773824427364,-20.914879045409,-12.0553828626611));
#61688=CARTESIAN_POINT('Ctrl Pts',(-20.4449995356903,-20.8582679446643,
-12.0597693246736));
#61689=CARTESIAN_POINT('Ctrl Pts',(-20.5096108706381,-20.7982235859986,
-12.0641557866861));
#61690=CARTESIAN_POINT('Ctrl Pts',(-20.5708718020379,-20.735115807478,-12.0685422486987));
#61691=CARTESIAN_POINT('Ctrl Pts',(-20.6321327334377,-20.6720080289574,
-12.0729287107112));
#61692=CARTESIAN_POINT('Ctrl Pts',(-20.6900429364135,-20.6058373172988,
-12.0773151727238));
#61693=CARTESIAN_POINT('Ctrl Pts',(-20.7443085775788,-20.5370108589259,
-12.0817016347363));
#61694=CARTESIAN_POINT('Ctrl Pts',(-20.796026764239,-20.4714154002739,-12.0858821780095));
#61695=CARTESIAN_POINT('Ctrl Pts',(-20.8446312405901,-20.4031588919979,
-12.0900627212828));
#61696=CARTESIAN_POINT('Ctrl Pts',(-20.8898359348525,-20.3325692383937,
-12.0942432645561));
#61697=CARTESIAN_POINT('Ctrl Pts',(-20.9349778718437,-20.2620775837717,
-12.0984180040186));
#61698=CARTESIAN_POINT('Ctrl Pts',(-20.9767291512524,-20.1892595981083,
-12.1025927434812));
#61699=CARTESIAN_POINT('Ctrl Pts',(-21.0148441174669,-20.114475854294,-12.1067674829437));
#61700=CARTESIAN_POINT('Ctrl Pts',(-21.0529176328921,-20.0397734392993,
-12.1109376822935));
#61701=CARTESIAN_POINT('Ctrl Pts',(-21.0873624809752,-19.9631099194739,
-12.1151078816433));
#61702=CARTESIAN_POINT('Ctrl Pts',(-21.1179772351408,-19.884873272385,-12.119278080993));
#61703=CARTESIAN_POINT('Ctrl Pts',(-21.1485693987593,-19.8066943559137,
-12.1234452031636));
#61704=CARTESIAN_POINT('Ctrl Pts',(-21.1753369141578,-19.7269450449952,
-12.1276123253341));
#61705=CARTESIAN_POINT('Ctrl Pts',(-21.1981256703524,-19.6460350716717,
-12.1317794475047));
#61706=CARTESIAN_POINT('Ctrl Pts',(-21.2209040463206,-19.5651619526563,
-12.1359446715606));
#61707=CARTESIAN_POINT('Ctrl Pts',(-21.2397071410259,-19.4831296648113,
-12.1401098956165));
#61708=CARTESIAN_POINT('Ctrl Pts',(-21.2544305326003,-19.4003636139743,
-12.1442751196725));
#61709=CARTESIAN_POINT('Ctrl Pts',(-21.2691564647156,-19.3175832817451,
-12.1484410624433));
#61710=CARTESIAN_POINT('Ctrl Pts',(-21.2798011983648,-19.2340693856731,
-12.1526070052142));
#61711=CARTESIAN_POINT('Ctrl Pts',(-21.2863115236391,-19.1502571216861,
-12.1567729479851));
#61712=CARTESIAN_POINT('Ctrl Pts',(-21.2914878410454,-19.0836185341096,
-12.1600852620662));
#61713=CARTESIAN_POINT('Ctrl Pts',(-21.2940514917317,-19.0167915973239,
-12.1633975761474));
#61714=CARTESIAN_POINT('Ctrl Pts',(-21.2939992159918,-18.9499964727371,
-12.1667098902285));
#61715=CARTESIAN_POINT('Origin',(-18.734,-18.952,1.76670989022851));
#61716=CARTESIAN_POINT('',(-17.1757181146141,-16.923465526843,-10.8502164882119));
#61717=CARTESIAN_POINT('',(-17.1731949518433,-16.9201829956178,-10.9165936692269));
#61718=CARTESIAN_POINT('',(-17.1744641548914,-16.9218650419685,1.76670989022851));
#61719=CARTESIAN_POINT('',(-21.2940195831445,-18.9506989550129,-11.4332901033027));
#61720=CARTESIAN_POINT('Ctrl Pts',(-17.1731949518433,-16.9201829956178,
-10.9165936692269));
#61721=CARTESIAN_POINT('Ctrl Pts',(-17.0711421091448,-16.9970800397133,
-10.9229640523897));
#61722=CARTESIAN_POINT('Ctrl Pts',(-16.3366273566849,-17.6446400359971,
-10.9717263711129));
#61723=CARTESIAN_POINT('Ctrl Pts',(-15.7882885392514,-19.6491907555867,
-11.0628806253967));
#61724=CARTESIAN_POINT('Ctrl Pts',(-17.7257693487527,-21.8062533022748,
-11.1900564320781));
#61725=CARTESIAN_POINT('Ctrl Pts',(-20.5048168108401,-21.3581664234228,
-11.3135258905536));
#61726=CARTESIAN_POINT('Ctrl Pts',(-21.2925956727874,-19.7256331618843,
-11.3946034134688));
#61727=CARTESIAN_POINT('Ctrl Pts',(-21.2974134759181,-18.9507193137797,
-11.4332890008234));
#61728=CARTESIAN_POINT('Ctrl Pts',(-21.2939996693303,-18.9506988355569,
-11.4332901097715));
#61729=CARTESIAN_POINT('Ctrl Pts',(-21.293961988618,-18.8765632322752,-11.436996088328));
#61730=CARTESIAN_POINT('Ctrl Pts',(-21.2907042434478,-18.8025118189363,
-11.4407020668845));
#61731=CARTESIAN_POINT('Ctrl Pts',(-21.2842464642989,-18.7287446051466,
-11.444408045441));
#61732=CARTESIAN_POINT('Ctrl Pts',(-21.2769546129518,-18.6454497843058,
-11.4485926798341));
#61733=CARTESIAN_POINT('Ctrl Pts',(-21.2655641024497,-18.5623575749322,
-11.4527773142271));
#61734=CARTESIAN_POINT('Ctrl Pts',(-21.250093180474,-18.4799034980303,-11.4569619486201));
#61735=CARTESIAN_POINT('Ctrl Pts',(-21.2346442794409,-18.3975667843011,
-11.4611406267041));
#61736=CARTESIAN_POINT('Ctrl Pts',(-21.2151265874821,-18.3158668471444,
-11.465319304788));
#61737=CARTESIAN_POINT('Ctrl Pts',(-21.1916101807317,-18.2352349062881,
-11.469497982872));
#61738=CARTESIAN_POINT('Ctrl Pts',(-21.1676722592913,-18.1531576958412,
-11.4737515607574));
#61739=CARTESIAN_POINT('Ctrl Pts',(-21.1395909011584,-18.07218762626,-11.4780051386429));
#61740=CARTESIAN_POINT('Ctrl Pts',(-21.1074946738889,-17.9927695620858,
-11.4822587165283));
#61741=CARTESIAN_POINT('Ctrl Pts',(-21.0760206946157,-17.9148911720574,
-11.4864298305062));
#61742=CARTESIAN_POINT('Ctrl Pts',(-21.0406863094724,-17.8385055933015,
-11.4906009444842));
#61743=CARTESIAN_POINT('Ctrl Pts',(-21.0016627302193,-17.7640161019717,
-11.4947720584621));
#61744=CARTESIAN_POINT('Ctrl Pts',(-20.962652245705,-17.6895516063101,-11.4989417727825));
#61745=CARTESIAN_POINT('Ctrl Pts',(-20.9199552389621,-17.6169823416316,
-11.5031114871029));
#61746=CARTESIAN_POINT('Ctrl Pts',(-20.8737897249261,-17.5466886704004,
-11.5072812014233));
#61747=CARTESIAN_POINT('Ctrl Pts',(-20.8276258536571,-17.4763975005198,
-11.5114507673673));
#61748=CARTESIAN_POINT('Ctrl Pts',(-20.7779939737416,-17.4083821471397,
-11.5156203333113));
#61749=CARTESIAN_POINT('Ctrl Pts',(-20.725155694621,-17.3429944065422,-11.5197898992554));
#61750=CARTESIAN_POINT('Ctrl Pts',(-20.6704596867895,-17.2753077136497,
-11.5241060619943));
#61751=CARTESIAN_POINT('Ctrl Pts',(-20.6123279420988,-17.2104372553888,
-11.5284222247332));
#61752=CARTESIAN_POINT('Ctrl Pts',(-20.5510951122123,-17.1487348078626,
-11.5327383874721));
#61753=CARTESIAN_POINT('Ctrl Pts',(-20.4918569353188,-17.0890423110747,
-11.5369139516638));
#61754=CARTESIAN_POINT('Ctrl Pts',(-20.4297169860238,-17.0323148814138,
-11.5410895158555));
#61755=CARTESIAN_POINT('Ctrl Pts',(-20.3650134540526,-16.9788312001506,
-11.5452650800472));
#61756=CARTESIAN_POINT('Ctrl Pts',(-20.2970419004996,-16.9226461852921,
-11.5496515420597));
#61757=CARTESIAN_POINT('Ctrl Pts',(-20.2262414538865,-16.8700415621995,
-11.5540380040722));
#61758=CARTESIAN_POINT('Ctrl Pts',(-20.1530384991427,-16.8212889126043,
-11.5584244660848));
#61759=CARTESIAN_POINT('Ctrl Pts',(-20.0798355443989,-16.7725362630091,
-11.5628109280973));
#61760=CARTESIAN_POINT('Ctrl Pts',(-20.0042306192382,-16.7276358177823,
-11.5671973901099));
#61761=CARTESIAN_POINT('Ctrl Pts',(-19.9266775857363,-16.6868023979171,
-11.5715838521224));
#61762=CARTESIAN_POINT('Ctrl Pts',(-19.852692882267,-16.6478477842295,-11.5757684865155));
#61763=CARTESIAN_POINT('Ctrl Pts',(-19.7766600165143,-16.6124491640088,
-11.5799531209085));
#61764=CARTESIAN_POINT('Ctrl Pts',(-19.6989550698441,-16.5808269331021,
-11.5841377553016));
#61765=CARTESIAN_POINT('Ctrl Pts',(-19.6213607265476,-16.549249712527,-11.5883164333855));
#61766=CARTESIAN_POINT('Ctrl Pts',(-19.5420994522192,-16.5214383763015,
-11.5924951114694));
#61767=CARTESIAN_POINT('Ctrl Pts',(-19.4615717652903,-16.4975674125468,
-11.5966737895534));
#61768=CARTESIAN_POINT('Ctrl Pts',(-19.3796006774474,-16.4732685789225,
-11.6009273674388));
#61769=CARTESIAN_POINT('Ctrl Pts',(-19.2963177561687,-16.4530529941954,
-11.6051809453242));
#61770=CARTESIAN_POINT('Ctrl Pts',(-19.2121666533115,-16.4370533501363,
-11.6094345232097));
#61771=CARTESIAN_POINT('Ctrl Pts',(-19.1296469837906,-16.4213638903979,
-11.6136056371876));
#61772=CARTESIAN_POINT('Ctrl Pts',(-19.0462929678283,-16.4097284515022,
-11.6177767511656));
#61773=CARTESIAN_POINT('Ctrl Pts',(-18.9625363705284,-16.4022213571869,
-11.6219478651435));
#61774=CARTESIAN_POINT('Ctrl Pts',(-18.8788078785636,-16.3947167819496,
-11.6261175794639));
#61775=CARTESIAN_POINT('Ctrl Pts',(-18.794677531367,-16.3913378410871,-11.6302872937843));
#61776=CARTESIAN_POINT('Ctrl Pts',(-18.7105831609267,-16.3921071015279,
-11.6344570081047));
#61777=CARTESIAN_POINT('Ctrl Pts',(-18.6264917829249,-16.3928763345952,
-11.6386265740487));
#61778=CARTESIAN_POINT('Ctrl Pts',(-18.54243683914,-16.3977934704174,-11.6427961399927));
#61779=CARTESIAN_POINT('Ctrl Pts',(-18.4588557388009,-16.4068289575101,
-11.6469657059368));
#61780=CARTESIAN_POINT('Ctrl Pts',(-18.3723360300824,-16.4161821211824,
-11.6512818686757));
#61781=CARTESIAN_POINT('Ctrl Pts',(-18.2863246298123,-16.4299485702282,
-11.6555980314146));
#61782=CARTESIAN_POINT('Ctrl Pts',(-18.2012984666217,-16.4480373252909,
-11.6599141941535));
#61783=CARTESIAN_POINT('Ctrl Pts',(-18.1190420217539,-16.46553684106,-11.6640897583452));
#61784=CARTESIAN_POINT('Ctrl Pts',(-18.0377080547433,-16.4870812228023,
-11.6682653225369));
#61785=CARTESIAN_POINT('Ctrl Pts',(-17.9577139481205,-16.5125369513646,
-11.6724408867286));
#61786=CARTESIAN_POINT('Ctrl Pts',(-17.8736795293402,-16.5392783882614,
-11.6768273487411));
#61787=CARTESIAN_POINT('Ctrl Pts',(-17.7911244272665,-16.570336474695,-11.6812138107537));
#61788=CARTESIAN_POINT('Ctrl Pts',(-17.7105077932321,-16.605499690457,-11.6856002727662));
#61789=CARTESIAN_POINT('Ctrl Pts',(-17.6298911591977,-16.640662906219,-11.6899867347788));
#61790=CARTESIAN_POINT('Ctrl Pts',(-17.5512134783828,-16.6799309241434,
-11.6943731967913));
#61791=CARTESIAN_POINT('Ctrl Pts',(-17.4749010481801,-16.7230383965788,
-11.6987596588038));
#61792=CARTESIAN_POINT('Ctrl Pts',(-17.4021059540752,-16.7641589912739,
-11.7029439432532));
#61793=CARTESIAN_POINT('Ctrl Pts',(-17.3311919413797,-16.8089259475395,
-11.7071282277026));
#61794=CARTESIAN_POINT('Ctrl Pts',(-17.2625477971695,-16.8571423879449,
-11.7113125121519));
#61795=CARTESIAN_POINT('Ctrl Pts',(-17.2327489339405,-16.8780734539456,
-11.713128936866));
#61796=CARTESIAN_POINT('Ctrl Pts',(-17.2033775631655,-16.8996539586958,
-11.71494536158));
#61797=CARTESIAN_POINT('Ctrl Pts',(-17.1744641548914,-16.9218650419685,
-11.716761786294));
#61798=CARTESIAN_POINT('',(-21.2939995125392,-18.9535798097909,-11.3667098902285));
#61799=CARTESIAN_POINT('Ctrl Pts',(-21.2939995125392,-18.9535798097909,
-11.3667098902285));
#61800=CARTESIAN_POINT('Ctrl Pts',(-21.2940518853803,-18.8687123476393,
-11.3709134538372));
#61801=CARTESIAN_POINT('Ctrl Pts',(-21.2898797137862,-18.7838299700766,
-11.3751170174459));
#61802=CARTESIAN_POINT('Ctrl Pts',(-21.2815050782104,-18.699377996817,-11.3793205810546));
#61803=CARTESIAN_POINT('Ctrl Pts',(-21.2731292177987,-18.6149136719984,
-11.3835247594572));
#61804=CARTESIAN_POINT('Ctrl Pts',(-21.2605497166712,-18.5308803238371,
-11.3877289378599));
#61805=CARTESIAN_POINT('Ctrl Pts',(-21.2438404672875,-18.4477175109462,
-11.3919331162626));
#61806=CARTESIAN_POINT('Ctrl Pts',(-21.2271240709727,-18.3645191274038,
-11.3961390928892));
#61807=CARTESIAN_POINT('Ctrl Pts',(-21.2062745049673,-18.2821924593938,
-11.4003450695159));
#61808=CARTESIAN_POINT('Ctrl Pts',(-21.1814163656274,-18.2011650425965,
-11.4045510461425));
#61809=CARTESIAN_POINT('Ctrl Pts',(-21.1565238219894,-18.1200254817903,
-11.408762843948));
#61810=CARTESIAN_POINT('Ctrl Pts',(-21.1276117659034,-18.0401891906194,
-11.4129746417534));
#61811=CARTESIAN_POINT('Ctrl Pts',(-21.0948539828413,-17.9620664306619,
-11.4171864395589));
#61812=CARTESIAN_POINT('Ctrl Pts',(-21.0620694457193,-17.8838798659899,
-11.4214016772397));
#61813=CARTESIAN_POINT('Ctrl Pts',(-21.0254331231614,-17.8074100228063,
-11.4256169149205));
#61814=CARTESIAN_POINT('Ctrl Pts',(-20.985165001354,-17.7330430127856,-11.4298321526013));
#61815=CARTESIAN_POINT('Ctrl Pts',(-20.9448260993907,-17.6585452862494,
-11.4340547994973));
#61816=CARTESIAN_POINT('Ctrl Pts',(-20.9008428915851,-17.5861581518394,
-11.4382774463933));
#61817=CARTESIAN_POINT('Ctrl Pts',(-20.853478708255,-17.5162388759777,-11.4425000932894));
#61818=CARTESIAN_POINT('Ctrl Pts',(-20.8410561777281,-17.497900666011,-11.4436075959693));
#61819=CARTESIAN_POINT('Ctrl Pts',(-20.828401284867,-17.4797320374709,-11.4447150986492));
#61820=CARTESIAN_POINT('Ctrl Pts',(-20.8155192213963,-17.4617390393097,
-11.4458226013291));
#61821=CARTESIAN_POINT('Ctrl Pts',(-20.766845094615,-17.3937535433782,-11.4500072357222));
#61822=CARTESIAN_POINT('Ctrl Pts',(-20.7147461245074,-17.3280286903786,
-11.4541918701152));
#61823=CARTESIAN_POINT('Ctrl Pts',(-20.6594597008471,-17.2649300724588,
-11.4583765045082));
#61824=CARTESIAN_POINT('Ctrl Pts',(-20.6042519705678,-17.2019212676116,
-11.4625551825922));
#61825=CARTESIAN_POINT('Ctrl Pts',(-20.5458660991116,-17.1415316158069,
-11.4667338606761));
#61826=CARTESIAN_POINT('Ctrl Pts',(-20.4845818988859,-17.0840966258147,
-11.4709125387601));
#61827=CARTESIAN_POINT('Ctrl Pts',(-20.4221992234154,-17.0256321549047,
-11.4751661166455));
#61828=CARTESIAN_POINT('Ctrl Pts',(-20.3568135727528,-16.9702297043271,
-11.479419694531));
#61829=CARTESIAN_POINT('Ctrl Pts',(-20.2887620518454,-16.9182067553113,
-11.4836732724164));
#61830=CARTESIAN_POINT('Ctrl Pts',(-20.2220298424625,-16.8671923726766,
-11.4878443863943));
#61831=CARTESIAN_POINT('Ctrl Pts',(-20.152734588911,-16.8194279167438,-11.4920155003723));
#61832=CARTESIAN_POINT('Ctrl Pts',(-20.081228933945,-16.7751733648401,-11.4961866143502));
#61833=CARTESIAN_POINT('Ctrl Pts',(-20.0097472733921,-16.7309336629788,
-11.5003563286706));
#61834=CARTESIAN_POINT('Ctrl Pts',(-19.9360570753463,-16.6902017679485,
-11.504526042991));
#61835=CARTESIAN_POINT('Ctrl Pts',(-19.8605396057917,-16.6531941107213,
-11.5086957573114));
#61836=CARTESIAN_POINT('Ctrl Pts',(-19.7850248234727,-16.6161877703852,
-11.5128653232554));
#61837=CARTESIAN_POINT('Ctrl Pts',(-19.7076833123969,-16.5829056060341,
-11.5170348891994));
#61838=CARTESIAN_POINT('Ctrl Pts',(-19.6289193227216,-16.5535172700602,
-11.5212044551435));
#61839=CARTESIAN_POINT('Ctrl Pts',(-19.5473860883352,-16.5230956764479,
-11.5255206178824));
#61840=CARTESIAN_POINT('Ctrl Pts',(-19.4643289796728,-16.4968470041692,
-11.5298367806213));
#61841=CARTESIAN_POINT('Ctrl Pts',(-19.3802151086562,-16.4749037093111,
-11.5341529433602));
#61842=CARTESIAN_POINT('Ctrl Pts',(-19.2988412381407,-16.453675214975,-11.5383285075519));
#61843=CARTESIAN_POINT('Ctrl Pts',(-19.2164788667992,-16.4364759603011,
-11.5425040717436));
#61844=CARTESIAN_POINT('Ctrl Pts',(-19.1335609462709,-16.4233736831601,
-11.5466796359353));
#61845=CARTESIAN_POINT('Ctrl Pts',(-19.0464550386954,-16.4096096411485,
-11.5510660979478));
#61846=CARTESIAN_POINT('Ctrl Pts',(-18.9587365661204,-16.4003673913993,
-11.5554525599604));
#61847=CARTESIAN_POINT('Ctrl Pts',(-18.8709107816371,-16.3956636688668,
-11.5598390219729));
#61848=CARTESIAN_POINT('Ctrl Pts',(-18.7830849971538,-16.3909599463343,
-11.5642254839854));
#61849=CARTESIAN_POINT('Ctrl Pts',(-18.6951524811212,-16.3907946760441,
-11.568611945998));
#61850=CARTESIAN_POINT('Ctrl Pts',(-18.607613246377,-16.3951217493771,-11.5729984080105));
#61851=CARTESIAN_POINT('Ctrl Pts',(-18.5241126314364,-16.3992491933198,
-11.577182500738));
#61852=CARTESIAN_POINT('Ctrl Pts',(-18.4406590445841,-16.4074789682953,
-11.5813665934654));
#61853=CARTESIAN_POINT('Ctrl Pts',(-18.3576882161454,-16.4198093592045,
-11.5855506861929));
#61854=CARTESIAN_POINT('Ctrl Pts',(-18.2748290034306,-16.4321231627717,
-11.5897291503091));
#61855=CARTESIAN_POINT('Ctrl Pts',(-18.1924517105566,-16.4485265622829,
-11.5939076144253));
#61856=CARTESIAN_POINT('Ctrl Pts',(-18.1109898384805,-16.4689659006281,
-11.5980860785415));
#61857=CARTESIAN_POINT('Ctrl Pts',(-18.0265307040886,-16.4901572724956,
-11.6024182827169));
#61858=CARTESIAN_POINT('Ctrl Pts',(-17.9430561635435,-16.5156873289273,
-11.6067504868923));
#61859=CARTESIAN_POINT('Ctrl Pts',(-17.8610409031935,-16.5454376352766,
-11.6110826910677));
#61860=CARTESIAN_POINT('Ctrl Pts',(-17.7820790639581,-16.5740803402701,
-11.6152536076529));
#61861=CARTESIAN_POINT('Ctrl Pts',(-17.7044702469478,-16.6066344546583,
-11.6194245242381));
#61862=CARTESIAN_POINT('Ctrl Pts',(-17.628623544901,-16.6429432894551,-11.6235954408233));
#61863=CARTESIAN_POINT('Ctrl Pts',(-17.5528073678039,-16.6792375115484,
-11.6277646787987));
#61864=CARTESIAN_POINT('Ctrl Pts',(-17.4787523097007,-16.7192832503609,
-11.631933916774));
#61865=CARTESIAN_POINT('Ctrl Pts',(-17.4068461498779,-16.7628762807676,
-11.6361031547494));
#61866=CARTESIAN_POINT('Ctrl Pts',(-17.3349387611569,-16.8064700561923,
-11.6402724639783));
#61867=CARTESIAN_POINT('Ctrl Pts',(-17.2651807378934,-16.853611006874,-11.6444417732072));
#61868=CARTESIAN_POINT('Ctrl Pts',(-17.1979329260742,-16.9040503071606,
-11.6486110824361));
#61869=CARTESIAN_POINT('Ctrl Pts',(-17.19007558454,-16.9099437154125,-11.6490982311728));
#61870=CARTESIAN_POINT('Ctrl Pts',(-17.1822524782037,-16.9158821050555,
-11.6495853799095));
#61871=CARTESIAN_POINT('Ctrl Pts',(-17.1744641548914,-16.9218650419685,
-11.6500725286462));
#61872=CARTESIAN_POINT('Ctrl Pts',(-17.1757181146138,-16.9234655268432,
-10.8502164882119));
#61873=CARTESIAN_POINT('Ctrl Pts',(-16.7160810052314,-17.2828444135616,
-10.8791841170091));
#61874=CARTESIAN_POINT('Ctrl Pts',(-15.8690425361355,-18.550019865754,-10.9505436813667));
#61875=CARTESIAN_POINT('Ctrl Pts',(-16.5533151791368,-21.0515010217726,
-11.0642951812848));
#61876=CARTESIAN_POINT('Ctrl Pts',(-19.3189847724962,-21.9220309163904,
-11.1914709879662));
#61877=CARTESIAN_POINT('Ctrl Pts',(-21.0857645353049,-20.4522478666649,
-11.2922755722919));
#61878=CARTESIAN_POINT('Ctrl Pts',(-21.2926071426957,-19.2766421748681,
-11.3506882210569));
#61879=CARTESIAN_POINT('Ctrl Pts',(-21.2907951752863,-18.9535971086061,
-11.3667089342616));
#61880=CARTESIAN_POINT('Origin',(-18.734,-18.952,1.76670989022851));
#61881=CARTESIAN_POINT('',(-17.1744641548914,-16.9218650419685,-10.0501312754282));
#61882=CARTESIAN_POINT('',(-17.1744641548914,-16.9218650419685,-10.1166694944115));
#61883=CARTESIAN_POINT('',(-17.1744641548914,-16.9218650419685,1.76670989022851));
#61884=CARTESIAN_POINT('',(-21.2939995125392,-18.9504201902087,-10.6332901097715));
#61885=CARTESIAN_POINT('Ctrl Pts',(-17.1744641548914,-16.9218650419685,
-10.1166694944115));
#61886=CARTESIAN_POINT('Ctrl Pts',(-17.1077744001828,-16.9730956572329,
-10.1208396545281));
#61887=CARTESIAN_POINT('Ctrl Pts',(-17.0436265325669,-17.0276044195277,
-10.1250098146447));
#61888=CARTESIAN_POINT('Ctrl Pts',(-16.9823480053276,-17.0851000858213,
-10.1291799747613));
#61889=CARTESIAN_POINT('Ctrl Pts',(-16.9210021848053,-17.1426588912327,
-10.1333547143575));
#61890=CARTESIAN_POINT('Ctrl Pts',(-16.8625323295411,-17.2032108319124,
-10.1375294539537));
#61891=CARTESIAN_POINT('Ctrl Pts',(-16.8072292042644,-17.2664276044321,
-10.1417041935499));
#61892=CARTESIAN_POINT('Ctrl Pts',(-16.7518918010427,-17.3296835599282,
-10.1458815207303));
#61893=CARTESIAN_POINT('Ctrl Pts',(-16.6997253198987,-17.3956072743516,
-10.1500588479107));
#61894=CARTESIAN_POINT('Ctrl Pts',(-16.6509788801178,-17.4638390496574,
-10.1542361750911));
#61895=CARTESIAN_POINT('Ctrl Pts',(-16.6021519993064,-17.5321834205567,
-10.1584203956673));
#61896=CARTESIAN_POINT('Ctrl Pts',(-16.5567566733308,-17.6028430682362,
-10.1626046162435));
#61897=CARTESIAN_POINT('Ctrl Pts',(-16.5149973069474,-17.6754315340627,
-10.1667888368197));
#61898=CARTESIAN_POINT('Ctrl Pts',(-16.4954988473035,-17.7093248469674,
-10.1687425507553));
#61899=CARTESIAN_POINT('Ctrl Pts',(-16.4767924206289,-17.7436383608983,
-10.170696264691));
#61900=CARTESIAN_POINT('Ctrl Pts',(-16.4588952312818,-17.7783312684767,
-10.1726499786266));
#61901=CARTESIAN_POINT('Ctrl Pts',(-16.4205614748832,-17.852639554659,-10.1768346130196));
#61902=CARTESIAN_POINT('Ctrl Pts',(-16.3858007370466,-17.9289661561368,
-10.1810192474127));
#61903=CARTESIAN_POINT('Ctrl Pts',(-16.3548302568731,-18.0069331593007,
-10.1852038818057));
#61904=CARTESIAN_POINT('Ctrl Pts',(-16.3239038593448,-18.0847891860857,
-10.1893825598897));
#61905=CARTESIAN_POINT('Ctrl Pts',(-16.2967571717625,-18.1642805528124,
-10.1935612379736));
#61906=CARTESIAN_POINT('Ctrl Pts',(-16.2735613224932,-18.2450052940591,
-10.1977399160575));
#61907=CARTESIAN_POINT('Ctrl Pts',(-16.2499497042962,-18.327176968277,-10.201993493943));
#61908=CARTESIAN_POINT('Ctrl Pts',(-16.2304321761498,-18.4106262399194,
-10.2062470718284));
#61909=CARTESIAN_POINT('Ctrl Pts',(-16.2151377103692,-18.4949083616214,
-10.2105006497138));
#61910=CARTESIAN_POINT('Ctrl Pts',(-16.2001397576524,-18.577556509931,-10.2146717636918));
#61911=CARTESIAN_POINT('Ctrl Pts',(-16.189202669843,-18.6610050301429,-10.2188428776697));
#61912=CARTESIAN_POINT('Ctrl Pts',(-16.1823971528001,-18.744821549959,-10.2230139916477));
#61913=CARTESIAN_POINT('Ctrl Pts',(-16.1755939194142,-18.8286099443324,
-10.2271837059681));
#61914=CARTESIAN_POINT('Ctrl Pts',(-16.1729195406043,-18.9127656349229,
-10.2313534202884));
#61915=CARTESIAN_POINT('Ctrl Pts',(-16.1743929164357,-18.9968506161326,
-10.2355231346088));
#61916=CARTESIAN_POINT('Ctrl Pts',(-16.175866239838,-19.0809326052378,-10.2396927005528));
#61917=CARTESIAN_POINT('Ctrl Pts',(-16.1814870155133,-19.1649434300175,
-10.2438622664969));
#61918=CARTESIAN_POINT('Ctrl Pts',(-16.1912220304802,-19.2484459440185,
-10.2480318324409));
#61919=CARTESIAN_POINT('Ctrl Pts',(-16.201299316564,-19.3348843034003,-10.2523479951798));
#61920=CARTESIAN_POINT('Ctrl Pts',(-16.2157854771196,-19.4207774186548,
-10.2566641579188));
#61921=CARTESIAN_POINT('Ctrl Pts',(-16.2345855425418,-19.5056491396623,
-10.2609803206577));
#61922=CARTESIAN_POINT('Ctrl Pts',(-16.2527731978103,-19.5877561732848,
-10.2651558848494));
#61923=CARTESIAN_POINT('Ctrl Pts',(-16.2749978531257,-19.6689068927544,
-10.269331449041));
#61924=CARTESIAN_POINT('Ctrl Pts',(-16.3011224991715,-19.7486850481605,
-10.2735070132327));
#61925=CARTESIAN_POINT('Ctrl Pts',(-16.3285666389836,-19.8324926085417,
-10.2778934752453));
#61926=CARTESIAN_POINT('Ctrl Pts',(-16.3603148903334,-19.9147847597323,
-10.2822799372578));
#61927=CARTESIAN_POINT('Ctrl Pts',(-16.3961518958429,-19.9951041376052,
-10.2866663992704));
#61928=CARTESIAN_POINT('Ctrl Pts',(-16.4319889013525,-20.0754235154782,
-10.2910528612829));
#61929=CARTESIAN_POINT('Ctrl Pts',(-16.4719143298048,-20.1537696376097,
-10.2954393232955));
#61930=CARTESIAN_POINT('Ctrl Pts',(-16.5156592733601,-20.2297184433711,
-10.299825785308));
#61931=CARTESIAN_POINT('Ctrl Pts',(-16.5573914472169,-20.3021727319963,
-10.3040104197011));
#61932=CARTESIAN_POINT('Ctrl Pts',(-16.6027547120117,-20.3727151532423,
-10.3081950540941));
#61933=CARTESIAN_POINT('Ctrl Pts',(-16.6515488896105,-20.4409584859349,
-10.3123796884872));
#61934=CARTESIAN_POINT('Ctrl Pts',(-16.7002736147369,-20.5091046826902,
-10.3165583665711));
#61935=CARTESIAN_POINT('Ctrl Pts',(-16.752419287262,-20.5749579200268,-10.3207370446551));
#61936=CARTESIAN_POINT('Ctrl Pts',(-16.807740546418,-20.6381567298107,-10.324915722739));
#61937=CARTESIAN_POINT('Ctrl Pts',(-16.8640533993856,-20.7024883328398,
-10.3291693006244));
#61938=CARTESIAN_POINT('Ctrl Pts',(-16.9236565628968,-20.7640689932945,
-10.3334228785099));
#61939=CARTESIAN_POINT('Ctrl Pts',(-16.9862458850687,-20.8225495325547,
-10.3376764563953));
#61940=CARTESIAN_POINT('Ctrl Pts',(-17.0476217910972,-20.8798963124459,
-10.3418475703733));
#61941=CARTESIAN_POINT('Ctrl Pts',(-17.1118687523879,-20.9342617737264,
-10.3460186843512));
#61942=CARTESIAN_POINT('Ctrl Pts',(-17.178661484003,-20.9853524290335,-10.3501897983292));
#61943=CARTESIAN_POINT('Ctrl Pts',(-17.2454318026719,-21.0364259403777,
-10.3543595126495));
#61944=CARTESIAN_POINT('Ctrl Pts',(-17.3147458300056,-21.0842265489049,
-10.3585292269699));
#61945=CARTESIAN_POINT('Ctrl Pts',(-17.3862455028589,-21.1285012785284,
-10.3626989412903));
#61946=CARTESIAN_POINT('Ctrl Pts',(-17.4577426314471,-21.1727744326672,
-10.3668685072343));
#61947=CARTESIAN_POINT('Ctrl Pts',(-17.5314248593523,-21.2135217158933,
-10.3710380731784));
#61948=CARTESIAN_POINT('Ctrl Pts',(-17.6069066380304,-21.2505344359839,
-10.3752076391224));
#61949=CARTESIAN_POINT('Ctrl Pts',(-17.6850422629298,-21.2888484776527,
-10.3795238018614));
#61950=CARTESIAN_POINT('Ctrl Pts',(-17.7651058639355,-21.3231602233056,
-10.3838399646003));
#61951=CARTESIAN_POINT('Ctrl Pts',(-17.8466456689033,-21.3532917963221,
-10.3881561273392));
#61952=CARTESIAN_POINT('Ctrl Pts',(-17.9255293233008,-21.382441836517,-10.3923316915309));
#61953=CARTESIAN_POINT('Ctrl Pts',(-18.0057940203934,-21.4076797638284,
-10.3965072557226));
#61954=CARTESIAN_POINT('Ctrl Pts',(-18.0870155993347,-21.4288954732277,
-10.4006828199143));
#61955=CARTESIAN_POINT('Ctrl Pts',(-18.1723394871422,-21.4511827376731,
-10.4050692819268));
#61956=CARTESIAN_POINT('Ctrl Pts',(-18.2587188895804,-21.469030663203,-10.4094557439393));
#61957=CARTESIAN_POINT('Ctrl Pts',(-18.345652666934,-21.4823727687636,-10.4138422059519));
#61958=CARTESIAN_POINT('Ctrl Pts',(-18.4325864442876,-21.4957148743243,
-10.4182286679644));
#61959=CARTESIAN_POINT('Ctrl Pts',(-18.5200740116329,-21.50455117729,-10.4226151299769));
#61960=CARTESIAN_POINT('Ctrl Pts',(-18.607613246377,-21.5088782506229,-10.4270015919895));
#61961=CARTESIAN_POINT('Ctrl Pts',(-18.6911246711665,-21.5130062288976,
-10.4311862263825));
#61962=CARTESIAN_POINT('Ctrl Pts',(-18.7749939587053,-21.5130461767751,
-10.4353708607756));
#61963=CARTESIAN_POINT('Ctrl Pts',(-18.8587871646378,-21.5089568169098,
-10.4395554951686));
#61964=CARTESIAN_POINT('Ctrl Pts',(-18.9424611013128,-21.5048732777422,
-10.4437341732526));
#61965=CARTESIAN_POINT('Ctrl Pts',(-19.0260587159289,-21.4966721277451,
-10.4479128513365));
#61966=CARTESIAN_POINT('Ctrl Pts',(-19.109143261859,-21.4843640206498,-10.4520915294204));
#61967=CARTESIAN_POINT('Ctrl Pts',(-19.1937170385632,-21.4718352995806,
-10.4563451073059));
#61968=CARTESIAN_POINT('Ctrl Pts',(-19.2777586906,-21.4550509150073,-10.4605986851913));
#61969=CARTESIAN_POINT('Ctrl Pts',(-19.3608099823631,-21.4340776067661,
-10.4648522630768));
#61970=CARTESIAN_POINT('Ctrl Pts',(-19.4422511627742,-21.4135109070312,
-10.4690233770547));
#61971=CARTESIAN_POINT('Ctrl Pts',(-19.5227395737971,-21.3889163729564,
-10.4731944910327));
#61972=CARTESIAN_POINT('Ctrl Pts',(-19.6018523684378,-21.3604086585538,
-10.4773656050106));
#61973=CARTESIAN_POINT('Ctrl Pts',(-19.6809386160161,-21.3319105101902,
-10.481535319331));
#61974=CARTESIAN_POINT('Ctrl Pts',(-19.7586497315282,-21.2995019451708,
-10.4857050336513));
#61975=CARTESIAN_POINT('Ctrl Pts',(-19.8345791893306,-21.2633471067783,
-10.4898747479717));
#61976=CARTESIAN_POINT('Ctrl Pts',(-19.9105059452373,-21.22719355493,-10.4940443139158));
#61977=CARTESIAN_POINT('Ctrl Pts',(-19.9846507545042,-21.1872941933041,
-10.4982138798598));
#61978=CARTESIAN_POINT('Ctrl Pts',(-20.0566294498838,-21.1438602460696,
-10.5023834458039));
#61979=CARTESIAN_POINT('Ctrl Pts',(-20.1311388273975,-21.0988992148319,
-10.5066996085428));
#61980=CARTESIAN_POINT('Ctrl Pts',(-20.2033264842381,-21.0501506938738,
-10.5110157712817));
#61981=CARTESIAN_POINT('Ctrl Pts',(-20.2727983186246,-20.9978982708332,
-10.5153319340206));
#61982=CARTESIAN_POINT('Ctrl Pts',(-20.3400071153131,-20.9473479649771,
-10.5195074982123));
#61983=CARTESIAN_POINT('Ctrl Pts',(-20.4046739763892,-20.8935188682645,
-10.523683062404));
#61984=CARTESIAN_POINT('Ctrl Pts',(-20.466476730727,-20.8367080350785,-10.5278586265957));
#61985=CARTESIAN_POINT('Ctrl Pts',(-20.5314009952643,-20.7770278217633,
-10.5322450886082));
#61986=CARTESIAN_POINT('Ctrl Pts',(-20.5931638083644,-20.7140571577261,
-10.5366315506207));
#61987=CARTESIAN_POINT('Ctrl Pts',(-20.651438012559,-20.6481814372272,-10.5410180126333));
#61988=CARTESIAN_POINT('Ctrl Pts',(-20.7097122167535,-20.5823057167282,
-10.5454044746458));
#61989=CARTESIAN_POINT('Ctrl Pts',(-20.7644975100435,-20.513525441,-10.5497909366584));
#61990=CARTESIAN_POINT('Ctrl Pts',(-20.8155192213965,-20.4422609606901,
-10.5541773986709));
#61991=CARTESIAN_POINT('Ctrl Pts',(-20.8646271615163,-20.3736695367859,
-10.5583993290636));
#61992=CARTESIAN_POINT('Ctrl Pts',(-20.9104308246501,-20.302523084569,-10.5626212594563));
#61993=CARTESIAN_POINT('Ctrl Pts',(-20.9526566798058,-20.2291697370174,
-10.5668431898491));
#61994=CARTESIAN_POINT('Ctrl Pts',(-20.9948201353165,-20.1559247880485,
-10.5710588812454));
#61995=CARTESIAN_POINT('Ctrl Pts',(-21.0334160638335,-20.0804798079433,
-10.5752745726417));
#61996=CARTESIAN_POINT('Ctrl Pts',(-21.0682129788551,-20.003213474678,-10.5794902640381));
#61997=CARTESIAN_POINT('Ctrl Pts',(-21.1029682787105,-19.9260395476302,
-10.583700913703));
#61998=CARTESIAN_POINT('Ctrl Pts',(-21.1339334100815,-19.8470490030809,
-10.587911563368));
#61999=CARTESIAN_POINT('Ctrl Pts',(-21.1609223976385,-19.7666457364035,
-10.592122213033));
#62000=CARTESIAN_POINT('Ctrl Pts',(-21.1878844462892,-19.6863227237952,
-10.5963286598616));
#62001=CARTESIAN_POINT('Ctrl Pts',(-21.2108781024615,-19.6045902181226,
-10.6005351066903));
#62002=CARTESIAN_POINT('Ctrl Pts',(-21.2297657078558,-19.5218715043685,
-10.6047415535189));
#62003=CARTESIAN_POINT('Ctrl Pts',(-21.24864245849,-19.4392003292924,-10.6089455828907));
#62004=CARTESIAN_POINT('Ctrl Pts',(-21.2634177498248,-19.3555445100527,
-10.6131496122625));
#62005=CARTESIAN_POINT('Ctrl Pts',(-21.27400421321,-19.2713408788045,-10.6173536416343));
#62006=CARTESIAN_POINT('Ctrl Pts',(-21.2845883389273,-19.1871558411237,
-10.6215567426863));
#62007=CARTESIAN_POINT('Ctrl Pts',(-21.2909854180498,-19.1024236771956,
-10.6257598437382));
#62008=CARTESIAN_POINT('Ctrl Pts',(-21.2931596531403,-19.0175886403171,
-10.6299629447901));
#62009=CARTESIAN_POINT('Ctrl Pts',(-21.2937333596144,-18.99520356793,-10.6310719997839));
#62010=CARTESIAN_POINT('Ctrl Pts',(-21.2940133304248,-18.9728113543426,
-10.6321810547777));
#62011=CARTESIAN_POINT('Ctrl Pts',(-21.2939995125392,-18.9504201902087,
-10.6332901097715));
#62012=CARTESIAN_POINT('Ctrl Pts',(-21.2907951936029,-18.9504028914923,
-10.633291065733));
#62013=CARTESIAN_POINT('Ctrl Pts',(-21.2926071610387,-18.6273578228792,
-10.6493117789394));
#62014=CARTESIAN_POINT('Ctrl Pts',(-21.0857645521851,-17.4517521226135,
-10.7077244277063));
#62015=CARTESIAN_POINT('Ctrl Pts',(-19.4306370810863,-16.0748525489571,
-10.802158628871));
#62016=CARTESIAN_POINT('Ctrl Pts',(-17.7502562881359,-16.4853659944509,
-10.8805721168292));
#62017=CARTESIAN_POINT('Ctrl Pts',(-17.1731949518433,-16.9201829956178,
-10.9165936692269));
#62018=CARTESIAN_POINT('',(-21.2940195635259,-18.9533010451044,-10.566709896691));
#62019=CARTESIAN_POINT('Ctrl Pts',(-21.2974134575541,-18.9532806863302,
-10.5667109991706));
#62020=CARTESIAN_POINT('Ctrl Pts',(-21.2925956544959,-18.178366843738,-10.6053965865272));
#62021=CARTESIAN_POINT('Ctrl Pts',(-20.5048167981983,-16.5458335938225,
-10.6864741094444));
#62022=CARTESIAN_POINT('Ctrl Pts',(-18.3777720107911,-16.2028740463623,
-10.7809759391248));
#62023=CARTESIAN_POINT('Ctrl Pts',(-17.3887251784425,-16.7569205723577,
-10.8367921814486));
#62024=CARTESIAN_POINT('Ctrl Pts',(-17.1757181146138,-16.9234655268432,
-10.8502164882119));
#62025=CARTESIAN_POINT('Ctrl Pts',(-17.1744641548914,-16.9218650419685,
-10.0501312754282));
#62026=CARTESIAN_POINT('Ctrl Pts',(-17.1081215409048,-16.972828986095,-10.0543142385325));
#62027=CARTESIAN_POINT('Ctrl Pts',(-17.0441627240079,-17.0271382362881,
-10.0584972016367));
#62028=CARTESIAN_POINT('Ctrl Pts',(-16.9829439471694,-17.084541111605,-10.0626801647409));
#62029=CARTESIAN_POINT('Ctrl Pts',(-16.9218070707038,-17.1418671915801,
-10.0668575317478));
#62030=CARTESIAN_POINT('Ctrl Pts',(-16.8634032855558,-17.2022783629591,
-10.0710348987546));
#62031=CARTESIAN_POINT('Ctrl Pts',(-16.8080570528915,-17.2654817627778,
-10.0752122657615));
#62032=CARTESIAN_POINT('Ctrl Pts',(-16.7527684355283,-17.3286193680025,
-10.0793852841388));
#62033=CARTESIAN_POINT('Ctrl Pts',(-16.7005313462713,-17.3945430800416,
-10.0835583025162));
#62034=CARTESIAN_POINT('Ctrl Pts',(-16.6516335517556,-17.4629231130576,
-10.0877313208936));
#62035=CARTESIAN_POINT('Ctrl Pts',(-16.6027633272263,-17.5312645914395,
-10.0919019864029));
#62036=CARTESIAN_POINT('Ctrl Pts',(-16.5572289263105,-17.6020592677418,
-10.0960726519122));
#62037=CARTESIAN_POINT('Ctrl Pts',(-16.515277225619,-17.6749450871466,-10.1002433174215));
#62038=CARTESIAN_POINT('Ctrl Pts',(-16.4733365938618,-17.7478116756661,
-10.1044128825029));
#62039=CARTESIAN_POINT('Ctrl Pts',(-16.4349770140236,-17.8227679128389,
-10.1085824475843));
#62040=CARTESIAN_POINT('Ctrl Pts',(-16.4004007511752,-17.8994248027412,
-10.1127520126657));
#62041=CARTESIAN_POINT('Ctrl Pts',(-16.3658232392718,-17.9760844618461,
-10.1169217283712));
#62042=CARTESIAN_POINT('Ctrl Pts',(-16.335029503705,-18.0544444757753,-10.1210914440766));
#62043=CARTESIAN_POINT('Ctrl Pts',(-16.3081741883135,-18.1340946684636,
-10.125261159782));
#62044=CARTESIAN_POINT('Ctrl Pts',(-16.2812914154966,-18.213826297143,-10.1294351386904));
#62045=CARTESIAN_POINT('Ctrl Pts',(-16.2583552528147,-18.2948503023518,
-10.1336091175987));
#62046=CARTESIAN_POINT('Ctrl Pts',(-16.2394706734754,-18.3767405462675,
-10.137783096507));
#62047=CARTESIAN_POINT('Ctrl Pts',(-16.2205765545129,-18.4586721573776,
-10.141959183918));
#62048=CARTESIAN_POINT('Ctrl Pts',(-16.2057381766318,-18.5414704255045,
-10.146135271329));
#62049=CARTESIAN_POINT('Ctrl Pts',(-16.1950090364198,-18.6247006158602,
-10.15031135874));
#62050=CARTESIAN_POINT('Ctrl Pts',(-16.1842607815537,-18.7080790861592,
-10.1544948861196));
#62051=CARTESIAN_POINT('Ctrl Pts',(-16.177636427472,-18.7918905566104,-10.1586784134992));
#62052=CARTESIAN_POINT('Ctrl Pts',(-16.1751373938136,-18.875696902679,-10.1628619408788));
#62053=CARTESIAN_POINT('Ctrl Pts',(-16.1729067675168,-18.9505020733664,
-10.1665961387575));
#62054=CARTESIAN_POINT('Ctrl Pts',(-16.1739621469759,-19.0253029292838,
-10.1703303366361));
#62055=CARTESIAN_POINT('Ctrl Pts',(-16.1782696504243,-19.0997916785801,
-10.1740645345148));
#62056=CARTESIAN_POINT('Ctrl Pts',(-16.1830967452018,-19.1832656112237,
-10.1782491689078));
#62057=CARTESIAN_POINT('Ctrl Pts',(-16.1920266966377,-19.2666581465938,
-10.1824338033009));
#62058=CARTESIAN_POINT('Ctrl Pts',(-16.205054135763,-19.3495334146438,-10.1866184376939));
#62059=CARTESIAN_POINT('Ctrl Pts',(-16.2180630319411,-19.4322907200076,
-10.1907971157779));
#62060=CARTESIAN_POINT('Ctrl Pts',(-16.235157760266,-19.514531769942,-10.1949757938618));
#62061=CARTESIAN_POINT('Ctrl Pts',(-16.2562810188397,-19.595823462137,-10.1991544719458));
#62062=CARTESIAN_POINT('Ctrl Pts',(-16.2777828966423,-19.6785722494913,
-10.2034080498312));
#62063=CARTESIAN_POINT('Ctrl Pts',(-16.3034591202046,-19.7603368285348,
-10.2076616277166));
#62064=CARTESIAN_POINT('Ctrl Pts',(-16.3331943249928,-19.840668729535,-10.2119152056021));
#62065=CARTESIAN_POINT('Ctrl Pts',(-16.3623530548127,-19.9194432398795,
-10.21608631958));
#62066=CARTESIAN_POINT('Ctrl Pts',(-16.3954146207213,-19.9968396756824,
-10.220257433558));
#62067=CARTESIAN_POINT('Ctrl Pts',(-16.4322198035646,-20.0724498771911,
-10.2244285475359));
#62068=CARTESIAN_POINT('Ctrl Pts',(-16.4690126360733,-20.1480347069665,
-10.2285982618563));
#62069=CARTESIAN_POINT('Ctrl Pts',(-16.5095463894923,-20.2218340795556,
-10.2327679761767));
#62070=CARTESIAN_POINT('Ctrl Pts',(-16.5536143847776,-20.2934613557352,
-10.236937690497));
#62071=CARTESIAN_POINT('Ctrl Pts',(-16.5976808119344,-20.365086083109,-10.2411072564411));
#62072=CARTESIAN_POINT('Ctrl Pts',(-16.6452809891204,-20.4345384763812,
-10.2452768223851));
#62073=CARTESIAN_POINT('Ctrl Pts',(-16.6961638176234,-20.5014591617066,
-10.2494463883292));
#62074=CARTESIAN_POINT('Ctrl Pts',(-16.7488356236058,-20.5707326957725,
-10.2537625510681));
#62075=CARTESIAN_POINT('Ctrl Pts',(-16.805024892642,-20.6372927599322,-10.258078713807));
#62076=CARTESIAN_POINT('Ctrl Pts',(-16.8644075151043,-20.7007778419289,
-10.2623948765459));
#62077=CARTESIAN_POINT('Ctrl Pts',(-16.9218557548858,-20.762194904057,-10.2665704407376));
#62078=CARTESIAN_POINT('Ctrl Pts',(-16.9822921248587,-20.820733948795,-10.2707460049293));
#62079=CARTESIAN_POINT('Ctrl Pts',(-17.0453868187422,-20.8761064222341,
-10.274921569121));
#62080=CARTESIAN_POINT('Ctrl Pts',(-17.1116682756204,-20.934275627671,-10.2793080311335));
#62081=CARTESIAN_POINT('Ctrl Pts',(-17.1808831995725,-20.9889496060668,
-10.283694493146));
#62082=CARTESIAN_POINT('Ctrl Pts',(-17.2526134178258,-21.0398442935608,
-10.2880809551586));
#62083=CARTESIAN_POINT('Ctrl Pts',(-17.3243436360791,-21.0907389810547,
-10.2924674171711));
#62084=CARTESIAN_POINT('Ctrl Pts',(-17.3985886179774,-21.1378541309858,
-10.2968538791837));
#62085=CARTESIAN_POINT('Ctrl Pts',(-17.4749010481802,-21.1809616034213,
-10.3012403411962));
#62086=CARTESIAN_POINT('Ctrl Pts',(-17.5477022303472,-21.2220856371494,
-10.3054249755892));
#62087=CARTESIAN_POINT('Ctrl Pts',(-17.6226557687809,-21.2597157589185,
-10.3096096099823));
#62088=CARTESIAN_POINT('Ctrl Pts',(-17.6993922596291,-21.2936205549928,
-10.3137942443753));
#62089=CARTESIAN_POINT('Ctrl Pts',(-17.7760195255806,-21.3274770917864,
-10.3179729224593));
#62090=CARTESIAN_POINT('Ctrl Pts',(-17.8544242858621,-21.3576186510691,
-10.3221516005432));
#62091=CARTESIAN_POINT('Ctrl Pts',(-17.9342113535405,-21.383858984603,-10.3263302786272));
#62092=CARTESIAN_POINT('Ctrl Pts',(-18.0154285470652,-21.410569657257,-10.3305838565126));
#62093=CARTESIAN_POINT('Ctrl Pts',(-18.0980776713418,-21.4332376324399,
-10.334837434398));
#62094=CARTESIAN_POINT('Ctrl Pts',(-18.1817191896631,-21.4517171653076,
-10.3390910122835));
#62095=CARTESIAN_POINT('Ctrl Pts',(-18.2637391539388,-21.4698384363709,
-10.3432621262614));
#62096=CARTESIAN_POINT('Ctrl Pts',(-18.3467129067617,-21.4839321143086,
-10.3474332402394));
#62097=CARTESIAN_POINT('Ctrl Pts',(-18.4302110680643,-21.4939111480997,
-10.3516043542173));
#62098=CARTESIAN_POINT('Ctrl Pts',(-18.5136812107525,-21.5038868333295,
-10.3557740685377));
#62099=CARTESIAN_POINT('Ctrl Pts',(-18.5976749560383,-21.5097505619763,
-10.3599437828581));
#62100=CARTESIAN_POINT('Ctrl Pts',(-18.6817553300755,-21.5114668379302,
-10.3641134971784));
#62101=CARTESIAN_POINT('Ctrl Pts',(-18.7658327121721,-21.5131830528116,
-10.3682830631225));
#62102=CARTESIAN_POINT('Ctrl Pts',(-18.8499962569365,-21.510752099899,-10.3724526290665));
#62103=CARTESIAN_POINT('Ctrl Pts',(-18.9338078728666,-21.5041905912256,
-10.3766221950106));
#62104=CARTESIAN_POINT('Ctrl Pts',(-19.02056620182,-21.4973983880017,-10.3809383577495));
#62105=CARTESIAN_POINT('Ctrl Pts',(-19.1069468680352,-21.4861798052051,
-10.3852545204884));
#62106=CARTESIAN_POINT('Ctrl Pts',(-19.1924704625208,-21.4706116880131,
-10.3895706832273));
#62107=CARTESIAN_POINT('Ctrl Pts',(-19.2752081349115,-21.4555507006011,
-10.393746247419));
#62108=CARTESIAN_POINT('Ctrl Pts',(-19.3571432683313,-21.4364193523527,
-10.3979218116107));
#62109=CARTESIAN_POINT('Ctrl Pts',(-19.4378547167233,-21.4133387693989,
-10.4020973758024));
#62110=CARTESIAN_POINT('Ctrl Pts',(-19.5226427085004,-21.3890924410691,
-10.4064838378149));
#62111=CARTESIAN_POINT('Ctrl Pts',(-19.6060795975569,-21.3604876310562,
-10.4108702998275));
#62112=CARTESIAN_POINT('Ctrl Pts',(-19.6877001821498,-21.3277221981047,
-10.41525676184));
#62113=CARTESIAN_POINT('Ctrl Pts',(-19.7693207667426,-21.2949567651532,
-10.4196432238525));
#62114=CARTESIAN_POINT('Ctrl Pts',(-19.8491245522346,-21.2580310219481,
-10.4240296858651));
#62115=CARTESIAN_POINT('Ctrl Pts',(-19.9266775857364,-21.2171976020829,
-10.4284161478776));
#62116=CARTESIAN_POINT('Ctrl Pts',(-20.0006622892057,-21.1782429883953,
-10.4326007822707));
#62117=CARTESIAN_POINT('Ctrl Pts',(-20.0728741952655,-21.1355873954291,
-10.4367854166637));
#62118=CARTESIAN_POINT('Ctrl Pts',(-20.1429187702871,-21.0894161734984,
-10.4409700510568));
#62119=CARTESIAN_POINT('Ctrl Pts',(-20.212863645526,-21.0433106705873,-10.4451487291407));
#62120=CARTESIAN_POINT('Ctrl Pts',(-20.2806469365542,-20.9936997293726,
-10.4493274072247));
#62121=CARTESIAN_POINT('Ctrl Pts',(-20.3458981308864,-20.9408148268869,
-10.4535060853086));
#62122=CARTESIAN_POINT('Ctrl Pts',(-20.4123189059818,-20.8869820005318,
-10.4577596631941));
#62123=CARTESIAN_POINT('Ctrl Pts',(-20.476115489232,-20.829756911557,-10.4620132410795));
#62124=CARTESIAN_POINT('Ctrl Pts',(-20.5369274194047,-20.7694302518553,
-10.4662668189649));
#62125=CARTESIAN_POINT('Ctrl Pts',(-20.5965603916463,-20.7102731421696,
-10.4704379329429));
#62126=CARTESIAN_POINT('Ctrl Pts',(-20.6533230631004,-20.6481339874866,
-10.4746090469208));
#62127=CARTESIAN_POINT('Ctrl Pts',(-20.7069098223475,-20.5833267094254,
-10.4787801608988));
#62128=CARTESIAN_POINT('Ctrl Pts',(-20.7604786000401,-20.5185411780722,
-10.4829498752192));
#62129=CARTESIAN_POINT('Ctrl Pts',(-20.8108732891326,-20.4510896556873,
-10.4871195895395));
#62130=CARTESIAN_POINT('Ctrl Pts',(-20.8578275173592,-20.3813203547519,
-10.4912893038599));
#62131=CARTESIAN_POINT('Ctrl Pts',(-20.9047800747528,-20.3115535365075,
-10.4954588698039));
#62132=CARTESIAN_POINT('Ctrl Pts',(-20.948292158553,-20.2394694858254,-10.499628435748));
#62133=CARTESIAN_POINT('Ctrl Pts',(-20.9881406062299,-20.1654455601079,
-10.503798001692));
#62134=CARTESIAN_POINT('Ctrl Pts',(-21.0293900761687,-20.0888190444805,
-10.508114164431));
#62135=CARTESIAN_POINT('Ctrl Pts',(-21.0667132396993,-20.0101141681398,
-10.5124303271699));
#62136=CARTESIAN_POINT('Ctrl Pts',(-21.0999152164605,-19.9297756330163,
-10.5167464899088));
#62137=CARTESIAN_POINT('Ctrl Pts',(-21.132035642321,-19.8520541172245,-10.5209220541005));
#62138=CARTESIAN_POINT('Ctrl Pts',(-21.160299139743,-19.7728042005822,-10.5250976182921));
#62139=CARTESIAN_POINT('Ctrl Pts',(-21.1845795982613,-19.6924455635532,
-10.5292731824838));
#62140=CARTESIAN_POINT('Ctrl Pts',(-21.210086405018,-19.6080282028024,-10.5336596444964));
#62141=CARTESIAN_POINT('Ctrl Pts',(-21.231197092147,-19.522387742153,-10.5380461065089));
#62142=CARTESIAN_POINT('Ctrl Pts',(-21.2478262226603,-19.4360224398369,
-10.5424325685214));
#62143=CARTESIAN_POINT('Ctrl Pts',(-21.2644553531735,-19.3496571375209,
-10.546819030534));
#62144=CARTESIAN_POINT('Ctrl Pts',(-21.2766029222518,-19.2625675787001,
-10.5512054925465));
#62145=CARTESIAN_POINT('Ctrl Pts',(-21.2842464642989,-19.1752553948527,
-10.555591954559));
#62146=CARTESIAN_POINT('Ctrl Pts',(-21.2907042434478,-19.1014881810632,
-10.5592979331155));
#62147=CARTESIAN_POINT('Ctrl Pts',(-21.293961988618,-19.0274367677245,-10.563003911672));
#62148=CARTESIAN_POINT('Ctrl Pts',(-21.2939996693303,-18.9533011644427,
-10.5667098902285));
#62149=CARTESIAN_POINT('Origin',(-18.734,-18.952,1.76670989022851));
#62150=CARTESIAN_POINT('',(-17.1744641548915,-16.9218650419685,-9.25004024527531));
#62151=CARTESIAN_POINT('',(-17.1750494511462,-16.9226083978001,-9.31680761352202));
#62152=CARTESIAN_POINT('',(-17.1744641548914,-16.9218650419685,1.76670989022851));
#62153=CARTESIAN_POINT('',(-21.2939992159918,-18.9540035272626,-9.8332901097715));
#62154=CARTESIAN_POINT('Ctrl Pts',(-17.1750494511459,-16.9226083978003,
-9.31680761352203));
#62155=CARTESIAN_POINT('Ctrl Pts',(-16.6852502582289,-17.3064745807427,
-9.34773678852736));
#62156=CARTESIAN_POINT('Ctrl Pts',(-15.8397231142329,-18.6405173911589,
-9.42105789909317));
#62157=CARTESIAN_POINT('Ctrl Pts',(-16.6528319614933,-21.1501880163351,
-9.53677094521944));
#62158=CARTESIAN_POINT('Ctrl Pts',(-19.4558314641724,-21.8917704497106,
-9.66394675190088));
#62159=CARTESIAN_POINT('Ctrl Pts',(-21.1196059552395,-20.3720005573578,
-9.76278617060466));
#62160=CARTESIAN_POINT('Ctrl Pts',(-21.2937096219977,-19.2372014343179,
-9.81923365374796));
#62161=CARTESIAN_POINT('Ctrl Pts',(-21.2916488755515,-18.9540199903513,
-9.83328920133079));
#62162=CARTESIAN_POINT('Ctrl Pts',(-21.2939992159918,-18.9540035272626,
-9.8332901097715));
#62163=CARTESIAN_POINT('Ctrl Pts',(-21.2940649620946,-18.8699966984849,
-9.83745593779552));
#62164=CARTESIAN_POINT('Ctrl Pts',(-21.2899913508454,-18.7859395799201,
-9.84162176581954));
#62165=CARTESIAN_POINT('Ctrl Pts',(-21.281790209728,-18.7022700514273,-9.84578759384357));
#62166=CARTESIAN_POINT('Ctrl Pts',(-21.2735905258927,-18.6186153903907,
-9.84995268163077));
#62167=CARTESIAN_POINT('Ctrl Pts',(-21.2612648140692,-18.5353486407622,
-9.85411776941798));
#62168=CARTESIAN_POINT('Ctrl Pts',(-21.244876840873,-18.4529033260305,-9.85828285720518));
#62169=CARTESIAN_POINT('Ctrl Pts',(-21.2284868533626,-18.3704478776001,
-9.86244845694076));
#62170=CARTESIAN_POINT('Ctrl Pts',(-21.2080337038202,-18.2888145159798,
-9.86661405667634));
#62171=CARTESIAN_POINT('Ctrl Pts',(-21.183632148948,-18.2084259721853,-9.87077965641192));
#62172=CARTESIAN_POINT('Ctrl Pts',(-21.1592030081949,-18.1279465493957,
-9.87494996534485));
#62173=CARTESIAN_POINT('Ctrl Pts',(-21.1308166833998,-18.0487151959126,
-9.87912027427778));
#62174=CARTESIAN_POINT('Ctrl Pts',(-21.0986375209737,-17.9711384427947,
-9.88329058321071));
#62175=CARTESIAN_POINT('Ctrl Pts',(-21.0664396371008,-17.8935165564616,
-9.88746331837886));
#62176=CARTESIAN_POINT('Ctrl Pts',(-21.0304447198543,-17.8175516031279,
-9.89163605354701));
#62177=CARTESIAN_POINT('Ctrl Pts',(-20.9908638255707,-17.7436268486802,
-9.89580878871516));
#62178=CARTESIAN_POINT('Ctrl Pts',(-20.951210438291,-17.6695666999462,-9.89998916630977));
#62179=CARTESIAN_POINT('Ctrl Pts',(-20.9079581930336,-17.5975546086432,
-9.90416954390439));
#62180=CARTESIAN_POINT('Ctrl Pts',(-20.8613622504217,-17.5279459787351,
-9.90834992149901));
#62181=CARTESIAN_POINT('Ctrl Pts',(-20.8243993123259,-17.4727278774585,
-9.91166606942059));
#62182=CARTESIAN_POINT('Ctrl Pts',(-20.7853331875372,-17.4190216712153,
-9.91498221734217));
#62183=CARTESIAN_POINT('Ctrl Pts',(-20.7443085775785,-17.3669891410737,
-9.91829836526374));
#62184=CARTESIAN_POINT('Ctrl Pts',(-20.6925397790042,-17.3013294900759,
-9.92248299965679));
#62185=CARTESIAN_POINT('Ctrl Pts',(-20.6374544461771,-17.2380865845811,
-9.92666763404984));
#62186=CARTESIAN_POINT('Ctrl Pts',(-20.5793066365797,-17.1776146368404,
-9.93085226844289));
#62187=CARTESIAN_POINT('Ctrl Pts',(-20.521241593192,-17.1172287634325,-9.93503094652683));
#62188=CARTESIAN_POINT('Ctrl Pts',(-20.4601230476225,-17.0596063422906,
-9.93920962461077));
#62189=CARTESIAN_POINT('Ctrl Pts',(-20.3962460420503,-17.0050695709173,
-9.94338830269471));
#62190=CARTESIAN_POINT('Ctrl Pts',(-20.3312240870607,-16.9495552671121,
-9.94764188058015));
#62191=CARTESIAN_POINT('Ctrl Pts',(-20.2633441071061,-16.897238700291,-9.95189545846559));
#62192=CARTESIAN_POINT('Ctrl Pts',(-20.1929575410585,-16.8484214078413,
-9.95614903635102));
#62193=CARTESIAN_POINT('Ctrl Pts',(-20.1239355559418,-16.8005505338648,
-9.96032015032898));
#62194=CARTESIAN_POINT('Ctrl Pts',(-20.0525037029721,-16.7560447387742,
-9.96449126430693));
#62195=CARTESIAN_POINT('Ctrl Pts',(-19.9790262804939,-16.7151473984905,
-9.96866237828488));
#62196=CARTESIAN_POINT('Ctrl Pts',(-19.9055735140744,-16.6742637817044,
-9.97283209260525));
#62197=CARTESIAN_POINT('Ctrl Pts',(-19.8300769429975,-16.6369864384996,
-9.97700180692563));
#62198=CARTESIAN_POINT('Ctrl Pts',(-19.7529274425307,-16.6035139202333,
-9.981171521246));
#62199=CARTESIAN_POINT('Ctrl Pts',(-19.6757806873741,-16.5700425930628,
-9.98534108719004));
#62200=CARTESIAN_POINT('Ctrl Pts',(-19.5969815421365,-16.5403760039566,
-9.98951065313409));
#62201=CARTESIAN_POINT('Ctrl Pts',(-19.5169416763859,-16.5146649119627,
-9.99368021907813));
#62202=CARTESIAN_POINT('Ctrl Pts',(-19.4340877076954,-16.4880498496923,
-9.99799638181705));
#62203=CARTESIAN_POINT('Ctrl Pts',(-19.3499046498555,-16.4656737716516,
-10.002312544556));
#62204=CARTESIAN_POINT('Ctrl Pts',(-19.264865245119,-16.4476473707713,-10.0066287072949));
#62205=CARTESIAN_POINT('Ctrl Pts',(-19.1825959900472,-16.4302081780036,
-10.0108042714866));
#62206=CARTESIAN_POINT('Ctrl Pts',(-19.0995257948678,-16.4168396609884,
-10.0149798356783));
#62207=CARTESIAN_POINT('Ctrl Pts',(-19.0160902825553,-16.4075894449818,
-10.0191553998699));
#62208=CARTESIAN_POINT('Ctrl Pts',(-18.928440640865,-16.397872022555,-10.0235418618825));
#62209=CARTESIAN_POINT('Ctrl Pts',(-18.8403883907189,-16.3926998996315,
-10.027928323895));
#62210=CARTESIAN_POINT('Ctrl Pts',(-18.7524390182802,-16.3920664066025,
-10.0323147859076));
#62211=CARTESIAN_POINT('Ctrl Pts',(-18.6644896458415,-16.3914329135735,
-10.0367012479201));
#62212=CARTESIAN_POINT('Ctrl Pts',(-18.5766437273768,-16.395337948682,-10.0410877099327));
#62213=CARTESIAN_POINT('Ctrl Pts',(-18.4893986055749,-16.403712308658,-10.0454741719452));
#62214=CARTESIAN_POINT('Ctrl Pts',(-18.4061740830955,-16.4117007450963,
-10.0496584884872));
#62215=CARTESIAN_POINT('Ctrl Pts',(-18.3231864480459,-16.4237853774939,
-10.0538428050293));
#62216=CARTESIAN_POINT('Ctrl Pts',(-18.2408709541789,-16.4399443190551,
-10.0580271215713));
#62217=CARTESIAN_POINT('Ctrl Pts',(-18.1586671962098,-16.4560813263029,
-10.062205758279));
#62218=CARTESIAN_POINT('Ctrl Pts',(-18.0771342151715,-16.4762815730405,
-10.0663843949868));
#62219=CARTESIAN_POINT('Ctrl Pts',(-17.9967026166349,-16.5004713812637,
-10.0705630316945));
#62220=CARTESIAN_POINT('Ctrl Pts',(-17.9163646373239,-16.5246330334991,
-10.074736804633));
#62221=CARTESIAN_POINT('Ctrl Pts',(-17.8371259305098,-16.5527748851385,
-10.0789105775716));
#62222=CARTESIAN_POINT('Ctrl Pts',(-17.7594058894995,-16.5847724402209,
-10.0830843505101));
#62223=CARTESIAN_POINT('Ctrl Pts',(-17.6817391960101,-16.6167480319819,
-10.0872552585448));
#62224=CARTESIAN_POINT('Ctrl Pts',(-17.6055895218756,-16.6525738957107,
-10.0914261665796));
#62225=CARTESIAN_POINT('Ctrl Pts',(-17.5313590153092,-16.6920764035167,
-10.0955970746143));
#62226=CARTESIAN_POINT('Ctrl Pts',(-17.4571459112411,-16.7315696504089,
-10.0997670048271));
#62227=CARTESIAN_POINT('Ctrl Pts',(-17.3848514901433,-16.7747376197236,
-10.1039369350399));
#62228=CARTESIAN_POINT('Ctrl Pts',(-17.3148548334046,-16.821359956227,-10.1081068652527));
#62229=CARTESIAN_POINT('Ctrl Pts',(-17.2669439265524,-16.8532717435255,
-10.1109610749723));
#62230=CARTESIAN_POINT('Ctrl Pts',(-17.2201090559903,-16.8868009398858,
-10.1138152846919));
#62231=CARTESIAN_POINT('Ctrl Pts',(-17.1744641548914,-16.9218650419685,
-10.1166694944115));
#62232=CARTESIAN_POINT('',(-21.2939989766127,-18.9497109517324,-9.7667098901893));
#62233=CARTESIAN_POINT('Ctrl Pts',(-21.293998976612,-18.9497109509451,-9.76670989022851));
#62234=CARTESIAN_POINT('Ctrl Pts',(-21.2938920610985,-18.8301400729742,
-9.77266511192846));
#62235=CARTESIAN_POINT('Ctrl Pts',(-21.2854044483395,-18.7109297707717,
-9.77862033362841));
#62236=CARTESIAN_POINT('Ctrl Pts',(-21.2687069780221,-18.5930285031284,
-9.78457555532836));
#62237=CARTESIAN_POINT('Ctrl Pts',(-21.2612660069352,-18.5404876147807,
-9.78722940837572));
#62238=CARTESIAN_POINT('Ctrl Pts',(-21.2521952261608,-18.4882062515499,
-9.78988326142308));
#62239=CARTESIAN_POINT('Ctrl Pts',(-21.2415125421986,-18.4362666864387,
-9.79253711447044));
#62240=CARTESIAN_POINT('Ctrl Pts',(-21.2246679295087,-18.3543676186888,
-9.79672174886349));
#62241=CARTESIAN_POINT('Ctrl Pts',(-21.2037753333229,-18.2731422629634,
-9.80090638325654));
#62242=CARTESIAN_POINT('Ctrl Pts',(-21.1789030820534,-18.1930211337819,
-9.80509101764958));
#62243=CARTESIAN_POINT('Ctrl Pts',(-21.1540662333551,-18.1130140471107,
-9.80926969573353));
#62244=CARTESIAN_POINT('Ctrl Pts',(-21.125261116367,-18.0341085006255,-9.81344837381748));
#62245=CARTESIAN_POINT('Ctrl Pts',(-21.0926070466711,-17.9567247619913,
-9.81762705190143));
#62246=CARTESIAN_POINT('Ctrl Pts',(-21.059367676244,-17.8779539754568,-9.82188062978687));
#62247=CARTESIAN_POINT('Ctrl Pts',(-21.022140108072,-17.8007605624569,-9.8261342076723));
#62248=CARTESIAN_POINT('Ctrl Pts',(-20.9811033321017,-17.7255716022296,
-9.83038778555774));
#62249=CARTESIAN_POINT('Ctrl Pts',(-20.9408621341102,-17.6518403267155,
-9.83455889953569));
#62250=CARTESIAN_POINT('Ctrl Pts',(-20.8969583386824,-17.5800368994828,
-9.83873001351364));
#62251=CARTESIAN_POINT('Ctrl Pts',(-20.8496085018329,-17.5105421730164,
-9.84290112749159));
#62252=CARTESIAN_POINT('Ctrl Pts',(-20.8022745536785,-17.4410707661766,
-9.84707084181197));
#62253=CARTESIAN_POINT('Ctrl Pts',(-20.7514971194517,-17.3739069013821,
-9.85124055613235));
#62254=CARTESIAN_POINT('Ctrl Pts',(-20.69753660511,-17.3094032751789,-9.85541027045272));
#62255=CARTESIAN_POINT('Ctrl Pts',(-20.643578010915,-17.2449019442916,-9.85957983639677));
#62256=CARTESIAN_POINT('Ctrl Pts',(-20.5864368576392,-17.1830610160831,
-9.86374940234081));
#62257=CARTESIAN_POINT('Ctrl Pts',(-20.5264135623406,-17.1241997862082,
-9.86791896828485));
#62258=CARTESIAN_POINT('Ctrl Pts',(-20.4642799220261,-17.063269068104,-9.87223513102377));
#62259=CARTESIAN_POINT('Ctrl Pts',(-20.3990580731256,-17.0055318485508,
-9.87655129376269));
#62260=CARTESIAN_POINT('Ctrl Pts',(-20.3311209857106,-16.9512989836053,
-9.88086745650161));
#62261=CARTESIAN_POINT('Ctrl Pts',(-20.2653969417724,-16.8988327485311,
-9.88504302069329));
#62262=CARTESIAN_POINT('Ctrl Pts',(-20.1971322502977,-16.84964630251,-9.88921858488496));
#62263=CARTESIAN_POINT('Ctrl Pts',(-20.1266949702185,-16.8039774861682,
-9.89339414907664));
#62264=CARTESIAN_POINT('Ctrl Pts',(-20.0527000705712,-16.7560020464804,
-9.89778061108918));
#62265=CARTESIAN_POINT('Ctrl Pts',(-19.9763078452048,-16.7119092180967,
-9.90216707310172));
#62266=CARTESIAN_POINT('Ctrl Pts',(-19.8979731420051,-16.6719196231951,
-9.90655353511426));
#62267=CARTESIAN_POINT('Ctrl Pts',(-19.8196384388055,-16.6319300282936,
-9.9109399971268));
#62268=CARTESIAN_POINT('Ctrl Pts',(-19.7393618185146,-16.5960438342244,
-9.91532645913934));
#62269=CARTESIAN_POINT('Ctrl Pts',(-19.6576188802165,-16.5644221134992,
-9.91971292115188));
#62270=CARTESIAN_POINT('Ctrl Pts',(-19.5796370556816,-16.5342553550192,
-9.92389755554493));
#62271=CARTESIAN_POINT('Ctrl Pts',(-19.5000306196518,-16.5078569775931,
-9.92808218993798));
#62272=CARTESIAN_POINT('Ctrl Pts',(-19.4191985515812,-16.4854025571831,
-9.93226682433103));
#62273=CARTESIAN_POINT('Ctrl Pts',(-19.3384815379545,-16.4629800978612,
-9.93644550241497));
#62274=CARTESIAN_POINT('Ctrl Pts',(-19.2565427969406,-16.4444905669892,
-9.94062418049891));
#62275=CARTESIAN_POINT('Ctrl Pts',(-19.1738002903985,-16.4300611219609,
-9.94480285858285));
#62276=CARTESIAN_POINT('Ctrl Pts',(-19.0895746838926,-16.4153730395006,
-9.94905643646829));
#62277=CARTESIAN_POINT('Ctrl Pts',(-19.0045166631073,-16.404892202575,-9.95331001435372));
#62278=CARTESIAN_POINT('Ctrl Pts',(-18.9190822179583,-16.3986992788558,
-9.95756359223916));
#62279=CARTESIAN_POINT('Ctrl Pts',(-18.8353040862402,-16.3926264170474,
-9.96173470621711));
#62280=CARTESIAN_POINT('Ctrl Pts',(-18.7511644753125,-16.3906767277746,
-9.96590582019506));
#62281=CARTESIAN_POINT('Ctrl Pts',(-18.6671008395072,-16.3928742699263,
-9.97007693417301));
#62282=CARTESIAN_POINT('Ctrl Pts',(-18.5830654120667,-16.3950710746715,
-9.97424664849338));
#62283=CARTESIAN_POINT('Ctrl Pts',(-18.4991063686099,-16.4014123350032,
-9.97841636281376));
#62284=CARTESIAN_POINT('Ctrl Pts',(-18.4156612239222,-16.4118699986723,
-9.98258607713413));
#62285=CARTESIAN_POINT('Ctrl Pts',(-18.3322190485708,-16.4223272902128,
-9.98675564307817));
#62286=CARTESIAN_POINT('Ctrl Pts',(-18.249291191986,-16.4369006358009,-9.99092520902222));
#62287=CARTESIAN_POINT('Ctrl Pts',(-18.1673087413395,-16.4555102609148,
-9.99509477496626));
#62288=CARTESIAN_POINT('Ctrl Pts',(-18.0824438888645,-16.4747741774902,
-9.99941093770518));
#62289=CARTESIAN_POINT('Ctrl Pts',(-17.9985926745536,-16.498363368963,-10.0037271004441));
#62290=CARTESIAN_POINT('Ctrl Pts',(-17.9162183607824,-16.5261324870145,
-10.008043263183));
#62291=CARTESIAN_POINT('Ctrl Pts',(-17.836527381618,-16.5529970289662,-10.0122188273747));
#62292=CARTESIAN_POINT('Ctrl Pts',(-17.7582189816851,-16.5837731410384,
-10.0163943915664));
#62293=CARTESIAN_POINT('Ctrl Pts',(-17.6816923706303,-16.6182800825355,
-10.0205699557581));
#62294=CARTESIAN_POINT('Ctrl Pts',(-17.6013005823759,-16.6545298876153,
-10.0249564177706));
#62295=CARTESIAN_POINT('Ctrl Pts',(-17.5228758288488,-16.6948970480992,
-10.0293428797832));
#62296=CARTESIAN_POINT('Ctrl Pts',(-17.4468498189204,-16.7391185274971,
-10.0337293417957));
#62297=CARTESIAN_POINT('Ctrl Pts',(-17.3708238089919,-16.7833400068949,
-10.0381158038082));
#62298=CARTESIAN_POINT('Ctrl Pts',(-17.2971969868961,-16.8314154242948,
-10.0425022658208));
#62299=CARTESIAN_POINT('Ctrl Pts',(-17.2263622218887,-16.8830320616279,
-10.0468887278333));
#62300=CARTESIAN_POINT('Ctrl Pts',(-17.2089081327501,-16.8957506947588,
-10.0479695770316));
#62301=CARTESIAN_POINT('Ctrl Pts',(-17.1916066348401,-16.9086963056497,
-10.0490504262299));
#62302=CARTESIAN_POINT('Ctrl Pts',(-17.1744641548914,-16.9218650419685,
-10.0501312754282));
#62303=CARTESIAN_POINT('Ctrl Pts',(-17.1744641548915,-16.9218650419685,
-9.25004024527531));
#62304=CARTESIAN_POINT('Ctrl Pts',(-17.1077983713942,-16.9730772427116,
-9.25421688536645));
#62305=CARTESIAN_POINT('Ctrl Pts',(-17.0437156465026,-17.0275321795368,
-9.25839352545759));
#62306=CARTESIAN_POINT('Ctrl Pts',(-16.9825323038481,-17.0849271815657,
-9.26257016554873));
#62307=CARTESIAN_POINT('Ctrl Pts',(-16.9212437929918,-17.1424208400081,
-9.26675398487704));
#62308=CARTESIAN_POINT('Ctrl Pts',(-16.8628649371421,-17.2028643252882,
-9.27093780420536));
#62309=CARTESIAN_POINT('Ctrl Pts',(-16.8076737517062,-17.2659195792803,
-9.27512162353367));
#62310=CARTESIAN_POINT('Ctrl Pts',(-16.7693642429451,-17.3096877242506,
-9.27802571160402));
#62311=CARTESIAN_POINT('Ctrl Pts',(-16.7325897413083,-17.3547135268183,
-9.28092979967436));
#62312=CARTESIAN_POINT('Ctrl Pts',(-16.6974308899392,-17.4008758076974,
-9.28383388774471));
#62313=CARTESIAN_POINT('Ctrl Pts',(-16.6467688800086,-17.4673931665203,
-9.28801852213775));
#62314=CARTESIAN_POINT('Ctrl Pts',(-16.5992748500801,-17.5365189656784,
-9.2922031565308));
#62315=CARTESIAN_POINT('Ctrl Pts',(-16.5552283987657,-17.6079187860643,
-9.29638779092385));
#62316=CARTESIAN_POINT('Ctrl Pts',(-16.5112446421229,-17.6792169776433,
-9.3005664690078));
#62317=CARTESIAN_POINT('Ctrl Pts',(-16.4706989563139,-17.7527823729939,
-9.30474514709174));
#62318=CARTESIAN_POINT('Ctrl Pts',(-16.4338297096935,-17.8282488551323,
-9.30892382517568));
#62319=CARTESIAN_POINT('Ctrl Pts',(-16.3962996083249,-17.9050680197263,
-9.31317740306112));
#62320=CARTESIAN_POINT('Ctrl Pts',(-16.3625793350038,-17.9838567118701,
-9.31743098094656));
#62321=CARTESIAN_POINT('Ctrl Pts',(-16.3328731767861,-18.0641993586154,
-9.32168455883199));
#62322=CARTESIAN_POINT('Ctrl Pts',(-16.3037429304123,-18.1429844063778,
-9.32585567280994));
#62323=CARTESIAN_POINT('Ctrl Pts',(-16.2784727120491,-18.223263242189,-9.33002678678789));
#62324=CARTESIAN_POINT('Ctrl Pts',(-16.2572072783656,-18.3046223559168,
-9.33419790076585));
#62325=CARTESIAN_POINT('Ctrl Pts',(-16.2359489805037,-18.3859541688082,
-9.33836761508622));
#62326=CARTESIAN_POINT('Ctrl Pts',(-16.2186929146628,-18.4683650949799,
-9.34253732940659));
#62327=CARTESIAN_POINT('Ctrl Pts',(-16.2055337985359,-18.5514270752364,
-9.34670704372697));
#62328=CARTESIAN_POINT('Ctrl Pts',(-16.1923751506668,-18.6344860997912,
-9.35087660967101));
#62329=CARTESIAN_POINT('Ctrl Pts',(-16.183313233791,-18.7181956778687,-9.35504617561505));
#62330=CARTESIAN_POINT('Ctrl Pts',(-16.1783912959603,-18.8021195415123,
-9.3592157415591));
#62331=CARTESIAN_POINT('Ctrl Pts',(-16.1732963088673,-18.8889940646704,
-9.36353190429802));
#62332=CARTESIAN_POINT('Ctrl Pts',(-16.1726378716504,-18.9760976958013,
-9.36784806703694));
#62333=CARTESIAN_POINT('Ctrl Pts',(-16.1764051921424,-19.0629450261169,
-9.37216422977586));
#62334=CARTESIAN_POINT('Ctrl Pts',(-16.1800497925657,-19.1469633137821,
-9.37633979396754));
#62335=CARTESIAN_POINT('Ctrl Pts',(-16.1878361499306,-19.2307412775514,
-9.38051535815922));
#62336=CARTESIAN_POINT('Ctrl Pts',(-16.1997016639331,-19.3138451931539,
-9.3846909223509));
#62337=CARTESIAN_POINT('Ctrl Pts',(-16.2121664768403,-19.4011464899727,
-9.38907738436344));
#62338=CARTESIAN_POINT('Ctrl Pts',(-16.2291332400404,-19.487703283801,-9.39346384637598));
#62339=CARTESIAN_POINT('Ctrl Pts',(-16.2504693406595,-19.5730277482654,
-9.39785030838852));
#62340=CARTESIAN_POINT('Ctrl Pts',(-16.2718054412786,-19.6583522127299,
-9.40223677040106));
#62341=CARTESIAN_POINT('Ctrl Pts',(-16.2975106369606,-19.7424438151944,
-9.4066232324136));
#62342=CARTESIAN_POINT('Ctrl Pts',(-16.3273937923111,-19.8248382216157,
-9.41100969442614));
#62343=CARTESIAN_POINT('Ctrl Pts',(-16.3559019793865,-19.9034415392598,
-9.41519432881919));
#62344=CARTESIAN_POINT('Ctrl Pts',(-16.3883182194788,-19.9807929863463,
-9.41937896321224));
#62345=CARTESIAN_POINT('Ctrl Pts',(-16.4245126604672,-20.0564764499698,
-9.42356359760528));
#62346=CARTESIAN_POINT('Ctrl Pts',(-16.460655583149,-20.1320521875506,-9.42774227568923));
#62347=CARTESIAN_POINT('Ctrl Pts',(-16.5005658279439,-20.2059642460473,
-9.43192095377317));
#62348=CARTESIAN_POINT('Ctrl Pts',(-16.5440645726776,-20.2778140232167,
-9.43609963185712));
#62349=CARTESIAN_POINT('Ctrl Pts',(-16.5883430011486,-20.3509516560044,
-9.44035320974255));
#62350=CARTESIAN_POINT('Ctrl Pts',(-16.6363396782675,-20.4219518942302,
-9.44460678762799));
#62351=CARTESIAN_POINT('Ctrl Pts',(-16.6878157496594,-20.4904180230543,
-9.44886036551343));
#62352=CARTESIAN_POINT('Ctrl Pts',(-16.7382938569602,-20.5575568023704,
-9.45303147949138));
#62353=CARTESIAN_POINT('Ctrl Pts',(-16.7921173635638,-20.6222584681312,
-9.45720259346933));
#62354=CARTESIAN_POINT('Ctrl Pts',(-16.8490169269279,-20.6841774776944,
-9.46137370744728));
#62355=CARTESIAN_POINT('Ctrl Pts',(-16.905897397094,-20.746075709736,-9.46554342176766));
#62356=CARTESIAN_POINT('Ctrl Pts',(-16.9658515630401,-20.8051928015664,
-9.46971313608803));
#62357=CARTESIAN_POINT('Ctrl Pts',(-17.0285707636154,-20.8612174102717,
-9.4738828504084));
#62358=CARTESIAN_POINT('Ctrl Pts',(-17.0912877323723,-20.9172400253809,
-9.47805241635245));
#62359=CARTESIAN_POINT('Ctrl Pts',(-17.1567691964755,-20.9701700703297,
-9.48222198229649));
#62360=CARTESIAN_POINT('Ctrl Pts',(-17.2246717329647,-21.0197350367801,
-9.48639154824053));
#62361=CARTESIAN_POINT('Ctrl Pts',(-17.2949616388699,-21.071042646306,-9.49070771097946));
#62362=CARTESIAN_POINT('Ctrl Pts',(-17.3678456086252,-21.1187438312856,
-9.49502387371838));
#62363=CARTESIAN_POINT('Ctrl Pts',(-17.4429096486621,-21.1625849236531,
-9.4993400364573));
#62364=CARTESIAN_POINT('Ctrl Pts',(-17.5155284854901,-21.2049978970479,
-9.50351560064898));
#62365=CARTESIAN_POINT('Ctrl Pts',(-17.5901871024315,-21.2437982255354,
-9.50769116484066));
#62366=CARTESIAN_POINT('Ctrl Pts',(-17.6664869216557,-21.2788037793428,
-9.51186672903234));
#62367=CARTESIAN_POINT('Ctrl Pts',(-17.7466404633634,-21.3155773804553,
-9.51625319104488));
#62368=CARTESIAN_POINT('Ctrl Pts',(-17.8286048161834,-21.3481625684723,
-9.52063965305742));
#62369=CARTESIAN_POINT('Ctrl Pts',(-17.9118980145027,-21.3764067986709,
-9.52502611506996));
#62370=CARTESIAN_POINT('Ctrl Pts',(-17.9951912128221,-21.4046510288695,
-9.5294125770825));
#62371=CARTESIAN_POINT('Ctrl Pts',(-18.0798126775953,-21.428554216727,-9.53379903909504));
#62372=CARTESIAN_POINT('Ctrl Pts',(-18.1652685194105,-21.4480257416514,
-9.53818550110758));
#62373=CARTESIAN_POINT('Ctrl Pts',(-18.2467924112678,-21.4666013528503,
-9.54237013550063));
#62374=CARTESIAN_POINT('Ctrl Pts',(-18.3293790330749,-21.4812132961356,
-9.54655476989367));
#62375=CARTESIAN_POINT('Ctrl Pts',(-18.4126082132397,-21.4917455225678,
-9.55073940428672));
#62376=CARTESIAN_POINT('Ctrl Pts',(-18.4957189269682,-21.5022627576792,
-9.55491808237066));
#62377=CARTESIAN_POINT('Ctrl Pts',(-18.5794699298769,-21.508711753151,-9.5590967604546));
#62378=CARTESIAN_POINT('Ctrl Pts',(-18.663429267508,-21.5110271142986,-9.56327543853855));
#62379=CARTESIAN_POINT('Ctrl Pts',(-18.7488935159256,-21.5133839766308,
-9.56752901642398));
#62380=CARTESIAN_POINT('Ctrl Pts',(-18.8345731712377,-21.5114574491383,
-9.57178259430942));
#62381=CARTESIAN_POINT('Ctrl Pts',(-18.9200053717025,-21.5052336363321,
-9.57603617219485));
#62382=CARTESIAN_POINT('Ctrl Pts',(-19.0037813022541,-21.499130484282,-9.58020728617281));
#62383=CARTESIAN_POINT('Ctrl Pts',(-19.0873188071793,-21.4888952174951,
-9.58437840015076));
#62384=CARTESIAN_POINT('Ctrl Pts',(-19.1701815497897,-21.4745672747467,
-9.58854951412871));
#62385=CARTESIAN_POINT('Ctrl Pts',(-19.2530164870065,-21.4602441398779,
-9.59271922844908));
#62386=CARTESIAN_POINT('Ctrl Pts',(-19.3351766586593,-21.4418311348332,
-9.59688894276946));
#62387=CARTESIAN_POINT('Ctrl Pts',(-19.4162332022015,-21.4194192707795,
-9.60105865708983));
#62388=CARTESIAN_POINT('Ctrl Pts',(-19.497286861404,-21.3970082042361,-9.60522822303387));
#62389=CARTESIAN_POINT('Ctrl Pts',(-19.5772365274095,-21.3705986850247,
-9.60939778897791));
#62390=CARTESIAN_POINT('Ctrl Pts',(-19.6556671754964,-21.3403319739124,
-9.61356735492195));
#62391=CARTESIAN_POINT('Ctrl Pts',(-19.7368553484154,-21.3090011225755,
-9.61788351766088));
#62392=CARTESIAN_POINT('Ctrl Pts',(-19.8164152065818,-21.2735369848544,
-9.6221996803998));
#62393=CARTESIAN_POINT('Ctrl Pts',(-19.8939093684295,-21.2341503581117,
-9.62651584313872));
#62394=CARTESIAN_POINT('Ctrl Pts',(-19.9688791661059,-21.1960467465925,
-9.63069140733039));
#62395=CARTESIAN_POINT('Ctrl Pts',(-20.0419153954164,-21.1542725466308,
-9.63486697152208));
#62396=CARTESIAN_POINT('Ctrl Pts',(-20.112649171425,-21.1090643157146,-9.63904253571376));
#62397=CARTESIAN_POINT('Ctrl Pts',(-20.1869555423062,-21.0615727245271,
-9.6434289977263));
#62398=CARTESIAN_POINT('Ctrl Pts',(-20.2587202783153,-21.0102914191921,
-9.64781545973884));
#62399=CARTESIAN_POINT('Ctrl Pts',(-20.3275542346358,-20.9555430869523,
-9.65220192175138));
#62400=CARTESIAN_POINT('Ctrl Pts',(-20.3963881909563,-20.9007947547124,
-9.65658838376392));
#62401=CARTESIAN_POINT('Ctrl Pts',(-20.4622909830917,-20.8425798367028,
-9.66097484577646));
#62402=CARTESIAN_POINT('Ctrl Pts',(-20.5249190804939,-20.7812645645513,
-9.665361307789));
#62403=CARTESIAN_POINT('Ctrl Pts',(-20.5852113014986,-20.722236203594,-9.66958416538901));
#62404=CARTESIAN_POINT('Ctrl Pts',(-20.6427127908697,-20.6600954577448,
-9.67380702298902));
#62405=CARTESIAN_POINT('Ctrl Pts',(-20.6970796830689,-20.5951427685755,
-9.67802988058904));
#62406=CARTESIAN_POINT('Ctrl Pts',(-20.7500936846377,-20.5318063918539,
-9.68214765466763));
#62407=CARTESIAN_POINT('Ctrl Pts',(-20.8001269202378,-20.465796754398,-9.68626542874623));
#62408=CARTESIAN_POINT('Ctrl Pts',(-20.8468954124061,-20.3974317611819,
-9.69038320282483));
#62409=CARTESIAN_POINT('Ctrl Pts',(-20.89361966769,-20.3291314323191,-9.69449708202704));
#62410=CARTESIAN_POINT('Ctrl Pts',(-20.9370850392269,-20.2584805564847,
-9.69861096122924));
#62411=CARTESIAN_POINT('Ctrl Pts',(-20.9770478427321,-20.1858299620349,
-9.70272484043145));
#62412=CARTESIAN_POINT('Ctrl Pts',(-21.0169856434319,-20.1132248215702,
-9.70683614577717));
#62413=CARTESIAN_POINT('Ctrl Pts',(-21.0534249974543,-20.038622860247,-9.71094745112288));
#62414=CARTESIAN_POINT('Ctrl Pts',(-21.0861664418207,-19.9624024099201,
-9.7150587564686));
#62415=CARTESIAN_POINT('Ctrl Pts',(-21.1204445396302,-19.88260470698,-9.71936301761199));
#62416=CARTESIAN_POINT('Ctrl Pts',(-21.1506688210158,-19.8010333411259,
-9.72366727875538));
#62417=CARTESIAN_POINT('Ctrl Pts',(-21.1766659614561,-19.7181481584811,
-9.72797153989877));
#62418=CARTESIAN_POINT('Ctrl Pts',(-21.2014998963995,-19.6389715567968,
-9.73208321292912));
#62419=CARTESIAN_POINT('Ctrl Pts',(-21.222476755318,-19.5585966865054,-9.73619488595946));
#62420=CARTESIAN_POINT('Ctrl Pts',(-21.2394965458156,-19.4774398718274,
-9.74030655898981));
#62421=CARTESIAN_POINT('Ctrl Pts',(-21.2565208804896,-19.3962613887936,
-9.74441932981082));
#62422=CARTESIAN_POINT('Ctrl Pts',(-21.2695859645564,-19.3143010135805,
-9.74853210063183));
#62423=CARTESIAN_POINT('Ctrl Pts',(-21.2786432445868,-19.2319834955467,
-9.75264487145285));
#62424=CARTESIAN_POINT('Ctrl Pts',(-21.2877094512626,-19.1495848472747,
-9.75676169572548));
#62425=CARTESIAN_POINT('Ctrl Pts',(-21.2927599450141,-19.066828826857,-9.76087851999811));
#62426=CARTESIAN_POINT('Ctrl Pts',(-21.2937982075177,-18.9841424452888,
-9.76499534427074));
#62427=CARTESIAN_POINT('Ctrl Pts',(-21.2939423435977,-18.9726635650768,
-9.76556685957692));
#62428=CARTESIAN_POINT('Ctrl Pts',(-21.2940092371596,-18.9611860219109,
-9.76613837488311));
#62429=CARTESIAN_POINT('Ctrl Pts',(-21.2939989766127,-18.9497109517324,
-9.7667098901893));
#62430=CARTESIAN_POINT('Origin',(-18.734,-18.952,1.76670989022851));
#62431=CARTESIAN_POINT('',(-17.1744641548914,-16.9218650419685,-8.45013430174985));
#62432=CARTESIAN_POINT('',(-17.1744641548914,-16.9218650419685,-8.51667714937936));
#62433=CARTESIAN_POINT('',(-17.1744641548914,-16.9218650419685,1.76670989022851));
#62434=CARTESIAN_POINT('',(-21.294330140624,-18.9526425111494,-9.03329016589256));
#62435=CARTESIAN_POINT('Ctrl Pts',(-17.1744641548914,-16.9218650419685,
-8.51667714937936));
#62436=CARTESIAN_POINT('Ctrl Pts',(-17.160259116072,-16.9327772560222,-8.51757293017557));
#62437=CARTESIAN_POINT('Ctrl Pts',(-17.1461740119804,-16.9438344208981,
-8.51846871097177));
#62438=CARTESIAN_POINT('Ctrl Pts',(-17.1322119090441,-16.9550335727229,
-8.51936449176797));
#62439=CARTESIAN_POINT('Ctrl Pts',(-17.0669880324056,-17.0073503405056,
-8.52354912616102));
#62440=CARTESIAN_POINT('Ctrl Pts',(-17.0042085866859,-17.0629632902854,
-8.52773376055407));
#62441=CARTESIAN_POINT('Ctrl Pts',(-16.9442256444346,-17.1216154075822,
-8.53191839494711));
#62442=CARTESIAN_POINT('Ctrl Pts',(-16.8843280804771,-17.1801840408498,
-8.53609707303105));
#62443=CARTESIAN_POINT('Ctrl Pts',(-16.8272194396166,-17.2417829302055,
-8.540275751115));
#62444=CARTESIAN_POINT('Ctrl Pts',(-16.7732194376016,-17.3061143459764,
-8.54445442919894));
#62445=CARTESIAN_POINT('Ctrl Pts',(-16.7182515243597,-17.3715988561408,
-8.54870800708437));
#62446=CARTESIAN_POINT('Ctrl Pts',(-16.6665051669308,-17.4399145156591,
-8.55296158496981));
#62447=CARTESIAN_POINT('Ctrl Pts',(-16.6182789494494,-17.5107073731345,
-8.55721516285525));
#62448=CARTESIAN_POINT('Ctrl Pts',(-16.5709876912995,-17.5801277729268,
-8.5613862768332));
#62449=CARTESIAN_POINT('Ctrl Pts',(-16.5270815724709,-17.6519297794777,
-8.56555739081115));
#62450=CARTESIAN_POINT('Ctrl Pts',(-16.4868009099953,-17.7257470693687,
-8.5697285047891));
#62451=CARTESIAN_POINT('Ctrl Pts',(-16.446533764085,-17.7995395891551,-8.57389821910947));
#62452=CARTESIAN_POINT('Ctrl Pts',(-16.409889878601,-17.8753456457563,-8.57806793342985));
#62453=CARTESIAN_POINT('Ctrl Pts',(-16.3770645250475,-17.952772715089,-8.58223764775022));
#62454=CARTESIAN_POINT('Ctrl Pts',(-16.344240339561,-18.0301970292344,-8.58640721369426));
#62455=CARTESIAN_POINT('Ctrl Pts',(-16.315234594618,-18.1092418175489,-8.59057677963831));
#62456=CARTESIAN_POINT('Ctrl Pts',(-16.2901945969736,-18.1894941625542,
-8.59474634558235));
#62457=CARTESIAN_POINT('Ctrl Pts',(-16.2642742239021,-18.2725680810079,
-8.59906250832127));
#62458=CARTESIAN_POINT('Ctrl Pts',(-16.2426038152403,-18.3569355479853,
-8.60337867106019));
#62459=CARTESIAN_POINT('Ctrl Pts',(-16.2252901016539,-18.4421229109477,
-8.60769483379911));
#62460=CARTESIAN_POINT('Ctrl Pts',(-16.2085403804665,-18.5245353045217,
-8.61187039799079));
#62461=CARTESIAN_POINT('Ctrl Pts',(-16.1958678987932,-18.6077145253799,
-8.61604596218247));
#62462=CARTESIAN_POINT('Ctrl Pts',(-16.1873166326445,-18.6912245670412,
-8.62022152637415));
#62463=CARTESIAN_POINT('Ctrl Pts',(-16.1783334623714,-18.7789525023805,
-8.62460798838669));
#62464=CARTESIAN_POINT('Ctrl Pts',(-16.1738988033979,-18.8670449731774,
-8.62899445039923));
#62465=CARTESIAN_POINT('Ctrl Pts',(-16.1740017537922,-18.9549965668354,
-8.63338091241177));
#62466=CARTESIAN_POINT('Ctrl Pts',(-16.1741047041864,-19.0429481604934,
-8.63776737442431));
#62467=CARTESIAN_POINT('Ctrl Pts',(-16.1787451573697,-19.1307583016182,
-8.64215383643685));
#62468=CARTESIAN_POINT('Ctrl Pts',(-16.1878497481281,-19.2179302444114,
-8.64654029844939));
#62469=CARTESIAN_POINT('Ctrl Pts',(-16.1965354231695,-19.3010912768969,
-8.65072493284244));
#62470=CARTESIAN_POINT('Ctrl Pts',(-16.2093157897326,-19.3839810906174,
-8.65490956723549));
#62471=CARTESIAN_POINT('Ctrl Pts',(-16.2261653095063,-19.4661645312117,
-8.65909420162853));
#62472=CARTESIAN_POINT('Ctrl Pts',(-16.2429908460741,-19.5482309938506,
-8.66327287971248));
#62473=CARTESIAN_POINT('Ctrl Pts',(-16.2638739396399,-19.629592633669,-8.66745155779642));
#62474=CARTESIAN_POINT('Ctrl Pts',(-16.2887373027363,-19.7098194648929,
-8.67163023588037));
#62475=CARTESIAN_POINT('Ctrl Pts',(-16.3140463237472,-19.7914843044086,
-8.6758838137658));
#62476=CARTESIAN_POINT('Ctrl Pts',(-16.3434796603857,-19.871972772756,-8.68013739165124));
#62477=CARTESIAN_POINT('Ctrl Pts',(-16.3769013134697,-19.9508422207522,
-8.68439096953667));
#62478=CARTESIAN_POINT('Ctrl Pts',(-16.4096750225917,-20.0281826305979,
-8.68856208351462));
#62479=CARTESIAN_POINT('Ctrl Pts',(-16.4462835978106,-20.103965792552,-8.69273319749258));
#62480=CARTESIAN_POINT('Ctrl Pts',(-16.4865490981546,-20.1777913541033,
-8.69690431147053));
#62481=CARTESIAN_POINT('Ctrl Pts',(-16.5268010870211,-20.2515921427744,
-8.7010740257909));
#62482=CARTESIAN_POINT('Ctrl Pts',(-16.5707073438479,-20.3234362321085,
-8.70524374011128));
#62483=CARTESIAN_POINT('Ctrl Pts',(-16.618043514761,-20.3929469638315,-8.70941345443165));
#62484=CARTESIAN_POINT('Ctrl Pts',(-16.66537800125,-20.4624552220643,-8.71358302037569));
#62485=CARTESIAN_POINT('Ctrl Pts',(-16.7161418995133,-20.5296299080143,
-8.71775258631974));
#62486=CARTESIAN_POINT('Ctrl Pts',(-16.77006774565,-20.594123655613,-8.72192215226378));
#62487=CARTESIAN_POINT('Ctrl Pts',(-16.8258895580122,-20.6608849238157,
-8.7262383150027));
#62488=CARTESIAN_POINT('Ctrl Pts',(-16.8850994651022,-20.7247728178031,
-8.73055447774162));
#62489=CARTESIAN_POINT('Ctrl Pts',(-16.9473569713774,-20.7854412148401,
-8.73487064048054));
#62490=CARTESIAN_POINT('Ctrl Pts',(-17.0075864459339,-20.8441333452247,
-8.73904620467222));
#62491=CARTESIAN_POINT('Ctrl Pts',(-17.0706676333014,-20.8998122314802,
-8.7432217688639));
#62492=CARTESIAN_POINT('Ctrl Pts',(-17.1362577244092,-20.952204894702,-8.74739733305558));
#62493=CARTESIAN_POINT('Ctrl Pts',(-17.2051606150933,-21.0072437867915,
-8.75178379506812));
#62494=CARTESIAN_POINT('Ctrl Pts',(-17.2768320453054,-21.0586554168247,
-8.75617025708067));
#62495=CARTESIAN_POINT('Ctrl Pts',(-17.3508411420262,-21.1061753813486,
-8.76055671909321));
#62496=CARTESIAN_POINT('Ctrl Pts',(-17.4248502387469,-21.1536953458725,
-8.76494318110575));
#62497=CARTESIAN_POINT('Ctrl Pts',(-17.5011964604718,-21.1973234230529,
-8.76932964311829));
#62498=CARTESIAN_POINT('Ctrl Pts',(-17.5794224113972,-21.2368524223451,
-8.77371610513083));
#62499=CARTESIAN_POINT('Ctrl Pts',(-17.6540490703619,-21.2745626337838,
-8.77790073952388));
#62500=CARTESIAN_POINT('Ctrl Pts',(-17.7306640561251,-21.3086830520783,
-8.78208537391693));
#62501=CARTESIAN_POINT('Ctrl Pts',(-17.8088876493306,-21.3389996101045,
-8.78627000830998));
#62502=CARTESIAN_POINT('Ctrl Pts',(-17.8869999009332,-21.3692730162627,
-8.79044868639392));
#62503=CARTESIAN_POINT('Ctrl Pts',(-17.9667157867298,-21.3957531518832,
-8.79462736447786));
#62504=CARTESIAN_POINT('Ctrl Pts',(-18.047631922491,-21.4182722603509,-8.79880604256181));
#62505=CARTESIAN_POINT('Ctrl Pts',(-18.1299984218322,-21.4411950076538,
-8.80305962044724));
#62506=CARTESIAN_POINT('Ctrl Pts',(-18.2136081930111,-21.4600131107993,
-8.80731319833268));
#62507=CARTESIAN_POINT('Ctrl Pts',(-18.2980154243378,-21.4746013259698,
-8.81156677621812));
#62508=CARTESIAN_POINT('Ctrl Pts',(-18.3807862567781,-21.4889067201227,
-8.81573789019607));
#62509=CARTESIAN_POINT('Ctrl Pts',(-18.4643234304656,-21.4991446900207,
-8.81990900417402));
#62510=CARTESIAN_POINT('Ctrl Pts',(-18.5481939962224,-21.5052481526401,
-8.82408011815197));
#62511=CARTESIAN_POINT('Ctrl Pts',(-18.6320364184009,-21.5113495671838,
-8.82824983247235));
#62512=CARTESIAN_POINT('Ctrl Pts',(-18.7162115520295,-21.5133191964338,
-8.83241954679272));
#62513=CARTESIAN_POINT('Ctrl Pts',(-18.8002812486105,-21.5111418085137,
-8.83658926111309));
#62514=CARTESIAN_POINT('Ctrl Pts',(-18.884347953631,-21.5089644980744,-8.84075882705713));
#62515=CARTESIAN_POINT('Ctrl Pts',(-18.9683087692068,-21.502640476632,-8.84492839300118));
#62516=CARTESIAN_POINT('Ctrl Pts',(-19.0517268423098,-21.4922066163357,
-8.84909795894522));
#62517=CARTESIAN_POINT('Ctrl Pts',(-19.1380777919557,-21.481405914383,-8.85341412168414));
#62518=CARTESIAN_POINT('Ctrl Pts',(-19.2238466000238,-21.4662010579768,
-8.85773028442306));
#62519=CARTESIAN_POINT('Ctrl Pts',(-19.3085579282896,-21.4466910003124,
-8.86204644716198));
#62520=CARTESIAN_POINT('Ctrl Pts',(-19.3905097939473,-21.4278164807242,
-8.86622201135366));
#62521=CARTESIAN_POINT('Ctrl Pts',(-19.4714715762059,-21.404913110059,-8.87039757554534));
#62522=CARTESIAN_POINT('Ctrl Pts',(-19.551028186959,-21.3781213781908,-8.87457313973702));
#62523=CARTESIAN_POINT('Ctrl Pts',(-19.6346030129934,-21.3499764596372,
-8.87895960174956));
#62524=CARTESIAN_POINT('Ctrl Pts',(-19.716626443602,-21.3175402693169,-8.88334606376211));
#62525=CARTESIAN_POINT('Ctrl Pts',(-19.7966429339306,-21.2810319866776,
-8.88773252577465));
#62526=CARTESIAN_POINT('Ctrl Pts',(-19.8766594242592,-21.2445237040383,
-8.89211898778719));
#62527=CARTESIAN_POINT('Ctrl Pts',(-19.954668494674,-21.203943664325,-8.89650544979973));
#62528=CARTESIAN_POINT('Ctrl Pts',(-20.0302483510423,-21.159564316712,-8.90089191181227));
#62529=CARTESIAN_POINT('Ctrl Pts',(-20.102350666183,-21.1172269286686,-8.90507654620531));
#62530=CARTESIAN_POINT('Ctrl Pts',(-20.1725107769709,-21.071274585504,-8.90926118059836));
#62531=CARTESIAN_POINT('Ctrl Pts',(-20.2403431519459,-21.0219107006307,
-8.91344581499141));
#62532=CARTESIAN_POINT('Ctrl Pts',(-20.308078975931,-20.9726170791377,-8.91762449307535));
#62533=CARTESIAN_POINT('Ctrl Pts',(-20.3734932764658,-20.9199218296712,
-8.92180317115929));
#62534=CARTESIAN_POINT('Ctrl Pts',(-20.4362266525525,-20.8640733310571,
-8.92598184924322));
#62535=CARTESIAN_POINT('Ctrl Pts',(-20.50008447932,-20.807223788243,-8.93023542712866));
#62536=CARTESIAN_POINT('Ctrl Pts',(-20.5611639093904,-20.7471070845338,
-8.9344890050141));
#62537=CARTESIAN_POINT('Ctrl Pts',(-20.6191183231211,-20.6840302849064,
-8.93874258289954));
#62538=CARTESIAN_POINT('Ctrl Pts',(-20.675949177453,-20.6221763521241,-8.94291369687749));
#62539=CARTESIAN_POINT('Ctrl Pts',(-20.7297747776525,-20.5574764280246,
-8.94708481085544));
#62540=CARTESIAN_POINT('Ctrl Pts',(-20.7803043703346,-20.4902582435825,
-8.95125592483339));
#62541=CARTESIAN_POINT('Ctrl Pts',(-20.8308170073239,-20.4230626148514,
-8.95542563915376));
#62542=CARTESIAN_POINT('Ctrl Pts',(-20.8780355571481,-20.3533507714295,
-8.95959535347413));
#62543=CARTESIAN_POINT('Ctrl Pts',(-20.9217100507378,-20.2814828821391,
-8.9637650677945));
#62544=CARTESIAN_POINT('Ctrl Pts',(-20.9653829902015,-20.2096175502167,
-8.96793463373855));
#62545=CARTESIAN_POINT('Ctrl Pts',(-21.005511885995,-20.1355967185424,-8.97210419968259));
#62546=CARTESIAN_POINT('Ctrl Pts',(-21.0418912815017,-20.0598076695746,
-8.97627376562663));
#62547=CARTESIAN_POINT('Ctrl Pts',(-21.0795497316757,-19.9813539711409,
-8.98058992836555));
#62548=CARTESIAN_POINT('Ctrl Pts',(-21.113189882732,-19.901005876374,-8.98490609110447));
#62549=CARTESIAN_POINT('Ctrl Pts',(-21.1426376470827,-19.8192166309844,
-8.9892222538434));
#62550=CARTESIAN_POINT('Ctrl Pts',(-21.171126153607,-19.7400916616608,-8.99339781803508));
#62551=CARTESIAN_POINT('Ctrl Pts',(-21.1956911205895,-19.6596184551168,
-8.99757338222676));
#62552=CARTESIAN_POINT('Ctrl Pts',(-21.216225998462,-19.5782220792652,-9.00174894641843));
#62553=CARTESIAN_POINT('Ctrl Pts',(-21.2377980441989,-19.4927145659707,
-9.00613540843098));
#62554=CARTESIAN_POINT('Ctrl Pts',(-21.254922068569,-19.4061887466987,-9.01052187044353));
#62555=CARTESIAN_POINT('Ctrl Pts',(-21.2675357890124,-19.3191463002581,
-9.01490833245607));
#62556=CARTESIAN_POINT('Ctrl Pts',(-21.2801495094559,-19.2321038538175,
-9.01929479446862));
#62557=CARTESIAN_POINT('Ctrl Pts',(-21.288252948244,-19.1445453649661,-9.02368125648116));
#62558=CARTESIAN_POINT('Ctrl Pts',(-21.2918468828523,-19.0569729673898,
-9.02806771849371));
#62559=CARTESIAN_POINT('Ctrl Pts',(-21.2932731600888,-19.022219269613,-9.02980851558631));
#62560=CARTESIAN_POINT('Ctrl Pts',(-21.2939911726516,-18.9874363059255,
-9.03154931267891));
#62561=CARTESIAN_POINT('Ctrl Pts',(-21.2939999191096,-18.9526435515772,
-9.03329010977151));
#62562=CARTESIAN_POINT('Ctrl Pts',(-21.2980343851841,-18.9526308401995,
-9.03329079542781));
#62563=CARTESIAN_POINT('Ctrl Pts',(-21.295285921847,-18.1388728971705,-9.07394170534359));
#62564=CARTESIAN_POINT('Ctrl Pts',(-20.4360628655086,-16.4715240736058,
-9.15698455081984));
#62565=CARTESIAN_POINT('Ctrl Pts',(-18.2953377683469,-16.227376780493,-9.25149015685125));
#62566=CARTESIAN_POINT('Ctrl Pts',(-17.356575497914,-16.7803425229578,-9.30534485296688));
#62567=CARTESIAN_POINT('Ctrl Pts',(-17.1750494511459,-16.9226083978003,
-9.31680761352203));
#62568=CARTESIAN_POINT('',(-21.293999998394,-18.9519093211995,-8.96670989026365));
#62569=CARTESIAN_POINT('Ctrl Pts',(-21.293999998394,-18.9519093211995,-8.96670989026365));
#62570=CARTESIAN_POINT('Ctrl Pts',(-21.2939968622717,-18.8633718327361,
-8.97108917708312));
#62571=CARTESIAN_POINT('Ctrl Pts',(-21.2893963356695,-18.7749281972304,
-8.97546846390259));
#62572=CARTESIAN_POINT('Ctrl Pts',(-21.2802532223815,-18.6870575014991,
-8.97984775072206));
#62573=CARTESIAN_POINT('Ctrl Pts',(-21.2710840473103,-18.5989363367038,
-8.98423952038192));
#62574=CARTESIAN_POINT('Ctrl Pts',(-21.2573464424812,-18.5113917635122,
-8.98863129004178));
#62575=CARTESIAN_POINT('Ctrl Pts',(-21.2391468026208,-18.4248951742595,
-8.99302305970165));
#62576=CARTESIAN_POINT('Ctrl Pts',(-21.2209205771356,-18.3382722327336,
-8.99742124475991));
#62577=CARTESIAN_POINT('Ctrl Pts',(-21.1982194166656,-18.2527007028949,
-9.00181942981817));
#62578=CARTESIAN_POINT('Ctrl Pts',(-21.1711995861976,-18.1686366251616,
-9.00621761487642));
#62579=CARTESIAN_POINT('Ctrl Pts',(-21.1441046030878,-18.0843387325816,
-9.01062803299538));
#62580=CARTESIAN_POINT('Ctrl Pts',(-21.1126670698913,-18.0015570394273,
-9.01503845111433));
#62581=CARTESIAN_POINT('Ctrl Pts',(-21.0770917883152,-17.9207285170577,
-9.01944886923329));
#62582=CARTESIAN_POINT('Ctrl Pts',(-21.0501146625114,-17.859435362938,-9.02279333761614));
#62583=CARTESIAN_POINT('Ctrl Pts',(-21.0207591774504,-17.7992649146786,
-9.02613780599899));
#62584=CARTESIAN_POINT('Ctrl Pts',(-20.9891316170539,-17.7403971815138,
-9.02948227438184));
#62585=CARTESIAN_POINT('Ctrl Pts',(-20.949558877278,-17.6667412480012,-9.03366690877489));
#62586=CARTESIAN_POINT('Ctrl Pts',(-20.9063001320241,-17.5948890389388,
-9.03785154316794));
#62587=CARTESIAN_POINT('Ctrl Pts',(-20.8595440286336,-17.5252335221418,
-9.04203617756098));
#62588=CARTESIAN_POINT('Ctrl Pts',(-20.812854476769,-17.4556771513512,-9.04621485564493));
#62589=CARTESIAN_POINT('Ctrl Pts',(-20.7626777089518,-17.3883116408712,
-9.05039353372888));
#62590=CARTESIAN_POINT('Ctrl Pts',(-20.7092482964897,-17.3235055519854,
-9.05457221181283));
#62591=CARTESIAN_POINT('Ctrl Pts',(-20.6548612002084,-17.2575378605317,
-9.05882578969826));
#62592=CARTESIAN_POINT('Ctrl Pts',(-20.5971039332157,-17.1942226731584,
-9.06307936758369));
#62593=CARTESIAN_POINT('Ctrl Pts',(-20.5362701954422,-17.1339180044286,
-9.06733294546913));
#62594=CARTESIAN_POINT('Ctrl Pts',(-20.4766158383827,-17.0747824593771,
-9.07150405944708));
#62595=CARTESIAN_POINT('Ctrl Pts',(-20.4140035745828,-17.0185420838701,
-9.07567517342503));
#62596=CARTESIAN_POINT('Ctrl Pts',(-20.3487498736144,-16.9654998500724,
-9.07984628740299));
#62597=CARTESIAN_POINT('Ctrl Pts',(-20.2835180691556,-16.9124754151086,
-9.08401600172336));
#62598=CARTESIAN_POINT('Ctrl Pts',(-20.2156469445306,-16.8626472804563,
-9.08818571604373));
#62599=CARTESIAN_POINT('Ctrl Pts',(-20.1454869304126,-16.8162788933771,
-9.0923554303641));
#62600=CARTESIAN_POINT('Ctrl Pts',(-20.0753294128889,-16.7699121562841,
-9.09652499630815));
#62601=CARTESIAN_POINT('Ctrl Pts',(-20.0028835520724,-16.7270051749182,
-9.10069456225219));
#62602=CARTESIAN_POINT('Ctrl Pts',(-19.9285285607302,-16.687777944282,-9.10486412819624));
#62603=CARTESIAN_POINT('Ctrl Pts',(-19.8515593396191,-16.6471715326087,
-9.10918029093515));
#62604=CARTESIAN_POINT('Ctrl Pts',(-19.7725447065605,-16.6105086923156,
-9.11349645367407));
#62605=CARTESIAN_POINT('Ctrl Pts',(-19.6919309796755,-16.577980573336,-9.11781261641299));
#62606=CARTESIAN_POINT('Ctrl Pts',(-19.6139432364648,-16.5465120544109,
-9.12198818060467));
#62607=CARTESIAN_POINT('Ctrl Pts',(-19.5344594409715,-16.5189131263823,
-9.12616374479635));
#62608=CARTESIAN_POINT('Ctrl Pts',(-19.4539003149003,-16.4953063812094,
-9.13033930898803));
#62609=CARTESIAN_POINT('Ctrl Pts',(-19.3692723388824,-16.4705073154575,
-9.13472577100057));
#62610=CARTESIAN_POINT('Ctrl Pts',(-19.2834581156084,-16.4501144565313,
-9.13911223301311));
#62611=CARTESIAN_POINT('Ctrl Pts',(-19.1969566012277,-16.4342090663878,
-9.14349869502565));
#62612=CARTESIAN_POINT('Ctrl Pts',(-19.1104550868471,-16.4183036762444,
-9.14788515703819));
#62613=CARTESIAN_POINT('Ctrl Pts',(-19.0232668665414,-16.406885754803,-9.15227161905072));
#62614=CARTESIAN_POINT('Ctrl Pts',(-18.9358937423135,-16.3999735665917,
-9.15665808106326));
#62615=CARTESIAN_POINT('Ctrl Pts',(-18.8525619577046,-16.3933810933994,
-9.16084165250876));
#62616=CARTESIAN_POINT('Ctrl Pts',(-18.768751898504,-16.3908622168773,-9.16502522395427));
#62617=CARTESIAN_POINT('Ctrl Pts',(-18.6848957690259,-16.3924709858061,
-9.16920879539977));
#62618=CARTESIAN_POINT('Ctrl Pts',(-18.6011496144028,-16.3940776448816,
-9.17338688021399));
#62619=CARTESIAN_POINT('Ctrl Pts',(-18.517357964957,-16.3998011941734,-9.17756496502821));
#62620=CARTESIAN_POINT('Ctrl Pts',(-18.4339575045038,-16.4096439075345,
-9.18174304984243));
#62621=CARTESIAN_POINT('Ctrl Pts',(-18.3506413936532,-16.4194766661668,
-9.18591690902299));
#62622=CARTESIAN_POINT('Ctrl Pts',(-18.2677161403437,-16.4334202620682,
-9.19009076820354));
#62623=CARTESIAN_POINT('Ctrl Pts',(-18.185616418364,-16.4514249766519,-9.1942646273841));
#62624=CARTESIAN_POINT('Ctrl Pts',(-18.1035750976745,-16.4694168836581,
-9.19843551750757));
#62625=CARTESIAN_POINT('Ctrl Pts',(-18.0223585896044,-16.4914640715327,
-9.20260640763105));
#62626=CARTESIAN_POINT('Ctrl Pts',(-17.9423930915556,-16.517465444381,-9.20677729775453));
#62627=CARTESIAN_POINT('Ctrl Pts',(-17.8624446940949,-16.5434612568466,
-9.21094729593491));
#62628=CARTESIAN_POINT('Ctrl Pts',(-17.7837472149657,-16.5734094406324,
-9.21511729411528));
#62629=CARTESIAN_POINT('Ctrl Pts',(-17.7067122821122,-16.6071588657914,
-9.21928729229566));
#62630=CARTESIAN_POINT('Ctrl Pts',(-17.6296873849781,-16.6409038942468,
-9.22345674722987));
#62631=CARTESIAN_POINT('Ctrl Pts',(-17.5543250225282,-16.678448989543,-9.22762620216409));
#62632=CARTESIAN_POINT('Ctrl Pts',(-17.481015873204,-16.7195952925159,-9.2317956570983));
#62633=CARTESIAN_POINT('Ctrl Pts',(-17.4076680317964,-16.7607633122349,
-9.23596731264321));
#62634=CARTESIAN_POINT('Ctrl Pts',(-17.3363759656345,-16.805536104046,-9.24013896818811));
#62635=CARTESIAN_POINT('Ctrl Pts',(-17.267504027417,-16.8536698156873,-9.24431062373302));
#62636=CARTESIAN_POINT('Ctrl Pts',(-17.2359729692538,-16.8757064666173,
-9.24622049758045));
#62637=CARTESIAN_POINT('Ctrl Pts',(-17.2049487630074,-16.8984469736806,
-9.24813037142788));
#62638=CARTESIAN_POINT('Ctrl Pts',(-17.1744641548915,-16.9218650419685,
-9.25004024527531));
#62639=CARTESIAN_POINT('Ctrl Pts',(-17.1744641548914,-16.9218650419685,
-8.45013430174985));
#62640=CARTESIAN_POINT('Ctrl Pts',(-17.1077839597158,-16.9730883136647,
-8.45430378660374));
#62641=CARTESIAN_POINT('Ctrl Pts',(-17.0436166359205,-17.0276105362849,
-8.45847327145763));
#62642=CARTESIAN_POINT('Ctrl Pts',(-16.9822966765068,-17.0851482473258,
-8.46264275631152));
#62643=CARTESIAN_POINT('Ctrl Pts',(-16.9209698311314,-17.1426924195984,
-8.46681270938022));
#62644=CARTESIAN_POINT('Ctrl Pts',(-16.8624913196026,-17.2032524369424,
-8.47098266244893));
#62645=CARTESIAN_POINT('Ctrl Pts',(-16.8071595240486,-17.2665072589194,
-8.47515261551763));
#62646=CARTESIAN_POINT('Ctrl Pts',(-16.7517686221848,-17.3298296507098,
-8.47932702299695));
#62647=CARTESIAN_POINT('Ctrl Pts',(-16.6995314504634,-17.3958522471909,
-8.48350143047628));
#62648=CARTESIAN_POINT('Ctrl Pts',(-16.650706396123,-17.464220527079,-8.4876758379556));
#62649=CARTESIAN_POINT('Ctrl Pts',(-16.6018533425747,-17.5326280134299,
-8.49185263928996));
#62650=CARTESIAN_POINT('Ctrl Pts',(-16.5564165506132,-17.6033834741459,
-8.49602944062433));
#62651=CARTESIAN_POINT('Ctrl Pts',(-16.5146099894966,-17.6761050273326,
-8.50020624195869));
#62652=CARTESIAN_POINT('Ctrl Pts',(-16.4727322757655,-17.7489503488588,
-8.50439015199387));
#62653=CARTESIAN_POINT('Ctrl Pts',(-16.4344973396758,-17.8237680350171,
-8.50857406202906));
#62654=CARTESIAN_POINT('Ctrl Pts',(-16.4000721519639,-17.9001536233072,
-8.51275797206425));
#62655=CARTESIAN_POINT('Ctrl Pts',(-16.3780730306812,-17.9489671791,-8.5154316639282));
#62656=CARTESIAN_POINT('Ctrl Pts',(-16.3576287294878,-17.9984206275095,
-8.51810535579216));
#62657=CARTESIAN_POINT('Ctrl Pts',(-16.3387721302027,-18.0484052613331,
-8.52077904765611));
#62658=CARTESIAN_POINT('Ctrl Pts',(-16.3092593897976,-18.1266369456353,
-8.52496368204916));
#62659=CARTESIAN_POINT('Ctrl Pts',(-16.2835285016033,-18.2064616309202,
-8.5291483164422));
#62660=CARTESIAN_POINT('Ctrl Pts',(-16.2617516946765,-18.2874788815808,
-8.53333295083525));
#62661=CARTESIAN_POINT('Ctrl Pts',(-16.2400058843389,-18.3683808142131,
-8.5375116289192));
#62662=CARTESIAN_POINT('Ctrl Pts',(-16.2222030943944,-18.450471500049,-8.54169030700315));
#62663=CARTESIAN_POINT('Ctrl Pts',(-16.2084669780843,-18.5333319271626,
-8.5458689850871));
#62664=CARTESIAN_POINT('Ctrl Pts',(-16.1944846517613,-18.6176775678812,
-8.55012256297253));
#62665=CARTESIAN_POINT('Ctrl Pts',(-16.1847163934876,-18.7028203654208,
-8.55437614085797));
#62666=CARTESIAN_POINT('Ctrl Pts',(-16.1792390499939,-18.7883036704011,
-8.5586297187434));
#62667=CARTESIAN_POINT('Ctrl Pts',(-16.1738678954921,-18.8721297147074,
-8.56280083272135));
#62668=CARTESIAN_POINT('Ctrl Pts',(-16.1726227957354,-18.9562827012374,
-8.56697194669931));
#62669=CARTESIAN_POINT('Ctrl Pts',(-16.1755241458591,-19.0403249895438,
-8.57114306067726));
#62670=CARTESIAN_POINT('Ctrl Pts',(-16.1784245224067,-19.1243390766486,
-8.57531277499763));
#62671=CARTESIAN_POINT('Ctrl Pts',(-16.1854685696706,-19.2082420799258,
-8.579482489318));
#62672=CARTESIAN_POINT('Ctrl Pts',(-16.1966245729686,-19.2915967348155,
-8.58365220363837));
#62673=CARTESIAN_POINT('Ctrl Pts',(-16.2077801792882,-19.374948423589,-8.58782176958242));
#62674=CARTESIAN_POINT('Ctrl Pts',(-16.2230473888477,-19.4577513469169,
-8.59199133552647));
#62675=CARTESIAN_POINT('Ctrl Pts',(-16.2423428203254,-19.5395751007113,
-8.59616090147052));
#62676=CARTESIAN_POINT('Ctrl Pts',(-16.2623166553703,-19.6242756767484,
-8.60047706420944));
#62677=CARTESIAN_POINT('Ctrl Pts',(-16.2866071262492,-19.7079264335903,
-8.60479322694835));
#62678=CARTESIAN_POINT('Ctrl Pts',(-16.3150650107316,-19.790065342138,-8.60910938968727));
#62679=CARTESIAN_POINT('Ctrl Pts',(-16.3425958826201,-19.8695285843793,
-8.61328495387895));
#62680=CARTESIAN_POINT('Ctrl Pts',(-16.3740266108365,-19.9475765433412,
-8.61746051807063));
#62681=CARTESIAN_POINT('Ctrl Pts',(-16.409173118343,-20.0238115367569,-8.6216360822623));
#62682=CARTESIAN_POINT('Ctrl Pts',(-16.4460947923909,-20.1038969784586,
-8.62602254427484));
#62683=CARTESIAN_POINT('Ctrl Pts',(-16.48711720705,-20.1819809787842,-8.63040900628738));
#62684=CARTESIAN_POINT('Ctrl Pts',(-16.531973720249,-20.2576340464641,-8.63479546829992));
#62685=CARTESIAN_POINT('Ctrl Pts',(-16.5768302334481,-20.333287114144,-8.63918193031246));
#62686=CARTESIAN_POINT('Ctrl Pts',(-16.625520460569,-20.4065088081494,-8.643568392325));
#62687=CARTESIAN_POINT('Ctrl Pts',(-16.677728404917,-20.4769088914603,-8.64795485433753));
#62688=CARTESIAN_POINT('Ctrl Pts',(-16.7275341843547,-20.5440697625801,
-8.65213948873058));
#62689=CARTESIAN_POINT('Ctrl Pts',(-16.7807264703943,-20.6089129556999,
-8.65632412312363));
#62690=CARTESIAN_POINT('Ctrl Pts',(-16.8370617843823,-20.6710769052399,
-8.66050875751667));
#62691=CARTESIAN_POINT('Ctrl Pts',(-16.8933169120236,-20.7331523720919,
-8.66468743560061));
#62692=CARTESIAN_POINT('Ctrl Pts',(-16.9527058751385,-20.7925558323524,
-8.66886611368455));
#62693=CARTESIAN_POINT('Ctrl Pts',(-17.0149432821612,-20.8489565100058,
-8.67304479176848));
#62694=CARTESIAN_POINT('Ctrl Pts',(-17.0782962499757,-20.9063681292718,
-8.67729836965392));
#62695=CARTESIAN_POINT('Ctrl Pts',(-17.1446004956328,-20.960667870067,-8.68155194753935));
#62696=CARTESIAN_POINT('Ctrl Pts',(-17.2135136449479,-21.0115439408035,
-8.68580552542479));
#62697=CARTESIAN_POINT('Ctrl Pts',(-17.2810907783904,-21.0614336796322,
-8.68997663940274));
#62698=CARTESIAN_POINT('Ctrl Pts',(-17.3511761736801,-21.1080310270073,
-8.69414775338069));
#62699=CARTESIAN_POINT('Ctrl Pts',(-17.4234128839587,-21.1510819473741,
-8.69831886735864));
#62700=CARTESIAN_POINT('Ctrl Pts',(-17.4956253545116,-21.1941184215888,
-8.70248858167901));
#62701=CARTESIAN_POINT('Ctrl Pts',(-17.5699873115125,-21.2336105969121,
-8.70665829599938));
#62702=CARTESIAN_POINT('Ctrl Pts',(-17.6461139181095,-21.26934845736,-8.71082801031975));
#62703=CARTESIAN_POINT('Ctrl Pts',(-17.7222378157951,-21.3050850461015,
-8.71499757626379));
#62704=CARTESIAN_POINT('Ctrl Pts',(-17.8001258214361,-21.337067390866,-8.71916714220783));
#62705=CARTESIAN_POINT('Ctrl Pts',(-17.8793709005793,-21.3651326325802,
-8.72333670815187));
#62706=CARTESIAN_POINT('Ctrl Pts',(-17.9614021389459,-21.3941846135708,
-8.7276528708908));
#62707=CARTESIAN_POINT('Ctrl Pts',(-18.0448871586123,-21.4190387397285,
-8.73196903362972));
#62708=CARTESIAN_POINT('Ctrl Pts',(-18.1293566950608,-21.4395703957461,
-8.73628519636865));
#62709=CARTESIAN_POINT('Ctrl Pts',(-18.2110746452441,-21.4594332352284,
-8.74046076056033));
#62710=CARTESIAN_POINT('Ctrl Pts',(-18.2937134844264,-21.4752508467085,
-8.74463632475201));
#62711=CARTESIAN_POINT('Ctrl Pts',(-18.3768391873469,-21.4869627519759,
-8.74881188894369));
#62712=CARTESIAN_POINT('Ctrl Pts',(-18.4641633719094,-21.4992661977359,
-8.75319835095624));
#62713=CARTESIAN_POINT('Ctrl Pts',(-18.5520243141257,-21.5070382273415,
-8.75758481296878));
#62714=CARTESIAN_POINT('Ctrl Pts',(-18.6399165515108,-21.5102705690994,
-8.76197127498133));
#62715=CARTESIAN_POINT('Ctrl Pts',(-18.7278087888959,-21.5135029108574,
-8.76635773699387));
#62716=CARTESIAN_POINT('Ctrl Pts',(-18.8157317424276,-21.5121956494501,
-8.77074419900642));
#62717=CARTESIAN_POINT('Ctrl Pts',(-18.9031862415111,-21.5064032601928,
-8.77513066101897));
#62718=CARTESIAN_POINT('Ctrl Pts',(-18.9866168294529,-21.5008773873516,
-8.77931529541201));
#62719=CARTESIAN_POINT('Ctrl Pts',(-19.0699316687706,-21.4912494832414,
-8.78349992980506));
#62720=CARTESIAN_POINT('Ctrl Pts',(-19.1526949496532,-21.4775285662876,
-8.78768456419811));
#62721=CARTESIAN_POINT('Ctrl Pts',(-19.2353404272498,-21.4638271793609,
-8.79186324228205));
#62722=CARTESIAN_POINT('Ctrl Pts',(-19.317435455861,-21.4460444262517,-8.79604192036601));
#62723=CARTESIAN_POINT('Ctrl Pts',(-19.3985474281626,-21.424241233319,-8.80022059844995));
#62724=CARTESIAN_POINT('Ctrl Pts',(-19.4811132742735,-21.4020472338226,
-8.80447417633539));
#62725=CARTESIAN_POINT('Ctrl Pts',(-19.5626599937767,-21.3756872759158,
-8.80872775422082));
#62726=CARTESIAN_POINT('Ctrl Pts',(-19.6427400986363,-21.3452804752328,
-8.81298133210625));
#62727=CARTESIAN_POINT('Ctrl Pts',(-19.7212676943997,-21.315463169715,-8.8171524460842));
#62728=CARTESIAN_POINT('Ctrl Pts',(-19.7983845845478,-21.2817547038762,
-8.82132356006215));
#62729=CARTESIAN_POINT('Ctrl Pts',(-19.8736839568166,-21.2443177089083,
-8.8254946740401));
#62730=CARTESIAN_POINT('Ctrl Pts',(-19.9489580616539,-21.2068932762857,
-8.82966438836047));
#62731=CARTESIAN_POINT('Ctrl Pts',(-20.0224154482671,-21.1657430039569,
-8.83383410268084));
#62732=CARTESIAN_POINT('Ctrl Pts',(-20.0936712215604,-21.1210768011439,
-8.83800381700122));
#62733=CARTESIAN_POINT('Ctrl Pts',(-20.1649244592675,-21.076412187746,-8.84217338294525));
#62734=CARTESIAN_POINT('Ctrl Pts',(-20.2339758500892,-21.0282321376739,
-8.8463429488893));
#62735=CARTESIAN_POINT('Ctrl Pts',(-20.3004681352884,-20.9767907499606,
-8.85051251483334));
#62736=CARTESIAN_POINT('Ctrl Pts',(-20.3692982072082,-20.9235407465151,
-8.85482867757226));
#62737=CARTESIAN_POINT('Ctrl Pts',(-20.4353854517828,-20.8667961238598,
-8.85914484031118));
#62738=CARTESIAN_POINT('Ctrl Pts',(-20.4983710832766,-20.8068840072892,
-8.86346100305011));
#62739=CARTESIAN_POINT('Ctrl Pts',(-20.5593049644494,-20.7489235216143,
-8.86763656724179));
#62740=CARTESIAN_POINT('Ctrl Pts',(-20.6173359087927,-20.6879991088313,
-8.87181213143346));
#62741=CARTESIAN_POINT('Ctrl Pts',(-20.6721781340605,-20.6244429797902,
-8.87598769562514));
#62742=CARTESIAN_POINT('Ctrl Pts',(-20.7297903097517,-20.5576767817616,
-8.88037415763769));
#62743=CARTESIAN_POINT('Ctrl Pts',(-20.7838828183068,-20.4880064858706,
-8.88476061965023));
#62744=CARTESIAN_POINT('Ctrl Pts',(-20.8341751072844,-20.4158526287653,
-8.88914708166277));
#62745=CARTESIAN_POINT('Ctrl Pts',(-20.884467396262,-20.34369877166,-8.89353354367531));
#62746=CARTESIAN_POINT('Ctrl Pts',(-20.930959223453,-20.2690618860433,-8.89792000568786));
#62747=CARTESIAN_POINT('Ctrl Pts',(-20.9734262024012,-20.1923911818451,
-8.9023064677004));
#62748=CARTESIAN_POINT('Ctrl Pts',(-21.0159038253685,-20.1157012607291,
-8.90669402914565));
#62749=CARTESIAN_POINT('Ctrl Pts',(-21.0545007977188,-20.0367143701651,
-8.9110815905909));
#62750=CARTESIAN_POINT('Ctrl Pts',(-21.0889748257324,-19.9558394145314,
-8.91546915203614));
#62751=CARTESIAN_POINT('Ctrl Pts',(-21.1233545067051,-19.8751857940067,
-8.91984470579146));
#62752=CARTESIAN_POINT('Ctrl Pts',(-21.1536335666925,-19.7926547636184,
-8.92422025954678));
#62753=CARTESIAN_POINT('Ctrl Pts',(-21.1796158858339,-19.7086788876113,
-8.92859581330209));
#62754=CARTESIAN_POINT('Ctrl Pts',(-21.2055560013419,-19.6248394154053,
-8.9329642597524));
#62755=CARTESIAN_POINT('Ctrl Pts',(-21.227213143681,-19.5395601416149,-8.9373327062027));
#62756=CARTESIAN_POINT('Ctrl Pts',(-21.2444392039472,-19.4532933305808,
-8.94170115265301));
#62757=CARTESIAN_POINT('Ctrl Pts',(-21.2616295048391,-19.3672055997974,
-8.94606053069709));
#62758=CARTESIAN_POINT('Ctrl Pts',(-21.2744069696189,-19.2801348014838,
-8.95041990874118));
#62759=CARTESIAN_POINT('Ctrl Pts',(-21.2826736357251,-19.1925466660746,
-8.95477928678526));
#62760=CARTESIAN_POINT('Ctrl Pts',(-21.2902149496553,-19.1126438833585,
-8.95875615459968));
#62761=CARTESIAN_POINT('Ctrl Pts',(-21.2940028463113,-19.0323109723971,
-8.9627330224141));
#62762=CARTESIAN_POINT('Ctrl Pts',(-21.293999998394,-18.95190932191,-8.96670989022851));
#62763=CARTESIAN_POINT('Origin',(-18.734,-18.952,1.76670989022851));
#62764=CARTESIAN_POINT('',(-17.1732300669911,-16.9202871232308,-7.65021348292981));
#62765=CARTESIAN_POINT('',(-17.1756294774617,-16.9234129801347,-7.71658757349708));
#62766=CARTESIAN_POINT('',(-17.1744641548914,-16.9218650419685,1.76670989022851));
#62767=CARTESIAN_POINT('',(-21.2939989173812,-18.9496456407966,-8.23329012251171));
#62768=CARTESIAN_POINT('Ctrl Pts',(-17.175629477462,-16.9234129801345,-7.71658757349706));
#62769=CARTESIAN_POINT('Ctrl Pts',(-16.9627571704335,-17.084021412314,-7.72982826622449));
#62770=CARTESIAN_POINT('Ctrl Pts',(-16.1737486124771,-17.8922292135007,
-7.7854608945124));
#62771=CARTESIAN_POINT('Ctrl Pts',(-15.939111508382,-20.1147077358832,-7.88348545836079));
#62772=CARTESIAN_POINT('Ctrl Pts',(-18.1988330721293,-21.9314105656949,
-8.01066126504222));
#62773=CARTESIAN_POINT('Ctrl Pts',(-20.7208249517526,-21.0909115417432,
-8.12726281551247));
#62774=CARTESIAN_POINT('Ctrl Pts',(-21.2877697529773,-19.5894613481947,
-8.20147243042223));
#62775=CARTESIAN_POINT('Ctrl Pts',(-21.2935816048406,-18.9496462807751,
-8.23329010977151));
#62776=CARTESIAN_POINT('Ctrl Pts',(-21.2939989173812,-18.9496456407966,
-8.23329012251171));
#62777=CARTESIAN_POINT('Ctrl Pts',(-21.2938985191548,-18.8404782076697,
-8.23871812867059));
#62778=CARTESIAN_POINT('Ctrl Pts',(-21.2868114602984,-18.7316228556169,
-8.24414613482947));
#62779=CARTESIAN_POINT('Ctrl Pts',(-21.272879163598,-18.6238345041783,-8.24957414098835));
#62780=CARTESIAN_POINT('Ctrl Pts',(-21.2596700733063,-18.5216412981934,
-8.25472038679393));
#62781=CARTESIAN_POINT('Ctrl Pts',(-21.2403084403045,-18.4204066645113,
-8.25986663259951));
#62782=CARTESIAN_POINT('Ctrl Pts',(-21.2149532278239,-18.3207543415199,
-8.26501287840509));
#62783=CARTESIAN_POINT('Ctrl Pts',(-21.1943358111288,-18.2397227402535,
-8.26919751279814));
#62784=CARTESIAN_POINT('Ctrl Pts',(-21.1697059337058,-18.1595514977396,
-8.27338214719119));
#62785=CARTESIAN_POINT('Ctrl Pts',(-21.1411517779373,-18.0806675043515,
-8.27756678158423));
#62786=CARTESIAN_POINT('Ctrl Pts',(-21.1126382654753,-18.001895792564,-8.28174545966817));
#62787=CARTESIAN_POINT('Ctrl Pts',(-21.0802117249138,-17.9244081193636,
-8.28592413775212));
#62788=CARTESIAN_POINT('Ctrl Pts',(-21.0440107968602,-17.8486187792111,
-8.29010281583606));
#62789=CARTESIAN_POINT('Ctrl Pts',(-21.0071609931883,-17.7714709696052,
-8.29435639372149));
#62790=CARTESIAN_POINT('Ctrl Pts',(-20.9664002781983,-17.6960834444032,
-8.29860997160693));
#62791=CARTESIAN_POINT('Ctrl Pts',(-20.9219272181895,-17.6228745401936,
-8.30286354949236));
#62792=CARTESIAN_POINT('Ctrl Pts',(-20.8783163552311,-17.5510849334477,
-8.30703466347032));
#62793=CARTESIAN_POINT('Ctrl Pts',(-20.8311360546879,-17.481390639162,-8.31120577744827));
#62794=CARTESIAN_POINT('Ctrl Pts',(-20.7806202689679,-17.4141620778997,
-8.31537689142622));
#62795=CARTESIAN_POINT('Ctrl Pts',(-20.7301214343076,-17.3469560758303,
-8.31954660574659));
#62796=CARTESIAN_POINT('Ctrl Pts',(-20.6762896134472,-17.282214531026,-8.32371632006697));
#62797=CARTESIAN_POINT('Ctrl Pts',(-20.6194012584856,-17.2202777086088,
-8.32788603438734));
#62798=CARTESIAN_POINT('Ctrl Pts',(-20.5625149278558,-17.1583430901696,
-8.33205560033139));
#62799=CARTESIAN_POINT('Ctrl Pts',(-20.5025725911955,-17.0992133339121,
-8.33622516627543));
#62800=CARTESIAN_POINT('Ctrl Pts',(-20.4398891227942,-17.0431934878746,
-8.34039473221947));
#62801=CARTESIAN_POINT('Ctrl Pts',(-20.3750017809723,-16.9852040531583,
-8.34471089495839));
#62802=CARTESIAN_POINT('Ctrl Pts',(-20.307177357872,-16.9305476379184,-8.34902705769732));
#62803=CARTESIAN_POINT('Ctrl Pts',(-20.2368028123898,-16.8795175013831,
-8.35334322043624));
#62804=CARTESIAN_POINT('Ctrl Pts',(-20.1687207103246,-16.8301496661781,
-8.35751878462792));
#62805=CARTESIAN_POINT('Ctrl Pts',(-20.0982524952705,-16.7841757035315,
-8.3616943488196));
#62806=CARTESIAN_POINT('Ctrl Pts',(-20.0257768405865,-16.7418161628217,
-8.36586991301128));
#62807=CARTESIAN_POINT('Ctrl Pts',(-19.949640612879,-16.6973171424109,-8.37025637502382));
#62808=CARTESIAN_POINT('Ctrl Pts',(-19.8712893431908,-16.6568075367651,
-8.37464283703636));
#62809=CARTESIAN_POINT('Ctrl Pts',(-19.7911876038235,-16.6204866780733,
-8.3790292990489));
#62810=CARTESIAN_POINT('Ctrl Pts',(-19.7110858644562,-16.5841658193814,
-8.38341576106144));
#62811=CARTESIAN_POINT('Ctrl Pts',(-19.6292342232969,-16.5520338488593,
-8.38780222307399));
#62812=CARTESIAN_POINT('Ctrl Pts',(-19.5461152252309,-16.524229652346,-8.39218868508653));
#62813=CARTESIAN_POINT('Ctrl Pts',(-19.4668195289802,-16.4977043913044,
-8.39637337892856));
#62814=CARTESIAN_POINT('Ctrl Pts',(-19.3860753481911,-16.4750187798306,
-8.40055807277059));
#62815=CARTESIAN_POINT('Ctrl Pts',(-19.304289379044,-16.4563297445076,-8.40474276661262));
#62816=CARTESIAN_POINT('Ctrl Pts',(-19.2226201402028,-16.4376673834031,
-8.40892148778481));
#62817=CARTESIAN_POINT('Ctrl Pts',(-19.1399125111903,-16.4229903695736,
-8.41310020895699));
#62818=CARTESIAN_POINT('Ctrl Pts',(-19.0565899050055,-16.4124063803064,
-8.41727893012918));
#62819=CARTESIAN_POINT('Ctrl Pts',(-18.973365253887,-16.4018348337053,-8.42145273874608));
#62820=CARTESIAN_POINT('Ctrl Pts',(-18.8895275166888,-16.3953468042853,
-8.42562654736298));
#62821=CARTESIAN_POINT('Ctrl Pts',(-18.8055104987655,-16.392998974489,-8.42980035597989));
#62822=CARTESIAN_POINT('Ctrl Pts',(-18.7215478255247,-16.3906526633382,
-8.43397146485441));
#62823=CARTESIAN_POINT('Ctrl Pts',(-18.6374065603179,-16.3924412477093,
-8.43814257372892));
#62824=CARTESIAN_POINT('Ctrl Pts',(-18.5535247699726,-16.3983695076722,
-8.44231368260344));
#62825=CARTESIAN_POINT('Ctrl Pts',(-18.4696720738781,-16.4042957114285,
-8.44648334473622));
#62826=CARTESIAN_POINT('Ctrl Pts',(-18.3860791323488,-16.4143587064509,
-8.45065300686901));
#62827=CARTESIAN_POINT('Ctrl Pts',(-18.3031817775233,-16.4285112127885,
-8.45482266900179));
#62828=CARTESIAN_POINT('Ctrl Pts',(-18.2202883084439,-16.4426630557389,
-8.45899213568505));
#62829=CARTESIAN_POINT('Ctrl Pts',(-18.1380908144806,-16.4609039503763,
-8.46316160236831));
#62830=CARTESIAN_POINT('Ctrl Pts',(-18.0570164290525,-16.4831352315959,
-8.46733106905157));
#62831=CARTESIAN_POINT('Ctrl Pts',(-17.9758686662696,-16.5053866335059,
-8.47150430936117));
#62832=CARTESIAN_POINT('Ctrl Pts',(-17.8958464874503,-16.5316355155317,
-8.47567754967078));
#62833=CARTESIAN_POINT('Ctrl Pts',(-17.8173628033139,-16.5617330170771,
-8.47985078998038));
#62834=CARTESIAN_POINT('Ctrl Pts',(-17.738845097665,-16.5918435654428,-8.48402583932774));
#62835=CARTESIAN_POINT('Ctrl Pts',(-17.6618676372617,-16.6258058721945,
-8.48820088867509));
#62836=CARTESIAN_POINT('Ctrl Pts',(-17.5868220329166,-16.6634234310737,
-8.49237593802245));
#62837=CARTESIAN_POINT('Ctrl Pts',(-17.5116490487983,-16.7011048406762,
-8.49655807395194));
#62838=CARTESIAN_POINT('Ctrl Pts',(-17.4384148750597,-16.7424536740456,
-8.50074020988144));
#62839=CARTESIAN_POINT('Ctrl Pts',(-17.3674851350989,-16.7872281589035,
-8.50492234581094));
#62840=CARTESIAN_POINT('Ctrl Pts',(-17.3010306427489,-16.829177638249,-8.50884061366708));
#62841=CARTESIAN_POINT('Ctrl Pts',(-17.2365989396928,-16.8741335235576,
-8.51275888152322));
#62842=CARTESIAN_POINT('Ctrl Pts',(-17.1744641548914,-16.9218650419685,
-8.51667714937936));
#62843=CARTESIAN_POINT('',(-21.2939989424941,-18.9543268925436,-8.16670989022853));
#62844=CARTESIAN_POINT('Ctrl Pts',(-21.2939989424941,-18.9543268925437,
-8.16670989022852));
#62845=CARTESIAN_POINT('Ctrl Pts',(-21.2940748047761,-18.8708647825268,
-8.17086478789788));
#62846=CARTESIAN_POINT('Ctrl Pts',(-21.2900646933588,-18.7872780169979,
-8.17501968556725));
#62847=CARTESIAN_POINT('Ctrl Pts',(-21.2819596922617,-18.7040052286649,
-8.17917458323661));
#62848=CARTESIAN_POINT('Ctrl Pts',(-21.2739328413916,-18.621535375116,-8.18328941845664));
#62849=CARTESIAN_POINT('Ctrl Pts',(-21.2618897634889,-18.539373952273,-8.18740425367668));
#62850=CARTESIAN_POINT('Ctrl Pts',(-21.2458740550218,-18.4579466307083,
-8.19151908889671));
#62851=CARTESIAN_POINT('Ctrl Pts',(-21.2298653109089,-18.3765547174254,
-8.19563213480031));
#62852=CARTESIAN_POINT('Ctrl Pts',(-21.2098874553344,-18.2958967363637,
-8.1997451807039));
#62853=CARTESIAN_POINT('Ctrl Pts',(-21.1860355605651,-18.2163903142807,
-8.20385822660749));
#62854=CARTESIAN_POINT('Ctrl Pts',(-21.1621864189584,-18.1368930694186,
-8.20797079775283));
#62855=CARTESIAN_POINT('Ctrl Pts',(-21.1344642632166,-18.0585475732026,
-8.21208336889816));
#62856=CARTESIAN_POINT('Ctrl Pts',(-21.1030141994635,-17.9817568744174,
-8.2161959400435));
#62857=CARTESIAN_POINT('Ctrl Pts',(-21.0710029255601,-17.9035958852586,
-8.22038189789764));
#62858=CARTESIAN_POINT('Ctrl Pts',(-21.035129571801,-17.8270462022335,-8.22456785575179));
#62859=CARTESIAN_POINT('Ctrl Pts',(-20.9955977974881,-17.7525103575283,
-8.22875381360593));
#62860=CARTESIAN_POINT('Ctrl Pts',(-20.9567081892511,-17.6791852955855,
-8.23287177349703));
#62861=CARTESIAN_POINT('Ctrl Pts',(-20.9142784405326,-17.6078095092631,
-8.23698973338812));
#62862=CARTESIAN_POINT('Ctrl Pts',(-20.8685472200434,-17.5387384653204,
-8.24110769327921));
#62863=CARTESIAN_POINT('Ctrl Pts',(-20.8216832918823,-17.4679566141755,
-8.24532765011488));
#62864=CARTESIAN_POINT('Ctrl Pts',(-20.7713524862055,-17.399595623106,-8.24954760695055));
#62865=CARTESIAN_POINT('Ctrl Pts',(-20.7178552814754,-17.3340017854886,
-8.25376756378622));
#62866=CARTESIAN_POINT('Ctrl Pts',(-20.6643580767453,-17.2684079478711,
-8.25798752062189));
#62867=CARTESIAN_POINT('Ctrl Pts',(-20.6076948817587,-17.2055816046285,
-8.26220747745756));
#62868=CARTESIAN_POINT('Ctrl Pts',(-20.5482046419776,-17.1458268308308,
-8.26642743429323));
#62869=CARTESIAN_POINT('Ctrl Pts',(-20.4892123552949,-17.0865722243692,
-8.27061206868627));
#62870=CARTESIAN_POINT('Ctrl Pts',(-20.427204219073,-17.0301005497847,-8.27479670307932));
#62871=CARTESIAN_POINT('Ctrl Pts',(-20.3624734272386,-16.9767343731088,
-8.27898133747237));
#62872=CARTESIAN_POINT('Ctrl Pts',(-20.2978347716741,-16.9234441565799,
-8.28316001555632));
#62873=CARTESIAN_POINT('Ctrl Pts',(-20.230481510108,-16.8732509480032,-8.28733869364026));
#62874=CARTESIAN_POINT('Ctrl Pts',(-20.1607438576395,-16.8264407877718,
-8.29151737172421));
#62875=CARTESIAN_POINT('Ctrl Pts',(-20.08975620787,-16.7787915890602,-8.29577094960965));
#62876=CARTESIAN_POINT('Ctrl Pts',(-20.0162981861697,-16.7346482555833,
-8.30002452749508));
#62877=CARTESIAN_POINT('Ctrl Pts',(-19.9407536469187,-16.6942698045053,
-8.30427810538052));
#62878=CARTESIAN_POINT('Ctrl Pts',(-19.8666736859741,-16.6546741684936,
-8.30844921935847));
#62879=CARTESIAN_POINT('Ctrl Pts',(-19.7905878123475,-16.6186989652308,
-8.31262033333642));
#62880=CARTESIAN_POINT('Ctrl Pts',(-19.7128859499199,-16.5865439557985,
-8.31679144731437));
#62881=CARTESIAN_POINT('Ctrl Pts',(-19.6352101611027,-16.5543997362902,
-8.32096116163474));
#62882=CARTESIAN_POINT('Ctrl Pts',(-19.5559198851422,-16.5260733404925,
-8.32513087595511));
#62883=CARTESIAN_POINT('Ctrl Pts',(-19.4754262787741,-16.5017169401999,
-8.32930059027548));
#62884=CARTESIAN_POINT('Ctrl Pts',(-19.3949355367137,-16.4773614066125,
-8.33347015621953));
#62885=CARTESIAN_POINT('Ctrl Pts',(-19.3132419899457,-16.4569757200691,
-8.33763972216358));
#62886=CARTESIAN_POINT('Ctrl Pts',(-19.230771941892,-16.4406621816751,-8.34180928810762));
#62887=CARTESIAN_POINT('Ctrl Pts',(-19.1454023486867,-16.4237750793961,
-8.34612545084654));
#62888=CARTESIAN_POINT('Ctrl Pts',(-19.0592011520725,-16.4112519089494,
-8.35044161358546));
#62889=CARTESIAN_POINT('Ctrl Pts',(-18.9726507026517,-16.4031481325656,
-8.35475777632438));
#62890=CARTESIAN_POINT('Ctrl Pts',(-18.8889196250172,-16.3953083358451,
-8.35893334051606));
#62891=CARTESIAN_POINT('Ctrl Pts',(-18.8048621716341,-16.3916044048151,
-8.36310890470774));
#62892=CARTESIAN_POINT('Ctrl Pts',(-18.7209165514642,-16.392033433153,-8.36728446889942));
#62893=CARTESIAN_POINT('Ctrl Pts',(-18.6327310375814,-16.3924841306923,
-8.37167093091196));
#62894=CARTESIAN_POINT('Ctrl Pts',(-18.544669534143,-16.3974962383813,-8.3760573929245));
#62895=CARTESIAN_POINT('Ctrl Pts',(-18.4572333890563,-16.4070048638422,
-8.38044385493705));
#62896=CARTESIAN_POINT('Ctrl Pts',(-18.3697972439697,-16.4165134893032,
-8.38483031694959));
#62897=CARTESIAN_POINT('Ctrl Pts',(-18.2829870179305,-16.4305184650313,
-8.38921677896213));
#62898=CARTESIAN_POINT('Ctrl Pts',(-18.1972887614196,-16.4488937205182,
-8.39360324097467));
#62899=CARTESIAN_POINT('Ctrl Pts',(-18.1155272922731,-16.4664248576231,
-8.39778819867512));
#62900=CARTESIAN_POINT('Ctrl Pts',(-18.0344735156912,-16.4879988204612,
-8.40197315637556));
#62901=CARTESIAN_POINT('Ctrl Pts',(-17.9545574583907,-16.51354365954,-8.40615811407601));
#62902=CARTESIAN_POINT('Ctrl Pts',(-17.8747749678687,-16.5390458045473,
-8.41033607729579));
#62903=CARTESIAN_POINT('Ctrl Pts',(-17.7961268504911,-16.5685054918742,
-8.41451404051556));
#62904=CARTESIAN_POINT('Ctrl Pts',(-17.7190321451558,-16.6017999545501,
-8.41869200373534));
#62905=CARTESIAN_POINT('Ctrl Pts',(-17.6420120287581,-16.6350622049153,
-8.42286592478599));
#62906=CARTESIAN_POINT('Ctrl Pts',(-17.5665427606548,-16.6721516838674,
-8.42703984583664));
#62907=CARTESIAN_POINT('Ctrl Pts',(-17.4930266305908,-16.7128963631808,
-8.43121376688728));
#62908=CARTESIAN_POINT('Ctrl Pts',(-17.4195625033497,-16.7536122210866,
-8.43538473544741));
#62909=CARTESIAN_POINT('Ctrl Pts',(-17.348049170532,-16.7979779202157,-8.43955570400754));
#62910=CARTESIAN_POINT('Ctrl Pts',(-17.2788661013312,-16.8457746234211,
-8.44372667256767));
#62911=CARTESIAN_POINT('Ctrl Pts',(-17.2434387222357,-16.8702504372804,
-8.44586254896173));
#62912=CARTESIAN_POINT('Ctrl Pts',(-17.2086220088753,-16.8956252112277,
-8.44799842535579));
#62913=CARTESIAN_POINT('Ctrl Pts',(-17.1744641548914,-16.9218650419685,
-8.45013430174985));
#62914=CARTESIAN_POINT('Ctrl Pts',(-17.173230066991,-16.9202871232309,-7.65021348292981));
#62915=CARTESIAN_POINT('Ctrl Pts',(-16.6072658842675,-17.3635947026003,
-7.68605039114237));
#62916=CARTESIAN_POINT('Ctrl Pts',(-15.7765851280492,-18.874458207751,-7.76427923491542));
#62917=CARTESIAN_POINT('Ctrl Pts',(-16.9200889756585,-21.3754309612901,
-7.88490001424892));
#62918=CARTESIAN_POINT('Ctrl Pts',(-19.7898862882482,-21.7889693291709,
-8.01207582093036));
#62919=CARTESIAN_POINT('Ctrl Pts',(-21.1940976605954,-20.1719438373811,
-8.10601244625689));
#62920=CARTESIAN_POINT('Ctrl Pts',(-21.2961551338926,-19.1382186499617,
-8.15755713602294));
#62921=CARTESIAN_POINT('Ctrl Pts',(-21.2944496155086,-18.9543273021797,
-8.16670989022852));
#62922=CARTESIAN_POINT('Origin',(-18.734,-18.952,1.76670989022851));
#62923=CARTESIAN_POINT('',(-17.1744641548914,-16.9218650419685,-6.85004462002157));
#62924=CARTESIAN_POINT('',(-17.1744641548914,-16.9218650419685,-6.91673142062773));
#62925=CARTESIAN_POINT('',(-17.1744641548914,-16.9218650419685,1.76670989022851));
#62926=CARTESIAN_POINT('',(-21.29363549648,-18.9525601738873,-7.43329008494618));
#62927=CARTESIAN_POINT('Ctrl Pts',(-17.1744641548914,-16.9218650419685,
-6.91673142062773));
#62928=CARTESIAN_POINT('Ctrl Pts',(-17.1077986118319,-16.9730770580089,
-6.92090111744156));
#62929=CARTESIAN_POINT('Ctrl Pts',(-17.0436334872203,-17.0275952975788,
-6.92507081425539));
#62930=CARTESIAN_POINT('Ctrl Pts',(-16.9823059547924,-17.0851395413732,
-6.92924051106922));
#62931=CARTESIAN_POINT('Ctrl Pts',(-16.9209801805697,-17.1426821354258,
-6.93341008834158));
#62932=CARTESIAN_POINT('Ctrl Pts',(-16.862492171621,-17.2032502457524,-6.93757966561394));
#62933=CARTESIAN_POINT('Ctrl Pts',(-16.807143454622,-17.2665256295233,-6.94174924288631));
#62934=CARTESIAN_POINT('Ctrl Pts',(-16.7501679117016,-17.3316608221585,
-6.94604137361168));
#62935=CARTESIAN_POINT('Ctrl Pts',(-16.696519444733,-17.3996645488824,-6.95033350433705));
#62936=CARTESIAN_POINT('Ctrl Pts',(-16.6464823134451,-17.4701532102405,
-6.95462563506242));
#62937=CARTESIAN_POINT('Ctrl Pts',(-16.5978036071207,-17.5387282215798,
-6.9588012415712));
#62938=CARTESIAN_POINT('Ctrl Pts',(-16.5525428475067,-17.6096545305514,
-6.96297684807997));
#62939=CARTESIAN_POINT('Ctrl Pts',(-16.5109166141274,-17.6825511985679,
-6.96715245458875));
#62940=CARTESIAN_POINT('Ctrl Pts',(-16.4675479521126,-17.7584992414381,
-6.97150284742242));
#62941=CARTESIAN_POINT('Ctrl Pts',(-16.4281250253917,-17.836585719324,-6.97585324025609));
#62942=CARTESIAN_POINT('Ctrl Pts',(-16.3928377730059,-17.9163555499612,
-6.98020363308976));
#62943=CARTESIAN_POINT('Ctrl Pts',(-16.3575505206202,-17.9961253805984,
-6.98455402592343));
#62944=CARTESIAN_POINT('Ctrl Pts',(-16.326399072824,-18.0775780178091,-6.98890441875709));
#62945=CARTESIAN_POINT('Ctrl Pts',(-16.2995147249234,-18.1602415485545,
-6.99325481159076));
#62946=CARTESIAN_POINT('Ctrl Pts',(-16.273654723043,-18.2397554377671,-6.99743944598381));
#62947=CARTESIAN_POINT('Ctrl Pts',(-16.251646255088,-18.3206855701428,-7.00162408037685));
#62948=CARTESIAN_POINT('Ctrl Pts',(-16.233642830573,-18.4026239673095,-7.00580871476989));
#62949=CARTESIAN_POINT('Ctrl Pts',(-16.2156650317043,-18.4844457353098,
-7.00998739285384));
#62950=CARTESIAN_POINT('Ctrl Pts',(-16.2016810508028,-18.5672724719892,
-7.01416607093778));
#62951=CARTESIAN_POINT('Ctrl Pts',(-16.1917950137906,-18.6506798909931,
-7.01834474902173));
#62952=CARTESIAN_POINT('Ctrl Pts',(-16.1817317766699,-18.7355823280388,
-7.02259832690716));
#62953=CARTESIAN_POINT('Ctrl Pts',(-16.1759149888559,-18.8210860111297,
-7.0268519047926));
#62954=CARTESIAN_POINT('Ctrl Pts',(-16.1744002778054,-18.9067312233283,
-7.03110548267803));
#62955=CARTESIAN_POINT('Ctrl Pts',(-16.1729149323844,-18.9907160359655,
-7.03527659665599));
#62956=CARTESIAN_POINT('Ctrl Pts',(-16.1755663524988,-19.0748364579016,
-7.03944771063394));
#62957=CARTESIAN_POINT('Ctrl Pts',(-16.1823546543812,-19.1586543737303,
-7.04361882461189));
#62958=CARTESIAN_POINT('Ctrl Pts',(-16.1891406783834,-19.2424441636479,
-7.04778853893226));
#62959=CARTESIAN_POINT('Ctrl Pts',(-16.2000607901197,-19.3259311909063,
-7.05195825325264));
#62960=CARTESIAN_POINT('Ctrl Pts',(-16.2150630692561,-19.4086801275888,
-7.05612796757301));
#62961=CARTESIAN_POINT('Ctrl Pts',(-16.230064814547,-19.4914261197089,-7.06029753351705));
#62962=CARTESIAN_POINT('Ctrl Pts',(-16.2491483555176,-19.5734336209717,
-7.06446709946108));
#62963=CARTESIAN_POINT('Ctrl Pts',(-16.2722104781215,-19.6542765480702,
-7.06863666540512));
#62964=CARTESIAN_POINT('Ctrl Pts',(-16.2960834365061,-19.7379618127552,
-7.07295282814404));
#62965=CARTESIAN_POINT('Ctrl Pts',(-16.3242198111558,-19.8203985795364,
-7.07726899088297));
#62966=CARTESIAN_POINT('Ctrl Pts',(-16.3564491538595,-19.901132221567,-7.08158515362189));
#62967=CARTESIAN_POINT('Ctrl Pts',(-16.3876286291145,-19.9792359737001,
-7.08576071781356));
#62968=CARTESIAN_POINT('Ctrl Pts',(-16.4226382716202,-20.0557454470086,
-7.08993628200524));
#62969=CARTESIAN_POINT('Ctrl Pts',(-16.4612757941351,-20.1302719058331,
-7.09411184619692));
#62970=CARTESIAN_POINT('Ctrl Pts',(-16.5018648060602,-20.2085625189232,
-7.09849830820946));
#62971=CARTESIAN_POINT('Ctrl Pts',(-16.5464575227362,-20.2846640250238,
-7.10288477022201));
#62972=CARTESIAN_POINT('Ctrl Pts',(-16.5947677080406,-20.3581597352499,
-7.10727123223455));
#62973=CARTESIAN_POINT('Ctrl Pts',(-16.6430778933449,-20.4316554454761,
-7.1116576942471));
#62974=CARTESIAN_POINT('Ctrl Pts',(-16.6951051426578,-20.5025449370743,
-7.11604415625964));
#62975=CARTESIAN_POINT('Ctrl Pts',(-16.7505157350918,-20.5704530178111,
-7.12043061827219));
#62976=CARTESIAN_POINT('Ctrl Pts',(-16.8033768040298,-20.6352365470892,
-7.12461525266524));
#62977=CARTESIAN_POINT('Ctrl Pts',(-16.8595134716063,-20.6975481314175,
-7.12879988705829));
#62978=CARTESIAN_POINT('Ctrl Pts',(-16.918665784363,-20.7570378626327,-7.13298452145133));
#62979=CARTESIAN_POINT('Ctrl Pts',(-16.9777339011242,-20.816442917579,-7.13716319953528));
#62980=CARTESIAN_POINT('Ctrl Pts',(-17.0398088154215,-20.8730337741355,
-7.14134187761923));
#62981=CARTESIAN_POINT('Ctrl Pts',(-17.1045901309625,-20.9264932207236,
-7.14552055570318));
#62982=CARTESIAN_POINT('Ctrl Pts',(-17.170532605027,-20.980910889471,-7.14977413358862));
#62983=CARTESIAN_POINT('Ctrl Pts',(-17.2392791543356,-21.0320834094474,
-7.15402771147406));
#62984=CARTESIAN_POINT('Ctrl Pts',(-17.310473339783,-21.0797151707058,-7.15828128935949));
#62985=CARTESIAN_POINT('Ctrl Pts',(-17.3802872870216,-21.1264234973264,
-7.16245240333745));
#62986=CARTESIAN_POINT('Ctrl Pts',(-17.4524544129442,-21.1697268615306,
-7.1666235173154));
#62987=CARTESIAN_POINT('Ctrl Pts',(-17.5266063947421,-21.2093880220251,
-7.17079463129335));
#62988=CARTESIAN_POINT('Ctrl Pts',(-17.6007334941263,-21.2490358738341,
-7.17496434561372));
#62989=CARTESIAN_POINT('Ctrl Pts',(-17.6768437213087,-21.2850437324073,
-7.1791340599341));
#62990=CARTESIAN_POINT('Ctrl Pts',(-17.7545429309113,-21.3172196197842,
-7.18330377425447));
#62991=CARTESIAN_POINT('Ctrl Pts',(-17.8322393756429,-21.3493943622051,
-7.18747334019852));
#62992=CARTESIAN_POINT('Ctrl Pts',(-17.9115242650163,-21.3777372293231,
-7.19164290614258));
#62993=CARTESIAN_POINT('Ctrl Pts',(-17.9919834625938,-21.4021043770043,
-7.19581247208664));
#62994=CARTESIAN_POINT('Ctrl Pts',(-18.0752715063007,-21.4273282435378,
-7.20012863482555));
#62995=CARTESIAN_POINT('Ctrl Pts',(-18.1598174672116,-21.4482914634568,
-7.20444479756447));
#62996=CARTESIAN_POINT('Ctrl Pts',(-18.2451468157111,-21.4648912758435,
-7.20876096030339));
#62997=CARTESIAN_POINT('Ctrl Pts',(-18.3276965696584,-21.4809503510878,
-7.21293652449507));
#62998=CARTESIAN_POINT('Ctrl Pts',(-18.4109789843022,-21.4929259089215,
-7.21711208868675));
#62999=CARTESIAN_POINT('Ctrl Pts',(-18.4945577002246,-21.5007776256626,
-7.22128765287843));
#63000=CARTESIAN_POINT('Ctrl Pts',(-18.5823577783985,-21.5090259139506,
-7.22567411489096));
#63001=CARTESIAN_POINT('Ctrl Pts',(-18.6704842934734,-21.5127227980494,
-7.23006057690349));
#63002=CARTESIAN_POINT('Ctrl Pts',(-18.7584319418552,-21.5118834114501,
-7.23444703891603));
#63003=CARTESIAN_POINT('Ctrl Pts',(-18.8463795902369,-21.5110440248507,
-7.23883350092856));
#63004=CARTESIAN_POINT('Ctrl Pts',(-18.9341477974438,-21.5056684789459,
-7.24321996294109));
#63005=CARTESIAN_POINT('Ctrl Pts',(-19.0212404493959,-21.4958342957494,
-7.24760642495362));
#63006=CARTESIAN_POINT('Ctrl Pts',(-19.1043258393297,-21.4864525978996,
-7.25179105934668));
#63007=CARTESIAN_POINT('Ctrl Pts',(-19.1871057341709,-21.4729786230522,
-7.25597569373973));
#63008=CARTESIAN_POINT('Ctrl Pts',(-19.2691452086518,-21.455441552275,-7.26016032813278));
#63009=CARTESIAN_POINT('Ctrl Pts',(-19.351067910095,-21.4379294433475,-7.26433900621672));
#63010=CARTESIAN_POINT('Ctrl Pts',(-19.4322518385269,-21.4163658213152,
-7.26851768430066));
#63011=CARTESIAN_POINT('Ctrl Pts',(-19.5122676703939,-21.3908315713103,
-7.2726963623846));
#63012=CARTESIAN_POINT('Ctrl Pts',(-19.5937177285409,-21.3648396382251,
-7.27694994027004));
#63013=CARTESIAN_POINT('Ctrl Pts',(-19.6739569228735,-21.3347333841335,
-7.28120351815547));
#63014=CARTESIAN_POINT('Ctrl Pts',(-19.7525437584804,-21.3006525098577,
-7.2854570960409));
#63015=CARTESIAN_POINT('Ctrl Pts',(-19.8296070349294,-21.267232359833,-7.28962821001886));
#63016=CARTESIAN_POINT('Ctrl Pts',(-19.9050810078233,-21.2299905173577,
-7.29379932399682));
#63017=CARTESIAN_POINT('Ctrl Pts',(-19.9785668286282,-21.1891082694135,
-7.29797043797477));
#63018=CARTESIAN_POINT('Ctrl Pts',(-20.052027990556,-21.1482397399025,-7.30214015229515));
#63019=CARTESIAN_POINT('Ctrl Pts',(-20.1235019236781,-21.1037334544493,
-7.30630986661552));
#63020=CARTESIAN_POINT('Ctrl Pts',(-20.1926138614934,-21.0558169129131,
-7.31047958093589));
#63021=CARTESIAN_POINT('Ctrl Pts',(-20.2617233400094,-21.0079020764531,
-7.31464914687994));
#63022=CARTESIAN_POINT('Ctrl Pts',(-20.3284706127605,-20.9565774880019,
-7.31881871282399));
#63023=CARTESIAN_POINT('Ctrl Pts',(-20.3925105653949,-20.9021135106638,
-7.32298827876803));
#63024=CARTESIAN_POINT('Ctrl Pts',(-20.458802083762,-20.8457346470711,-7.32730444150695));
#63025=CARTESIAN_POINT('Ctrl Pts',(-20.5221919593126,-20.7859918669766,
-7.33162060424587));
#63026=CARTESIAN_POINT('Ctrl Pts',(-20.5823369324963,-20.7232285521553,
-7.33593676698479));
#63027=CARTESIAN_POINT('Ctrl Pts',(-20.6405226895047,-20.6625097457128,
-7.34011233117647));
#63028=CARTESIAN_POINT('Ctrl Pts',(-20.6956714299404,-20.5989645570462,
-7.34428789536814));
#63029=CARTESIAN_POINT('Ctrl Pts',(-20.7475130548916,-20.5329380689265,
-7.34846345955982));
#63030=CARTESIAN_POINT('Ctrl Pts',(-20.8019730770774,-20.4635767398549,
-7.35284992157236));
#63031=CARTESIAN_POINT('Ctrl Pts',(-20.8527827827185,-20.3914773402459,
-7.3572363835849));
#63032=CARTESIAN_POINT('Ctrl Pts',(-20.8996813854343,-20.3170729419278,
-7.36162284559744));
#63033=CARTESIAN_POINT('Ctrl Pts',(-20.94657998815,-20.2426685436098,-7.36600930760998));
#63034=CARTESIAN_POINT('Ctrl Pts',(-20.9895672706481,-20.1659596899256,
-7.37039576962251));
#63035=CARTESIAN_POINT('Ctrl Pts',(-21.0284398795321,-20.0874054955005,
-7.37478223163505));
#63036=CARTESIAN_POINT('Ctrl Pts',(-21.0682036058612,-20.0070505211677,
-7.37926924910127));
#63037=CARTESIAN_POINT('Ctrl Pts',(-21.103794382086,-19.9244993534847,-7.38375626656748));
#63038=CARTESIAN_POINT('Ctrl Pts',(-21.1349820909847,-19.8401919830593,
-7.38824328403369));
#63039=CARTESIAN_POINT('Ctrl Pts',(-21.1660643193882,-19.7561697500644,
-7.39271512587973));
#63040=CARTESIAN_POINT('Ctrl Pts',(-21.1927730322953,-19.6704034844231,
-7.39718696772577));
#63041=CARTESIAN_POINT('Ctrl Pts',(-21.2149257129941,-19.5833537887784,
-7.40165880957181));
#63042=CARTESIAN_POINT('Ctrl Pts',(-21.2370311427379,-19.4964897673327,
-7.40612111312314));
#63043=CARTESIAN_POINT('Ctrl Pts',(-21.2545997969947,-19.4083481090824,
-7.41058341667445));
#63044=CARTESIAN_POINT('Ctrl Pts',(-21.2674980351242,-19.3194067310512,
-7.41504572022578));
#63045=CARTESIAN_POINT('Ctrl Pts',(-21.2803582069864,-19.2307278436205,
-7.41949485428542));
#63046=CARTESIAN_POINT('Ctrl Pts',(-21.2885753721633,-19.1412542906272,
-7.42394398834506));
#63047=CARTESIAN_POINT('Ctrl Pts',(-21.292066600817,-19.0514749505384,-7.4283931224047));
#63048=CARTESIAN_POINT('Ctrl Pts',(-21.2933474798422,-19.0185362676211,
-7.43002544244517));
#63049=CARTESIAN_POINT('Ctrl Pts',(-21.2939927168564,-18.9855565464178,
-7.43165776248564));
#63050=CARTESIAN_POINT('Ctrl Pts',(-21.2939999386838,-18.9525603024938,
-7.43329008252611));
#63051=CARTESIAN_POINT('Ctrl Pts',(-21.2898970146452,-18.9525588546298,
-7.4332901097715));
#63052=CARTESIAN_POINT('Ctrl Pts',(-21.288997505724,-18.4906083046144,-7.4561794192865));
#63053=CARTESIAN_POINT('Ctrl Pts',(-20.9482575273653,-17.1718695394144,
-7.52146066436198));
#63054=CARTESIAN_POINT('Ctrl Pts',(-19.0929371605554,-16.0796618992124,
-7.6158931522705));
#63055=CARTESIAN_POINT('Ctrl Pts',(-17.6442977293701,-16.5698109818192,
-7.68743633066402));
#63056=CARTESIAN_POINT('Ctrl Pts',(-17.175629477462,-16.9234129801345,-7.71658757349706));
#63057=CARTESIAN_POINT('',(-21.2941233546374,-18.9508698167174,-7.36670989022851));
#63058=CARTESIAN_POINT('Ctrl Pts',(-21.2976210191122,-18.9508682726504,
-7.36670989022851));
#63059=CARTESIAN_POINT('Ctrl Pts',(-21.2979707979485,-18.88753758729,-7.36987218932674));
#63060=CARTESIAN_POINT('Ctrl Pts',(-21.2671017039969,-17.9755793917529,
-7.41542642398544));
#63061=CARTESIAN_POINT('Ctrl Pts',(-20.1784866426459,-16.2917839998255,
-7.50337259420463));
#63062=CARTESIAN_POINT('Ctrl Pts',(-18.0960849448548,-16.2958827240454,
-7.5947114926735));
#63063=CARTESIAN_POINT('Ctrl Pts',(-17.2767521307163,-16.8392005158408,
-7.64365845558189));
#63064=CARTESIAN_POINT('Ctrl Pts',(-17.173230066991,-16.9202871232309,-7.65021348292981));
#63065=CARTESIAN_POINT('Ctrl Pts',(-17.1744641548914,-16.9218650419685,
-6.85004462002157));
#63066=CARTESIAN_POINT('Ctrl Pts',(-17.1078661424704,-16.9730251814325,
-6.85422899264962));
#63067=CARTESIAN_POINT('Ctrl Pts',(-17.0438780188053,-17.0273968013221,
-6.85841336527767));
#63068=CARTESIAN_POINT('Ctrl Pts',(-16.9828072236318,-17.0846693222688,
-6.86259773790572));
#63069=CARTESIAN_POINT('Ctrl Pts',(-16.9589890933644,-17.1070060932373,
-6.86422967886963));
#63070=CARTESIAN_POINT('Ctrl Pts',(-16.9356142875333,-17.1297837384485,
-6.86586161983354));
#63071=CARTESIAN_POINT('Ctrl Pts',(-16.9126993772538,-17.1529824788001,
-6.86749356079746));
#63072=CARTESIAN_POINT('Ctrl Pts',(-16.8539408046155,-17.2124688504872,
-6.8716781951905));
#63073=CARTESIAN_POINT('Ctrl Pts',(-16.7979903187279,-17.2749476638324,
-6.87586282958355));
#63074=CARTESIAN_POINT('Ctrl Pts',(-16.7451680193311,-17.3401230342645,
-6.8800474639766));
#63075=CARTESIAN_POINT('Ctrl Pts',(-16.6924209059394,-17.4052056356239,
-6.88422614206054));
#63076=CARTESIAN_POINT('Ctrl Pts',(-16.6427934219786,-17.4729768158299,
-6.88840482014449));
#63077=CARTESIAN_POINT('Ctrl Pts',(-16.5965688328438,-17.5431039762746,
-6.89258349822843));
#63078=CARTESIAN_POINT('Ctrl Pts',(-16.5495157011698,-17.6144881156707,
-6.89683707611387));
#63079=CARTESIAN_POINT('Ctrl Pts',(-16.5059889968457,-17.6883131849443,
-6.9010906539993));
#63080=CARTESIAN_POINT('Ctrl Pts',(-16.4662445138507,-17.7641931743589,
-6.90534423188474));
#63081=CARTESIAN_POINT('Ctrl Pts',(-16.4272705552134,-17.8386020821111,
-6.90951534586269));
#63082=CARTESIAN_POINT('Ctrl Pts',(-16.3919336983951,-17.9149865174728,
-6.91368645984064));
#63083=CARTESIAN_POINT('Ctrl Pts',(-16.3604304325482,-17.9929548975848,
-6.9178575738186));
#63084=CARTESIAN_POINT('Ctrl Pts',(-16.3289377379263,-18.0708971146538,
-6.92202728813897));
#63085=CARTESIAN_POINT('Ctrl Pts',(-16.3012762516654,-18.1504217947137,
-6.92619700245934));
#63086=CARTESIAN_POINT('Ctrl Pts',(-16.277594697511,-18.2311165212713,-6.93036671677971));
#63087=CARTESIAN_POINT('Ctrl Pts',(-16.253913986048,-18.3118083763642,-6.93453628272376));
#63088=CARTESIAN_POINT('Ctrl Pts',(-16.2342130538339,-18.3936697535165,
-6.9387058486678));
#63089=CARTESIAN_POINT('Ctrl Pts',(-16.2185906288469,-18.4762735076589,
-6.94287541461184));
#63090=CARTESIAN_POINT('Ctrl Pts',(-16.2024189386697,-18.5617815078941,
-6.94719157735077));
#63091=CARTESIAN_POINT('Ctrl Pts',(-16.190617990557,-18.6480845421363,-6.95150774008969));
#63092=CARTESIAN_POINT('Ctrl Pts',(-16.1832392059578,-18.7346998122939,
-6.95582390282861));
#63093=CARTESIAN_POINT('Ctrl Pts',(-16.1761007844907,-18.8184935991364,
-6.95999946702029));
#63094=CARTESIAN_POINT('Ctrl Pts',(-16.1731008165489,-18.9025791196894,
-6.96417503121196));
#63095=CARTESIAN_POINT('Ctrl Pts',(-16.1742327266829,-18.9865182046884,
-6.96835059540364));
#63096=CARTESIAN_POINT('Ctrl Pts',(-16.1754218069069,-19.0746968533245,
-6.97273705741619));
#63097=CARTESIAN_POINT('Ctrl Pts',(-16.1811710990057,-19.1627133020808,
-6.97712351942873));
#63098=CARTESIAN_POINT('Ctrl Pts',(-16.1914115149699,-19.2500667639851,
-6.98150998144128));
#63099=CARTESIAN_POINT('Ctrl Pts',(-16.2016519309342,-19.3374202258893,
-6.98589644345382));
#63100=CARTESIAN_POINT('Ctrl Pts',(-16.2163832985703,-19.4241101416678,
-6.99028290546636));
#63101=CARTESIAN_POINT('Ctrl Pts',(-16.2354754819719,-19.5096515334977,
-6.9946693674789));
#63102=CARTESIAN_POINT('Ctrl Pts',(-16.2536892057137,-19.5912570390867,
-6.99885400187195));
#63103=CARTESIAN_POINT('Ctrl Pts',(-16.2759390634244,-19.6721211400212,
-7.003038636265));
#63104=CARTESIAN_POINT('Ctrl Pts',(-16.3021495269225,-19.75181452637,-7.00722327065805));
#63105=CARTESIAN_POINT('Ctrl Pts',(-16.32832268307,-19.8313944790475,-7.01140194874199));
#63106=CARTESIAN_POINT('Ctrl Pts',(-16.3584451047931,-19.9098065938024,
-7.01558062682593));
#63107=CARTESIAN_POINT('Ctrl Pts',(-16.3923904554834,-19.9866326599468,
-7.01975930490988));
#63108=CARTESIAN_POINT('Ctrl Pts',(-16.4269442521886,-20.0648357781129,
-7.02401288279531));
#63109=CARTESIAN_POINT('Ctrl Pts',(-16.4654592728758,-20.1413949579938,
-7.02826646068075));
#63110=CARTESIAN_POINT('Ctrl Pts',(-16.5077494008733,-20.2158861775841,
-7.03252003856618));
#63111=CARTESIAN_POINT('Ctrl Pts',(-16.5492196522172,-20.288933239525,-7.03669115254414));
#63112=CARTESIAN_POINT('Ctrl Pts',(-16.5943197038782,-20.3599913900463,
-7.04086226652209));
#63113=CARTESIAN_POINT('Ctrl Pts',(-16.6428266524925,-20.428683456491,-7.04503338050004));
#63114=CARTESIAN_POINT('Ctrl Pts',(-16.6913173241317,-20.4973524726494,
-7.04920309482041));
#63115=CARTESIAN_POINT('Ctrl Pts',(-16.7432123571371,-20.5636566060813,
-7.05337280914078));
#63116=CARTESIAN_POINT('Ctrl Pts',(-16.7982454758471,-20.627247570427,-7.05754252346116));
#63117=CARTESIAN_POINT('Ctrl Pts',(-16.8532766362426,-20.6908362719333,
-7.0617120894052));
#63118=CARTESIAN_POINT('Ctrl Pts',(-16.9114453586341,-20.751711649014,-7.06588165534924));
#63119=CARTESIAN_POINT('Ctrl Pts',(-16.9724459211977,-20.8095594815388,
-7.07005122129329));
#63120=CARTESIAN_POINT('Ctrl Pts',(-17.0355911882886,-20.8694411724922,
-7.0743673840322));
#63121=CARTESIAN_POINT('Ctrl Pts',(-17.1017707529442,-20.9260780978832,
-7.07868354677113));
#63122=CARTESIAN_POINT('Ctrl Pts',(-17.1706064918292,-20.979165690961,-7.08299970951004));
#63123=CARTESIAN_POINT('Ctrl Pts',(-17.2371999137602,-21.030523961278,-7.08717527370172));
#63124=CARTESIAN_POINT('Ctrl Pts',(-17.3062787039752,-21.0785603570292,
-7.0913508378934));
#63125=CARTESIAN_POINT('Ctrl Pts',(-17.3774708722983,-21.1230432344145,
-7.09552640208508));
#63126=CARTESIAN_POINT('Ctrl Pts',(-17.4522587878001,-21.1697728361884,
-7.09991286409762));
#63127=CARTESIAN_POINT('Ctrl Pts',(-17.5293786750682,-21.2125802257264,
-7.10429932611016));
#63128=CARTESIAN_POINT('Ctrl Pts',(-17.6083720554812,-21.2512524286208,
-7.1086857881227));
#63129=CARTESIAN_POINT('Ctrl Pts',(-17.6873654358942,-21.2899246315151,
-7.11307225013524));
#63130=CARTESIAN_POINT('Ctrl Pts',(-17.7682317459862,-21.3244614898292,
-7.11745871214778));
#63131=CARTESIAN_POINT('Ctrl Pts',(-17.8504927560597,-21.3547099179687,
-7.12184517416032));
#63132=CARTESIAN_POINT('Ctrl Pts',(-17.9289688151197,-21.3835665710906,
-7.12602980855337));
#63133=CARTESIAN_POINT('Ctrl Pts',(-18.009006152961,-21.4086281659991,-7.13021444294641));
#63134=CARTESIAN_POINT('Ctrl Pts',(-18.0902029058993,-21.429725832619,-7.13439907733946));
#63135=CARTESIAN_POINT('Ctrl Pts',(-18.1712840853099,-21.4507934693218,
-7.1385777554234));
#63136=CARTESIAN_POINT('Ctrl Pts',(-18.2535209603944,-21.4679082701427,
-7.14275643350735));
#63137=CARTESIAN_POINT('Ctrl Pts',(-18.3364934985374,-21.4809500946628,
-7.14693511159129));
#63138=CARTESIAN_POINT('Ctrl Pts',(-18.4209532597953,-21.4942256845144,
-7.15118868947673));
#63139=CARTESIAN_POINT('Ctrl Pts',(-18.5061748645251,-21.5032806792605,
-7.15544226736216));
#63140=CARTESIAN_POINT('Ctrl Pts',(-18.5917010358989,-21.508042058499,-7.1596958452476));
#63141=CARTESIAN_POINT('Ctrl Pts',(-18.6755691155499,-21.5127111291099,
-7.16386695922555));
#63142=CARTESIAN_POINT('Ctrl Pts',(-18.7597295775162,-21.5132515520536,
-7.1680380732035));
#63143=CARTESIAN_POINT('Ctrl Pts',(-18.8437446259189,-21.5096465973785,
-7.17220918718146));
#63144=CARTESIAN_POINT('Ctrl Pts',(-18.9277314822607,-21.5060428523808,
-7.17637890150183));
#63145=CARTESIAN_POINT('Ctrl Pts',(-19.0115725627189,-21.4982965120596,
-7.1805486158222));
#63146=CARTESIAN_POINT('Ctrl Pts',(-19.0948308836175,-21.4864429513066,
-7.18471833014257));
#63147=CARTESIAN_POINT('Ctrl Pts',(-19.1780862418277,-21.4745898123542,
-7.18888789608662));
#63148=CARTESIAN_POINT('Ctrl Pts',(-19.2607584263887,-21.4586298092438,
-7.19305746203066));
#63149=CARTESIAN_POINT('Ctrl Pts',(-19.3424177464726,-21.4386499242509,
-7.19722702797471));
#63150=CARTESIAN_POINT('Ctrl Pts',(-19.426948107513,-21.4179675711496,-7.20154319071363));
#63151=CARTESIAN_POINT('Ctrl Pts',(-19.5103925419325,-21.3929775239273,
-7.20585935345255));
#63152=CARTESIAN_POINT('Ctrl Pts',(-19.5922902863025,-21.363832868264,-7.21017551619147));
#63153=CARTESIAN_POINT('Ctrl Pts',(-19.6715202202638,-21.3356375966935,
-7.21435108038315));
#63154=CARTESIAN_POINT('Ctrl Pts',(-19.7493022661266,-21.3035544560161,
-7.21852664457483));
#63155=CARTESIAN_POINT('Ctrl Pts',(-19.8252402968867,-21.2677708467054,
-7.22270220876651));
#63156=CARTESIAN_POINT('Ctrl Pts',(-19.9050137770549,-21.2301798923559,
-7.22708867077905));
#63157=CARTESIAN_POINT('Ctrl Pts',(-19.9827515495241,-21.1885050997007,
-7.23147513279159));
#63158=CARTESIAN_POINT('Ctrl Pts',(-20.058026370739,-21.1430166976971,-7.23586159480413));
#63159=CARTESIAN_POINT('Ctrl Pts',(-20.133301191954,-21.0975282956936,-7.24024805681667));
#63160=CARTESIAN_POINT('Ctrl Pts',(-20.2061126241217,-21.0482266726393,
-7.24463451882921));
#63161=CARTESIAN_POINT('Ctrl Pts',(-20.2760730898189,-20.9954310816997,
-7.24902098084176));
#63162=CARTESIAN_POINT('Ctrl Pts',(-20.3421228419793,-20.9455867065661,
-7.25316224442402));
#63163=CARTESIAN_POINT('Ctrl Pts',(-20.4058887674612,-20.892434299838,-7.25730350800628));
#63164=CARTESIAN_POINT('Ctrl Pts',(-20.4670153688586,-20.8362127616859,
-7.26144477158854));
#63165=CARTESIAN_POINT('Ctrl Pts',(-20.5280546973635,-20.7800714932714,
-7.26558012252323));
#63166=CARTESIAN_POINT('Ctrl Pts',(-20.5864618395735,-20.7208701082191,
-7.26971547345792));
#63167=CARTESIAN_POINT('Ctrl Pts',(-20.6419120481562,-20.6588894564384,
-7.27385082439262));
#63168=CARTESIAN_POINT('Ctrl Pts',(-20.6972986881794,-20.5969798597691,
-7.27798143452815));
#63169=CARTESIAN_POINT('Ctrl Pts',(-20.7497348173452,-20.5322976752762,
-7.28211204466369));
#63170=CARTESIAN_POINT('Ctrl Pts',(-20.7989315869957,-20.465161439182,-7.28624265479922));
#63171=CARTESIAN_POINT('Ctrl Pts',(-20.848098059321,-20.3980665482492,-7.29037072114094));
#63172=CARTESIAN_POINT('Ctrl Pts',(-20.8940288533086,-20.328520983131,-7.29449878748266));
#63173=CARTESIAN_POINT('Ctrl Pts',(-20.9364753744699,-20.2568763255013,
-7.29862685382437));
#63174=CARTESIAN_POINT('Ctrl Pts',(-20.9789091334294,-20.1852532089438,
-7.30275367899922));
#63175=CARTESIAN_POINT('Ctrl Pts',(-21.0178604599826,-20.11153265758,-7.30688050417406));
#63176=CARTESIAN_POINT('Ctrl Pts',(-21.0531249145872,-20.0360939214574,
-7.31100732934891));
#63177=CARTESIAN_POINT('Ctrl Pts',(-21.0883898804923,-19.9606540915461,
-7.31513421435873));
#63178=CARTESIAN_POINT('Ctrl Pts',(-21.1199676712092,-19.8834964546654,
-7.31926109936854));
#63179=CARTESIAN_POINT('Ctrl Pts',(-21.147701166054,-19.8050220870467,-7.32338798437836));
#63180=CARTESIAN_POINT('Ctrl Pts',(-21.175460263615,-19.7264752742866,-7.32751867920248));
#63181=CARTESIAN_POINT('Ctrl Pts',(-21.1993678247306,-19.6466097489538,
-7.3316493740266));
#63182=CARTESIAN_POINT('Ctrl Pts',(-21.2193162430201,-19.5658429540041,
-7.33578006885071));
#63183=CARTESIAN_POINT('Ctrl Pts',(-21.2392749611597,-19.4850344572076,
-7.33991289645233));
#63184=CARTESIAN_POINT('Ctrl Pts',(-21.2552703785522,-19.4033242264923,
-7.34404572405394));
#63185=CARTESIAN_POINT('Ctrl Pts',(-21.2672462583489,-19.3211387199431,
-7.34817855165556));
#63186=CARTESIAN_POINT('Ctrl Pts',(-21.2792406903518,-19.2388258972814,
-7.35231778154836));
#63187=CARTESIAN_POINT('Ctrl Pts',(-21.287203113202,-19.1560367972438,-7.35645701144116));
#63188=CARTESIAN_POINT('Ctrl Pts',(-21.291129302603,-19.0732011954116,-7.36059624133396));
#63189=CARTESIAN_POINT('Ctrl Pts',(-21.2930622985235,-19.0324184251309,
-7.36263412429881));
#63190=CARTESIAN_POINT('Ctrl Pts',(-21.2940177418851,-18.9916243590029,
-7.36467200726366));
#63191=CARTESIAN_POINT('Ctrl Pts',(-21.2939997505486,-18.9508698712832,
-7.36670989022851));
#63192=CARTESIAN_POINT('Origin',(-18.734,-18.952,1.76670989022851));
#63193=CARTESIAN_POINT('',(-17.1744641548914,-16.9218650419685,-6.05008448095771));
#63194=CARTESIAN_POINT('',(-17.1725993332886,-16.9194746534894,-6.11677129901302));
#63195=CARTESIAN_POINT('',(-17.1744641548914,-16.9218650419685,1.76670989022851));
#63196=CARTESIAN_POINT('',(-21.2939991231355,-18.954118854712,-6.6332901097715));
#63197=CARTESIAN_POINT('Ctrl Pts',(-17.1725993332886,-16.9194746534894,
-6.11677129901302));
#63198=CARTESIAN_POINT('Ctrl Pts',(-16.5753465810254,-17.3857070220397,
-6.1545808565094));
#63199=CARTESIAN_POINT('Ctrl Pts',(-15.7555915618427,-18.9714392322238,
-6.23478234956624));
#63200=CARTESIAN_POINT('Ctrl Pts',(-17.0342063769075,-21.4567939233708,
-6.35737577818358));
#63201=CARTESIAN_POINT('Ctrl Pts',(-19.9200692482785,-21.7370548823945,
-6.48455158486502));
#63202=CARTESIAN_POINT('Ctrl Pts',(-21.2201491927466,-20.0919179991473,
-6.57652302872766));
#63203=CARTESIAN_POINT('Ctrl Pts',(-21.2969228070761,-19.0983559330699,
-6.62610253702982));
#63204=CARTESIAN_POINT('Ctrl Pts',(-21.2956373923518,-18.9541202106712,
-6.6332901097715));
#63205=CARTESIAN_POINT('Ctrl Pts',(-21.2939991231355,-18.954118854712,-6.6332901097715));
#63206=CARTESIAN_POINT('Ctrl Pts',(-21.2940674480299,-18.8715687540988,
-6.63740642252224));
#63207=CARTESIAN_POINT('Ctrl Pts',(-21.2901386830331,-18.788875859184,-6.64152273527298));
#63208=CARTESIAN_POINT('Ctrl Pts',(-21.2821979940262,-18.7064659224447,
-6.64563904802373));
#63209=CARTESIAN_POINT('Ctrl Pts',(-21.2742662779566,-18.6241491085059,
-6.64975070936244));
#63210=CARTESIAN_POINT('Ctrl Pts',(-21.2623316869624,-18.5421150878493,
-6.65386237070115));
#63211=CARTESIAN_POINT('Ctrl Pts',(-21.2464314307689,-18.4607889397778,
-6.65797403203986));
#63212=CARTESIAN_POINT('Ctrl Pts',(-21.2305407999848,-18.3795120234587,
-6.66208320433541));
#63213=CARTESIAN_POINT('Ctrl Pts',(-21.2106893569247,-18.2989425946371,
-6.66619237663095));
#63214=CARTESIAN_POINT('Ctrl Pts',(-21.1869659077107,-18.2194986309849,
-6.6703015489265));
#63215=CARTESIAN_POINT('Ctrl Pts',(-21.1632492097462,-18.1400772755973,
-6.67440955182855));
#63216=CARTESIAN_POINT('Ctrl Pts',(-21.1356628286737,-18.0617812045221,
-6.67851755473059));
#63217=CARTESIAN_POINT('Ctrl Pts',(-21.1043458531986,-17.9850147176796,
-6.68262555763264));
#63218=CARTESIAN_POINT('Ctrl Pts',(-21.0730277445932,-17.9082454532244,
-6.686733709173));
#63219=CARTESIAN_POINT('Ctrl Pts',(-21.0379789552763,-17.8330063217982,
-6.69084186071337));
#63220=CARTESIAN_POINT('Ctrl Pts',(-20.9993866849094,-17.7596815996408,
-6.69495001225373));
#63221=CARTESIAN_POINT('Ctrl Pts',(-20.9607561733792,-17.6862842198592,
-6.69906223457025));
#63222=CARTESIAN_POINT('Ctrl Pts',(-20.9185753946451,-17.6148054564872,
-6.70317445688677));
#63223=CARTESIAN_POINT('Ctrl Pts',(-20.8730771242598,-17.5456042319217,
-6.70728667920329));
#63224=CARTESIAN_POINT('Ctrl Pts',(-20.8275541489319,-17.4763654320317,
-6.71140113440064));
#63225=CARTESIAN_POINT('Ctrl Pts',(-20.7787103793543,-17.4094070139061,
-6.715515589598));
#63226=CARTESIAN_POINT('Ctrl Pts',(-20.7268199445207,-17.3450561090317,
-6.71963004479535));
#63227=CARTESIAN_POINT('Ctrl Pts',(-20.6748438133914,-17.2805989295771,
-6.72375129495541));
#63228=CARTESIAN_POINT('Ctrl Pts',(-20.6198112918954,-17.2187582108668,
-6.72787254511546));
#63229=CARTESIAN_POINT('Ctrl Pts',(-20.5620341095491,-17.1598249822283,
-6.73199379527552));
#63230=CARTESIAN_POINT('Ctrl Pts',(-20.529745700387,-17.1268905239828,-6.73429692959298));
#63231=CARTESIAN_POINT('Ctrl Pts',(-20.4966007367167,-17.0948633881749,
-6.73660006391043));
#63232=CARTESIAN_POINT('Ctrl Pts',(-20.4626578964191,-17.0637887096122,
-6.73890319822789));
#63233=CARTESIAN_POINT('Ctrl Pts',(-20.400986123379,-17.0073281863674,-6.74308783262094));
#63234=CARTESIAN_POINT('Ctrl Pts',(-20.3364305466714,-16.9537872066972,
-6.74727246701399));
#63235=CARTESIAN_POINT('Ctrl Pts',(-20.2692989765721,-16.9034744198481,
-6.75145710140703));
#63236=CARTESIAN_POINT('Ctrl Pts',(-20.2022629599535,-16.8532332470235,
-6.75563577949098));
#63237=CARTESIAN_POINT('Ctrl Pts',(-20.1326585979522,-16.8062114135715,
-6.75981445757492));
#63238=CARTESIAN_POINT('Ctrl Pts',(-20.060828991676,-16.7626793686516,-6.76399313565886));
#63239=CARTESIAN_POINT('Ctrl Pts',(-19.9877118913304,-16.7183670431124,
-6.7682467135443));
#63240=CARTESIAN_POINT('Ctrl Pts',(-19.9122893426568,-16.6776711711576,
-6.77250029142973));
#63241=CARTESIAN_POINT('Ctrl Pts',(-19.8349567777298,-16.6408327248832,
-6.77675386931517));
#63242=CARTESIAN_POINT('Ctrl Pts',(-19.759123455476,-16.6047084637741,-6.78092498329312));
#63243=CARTESIAN_POINT('Ctrl Pts',(-19.6814539493098,-16.5722936025649,
-6.78509609727107));
#63244=CARTESIAN_POINT('Ctrl Pts',(-19.6023470115175,-16.5437696398416,
-6.78926721124902));
#63245=CARTESIAN_POINT('Ctrl Pts',(-19.5232666188221,-16.5152552486095,
-6.79343692556939));
#63246=CARTESIAN_POINT('Ctrl Pts',(-19.4427501848434,-16.4906293187767,
-6.79760663988977));
#63247=CARTESIAN_POINT('Ctrl Pts',(-19.3612154692014,-16.4700248278449,
-6.80177635421014));
#63248=CARTESIAN_POINT('Ctrl Pts',(-19.2796836549145,-16.4494210701093,
-6.80594592015419));
#63249=CARTESIAN_POINT('Ctrl Pts',(-19.1971340772291,-16.4328385786397,
-6.81011548609823));
#63250=CARTESIAN_POINT('Ctrl Pts',(-19.1139973178552,-16.4203598126071,
-6.81428505204228));
#63251=CARTESIAN_POINT('Ctrl Pts',(-19.027937572582,-16.407442308555,-6.8186012147812));
#63252=CARTESIAN_POINT('Ctrl Pts',(-18.941249108334,-16.3989225513938,-6.82291737752012));
#63253=CARTESIAN_POINT('Ctrl Pts',(-18.8544163259003,-16.3948336173693,
-6.82723354025904));
#63254=CARTESIAN_POINT('Ctrl Pts',(-18.7704121122212,-16.3908778799405,
-6.83140910445072));
#63255=CARTESIAN_POINT('Ctrl Pts',(-18.6862733092298,-16.3910686822566,
-6.8355846686424));
#63256=CARTESIAN_POINT('Ctrl Pts',(-18.6024375216843,-16.3953828377523,
-6.83976023283408));
#63257=CARTESIAN_POINT('Ctrl Pts',(-18.5143673878106,-16.3999148909862,
-6.84414669484662));
#63258=CARTESIAN_POINT('Ctrl Pts',(-18.4266322652434,-16.4089977253144,
-6.84853315685916));
#63259=CARTESIAN_POINT('Ctrl Pts',(-18.3397299608672,-16.4225433120446,
-6.8529196188717));
#63260=CARTESIAN_POINT('Ctrl Pts',(-18.252827656491,-16.4360888987749,-6.85730608088424));
#63261=CARTESIAN_POINT('Ctrl Pts',(-18.1667587226472,-16.4540970446291,
-6.86169254289678));
#63262=CARTESIAN_POINT('Ctrl Pts',(-18.0820028534405,-16.4764193164273,
-6.86607900490932));
#63263=CARTESIAN_POINT('Ctrl Pts',(-18.0004433963853,-16.4978997446872,
-6.87030003955252));
#63264=CARTESIAN_POINT('Ctrl Pts',(-17.9197934972278,-16.5234553456701,
-6.87452107419572));
#63265=CARTESIAN_POINT('Ctrl Pts',(-17.8404904722151,-16.5529917207818,
-6.87874210883892));
#63266=CARTESIAN_POINT('Ctrl Pts',(-17.7619934028019,-16.5822279181019,
-6.88292024516259));
#63267=CARTESIAN_POINT('Ctrl Pts',(-17.6848164097411,-16.6153642205991,
-6.88709838148626));
#63268=CARTESIAN_POINT('Ctrl Pts',(-17.6093723252539,-16.652258146401,-6.89127651780993));
#63269=CARTESIAN_POINT('Ctrl Pts',(-17.5327663263894,-16.6897202755698,
-6.89551900161289));
#63270=CARTESIAN_POINT('Ctrl Pts',(-17.4579475345501,-16.7310566404979,
-6.89976148541586));
#63271=CARTESIAN_POINT('Ctrl Pts',(-17.385329197042,-16.7760663922701,-6.90400396921883));
#63272=CARTESIAN_POINT('Ctrl Pts',(-17.3127108595338,-16.8210761440422,
-6.90824645302179));
#63273=CARTESIAN_POINT('Ctrl Pts',(-17.2422934238465,-16.8697590596227,
-6.91248893682476));
#63274=CARTESIAN_POINT('Ctrl Pts',(-17.1744641548914,-16.9218650419685,
-6.91673142062773));
#63275=CARTESIAN_POINT('',(-21.293999428374,-18.9502892327451,-6.5667098902584));
#63276=CARTESIAN_POINT('Ctrl Pts',(-21.293999428374,-18.9502892327451,-6.5667098902584));
#63277=CARTESIAN_POINT('Ctrl Pts',(-21.2939356382109,-18.8548333601135,
-6.57143929947811));
#63278=CARTESIAN_POINT('Ctrl Pts',(-21.2885288437516,-18.7595846663126,
-6.57616870869782));
#63279=CARTESIAN_POINT('Ctrl Pts',(-21.2778724975473,-18.6650980721178,
-6.58089811791753));
#63280=CARTESIAN_POINT('Ctrl Pts',(-21.2671635859909,-18.5701453968674,
-6.5856508562461));
#63281=CARTESIAN_POINT('Ctrl Pts',(-21.2511533349016,-18.4759625571734,
-6.59040359457466));
#63282=CARTESIAN_POINT('Ctrl Pts',(-21.2299860493113,-18.383094347327,-6.59515633290323));
#63283=CARTESIAN_POINT('Ctrl Pts',(-21.2086961910769,-18.2896883688573,
-6.59993659274375));
#63284=CARTESIAN_POINT('Ctrl Pts',(-21.1821895164639,-18.1976124823347,
-6.60471685258427));
#63285=CARTESIAN_POINT('Ctrl Pts',(-21.1506609174307,-18.1073994967067,
-6.60949711242479));
#63286=CARTESIAN_POINT('Ctrl Pts',(-21.1426476472041,-18.0844710744505,
-6.61071205742805));
#63287=CARTESIAN_POINT('Ctrl Pts',(-21.1343102131572,-18.061662873534,-6.61192700243132));
#63288=CARTESIAN_POINT('Ctrl Pts',(-21.1256522921827,-18.0389833992214,
-6.61314194743458));
#63289=CARTESIAN_POINT('Ctrl Pts',(-21.0958318198278,-17.9608684985716,
-6.61732658182763));
#63290=CARTESIAN_POINT('Ctrl Pts',(-21.062124806143,-17.8840707367778,-6.62151121622068));
#63291=CARTESIAN_POINT('Ctrl Pts',(-21.0246680532229,-17.8090039939071,
-6.62569585061373));
#63292=CARTESIAN_POINT('Ctrl Pts',(-20.9872646153543,-17.7340440992535,
-6.62987452869768));
#63293=CARTESIAN_POINT('Ctrl Pts',(-20.9461222434272,-17.6608107375728,
-6.63405320678162));
#63294=CARTESIAN_POINT('Ctrl Pts',(-20.9014264094921,-17.5896994606784,
-6.63823188486557));
#63295=CARTESIAN_POINT('Ctrl Pts',(-20.8559294348561,-17.5173135652524,
-6.64248546275101));
#63296=CARTESIAN_POINT('Ctrl Pts',(-20.8067505255347,-17.4471270300727,
-6.64673904063645));
#63297=CARTESIAN_POINT('Ctrl Pts',(-20.7541351457543,-17.3795325145211,
-6.65099261852188));
#63298=CARTESIAN_POINT('Ctrl Pts',(-20.7025398177813,-17.3132484505532,
-6.65516373249984));
#63299=CARTESIAN_POINT('Ctrl Pts',(-20.6476403712485,-17.2494571801025,
-6.65933484647779));
#63300=CARTESIAN_POINT('Ctrl Pts',(-20.5897118973504,-17.188499686977,-6.66350596045574));
#63301=CARTESIAN_POINT('Ctrl Pts',(-20.5318028619112,-17.127562648727,-6.66767567477611));
#63302=CARTESIAN_POINT('Ctrl Pts',(-20.4708671343697,-17.0694578324914,
-6.67184538909649));
#63303=CARTESIAN_POINT('Ctrl Pts',(-20.4072185463107,-17.0144913687206,
-6.67601510341686));
#63304=CARTESIAN_POINT('Ctrl Pts',(-20.3435722231415,-16.9595268608925,
-6.6801846693609));
#63305=CARTESIAN_POINT('Ctrl Pts',(-20.2772135801197,-16.9077007835214,
-6.68435423530495));
#63306=CARTESIAN_POINT('Ctrl Pts',(-20.2084905554454,-16.8592798558091,
-6.68852380124899));
#63307=CARTESIAN_POINT('Ctrl Pts',(-20.1373513140027,-16.8091565080122,
-6.69283996398791));
#63308=CARTESIAN_POINT('Ctrl Pts',(-20.0636787652557,-16.7626825189766,
-6.69715612672683));
#63309=CARTESIAN_POINT('Ctrl Pts',(-19.9878910926204,-16.7201045885062,
-6.70147228946575));
#63310=CARTESIAN_POINT('Ctrl Pts',(-19.9145721954497,-16.6789136296424,
-6.70564785365743));
#63311=CARTESIAN_POINT('Ctrl Pts',(-19.8392743011541,-16.6413689670526,
-6.70982341784911));
#63312=CARTESIAN_POINT('Ctrl Pts',(-19.7623989816003,-16.607646030429,-6.71399898204079));
#63313=CARTESIAN_POINT('Ctrl Pts',(-19.6816408724096,-16.5722198284451,
-6.71838544405333));
#63314=CARTESIAN_POINT('Ctrl Pts',(-19.5991423447411,-16.5410117758973,
-6.72277190606587));
#63315=CARTESIAN_POINT('Ctrl Pts',(-19.5153878511231,-16.5141663251737,
-6.72715836807841));
#63316=CARTESIAN_POINT('Ctrl Pts',(-19.4316333575051,-16.48732087445,-6.73154483009095));
#63317=CARTESIAN_POINT('Ctrl Pts',(-19.3466234783172,-16.4648381003647,
-6.73593129210349));
#63318=CARTESIAN_POINT('Ctrl Pts',(-19.2608535512399,-16.4468003401833,
-6.74031775411602));
#63319=CARTESIAN_POINT('Ctrl Pts',(-19.179022131781,-16.4295908639741,-6.74450279221877));
#63320=CARTESIAN_POINT('Ctrl Pts',(-19.0961943140763,-16.4163630651949,
-6.74868783032151));
#63321=CARTESIAN_POINT('Ctrl Pts',(-19.0127922770529,-16.4072259695101,
-6.75287286842426));
#63322=CARTESIAN_POINT('Ctrl Pts',(-18.9295335010323,-16.3981045687597,
-6.75705071782063));
#63323=CARTESIAN_POINT('Ctrl Pts',(-18.8457029204367,-16.3930599483569,
-6.761228567217));
#63324=CARTESIAN_POINT('Ctrl Pts',(-18.7617332667381,-16.3921502259086,
-6.76540641661338));
#63325=CARTESIAN_POINT('Ctrl Pts',(-18.6778456877694,-16.3912413926531,
-6.76958018244092));
#63326=CARTESIAN_POINT('Ctrl Pts',(-18.5938197628442,-16.3944594382541,
-6.77375394826846));
#63327=CARTESIAN_POINT('Ctrl Pts',(-18.5100929256538,-16.4018106693703,
-6.77792771409599));
#63328=CARTESIAN_POINT('Ctrl Pts',(-18.4264228070334,-16.409156920586,-6.78209865251434));
#63329=CARTESIAN_POINT('Ctrl Pts',(-18.3430518306328,-16.4206307562904,
-6.78626959093268));
#63330=CARTESIAN_POINT('Ctrl Pts',(-18.2604156415099,-16.4361864426406,
-6.79044052935102));
#63331=CARTESIAN_POINT('Ctrl Pts',(-18.1778106423856,-16.451736257691,-6.79460989350069));
#63332=CARTESIAN_POINT('Ctrl Pts',(-18.0959403308813,-16.4713647764078,
-6.79877925765036));
#63333=CARTESIAN_POINT('Ctrl Pts',(-18.0152320948012,-16.494974827468,-6.80294862180003));
#63334=CARTESIAN_POINT('Ctrl Pts',(-17.9344957178861,-16.5185931107307,
-6.8071194396971));
#63335=CARTESIAN_POINT('Ctrl Pts',(-17.8549226701269,-16.5461955784774,
-6.81129025759418));
#63336=CARTESIAN_POINT('Ctrl Pts',(-17.7769262676959,-16.5776348488631,
-6.81546107549126));
#63337=CARTESIAN_POINT('Ctrl Pts',(-17.6989179895211,-16.6090789061967,
-6.81963252843768));
#63338=CARTESIAN_POINT('Ctrl Pts',(-17.6224872570614,-16.644360746009,-6.82380398138411));
#63339=CARTESIAN_POINT('Ctrl Pts',(-17.5480265683097,-16.6832851613028,
-6.82797543433053));
#63340=CARTESIAN_POINT('Ctrl Pts',(-17.4734822892033,-16.722253273556,-6.83215157019405));
#63341=CARTESIAN_POINT('Ctrl Pts',(-17.4009128734863,-16.7648719041555,
-6.83632770605757));
#63342=CARTESIAN_POINT('Ctrl Pts',(-17.3306849630993,-16.8109005377591,
-6.84050384192108));
#63343=CARTESIAN_POINT('Ctrl Pts',(-17.2772041911319,-16.8459527961013,
-6.84368410128791));
#63344=CARTESIAN_POINT('Ctrl Pts',(-17.2250808115903,-16.8829816711023,
-6.84686436065474));
#63345=CARTESIAN_POINT('Ctrl Pts',(-17.1744641548914,-16.9218650419685,
-6.85004462002157));
#63346=CARTESIAN_POINT('Ctrl Pts',(-17.1744641548914,-16.9218650419685,
-6.05008448095771));
#63347=CARTESIAN_POINT('Ctrl Pts',(-17.1077757142765,-16.9730946477551,
-6.05425482184353));
#63348=CARTESIAN_POINT('Ctrl Pts',(-17.0436322004974,-17.027599857526,-6.05842516272933));
#63349=CARTESIAN_POINT('Ctrl Pts',(-16.9823602549826,-17.0850885924406,
-6.06259550361515));
#63350=CARTESIAN_POINT('Ctrl Pts',(-16.9210196771529,-17.1426417219966,
-6.06677051580929));
#63351=CARTESIAN_POINT('Ctrl Pts',(-16.8625574218519,-17.2031847300844,
-6.07094552800343));
#63352=CARTESIAN_POINT('Ctrl Pts',(-16.8072633052852,-17.2663886244928,
-6.07512054019757));
#63353=CARTESIAN_POINT('Ctrl Pts',(-16.7519329827071,-17.3296339041525,
-6.07929828614619));
#63354=CARTESIAN_POINT('Ctrl Pts',(-16.6997752124231,-17.3955431772239,
-6.08347603209481));
#63355=CARTESIAN_POINT('Ctrl Pts',(-16.651038064558,-17.4637562109992,-6.08765377804343));
#63356=CARTESIAN_POINT('Ctrl Pts',(-16.6022223342987,-17.5320792295344,
-6.09183826007106));
#63357=CARTESIAN_POINT('Ctrl Pts',(-16.5568384799099,-17.6027130346787,
-6.09602274209869));
#63358=CARTESIAN_POINT('Ctrl Pts',(-16.5150897345212,-17.6752708847399,
-6.10020722412632));
#63359=CARTESIAN_POINT('Ctrl Pts',(-16.5010171306903,-17.6997285748867,
-6.10161772298716));
#63360=CARTESIAN_POINT('Ctrl Pts',(-16.4873571552457,-17.7244046987976,
-6.103028221848));
#63361=CARTESIAN_POINT('Ctrl Pts',(-16.4741163568267,-17.7492839406919,
-6.10443872070885));
#63362=CARTESIAN_POINT('Ctrl Pts',(-16.4348338717473,-17.8230950824048,
-6.10862335510189));
#63363=CARTESIAN_POINT('Ctrl Pts',(-16.3990982578627,-17.8989701434485,
-6.11280798949494));
#63364=CARTESIAN_POINT('Ctrl Pts',(-16.3671315774458,-17.9765340240092,
-6.11699262388799));
#63365=CARTESIAN_POINT('Ctrl Pts',(-16.3352103976417,-18.0539875019864,
-6.12117130197193));
#63366=CARTESIAN_POINT('Ctrl Pts',(-16.3070476692934,-18.1331246030375,
-6.12534998005587));
#63367=CARTESIAN_POINT('Ctrl Pts',(-16.2828196558217,-18.2135455868409,
-6.12952865813981));
#63368=CARTESIAN_POINT('Ctrl Pts',(-16.2581573726209,-18.2954080589815,
-6.13378223602525));
#63369=CARTESIAN_POINT('Ctrl Pts',(-16.2375724777943,-18.3786004681759,
-6.13803581391068));
#63370=CARTESIAN_POINT('Ctrl Pts',(-16.2211996301978,-18.4626797556591,
-6.14228939179612));
#63371=CARTESIAN_POINT('Ctrl Pts',(-16.2051442022009,-18.5451290020872,
-6.14646050577408));
#63372=CARTESIAN_POINT('Ctrl Pts',(-16.1931390533222,-18.6284305735954,
-6.15063161975203));
#63373=CARTESIAN_POINT('Ctrl Pts',(-16.1852604222201,-18.7121530390888,
-6.15480273372998));
#63374=CARTESIAN_POINT('Ctrl Pts',(-16.1773844348688,-18.7958474107003,
-6.15897244805036));
#63375=CARTESIAN_POINT('Ctrl Pts',(-16.1736322583368,-18.8799619381736,
-6.16314216237074));
#63376=CARTESIAN_POINT('Ctrl Pts',(-16.1740284019004,-18.9640588939549,
-6.16731187669112));
#63377=CARTESIAN_POINT('Ctrl Pts',(-16.1744245313676,-19.0481528572053,
-6.17148144263516));
#63378=CARTESIAN_POINT('Ctrl Pts',(-16.1789686844146,-19.1322287899831,
-6.1756510085792));
#63379=CARTESIAN_POINT('Ctrl Pts',(-16.1876332505419,-19.2158491562505,
-6.17982057452324));
#63380=CARTESIAN_POINT('Ctrl Pts',(-16.1966024521253,-19.3024095114392,
-6.18413673726216));
#63381=CARTESIAN_POINT('Ctrl Pts',(-16.2099871509033,-19.3884811440156,
-6.18845290000108));
#63382=CARTESIAN_POINT('Ctrl Pts',(-16.2276984844482,-19.4735867263866,
-6.19276906274));
#63383=CARTESIAN_POINT('Ctrl Pts',(-16.2448328731658,-19.5559200033633,
-6.19694462693168));
#63384=CARTESIAN_POINT('Ctrl Pts',(-16.2660161808877,-19.6373487577949,
-6.20112019112336));
#63385=CARTESIAN_POINT('Ctrl Pts',(-16.2911167416148,-19.7174550188623,
-6.20529575531504));
#63386=CARTESIAN_POINT('Ctrl Pts',(-16.3174850719934,-19.8016072567417,
-6.20968221732758));
#63387=CARTESIAN_POINT('Ctrl Pts',(-16.3481765728435,-19.8842993445547,
-6.21406867934012));
#63388=CARTESIAN_POINT('Ctrl Pts',(-16.3829817631981,-19.9650711970168,
-6.21845514135267));
#63389=CARTESIAN_POINT('Ctrl Pts',(-16.4177869535527,-20.0458430494789,
-6.22284160336521));
#63390=CARTESIAN_POINT('Ctrl Pts',(-16.4567055084015,-20.1246941799628,
-6.22722806537775));
#63391=CARTESIAN_POINT('Ctrl Pts',(-16.4994739740983,-20.2011971179794,
-6.23161452739029));
#63392=CARTESIAN_POINT('Ctrl Pts',(-16.5402745992903,-20.2741800424133,
-6.23579916178334));
#63393=CARTESIAN_POINT('Ctrl Pts',(-16.5847305081231,-20.3452977698653,
-6.23998379617638));
#63394=CARTESIAN_POINT('Ctrl Pts',(-16.6326464991108,-20.4141605466913,
-6.24416843056943));
#63395=CARTESIAN_POINT('Ctrl Pts',(-16.680494287616,-20.4829253058779,-6.24834710865337));
#63396=CARTESIAN_POINT('Ctrl Pts',(-16.7317921151756,-20.5494411154154,
-6.2525257867373));
#63397=CARTESIAN_POINT('Ctrl Pts',(-16.786299271486,-20.6133433938069,-6.25670446482123));
#63398=CARTESIAN_POINT('Ctrl Pts',(-16.8417834293997,-20.678391074613,-6.26095804270667));
#63399=CARTESIAN_POINT('Ctrl Pts',(-16.9005928669018,-20.74073018676,-6.26521162059211));
#63400=CARTESIAN_POINT('Ctrl Pts',(-16.962427929971,-20.8000076841543,-6.26946519847754));
#63401=CARTESIAN_POINT('Ctrl Pts',(-17.0230641996815,-20.858135971591,-6.27363631245549));
#63402=CARTESIAN_POINT('Ctrl Pts',(-17.0866094791679,-20.91331996266,-6.27780742643344));
#63403=CARTESIAN_POINT('Ctrl Pts',(-17.1527422696948,-20.9652620272458,
-6.28197854041139));
#63404=CARTESIAN_POINT('Ctrl Pts',(-17.2188528687252,-21.0171866621702,
-6.28614825473177));
#63405=CARTESIAN_POINT('Ctrl Pts',(-17.2875488929265,-21.065871247202,-6.29031796905214));
#63406=CARTESIAN_POINT('Ctrl Pts',(-17.3584755491042,-21.1110582402955,
-6.29448768337252));
#63407=CARTESIAN_POINT('Ctrl Pts',(-17.429399681407,-21.1562436254418,-6.29865724931656));
#63408=CARTESIAN_POINT('Ctrl Pts',(-17.5025538994259,-21.1979314196434,
-6.30282681526059));
#63409=CARTESIAN_POINT('Ctrl Pts',(-17.5775553595551,-21.2359080090026,
-6.30699638120463));
#63410=CARTESIAN_POINT('Ctrl Pts',(-17.6551937784983,-21.2752198083945,
-6.31131254394355));
#63411=CARTESIAN_POINT('Ctrl Pts',(-17.7348112839516,-21.3105543371329,
-6.31562870668248));
#63412=CARTESIAN_POINT('Ctrl Pts',(-17.8159584194011,-21.3417279460833,
-6.3199448694214));
#63413=CARTESIAN_POINT('Ctrl Pts',(-17.8944621954484,-21.371886078001,-6.32412043361308));
#63414=CARTESIAN_POINT('Ctrl Pts',(-17.9743970142424,-21.3981501088934,
-6.32829599780477));
#63415=CARTESIAN_POINT('Ctrl Pts',(-18.0553401601613,-21.4204045093522,
-6.33247156199645));
#63416=CARTESIAN_POINT('Ctrl Pts',(-18.1403715519565,-21.4437829266733,
-6.336858024009));
#63417=CARTESIAN_POINT('Ctrl Pts',(-18.2265152388006,-21.4627358902474,
-6.34124448602154));
#63418=CARTESIAN_POINT('Ctrl Pts',(-18.3132709737048,-21.4771905049783,
-6.34563094803409));
#63419=CARTESIAN_POINT('Ctrl Pts',(-18.400026708609,-21.4916451197093,-6.35001741004663));
#63420=CARTESIAN_POINT('Ctrl Pts',(-18.487393906475,-21.5016013954773,-6.35440387205918));
#63421=CARTESIAN_POINT('Ctrl Pts',(-18.5748705298082,-21.5070494734381,
-6.35879033407172));
#63422=CARTESIAN_POINT('Ctrl Pts',(-18.6583222240302,-21.512246877256,-6.36297496846477));
#63423=CARTESIAN_POINT('Ctrl Pts',(-18.7421841184711,-21.5133611702432,
-6.36715960285781));
#63424=CARTESIAN_POINT('Ctrl Pts',(-18.826022833134,-21.5103455197025,-6.37134423725085));
#63425=CARTESIAN_POINT('Ctrl Pts',(-18.9097422137638,-21.5073341615672,
-6.37552291533479));
#63426=CARTESIAN_POINT('Ctrl Pts',(-18.9934380243477,-21.5002045527774,
-6.37970159341873));
#63427=CARTESIAN_POINT('Ctrl Pts',(-19.0766734176211,-21.4889617515556,
-6.38388027150267));
#63428=CARTESIAN_POINT('Ctrl Pts',(-19.1614007454988,-21.4775174312019,
-6.38813384938811));
#63429=CARTESIAN_POINT('Ctrl Pts',(-19.2456505065467,-21.4618109801084,
-6.39238742727355));
#63430=CARTESIAN_POINT('Ctrl Pts',(-19.3289636478325,-21.4419032627309,
-6.39664100515898));
#63431=CARTESIAN_POINT('Ctrl Pts',(-19.4106616013023,-21.4223814953014,
-6.40081211913693));
#63432=CARTESIAN_POINT('Ctrl Pts',(-19.4914584592899,-21.3988200192304,
-6.40498323311488));
#63433=CARTESIAN_POINT('Ctrl Pts',(-19.5709299408012,-21.3713280625394,
-6.40915434709283));
#63434=CARTESIAN_POINT('Ctrl Pts',(-19.6503747548895,-21.3438453310399,
-6.41332406141321));
#63435=CARTESIAN_POINT('Ctrl Pts',(-19.7284946413757,-21.3124348885696,
-6.41749377573358));
#63436=CARTESIAN_POINT('Ctrl Pts',(-19.8048810053292,-21.2772556574332,
-6.42166349005396));
#63437=CARTESIAN_POINT('Ctrl Pts',(-19.8812646511281,-21.2420776781249,
-6.425833055998));
#63438=CARTESIAN_POINT('Ctrl Pts',(-19.9559144795495,-21.2031313700067,
-6.43000262194205));
#63439=CARTESIAN_POINT('Ctrl Pts',(-20.0284436491279,-21.1606230188134,
-6.43417218788609));
#63440=CARTESIAN_POINT('Ctrl Pts',(-20.1035228548342,-21.116620126432,-6.43848835062502));
#63441=CARTESIAN_POINT('Ctrl Pts',(-20.1763290473291,-21.0688003143228,
-6.44280451336394));
#63442=CARTESIAN_POINT('Ctrl Pts',(-20.2464645244675,-21.0174420984931,
-6.44712067610286));
#63443=CARTESIAN_POINT('Ctrl Pts',(-20.314315345815,-20.967756871142,-6.45129624029455));
#63444=CARTESIAN_POINT('Ctrl Pts',(-20.3796664407519,-20.9147605602809,
-6.45547180448623));
#63445=CARTESIAN_POINT('Ctrl Pts',(-20.4421918593802,-20.8587460689739,
-6.45964736867791));
#63446=CARTESIAN_POINT('Ctrl Pts',(-20.5078752882633,-20.7999024188728,
-6.46403383069045));
#63447=CARTESIAN_POINT('Ctrl Pts',(-20.5704396751019,-20.7377280904822,
-6.46842029270299));
#63448=CARTESIAN_POINT('Ctrl Pts',(-20.6295529524493,-20.6726042556209,
-6.47280675471554));
#63449=CARTESIAN_POINT('Ctrl Pts',(-20.6886662297966,-20.6074804207597,
-6.47719321672808));
#63450=CARTESIAN_POINT('Ctrl Pts',(-20.7443280892575,-20.5394075767507,
-6.48157967874062));
#63451=CARTESIAN_POINT('Ctrl Pts',(-20.7962584977303,-20.4688025212726,
-6.48596614075316));
#63452=CARTESIAN_POINT('Ctrl Pts',(-20.8460908704135,-20.4010499743282,
-6.49017538570612));
#63453=CARTESIAN_POINT('Ctrl Pts',(-20.8926734978047,-20.3307132360494,
-6.49438463065908));
#63454=CARTESIAN_POINT('Ctrl Pts',(-20.9357293738869,-20.2581346654015,
-6.49859387561203));
#63455=CARTESIAN_POINT('Ctrl Pts',(-20.978722858141,-20.1856612676154,-6.50279702099133));
#63456=CARTESIAN_POINT('Ctrl Pts',(-21.0181995127225,-20.1109528753409,
-6.50700016637063));
#63457=CARTESIAN_POINT('Ctrl Pts',(-21.0539239335175,-20.0343829926107,
-6.51120331174993));
#63458=CARTESIAN_POINT('Ctrl Pts',(-21.0896068791139,-19.9579020056841,
-6.51540157737791));
#63459=CARTESIAN_POINT('Ctrl Pts',(-21.1215460556627,-19.8795642299174,
-6.51959984300589));
#63460=CARTESIAN_POINT('Ctrl Pts',(-21.1495512259748,-19.7997689984256,
-6.52379810863387));
#63461=CARTESIAN_POINT('Ctrl Pts',(-21.1775306085271,-19.7200472440895,
-6.52799250840908));
#63462=CARTESIAN_POINT('Ctrl Pts',(-21.2015830381501,-19.6388711282236,
-6.53218690818428));
#63463=CARTESIAN_POINT('Ctrl Pts',(-21.2215663308332,-19.556660028202,-6.53638130795949));
#63464=CARTESIAN_POINT('Ctrl Pts',(-21.2415389226779,-19.4744929513404,
-6.54057346167872));
#63465=CARTESIAN_POINT('Ctrl Pts',(-21.2574466025637,-19.391292431292,-6.54476561539796));
#63466=CARTESIAN_POINT('Ctrl Pts',(-21.2691973211301,-19.3074919730945,
-6.54895776911719));
#63467=CARTESIAN_POINT('Ctrl Pts',(-21.2809466969546,-19.2237010906845,
-6.55314944380356));
#63468=CARTESIAN_POINT('Ctrl Pts',(-21.288539988214,-19.1393108539585,-6.55734111848993));
#63469=CARTESIAN_POINT('Ctrl Pts',(-21.2919366299884,-19.0547628189733,
-6.5615327931763));
#63470=CARTESIAN_POINT('Ctrl Pts',(-21.2933350165072,-19.0199546642823,
-6.5632584921937));
#63471=CARTESIAN_POINT('Ctrl Pts',(-21.294022704555,-18.985119821685,-6.56498419121111));
#63472=CARTESIAN_POINT('Ctrl Pts',(-21.2939994283744,-18.9502892333484,
-6.56670989022851));
#63473=CARTESIAN_POINT('Origin',(-18.734,-18.952,1.76670989022851));
#63474=CARTESIAN_POINT('',(-17.1744641548914,-16.9218650419685,-5.25018234058848));
#63475=CARTESIAN_POINT('',(-17.1744641548914,-16.9218650419685,-5.31661774876036));
#63476=CARTESIAN_POINT('',(-17.1744641548914,-16.9218650419685,1.76670989022851));
#63477=CARTESIAN_POINT('',(-21.2939994369002,-18.9503020392335,-5.8332901097715));
#63478=CARTESIAN_POINT('Ctrl Pts',(-17.1744641548914,-16.9218650419685,
-5.31661774876036));
#63479=CARTESIAN_POINT('Ctrl Pts',(-17.1078003775552,-16.9730757015923,
-5.3208013195428));
#63480=CARTESIAN_POINT('Ctrl Pts',(-17.0437399774918,-17.0275131658057,
-5.32498489032524));
#63481=CARTESIAN_POINT('Ctrl Pts',(-16.9825941690676,-17.084869148834,-5.32916846110767));
#63482=CARTESIAN_POINT('Ctrl Pts',(-16.929973447652,-17.1342284308883,-5.33276874898248));
#63483=CARTESIAN_POINT('Ctrl Pts',(-16.8795107690236,-17.1857484040204,
-5.33636903685729));
#63484=CARTESIAN_POINT('Ctrl Pts',(-16.8313804354228,-17.239213150305,-5.3399693247321));
#63485=CARTESIAN_POINT('Ctrl Pts',(-16.7754382840342,-17.3013555188872,
-5.34415395912515));
#63486=CARTESIAN_POINT('Ctrl Pts',(-16.7224397206528,-17.3663571440022,
-5.3483385935182));
#63487=CARTESIAN_POINT('Ctrl Pts',(-16.6726908063355,-17.4339076417707,
-5.35252322791125));
#63488=CARTESIAN_POINT('Ctrl Pts',(-16.62301270344,-17.5013619897668,-5.35670190599519));
#63489=CARTESIAN_POINT('Ctrl Pts',(-16.5765753324319,-17.5713576368076,
-5.36088058407914));
#63490=CARTESIAN_POINT('Ctrl Pts',(-16.533646260122,-17.6435492292773,-5.36505926216308));
#63491=CARTESIAN_POINT('Ctrl Pts',(-16.4899477150434,-17.7170348041589,
-5.36931284004852));
#63492=CARTESIAN_POINT('Ctrl Pts',(-16.4498848008427,-17.7927954651138,
-5.37356641793395));
#63493=CARTESIAN_POINT('Ctrl Pts',(-16.4136951701205,-17.8704337762127,
-5.37781999581939));
#63494=CARTESIAN_POINT('Ctrl Pts',(-16.378207146008,-17.9465669171522,-5.38199110979734));
#63495=CARTESIAN_POINT('Ctrl Pts',(-16.3464437665668,-18.0245051179384,
-5.38616222377529));
#63496=CARTESIAN_POINT('Ctrl Pts',(-16.3185831851716,-18.1038481205325,
-5.39033333775324));
#63497=CARTESIAN_POINT('Ctrl Pts',(-16.2907319526636,-18.1831644988157,
-5.39450305207362));
#63498=CARTESIAN_POINT('Ctrl Pts',(-16.2667810695588,-18.2638843090192,
-5.39867276639399));
#63499=CARTESIAN_POINT('Ctrl Pts',(-16.2468600106956,-18.3455886927152,
-5.40284248071436));
#63500=CARTESIAN_POINT('Ctrl Pts',(-16.2269396607091,-18.4272901690186,
-5.40701204665841));
#63501=CARTESIAN_POINT('Ctrl Pts',(-16.2110489579957,-18.5099757020134,
-5.41118161260245));
#63502=CARTESIAN_POINT('Ctrl Pts',(-16.1992667534716,-18.5932140346339,
-5.4153511785465));
#63503=CARTESIAN_POINT('Ctrl Pts',(-16.1870703011713,-18.6793789243438,
-5.41966734128542));
#63504=CARTESIAN_POINT('Ctrl Pts',(-16.1792767060087,-18.7661356875971,
-5.42398350402433));
#63505=CARTESIAN_POINT('Ctrl Pts',(-16.1759149870658,-18.8529996636308,
-5.42829966676326));
#63506=CARTESIAN_POINT('Ctrl Pts',(-16.1726627757638,-18.9370340547817,
-5.43247523095494));
#63507=CARTESIAN_POINT('Ctrl Pts',(-16.1735580857934,-19.0211683105536,
-5.43665079514662));
#63508=CARTESIAN_POINT('Ctrl Pts',(-16.1785740672325,-19.1049650356758,
-5.4408263593383));
#63509=CARTESIAN_POINT('Ctrl Pts',(-16.1838433939698,-19.1929941341762,
-5.44521282135084));
#63510=CARTESIAN_POINT('Ctrl Pts',(-16.1936605371381,-19.2806501283314,
-5.44959928336338));
#63511=CARTESIAN_POINT('Ctrl Pts',(-16.2079333028748,-19.3674359657935,
-5.45398574537592));
#63512=CARTESIAN_POINT('Ctrl Pts',(-16.2222060686114,-19.4542218032555,
-5.45837220738846));
#63513=CARTESIAN_POINT('Ctrl Pts',(-16.2409342590202,-19.5401369333207,
-5.462758669401));
#63514=CARTESIAN_POINT('Ctrl Pts',(-16.2639654295305,-19.6247029215675,
-5.46714513141354));
#63515=CARTESIAN_POINT('Ctrl Pts',(-16.2859369017452,-19.7053779033382,
-5.47132976580659));
#63516=CARTESIAN_POINT('Ctrl Pts',(-16.3119058645756,-19.7851254547589,
-5.47551440019964));
#63517=CARTESIAN_POINT('Ctrl Pts',(-16.3417769993438,-19.863520222009,-5.47969903459269));
#63518=CARTESIAN_POINT('Ctrl Pts',(-16.3716056162489,-19.9418034040112,
-5.48387771267663));
#63519=CARTESIAN_POINT('Ctrl Pts',(-16.4053252101866,-20.0187372003264,
-5.48805639076057));
#63520=CARTESIAN_POINT('Ctrl Pts',(-16.4427902222593,-20.0939096962481,
-5.49223506884451));
#63521=CARTESIAN_POINT('Ctrl Pts',(-16.4809267677478,-20.1704296051337,
-5.49648864672995));
#63522=CARTESIAN_POINT('Ctrl Pts',(-16.5229441986227,-20.2451239847432,
-5.50074222461539));
#63523=CARTESIAN_POINT('Ctrl Pts',(-16.5686369710085,-20.3175778823182,
-5.50499580250082));
#63524=CARTESIAN_POINT('Ctrl Pts',(-16.6134438998394,-20.3886271197065,
-5.50916691647877));
#63525=CARTESIAN_POINT('Ctrl Pts',(-16.6617846778615,-20.4575215650235,
-5.51333803045673));
#63526=CARTESIAN_POINT('Ctrl Pts',(-16.7134191824493,-20.5238947673893,
-5.51750914443468));
#63527=CARTESIAN_POINT('Ctrl Pts',(-16.7650363605803,-20.5902456975861,
-5.52167885875505));
#63528=CARTESIAN_POINT('Ctrl Pts',(-16.8199447880143,-20.6540767022587,
-5.52584857307543));
#63529=CARTESIAN_POINT('Ctrl Pts',(-16.8778623533737,-20.7150521934352,
-5.5300182873958));
#63530=CARTESIAN_POINT('Ctrl Pts',(-16.9357778577776,-20.776025514842,-5.53418785333984));
#63531=CARTESIAN_POINT('Ctrl Pts',(-16.9967019697692,-20.8341431918207,
-5.53835741928388));
#63532=CARTESIAN_POINT('Ctrl Pts',(-17.0603147509096,-20.8891054919589,
-5.54252698522793));
